#73184 = ORIENTED_EDGE ( 'NONE', *, *, #81814, .F. ) ;
#73185 = CARTESIAN_POINT ( 'NONE',  ( 74.79166666666667140, 3.975000000000003642, -6.884901960086285300 ) ) ;
#73186 = DIRECTION ( 'NONE',  ( 1.000000000000000000, 0.000000000000000000, 0.000000000000000000 ) ) ;
#73187 = CARTESIAN_POINT ( 'NONE',  ( 95.28709685856479439, 3.054999999999997495, 5.291415217122919401 ) ) ;
#73188 = ORIENTED_EDGE ( 'NONE', *, *, #112105, .T. ) ;
#73189 = FACE_OUTER_BOUND ( 'NONE', #142407, .T. ) ;
#73190 = VERTEX_POINT ( 'NONE', #127683 ) ;
#73192 = EDGE_CURVE ( 'NONE', #14419, #121472, #83459, .T. ) ;
#73191 = CARTESIAN_POINT ( 'NONE',  ( -21.29974487139158512, -27.71228299555221142, 4.000000000000000000 ) ) ;
#73193 = LINE ( 'NONE', #52813, #137143 ) ;
#73194 = LINE ( 'NONE', #9287, #99476 ) ;
#73195 = EDGE_LOOP ( 'NONE', ( #53444, #4989, #10081, #53711 ) ) ;
#73196 = ORIENTED_EDGE ( 'NONE', *, *, #96369, .F. ) ;
#73197 = VERTEX_POINT ( 'NONE', #5133 ) ;
#73198 = DIRECTION ( 'NONE',  ( -0.3543493200069162685, -0.000000000000000000, -0.9351131265310288487 ) ) ;
#73199 = DIRECTION ( 'NONE',  ( -0.3543493200069164351, 0.000000000000000000, -0.9351131265310288487 ) ) ;
#73200 = CARTESIAN_POINT ( 'NONE',  ( 11.87956980810188767, 3.967499999999998916, 6.871911579029510442 ) ) ;
#73201 = DIRECTION ( 'NONE',  ( 0.000000000000000000, 0.000000000000000000, 1.000000000000000000 ) ) ;
#73202 = EDGE_CURVE ( 'NONE', #141613, #80963, #56916, .T. ) ;
#73203 = VERTEX_POINT ( 'NONE', #72626 ) ;
#73204 = VERTEX_POINT ( 'NONE', #101089 ) ;
#73205 = DIRECTION ( 'NONE',  ( 0.7071067811865487940, 0.7071067811865463515, 0.000000000000000000 ) ) ;
#73207 = ORIENTED_EDGE ( 'NONE', *, *, #90817, .F. ) ;
#73206 = EDGE_CURVE ( 'NONE', #34286, #108094, #16010, .T. ) ;
#73208 = EDGE_LOOP ( 'NONE', ( #142608, #43343, #107696, #115470 ) ) ;
#73209 = VECTOR ( 'NONE', #70530, 1000.000000000000000 ) ;
#73210 = CARTESIAN_POINT ( 'NONE',  ( -11.99999999999991473, -0.4125381241607498639, 4.000000000000000000 ) ) ;
#73211 = DIRECTION ( 'NONE',  ( -0.5735764363510507113, 0.8191520442889885789, 1.003171929053520926E-16 ) ) ;
#73212 = ORIENTED_EDGE ( 'NONE', *, *, #111933, .T. ) ;
#73213 = CARTESIAN_POINT ( 'NONE',  ( 25.82816939922335209, 21.75929247661549581, 4.000000000000000000 ) ) ;
#73214 = EDGE_CURVE ( 'NONE', #84066, #77643, #2468, .T. ) ;
#73215 = CARTESIAN_POINT ( 'NONE',  ( 11.51078643762690490, -27.52281430457047406, 5.000000000000000000 ) ) ;
#73216 = CYLINDRICAL_SURFACE ( 'NONE', #96983, 0.5000000000000004441 ) ;
#73217 = SURFACE_STYLE_FILL_AREA ( #118089 ) ;
#73218 = ORIENTED_EDGE ( 'NONE', *, *, #58289, .F. ) ;
#73219 = CARTESIAN_POINT ( 'NONE',  ( -4.499999999999976019, 22.08746187583903264, 4.000000000000000000 ) ) ;
#73220 = FACE_BOUND ( 'NONE', #99599, .T. ) ;
#73221 = EDGE_LOOP ( 'NONE', ( #83106, #1332, #95031 ) ) ;
#73222 = LINE ( 'NONE', #62349, #96658 ) ;
#73224 = ADVANCED_FACE ( 'NONE', ( #17467 ), #99689, .T. ) ;
#73223 = CARTESIAN_POINT ( 'NONE',  ( 5.380000000000000782, 9.521314400968980422E-16, 0.000000000000000000 ) ) ;
#73225 = CARTESIAN_POINT ( 'NONE',  ( 78.29974487139158157, -27.71228299555260577, 4.000000000000000000 ) ) ;
#73226 = ORIENTED_EDGE ( 'NONE', *, *, #34838, .T. ) ;
#73227 = DIRECTION ( 'NONE',  ( 0.7071067811865487940, 0.7071067811865463515, 0.000000000000000000 ) ) ;
#73228 = ORIENTED_EDGE ( 'NONE', *, *, #33554, .F. ) ;
#73229 = ORIENTED_EDGE ( 'NONE', *, *, #76056, .T. ) ;
#73230 = EDGE_LOOP ( 'NONE', ( #17879, #117761, #52761, #122548, #124549 ) ) ;
#73231 = AXIS2_PLACEMENT_3D ( 'NONE', #133835, #13445, #80193 ) ;
#73232 = CARTESIAN_POINT ( 'NONE',  ( 27.62043019189810877, 3.055000000000001936, -5.291415217122916737 ) ) ;
#73233 = DIRECTION ( 'NONE',  ( 0.6830127018922181881, 0.6830127018922202975, -0.2588190451025214056 ) ) ;
#73234 = VECTOR ( 'NONE', #6982, 1000.000000000000000 ) ;
#73235 = LINE ( 'NONE', #95671, #113257 ) ;
#73236 = CARTESIAN_POINT ( 'NONE',  ( 13.49159235450332162, 9.902892378096218942E-16, 0.000000000000000000 ) ) ;
#73237 = PLANE ( 'NONE',  #59844 ) ;
#73239 = LINE ( 'NONE', #52174, #75062 ) ;
#73238 = DIRECTION ( 'NONE',  ( -0.7071067811865486830, 0.7071067811865464625, 0.000000000000000000 ) ) ;
#73240 = DIRECTION ( 'NONE',  ( 0.6830127018922181881, 0.6830127018922202975, -0.2588190451025214056 ) ) ;
#73241 = CARTESIAN_POINT ( 'NONE',  ( -12.83829387547372924, -6.740707523384205757, 16.75550250614864112 ) ) ;
#73242 = ADVANCED_FACE ( 'NONE', ( #137851 ), #30252, .T. ) ;
#73243 = CARTESIAN_POINT ( 'NONE',  ( 10.49999999999993605, 4.087461875839200509, 4.000000000000000000 ) ) ;
#73244 = LINE ( 'NONE', #74679, #98047 ) ;
#73245 = AXIS2_PLACEMENT_3D ( 'NONE', #139492, #29249, #108930 ) ;
#73246 = ORIENTED_EDGE ( 'NONE', *, *, #39936, .T. ) ;
#73247 = ORIENTED_EDGE ( 'NONE', *, *, #98030, .T. ) ;
#73248 = VERTEX_POINT ( 'NONE', #24258 ) ;
#73249 = EDGE_LOOP ( 'NONE', ( #85188, #31285, #118676, #53814 ) ) ;
#73250 = CARTESIAN_POINT ( 'NONE',  ( -1.320800000000306618, -4.493284886149243553E-13, 3.775643966265820328 ) ) ;
#73251 = EDGE_LOOP ( 'NONE', ( #9558, #133742, #94702, #113882 ) ) ;
#73252 = ORIENTED_EDGE ( 'NONE', *, *, #67685, .F. ) ;
#73253 = LINE ( 'NONE', #29019, #51428 ) ;
#73254 = DIRECTION ( 'NONE',  ( 0.6830127018922181881, 0.6830127018922202975, -0.2588190451025214056 ) ) ;
#73255 = ADVANCED_FACE ( 'NONE', ( #5854 ), #134457, .F. ) ;
#73256 = VECTOR ( 'NONE', #138420, 1000.000000000000000 ) ;
#73257 = EDGE_CURVE ( 'NONE', #48371, #140728, #112684, .T. ) ;
#73258 = CARTESIAN_POINT ( 'NONE',  ( 1.499999999999990896, 19.39370406404967184, 1.459788787078198258 ) ) ;
#73259 = ORIENTED_EDGE ( 'NONE', *, *, #142555, .T. ) ;
#73260 = CARTESIAN_POINT ( 'NONE',  ( -12.69999999999998153, 3.061616997868383634E-16, -2.500000000000000444 ) ) ;
#73261 = VERTEX_POINT ( 'NONE', #46779 ) ;
#73262 = VECTOR ( 'NONE', #40896, 999.9999999999998863 ) ;
#73264 = CARTESIAN_POINT ( 'NONE',  ( -20.99999999999984368, 17.58746187583906462, 4.000000000000000000 ) ) ;
#73263 = AXIS2_PLACEMENT_3D ( 'NONE', #85112, #30009, #74250 ) ;
#73265 = CARTESIAN_POINT ( 'NONE',  ( 7.139999999999985469, -39.92999999999999972, 18.93259187797431764 ) ) ;
#73266 = VECTOR ( 'NONE', #90664, 1000.000000000000000 ) ;
#73267 = CARTESIAN_POINT ( 'NONE',  ( 9.983736474768551972, -5.808823158059035485, -5.808823158059033709 ) ) ;
#73268 = ORIENTED_EDGE ( 'NONE', *, *, #89538, .F. ) ;
#73269 = CARTESIAN_POINT ( 'NONE',  ( 100.8287635252314516, 0.000000000000000000, -6.109999999999999432 ) ) ;
#73270 = CARTESIAN_POINT ( 'NONE',  ( 3.250000000000000000, 4.999999999999998224, 8.040613248383180784E-16 ) ) ;
#73271 = DIRECTION ( 'NONE',  ( -0.000000000000000000, -0.3543493200069152693, 0.9351131265310292928 ) ) ;
#73272 = DIRECTION ( 'NONE',  ( -0.7071067811865487940, 0.7071067811865463515, -0.000000000000000000 ) ) ;
#73273 = EDGE_LOOP ( 'NONE', ( #133867, #61640, #124392, #215 ) ) ;
#73274 = ORIENTED_EDGE ( 'NONE', *, *, #70924, .F. ) ;
#73275 = CARTESIAN_POINT ( 'NONE',  ( 131.8806778009766276, -49.14999999999999147, -40.92499999999998295 ) ) ;
#73276 = ORIENTED_EDGE ( 'NONE', *, *, #18392, .T. ) ;
#73277 = LINE ( 'NONE', #59553, #90287 ) ;
#73278 = DIRECTION ( 'NONE',  ( -0.7071067811865486830, -0.7071067811865464625, -0.000000000000000000 ) ) ;
#73279 = VECTOR ( 'NONE', #139841, 1000.000000000000000 ) ;
#73280 = LINE ( 'NONE', #29042, #84002 ) ;
#73281 = PLANE ( 'NONE',  #100469 ) ;
#73282 = EDGE_CURVE ( 'NONE', #73190, #82074, #90961, .T. ) ;
#73283 = ORIENTED_EDGE ( 'NONE', *, *, #128807, .T. ) ;
#73284 = CARTESIAN_POINT ( 'NONE',  ( -10.49999999999992717, -1.533600742197722910, 5.000000000000000000 ) ) ;
#73285 = CARTESIAN_POINT ( 'NONE',  ( 34.92499999999998295, -4.662012949885794733, -5.188494296035330855 ) ) ;
#73286 = CARTESIAN_POINT ( 'NONE',  ( 6.328169399223488867, 11.25929247661560595, 4.000000000000000000 ) ) ;
#73287 = VERTEX_POINT ( 'NONE', #798 ) ;
#73288 = CARTESIAN_POINT ( 'NONE',  ( -66.18398860626901126, 28.73617430169833753, 5.000000000000000000 ) ) ;
#73289 = CARTESIAN_POINT ( 'NONE',  ( -5.999999999999956479, 18.08204922493373346, 0.9627537363045027830 ) ) ;
#73290 = EDGE_LOOP ( 'NONE', ( #48468, #71451, #73546, #93070 ) ) ;
#73292 = EDGE_LOOP ( 'NONE', ( #52663, #37207, #45699, #132720 ) ) ;
#73291 = CARTESIAN_POINT ( 'NONE',  ( 0.000000000000000000, 0.000000000000000000, 6.750000000000000888 ) ) ;
#73293 = DIRECTION ( 'NONE',  ( 0.7071067811865487940, 0.7071067811865463515, 0.000000000000000000 ) ) ;
#73294 = LINE ( 'NONE', #98587, #73872 ) ;
#73295 = EDGE_LOOP ( 'NONE', ( #31799, #120302, #10272, #70897 ) ) ;
#73296 = DIRECTION ( 'NONE',  ( 0.6830127018922181881, 0.6830127018922202975, -0.2588190451025214056 ) ) ;
#73297 = CARTESIAN_POINT ( 'NONE',  ( 13.74845587132416291, -11.24070752338416490, 10.39518518046006079 ) ) ;
#73298 = EDGE_CURVE ( 'NONE', #44162, #16196, #131340, .T. ) ;
#73299 = VECTOR ( 'NONE', #140454, 1000.000000000000000 ) ;
#73300 = CARTESIAN_POINT ( 'NONE',  ( 81.18398860626899705, 28.73617430169844056, 5.000000000000000000 ) ) ;
#73301 = CARTESIAN_POINT ( 'NONE',  ( -54.18398860626899705, 28.73617430169825226, 5.000000000000000000 ) ) ;
#73302 = EDGE_CURVE ( 'NONE', #99607, #100020, #129807, .T. ) ;
#73303 = CARTESIAN_POINT ( 'NONE',  ( 34.42499999999998295, -19.45860074219776692, 5.000000000000000000 ) ) ;
#73304 = CARTESIAN_POINT ( 'NONE',  ( 1.499999999999997780, -14.94781430457067728, 5.000000000000000000 ) ) ;
#73305 = CARTESIAN_POINT ( 'NONE',  ( 47.81249999999999289, 5.819803920172571310, 5.819803920172576639 ) ) ;
#73306 = DIRECTION ( 'NONE',  ( -0.7071067811865486830, -0.7071067811865464625, 0.000000000000000000 ) ) ;
#73307 = PLANE ( 'NONE',  #53642 ) ;
#73308 = CARTESIAN_POINT ( 'NONE',  ( 26.99999999999999645, 5.837062628940091535, 2.500239961634333596 ) ) ;
#73309 = DIRECTION ( 'NONE',  ( 0.6830127018922180770, -0.6830127018922204085, -0.2588190451025213501 ) ) ;
#73311 = EDGE_CURVE ( 'NONE', #127430, #131000, #3469, .T. ) ;
#73310 = DIRECTION ( 'NONE',  ( -0.7071067811865487940, 0.7071067811865463515, 0.000000000000000000 ) ) ;
#73313 = EDGE_CURVE ( 'NONE', #9187, #93841, #25971, .T. ) ;
#73312 = EDGE_LOOP ( 'NONE', ( #33625, #25393, #59330, #42979 ) ) ;
#73314 =( BOUNDED_CURVE ( )  B_SPLINE_CURVE ( 3, ( #15534, #59815, #126463, #5388 ),
 .UNSPECIFIED., .F., .T. ) 
 B_SPLINE_CURVE_WITH_KNOTS ( ( 4, 4 ),
 ( 2.779374508378134045, 4.199602562396851368 ),
 .UNSPECIFIED. ) 
 CURVE ( )  GEOMETRIC_REPRESENTATION_ITEM ( )  RATIONAL_B_SPLINE_CURVE ( ( 1.000000000000000000, 0.8388583629366599403, 0.8388583629366599403, 1.000000000000000000 ) ) 
 REPRESENTATION_ITEM ( '' )  );
#73315 = ORIENTED_EDGE ( 'NONE', *, *, #66068, .F. ) ;
#73316 = VERTEX_POINT ( 'NONE', #36833 ) ;
#73317 = CARTESIAN_POINT ( 'NONE',  ( 107.7500000000000000, -9.735942053221458872E-16, 7.950000000000000178 ) ) ;
#73318 = ORIENTED_EDGE ( 'NONE', *, *, #69750, .F. ) ;
#73319 = ORIENTED_EDGE ( 'NONE', *, *, #106985, .F. ) ;
#73320 = ORIENTED_EDGE ( 'NONE', *, *, #34878, .F. ) ;
#73321 = AXIS2_PLACEMENT_3D ( 'NONE', #122858, #56224, #80795 ) ;
#73322 = CARTESIAN_POINT ( 'NONE',  ( 4.499999999999976019, 19.46639925780205616, 5.000000000000000000 ) ) ;
#73323 = CARTESIAN_POINT ( 'NONE',  ( 18.29974487139159223, -27.71228299555219010, 4.000000000000000000 ) ) ;
#73324 = ORIENTED_EDGE ( 'NONE', *, *, #42802, .T. ) ;
#73325 =( BOUNDED_CURVE ( )  B_SPLINE_CURVE ( 2, ( #50344, #127918, #38049, #16236, #27862, #40209, #28600, #116302, #18381, #51059, #61951, #139525, #61268 ),
 .UNSPECIFIED., .F., .T. ) 
 B_SPLINE_CURVE_WITH_KNOTS ( ( 3, 2, 2, 2, 2, 2, 3 ),
 ( 0.2666666666666666630, 0.2694444444444444309, 0.2722222222222221988, 0.2750000000000000222, 0.2777777777777777901, 0.2805555555555555580, 0.2833333333333333259 ),
 .UNSPECIFIED. ) 
 CURVE ( )  GEOMETRIC_REPRESENTATION_ITEM ( )  RATIONAL_B_SPLINE_CURVE ( ( 1.000000000000000000, 0.9659258262890683122, 1.000000000000000000, 0.9659258262890683122, 1.000000000000000000, 0.9659258262890683122, 1.000000000000000000, 0.9659258262890683122, 1.000000000000000000, 0.9659258262890683122, 1.000000000000000000, 0.9659258262890683122, 1.000000000000000000 ) ) 
 REPRESENTATION_ITEM ( '' )  );
#73326 = CARTESIAN_POINT ( 'NONE',  ( 0.000000000000000000, -2.375000000000000000, 0.000000000000000000 ) ) ;
#73327 = LINE ( 'NONE', #140015, #53292 ) ;
#73328 = ADVANCED_FACE ( 'NONE', ( #45090 ), #125285, .F. ) ;
#73330 = AXIS2_PLACEMENT_3D ( 'NONE', #5231, #37171, #82839 ) ;
#73329 = DIRECTION ( 'NONE',  ( 0.7071067811865486830, -0.7071067811865464625, -0.000000000000000000 ) ) ;
#73331 = CARTESIAN_POINT ( 'NONE',  ( 7.720000000000001528, 9.521314400968980422E-16, 0.000000000000000000 ) ) ;
#73332 = CARTESIAN_POINT ( 'NONE',  ( 104.7087635252314328, -7.482591942790329030E-16, 6.110000000000001208 ) ) ;
#73333 = VERTEX_POINT ( 'NONE', #81081 ) ;
#73334 = EDGE_CURVE ( 'NONE', #119622, #91654, #44356, .T. ) ;
#73335 = CARTESIAN_POINT ( 'NONE',  ( -14.95213108811772784, 4.188779951252514344, -32.28871390651440976 ) ) ;
#73336 = CARTESIAN_POINT ( 'NONE',  ( -50.99451991528749062, 28.92564299267973738, 4.000000000000000000 ) ) ;
#73337 = CARTESIAN_POINT ( 'NONE',  ( 34.49999999999975842, 10.94296225409029510, -9.576120664313178210 ) ) ;
#73338 = PLANE ( 'NONE',  #16790 ) ;
#73339 = PLANE ( 'NONE',  #121764 ) ;
#73340 = CARTESIAN_POINT ( 'NONE',  ( 41.78752705046289151, 0.000000000000000000, -7.949999999999998401 ) ) ;
#73341 = ADVANCED_FACE ( 'NONE', ( #87123 ), #102827, .F. ) ;
#73342 = AXIS2_PLACEMENT_3D ( 'NONE', #9530, #29871, #98009 ) ;
#73343 = DIRECTION ( 'NONE',  ( -0.7071067811865486830, -0.7071067811865464625, -0.000000000000000000 ) ) ;
#73344 = CARTESIAN_POINT ( 'NONE',  ( 174.7500000000000000, 7.919999999999947526, -18.97500000000001918 ) ) ;
#73345 = ORIENTED_EDGE ( 'NONE', *, *, #107749, .F. ) ;
#73346 = ORIENTED_EDGE ( 'NONE', *, *, #136759, .T. ) ;
#73347 = CARTESIAN_POINT ( 'NONE',  ( 126.1462635252314328, -4.472830434245840259, 4.472830434245839371 ) ) ;
#73348 = AXIS2_PLACEMENT_3D ( 'NONE', #92417, #48958, #72164 ) ;
#73349 = ORIENTED_EDGE ( 'NONE', *, *, #73732, .T. ) ;
#73350 = DIRECTION ( 'NONE',  ( -0.6830127018922180770, -0.6830127018922204085, -0.2588190451025213501 ) ) ;
#73351 = LINE ( 'NONE', #129130, #96429 ) ;
#73352 = EDGE_CURVE ( 'NONE', #108369, #60317, #70239, .T. ) ;
#73353 = DIRECTION ( 'NONE',  ( -0.000000000000000000, -0.3543493200069152693, 0.9351131265310292928 ) ) ;
#73354 = DIRECTION ( 'NONE',  ( 0.7071067811865486830, -0.7071067811865464625, -0.000000000000000000 ) ) ;
#73355 = DIRECTION ( 'NONE',  ( -1.000000000000000000, 0.000000000000000000, 0.000000000000000000 ) ) ;
#73356 = LINE ( 'NONE', #138605, #81216 ) ;
#73357 = CARTESIAN_POINT ( 'NONE',  ( 125.4745968585647944, 1.637169565754164058, -6.109999999999996767 ) ) ;
#73359 = VERTEX_POINT ( 'NONE', #88569 ) ;
#73358 = VECTOR ( 'NONE', #38258, 1000.000000000000000 ) ;
#73360 = CARTESIAN_POINT ( 'NONE',  ( -34.92500000000001137, 18.20450307870169482, 3.476483422452869565 ) ) ;
#73361 = ORIENTED_EDGE ( 'NONE', *, *, #14239, .T. ) ;
#73362 = EDGE_CURVE ( 'NONE', #128274, #120044, #66102, .T. ) ;
#73363 = CARTESIAN_POINT ( 'NONE',  ( -2.000000000000000000, 2.375000000000000000, 4.319999999999998508 ) ) ;
#73364 = DIRECTION ( 'NONE',  ( 0.7071067811865487940, 0.7071067811865463515, 0.000000000000000000 ) ) ;
#73365 = DIRECTION ( 'NONE',  ( 1.000000000000000000, 0.000000000000000000, 0.000000000000000000 ) ) ;
#73366 = EDGE_LOOP ( 'NONE', ( #57325, #3835, #79293, #49556 ) ) ;
#73367 = AXIS2_PLACEMENT_3D ( 'NONE', #139541, #27876, #37342 ) ;
#73368 = CARTESIAN_POINT ( 'NONE',  ( 49.14626352523143282, -4.472830434245840259, 4.472830434245839371 ) ) ;
#73369 = EDGE_LOOP ( 'NONE', ( #117107, #43470, #60310, #73944 ) ) ;
#73370 = LINE ( 'NONE', #29827, #26237 ) ;
#73371 = LINE ( 'NONE', #130946, #25424 ) ;
#73372 = CARTESIAN_POINT ( 'NONE',  ( -54.48921356237310221, -27.52281430457093236, 5.000000000000000000 ) ) ;
#73373 = EDGE_CURVE ( 'NONE', #45800, #78583, #10948, .T. ) ;
#73374 = EDGE_CURVE ( 'NONE', #94538, #87694, #21141, .T. ) ;
#73375 = CARTESIAN_POINT ( 'NONE',  ( 5.999999999999963585, -10.06887692260771061, 4.000000000000000000 ) ) ;
#73376 = VECTOR ( 'NONE', #39681, 1000.000000000000000 ) ;
#73377 = AXIS2_PLACEMENT_3D ( 'NONE', #76957, #78358, #67507 ) ;
#73378 = EDGE_CURVE ( 'NONE', #44903, #59504, #62672, .T. ) ;
#73379 = VECTOR ( 'NONE', #70163, 1000.000000000000227 ) ;
#73380 = CARTESIAN_POINT ( 'NONE',  ( 50.51626352523143737, -4.472830434245839371, 4.472830434245839371 ) ) ;
#73381 = VERTEX_POINT ( 'NONE', #136150 ) ;
#73382 = CARTESIAN_POINT ( 'NONE',  ( 33.29974487139158867, -27.71228299555229313, 4.000000000000000000 ) ) ;
#73383 = VECTOR ( 'NONE', #34647, 1000.000000000000000 ) ;
#73384 = CARTESIAN_POINT ( 'NONE',  ( 3.489213562373097322, -27.52281430457057709, 5.000000000000000000 ) ) ;
#73385 = ORIENTED_EDGE ( 'NONE', *, *, #123024, .T. ) ;
#73386 = ORIENTED_EDGE ( 'NONE', *, *, #90756, .T. ) ;
#73387 = AXIS2_PLACEMENT_3D ( 'NONE', #105937, #63218, #137899 ) ;
#73388 = ORIENTED_EDGE ( 'NONE', *, *, #5294, .T. ) ;
#73389 = CARTESIAN_POINT ( 'NONE',  ( 60.01669371712956291, 7.950000000000000178, -2.130196079827421318 ) ) ;
#73390 = EDGE_LOOP ( 'NONE', ( #132288, #78655, #87510, #61570 ) ) ;
#73391 = CARTESIAN_POINT ( 'NONE',  ( 3.489213562373097322, -27.52281430457057709, 5.000000000000000000 ) ) ;
#73392 = FACE_BOUND ( 'NONE', #127083, .T. ) ;
#73393 = CARTESIAN_POINT ( 'NONE',  ( 18.29974487139159223, -27.71228299555219010, 4.000000000000000000 ) ) ;
#73394 = DIRECTION ( 'NONE',  ( 0.6830127018922180770, -0.6830127018922204085, -0.2588190451025213501 ) ) ;
#73395 = ORIENTED_EDGE ( 'NONE', *, *, #3075, .F. ) ;
#73396 =( NAMED_UNIT ( * ) PLANE_ANGLE_UNIT ( ) SI_UNIT ( $, .RADIAN. ) );
#73397 = ORIENTED_EDGE ( 'NONE', *, *, #10993, .F. ) ;
#73398 = VECTOR ( 'NONE', #132822, 1000.000000000000000 ) ;
#73399 = ORIENTED_EDGE ( 'NONE', *, *, #57929, .T. ) ;
#73400 = CARTESIAN_POINT ( 'NONE',  ( -32.29289321881322650, -15.74070752338412760, 5.000000000000000000 ) ) ;
#73401 = ORIENTED_EDGE ( 'NONE', *, *, #3516, .T. ) ;
#73402 = CARTESIAN_POINT ( 'NONE',  ( 57.66209685856478728, -5.291415217122919401, 3.054999999999997939 ) ) ;
#73403 = VECTOR ( 'NONE', #83977, 1000.000000000000227 ) ;
#73404 = EDGE_LOOP ( 'NONE', ( #84295, #111671, #88684, #77614 ) ) ;
#73405 = DIRECTION ( 'NONE',  ( -0.7071067811865487940, 0.7071067811865463515, 0.000000000000000000 ) ) ;
#73406 = DIRECTION ( 'NONE',  ( 0.7071067811865487940, 0.7071067811865463515, 0.000000000000000000 ) ) ;
#73407 = VERTEX_POINT ( 'NONE', #114397 ) ;
#73408 = DIRECTION ( 'NONE',  ( 0.7071067811865487940, 0.7071067811865463515, 0.000000000000000000 ) ) ;
#73409 = VECTOR ( 'NONE', #3180, 1000.000000000000000 ) ;
#73410 = DIRECTION ( 'NONE',  ( 0.1737853339090542071, 0.1737853339090537907, 0.9693282805305111216 ) ) ;
#73411 = FACE_OUTER_BOUND ( 'NONE', #135750, .T. ) ;
#73412 = CARTESIAN_POINT ( 'NONE',  ( 0.000000000000000000, -9.500000000000000000, 0.000000000000000000 ) ) ;
#73413 = CARTESIAN_POINT ( 'NONE',  ( 16.18750000000000000, 4.461849672132297329, -4.461849672132302658 ) ) ;
#73414 = DIRECTION ( 'NONE',  ( -0.7071067811865486830, -0.7071067811865464625, 0.000000000000000000 ) ) ;
#73415 = ORIENTED_EDGE ( 'NONE', *, *, #38820, .T. ) ;
#73416 = VECTOR ( 'NONE', #8177, 1000.000000000000000 ) ;
#73417 = ORIENTED_EDGE ( 'NONE', *, *, #32105, .F. ) ;
#73418 = DIRECTION ( 'NONE',  ( -0.000000000000000000, 0.000000000000000000, 1.000000000000000000 ) ) ;
#73419 = FACE_OUTER_BOUND ( 'NONE', #13669, .T. ) ;
#73420 = EDGE_LOOP ( 'NONE', ( #37883, #21267, #75239 ) ) ;
#73421 = ORIENTED_EDGE ( 'NONE', *, *, #114155, .T. ) ;
#73422 = ORIENTED_EDGE ( 'NONE', *, *, #132915, .T. ) ;
#73423 = DIRECTION ( 'NONE',  ( 0.7071067811865486830, -0.7071067811865464625, -0.000000000000000000 ) ) ;
#73424 = VECTOR ( 'NONE', #137214, 1000.000000000000000 ) ;
#73425 = EDGE_CURVE ( 'NONE', #82074, #27289, #76994, .T. ) ;
#73426 = EDGE_CURVE ( 'NONE', #92047, #92458, #54516, .T. ) ;
#73427 = FACE_OUTER_BOUND ( 'NONE', #29109, .T. ) ;
#73428 = ORIENTED_EDGE ( 'NONE', *, *, #121125, .F. ) ;
#73429 = CARTESIAN_POINT ( 'NONE',  ( -20.99999999999984368, -7.447814304570752775, 5.000000000000000000 ) ) ;
#73430 = CARTESIAN_POINT ( 'NONE',  ( 14.99999999999990052, -6.412538124160687580, 4.000000000000000000 ) ) ;
#73431 = CARTESIAN_POINT ( 'NONE',  ( 8.379569808101887674, 3.967499999999998916, 6.871911579029510442 ) ) ;
#73432 = DIRECTION ( 'NONE',  ( -0.000000000000000000, 0.3543493200069153248, 0.9351131265310292928 ) ) ;
#73433 = ORIENTED_EDGE ( 'NONE', *, *, #60595, .F. ) ;
#73434 = CARTESIAN_POINT ( 'NONE',  ( 127.8079301918981230, -6.109999999999999432, 1.637169565754158507 ) ) ;
#73435 = AXIS2_PLACEMENT_3D ( 'NONE', #108106, #29852, #119692 ) ;
#73436 = EDGE_CURVE ( 'NONE', #43782, #130838, #135464, .T. ) ;
#73437 = CARTESIAN_POINT ( 'NONE',  ( 20.19999999999999929, 2.055000000000001492, 0.000000000000000000 ) ) ;
#73438 = DIRECTION ( 'NONE',  ( -0.000000000000000000, -0.3543493200069152693, 0.9351131265310292928 ) ) ;
#73440 = ORIENTED_EDGE ( 'NONE', *, *, #64806, .F. ) ;
#73439 = CARTESIAN_POINT ( 'NONE',  ( 2.292893218813439216, 20.25929247661551713, 5.000000000000000000 ) ) ;
#73441 = LINE ( 'NONE', #4525, #97953 ) ;
#73442 = ORIENTED_EDGE ( 'NONE', *, *, #70512, .T. ) ;
#73443 = CARTESIAN_POINT ( 'NONE',  ( 75.47502705046287019, -5.819803920172573086, 5.819803920172573086 ) ) ;
#73444 = PLANE ( 'NONE',  #79472 ) ;
#73445 = DIRECTION ( 'NONE',  ( -0.7071067811865486830, -0.7071067811865464625, -0.000000000000000000 ) ) ;
#73446 = ADVANCED_FACE ( 'NONE', ( #21856 ), #132805, .F. ) ;
#73447 = VERTEX_POINT ( 'NONE', #80377 ) ;
#73448 = AXIS2_PLACEMENT_3D ( 'NONE', #29330, #83019, #39529 ) ;
#73449 = LINE ( 'NONE', #115467, #79655 ) ;
#73450 = LINE ( 'NONE', #18301, #16369 ) ;
#73451 = CARTESIAN_POINT ( 'NONE',  ( -13.49999999999990052, 6.052185695429106893, 5.000000000000000000 ) ) ;
#73452 = ORIENTED_EDGE ( 'NONE', *, *, #108765, .F. ) ;
#73453 = ADVANCED_FACE ( 'NONE', ( #124566 ), #135664, .F. ) ;
#73454 = DIRECTION ( 'NONE',  ( -0.000000000000000000, 0.000000000000000000, 1.000000000000000000 ) ) ;
#73455 = DIRECTION ( 'NONE',  ( -0.7071067811865487940, 0.7071067811865463515, 0.000000000000000000 ) ) ;
#73456 = DIRECTION ( 'NONE',  ( -0.6830127018922181881, 0.6830127018922202975, -0.2588190451025214056 ) ) ;
#73457 = DIRECTION ( 'NONE',  ( -0.000000000000000000, -0.3543493200069152693, 0.9351131265310292928 ) ) ;
#73458 = VECTOR ( 'NONE', #1299, 1000.000000000000000 ) ;
#73459 = CYLINDRICAL_SURFACE ( 'NONE', #99337, 5.999999999999998224 ) ;
#73460 = ORIENTED_EDGE ( 'NONE', *, *, #6277, .F. ) ;
#73461 = ORIENTED_EDGE ( 'NONE', *, *, #84309, .F. ) ;
#73462 = LINE ( 'NONE', #116239, #3173 ) ;
#73463 = VECTOR ( 'NONE', #66420, 1000.000000000000000 ) ;
#73464 = AXIS2_PLACEMENT_3D ( 'NONE', #68422, #90124, #35071 ) ;
#73465 = CARTESIAN_POINT ( 'NONE',  ( 14.99956980810188689, -3.967499999999998028, -6.871911579029511330 ) ) ;
#73466 = DIRECTION ( 'NONE',  ( 0.7071067811865486830, -0.7071067811865464625, -0.000000000000000000 ) ) ;
#73467 = CIRCLE ( 'NONE', #27181, 2.055000000000001048 ) ;
#73468 = LINE ( 'NONE', #82225, #120072 ) ;
#73469 = DIRECTION ( 'NONE',  ( -1.000000000000000000, -0.000000000000000000, -0.000000000000000000 ) ) ;
#73470 = EDGE_LOOP ( 'NONE', ( #43563, #57004, #23805, #2059 ) ) ;
#73471 = EDGE_CURVE ( 'NONE', #92630, #132295, #120455, .T. ) ;
#73472 = SPHERICAL_SURFACE ( 'NONE', #41916, 0.5000000000000000000 ) ;
#73473 = LINE ( 'NONE', #91808, #11885 ) ;
#73474 = AXIS2_PLACEMENT_3D ( 'NONE', #49117, #27320, #15699 ) ;
#73475 = CARTESIAN_POINT ( 'NONE',  ( 0.000000000000000000, 0.000000000000000000, 5.000000000000000000 ) ) ;
#73476 = CARTESIAN_POINT ( 'NONE',  ( 48.47459685856478728, 1.637169565754164280, -6.109999999999997655 ) ) ;
#73477 = DIRECTION ( 'NONE',  ( 0.000000000000000000, -1.000000000000000000, 0.000000000000000000 ) ) ;
#73478 = ADVANCED_FACE ( 'NONE', ( #12434 ), #45120, .T. ) ;
#73479 = EDGE_CURVE ( 'NONE', #71697, #25861, #89989, .T. ) ;
#73480 = ORIENTED_EDGE ( 'NONE', *, *, #71013, .F. ) ;
#73481 = DIRECTION ( 'NONE',  ( 0.7071067811865486830, -0.7071067811865464625, -0.000000000000000000 ) ) ;
#73482 = EDGE_LOOP ( 'NONE', ( #57183, #117200, #105332, #72064 ) ) ;
#73483 = EDGE_LOOP ( 'NONE', ( #31178, #113472, #11596, #15922 ) ) ;
#73484 = CARTESIAN_POINT ( 'NONE',  ( -7.499999999999954703, 3.653845994658382779, -4.504631822206354386 ) ) ;
#73485 = ADVANCED_FACE ( 'NONE', ( #3669 ), #23295, .F. ) ;
#73486 = CARTESIAN_POINT ( 'NONE',  ( 21.60486233187507921, 21.75929247661549226, 21.32995629748181443 ) ) ;
#73487 = PLANE ( 'NONE',  #23431 ) ;
#73488 = DIRECTION ( 'NONE',  ( -0.6830127018922180770, -0.6830127018922204085, -0.2588190451025213501 ) ) ;
#73489 = EDGE_CURVE ( 'NONE', #96482, #95547, #17413, .T. ) ;
#73490 = CARTESIAN_POINT ( 'NONE',  ( 82.66666666666667140, 6.884901960086285300, 3.975000000000003642 ) ) ;
#73491 = CARTESIAN_POINT ( 'NONE',  ( 126.8754301918981184, -5.291415217122920289, -3.055000000000001492 ) ) ;
#73492 = EDGE_LOOP ( 'NONE', ( #106106, #122240, #76945, #55718, #83057 ) ) ;
#73493 = EDGE_CURVE ( 'NONE', #98697, #83142, #26188, .T. ) ;
#73494 = FACE_OUTER_BOUND ( 'NONE', #136426, .T. ) ;
#73495 = DIRECTION ( 'NONE',  ( 0.3543493200069162685, -0.000000000000000000, -0.9351131265310288487 ) ) ;
#73496 = CIRCLE ( 'NONE', #85065, 2.499999999999998668 ) ;
#73497 = LINE ( 'NONE', #95942, #47307 ) ;
#73498 = PLANE ( 'NONE',  #6779 ) ;
#73499 = LINE ( 'NONE', #53140, #128391 ) ;
#73500 =( BOUNDED_CURVE ( )  B_SPLINE_CURVE ( 3, ( #26506, #70751, #125096, #4686 ),
 .UNSPECIFIED., .F., .T. ) 
 B_SPLINE_CURVE_WITH_KNOTS ( ( 4, 4 ),
 ( 4.350170835173024386, 4.500739107949264017 ),
 .UNSPECIFIED. ) 
 CURVE ( )  GEOMETRIC_REPRESENTATION_ITEM ( )  RATIONAL_B_SPLINE_CURVE ( ( 1.000000000000000000, 0.9981116584018943083, 0.9981116584018943083, 1.000000000000000000 ) ) 
 REPRESENTATION_ITEM ( '' )  );
#73501 = DIRECTION ( 'NONE',  ( 0.000000000000000000, -1.000000000000000000, 0.000000000000000000 ) ) ;
#73502 = CARTESIAN_POINT ( 'NONE',  ( 63.95419371712955581, 6.884901960086283523, 3.975000000000002753 ) ) ;
#73503 = AXIS2_PLACEMENT_3D ( 'NONE', #50625, #81865, #17274 ) ;
#73504 = PLANE ( 'NONE',  #99394 ) ;
#73505 = EDGE_LOOP ( 'NONE', ( #85808, #113104, #53282, #96153 ) ) ;
#73506 = ORIENTED_EDGE ( 'NONE', *, *, #109095, .F. ) ;
#73507 = CARTESIAN_POINT ( 'NONE',  ( 57.14583333333332860, 2.130196079827431976, -7.949999999999999289 ) ) ;
#73508 = EDGE_CURVE ( 'NONE', #46464, #49172, #14588, .T. ) ;
#73509 = CARTESIAN_POINT ( 'NONE',  ( 34.92499999999998295, -12.18334561358941137, 4.500000000000000888 ) ) ;
#73510 = DIRECTION ( 'NONE',  ( -0.000000000000000000, -0.3543493200069152693, 0.9351131265310292928 ) ) ;
#73511 = VECTOR ( 'NONE', #24315, 999.9999999999998863 ) ;
#73512 = CARTESIAN_POINT ( 'NONE',  ( 45.18398860626900415, 28.73617430169818832, 5.000000000000000000 ) ) ;
#73513 = ORIENTED_EDGE ( 'NONE', *, *, #40173, .F. ) ;
#73514 = EDGE_CURVE ( 'NONE', #84503, #29420, #45980, .T. ) ;
#73515 = DIRECTION ( 'NONE',  ( -0.7071067811865486830, -0.7071067811865464625, -0.000000000000000000 ) ) ;
#73516 = CARTESIAN_POINT ( 'NONE',  ( 58.62543019189810423, 5.291415217122919401, 3.055000000000002824 ) ) ;
#73517 = ORIENTED_EDGE ( 'NONE', *, *, #22513, .F. ) ;
#73518 = VECTOR ( 'NONE', #53527, 1000.000000000000000 ) ;
#73519 = CARTESIAN_POINT ( 'NONE',  ( -12.69999999999998153, 0.000000000000000000, 0.000000000000000000 ) ) ;
#73520 = ORIENTED_EDGE ( 'NONE', *, *, #96857, .T. ) ;
#73521 = EDGE_LOOP ( 'NONE', ( #20347, #135787, #82282, #126443 ) ) ;
#73522 = DIRECTION ( 'NONE',  ( 0.3543493200069162685, -0.000000000000000000, -0.9351131265310288487 ) ) ;
#73523 = SURFACE_SIDE_STYLE ('',( #63387 ) ) ;
#73524 = LINE ( 'NONE', #62647, #127672 ) ;
#73525 = VECTOR ( 'NONE', #62163, 1000.000000000000000 ) ;
#73526 = FACE_OUTER_BOUND ( 'NONE', #66794, .T. ) ;
#73527 = CARTESIAN_POINT ( 'NONE',  ( 9.183988606268997046, 28.73617430169793607, 5.000000000000000000 ) ) ;
#73528 = LINE ( 'NONE', #127167, #92788 ) ;
#73530 = VERTEX_POINT ( 'NONE', #78427 ) ;
#73529 = PLANE ( 'NONE',  #63813 ) ;
#73531 = CARTESIAN_POINT ( 'NONE',  ( -19.49999999999986855, 21.43112307739196609, 4.000000000000000000 ) ) ;
#73532 = LINE ( 'NONE', #95261, #100307 ) ;
#73533 = EDGE_CURVE ( 'NONE', #124853, #127004, #124774, .T. ) ;
#73534 = LINE ( 'NONE', #27151, #106299 ) ;
#73535 = EDGE_CURVE ( 'NONE', #22717, #133731, #24042, .T. ) ;
#73536 = ORIENTED_EDGE ( 'NONE', *, *, #79475, .F. ) ;
#73537 = EDGE_CURVE ( 'NONE', #10426, #67860, #56717, .T. ) ;
#73538 = ORIENTED_EDGE ( 'NONE', *, *, #116848, .T. ) ;
#73539 = VECTOR ( 'NONE', #90317, 999.9999999999998863 ) ;
#73540 = SURFACE_STYLE_FILL_AREA ( #119847 ) ;
#73541 = CARTESIAN_POINT ( 'NONE',  ( 78.80793019189810877, -6.109999999999998543, 1.637169565754158063 ) ) ;
#73542 = DIRECTION ( 'NONE',  ( 0.6830127018922180770, -0.6830127018922204085, -0.2588190451025213501 ) ) ;
#73543 = CARTESIAN_POINT ( 'NONE',  ( -12.19999999999999929, -59.76999999999998892, -39.50000000000000000 ) ) ;
#73544 = PLANE ( 'NONE',  #73367 ) ;
#73545 = ORIENTED_EDGE ( 'NONE', *, *, #51367, .T. ) ;
#73546 = ORIENTED_EDGE ( 'NONE', *, *, #22332, .F. ) ;
#73547 = PLANE ( 'NONE',  #130208 ) ;
#73548 = EDGE_CURVE ( 'NONE', #88210, #49923, #34933, .T. ) ;
#73549 = EDGE_LOOP ( 'NONE', ( #6152, #47391, #106576, #109590 ) ) ;
#73550 = VERTEX_POINT ( 'NONE', #1532 ) ;
#73551 = DIRECTION ( 'NONE',  ( -0.6830127018922181881, 0.6830127018922202975, -0.2588190451025214056 ) ) ;
#73552 = ORIENTED_EDGE ( 'NONE', *, *, #101235, .T. ) ;
#73553 = LINE ( 'NONE', #120579, #82670 ) ;
#73554 = DIRECTION ( 'NONE',  ( 0.3543493200069162685, -0.000000000000000000, -0.9351131265310288487 ) ) ;
#73555 = AXIS2_PLACEMENT_3D ( 'NONE', #27340, #18593, #51272 ) ;
#73556 = FACE_BOUND ( 'NONE', #29264, .T. ) ;
#73557 = CARTESIAN_POINT ( 'NONE',  ( -17.99451991528748351, 28.92564299267950645, 4.000000000000000000 ) ) ;
#73558 = CARTESIAN_POINT ( 'NONE',  ( -14.99999999999989697, 13.93112307739204070, 4.000000000000000000 ) ) ;
#73560 = ORIENTED_EDGE ( 'NONE', *, *, #54836, .F. ) ;
#73559 = DIRECTION ( 'NONE',  ( -0.7071067811865486830, -0.7071067811865464625, -0.000000000000000000 ) ) ;
#73561 = AXIS2_PLACEMENT_3D ( 'NONE', #25234, #1324, #58655 ) ;
#73562 = VECTOR ( 'NONE', #140756, 1000.000000000000000 ) ;
#73563 = FACE_OUTER_BOUND ( 'NONE', #37977, .T. ) ;
#73564 = APPLICATION_PROTOCOL_DEFINITION ( 'draft international standard', 'automotive_design', 1998, #129112 ) ;
#73565 = VERTEX_POINT ( 'NONE', #45815 ) ;
#73566 = ORIENTED_EDGE ( 'NONE', *, *, #121981, .T. ) ;
#73567 = CARTESIAN_POINT ( 'NONE',  ( 86.39126352523145158, -4.472830434245838482, -4.472830434245838482 ) ) ;
#73568 = VERTEX_POINT ( 'NONE', #24744 ) ;
#73569 = CARTESIAN_POINT ( 'NONE',  ( -23.01088028653932582, -22.02621442084247860, 4.990779571109221990 ) ) ;
#73570 = PLANE ( 'NONE',  #134619 ) ;
#73571 = EDGE_CURVE ( 'NONE', #87041, #94289, #124071, .T. ) ;
#73572 = CARTESIAN_POINT ( 'NONE',  ( -33.29974487139158867, -27.71228299555229313, 4.000000000000000000 ) ) ;
#73573 = CARTESIAN_POINT ( 'NONE',  ( 45.48921356237309510, -27.52281430457087197, 5.000000000000000000 ) ) ;
#73574 = CARTESIAN_POINT ( 'NONE',  ( 7.208502053023265077, 22.22500000000000142, 20.96595896090590117 ) ) ;
#73575 = CARTESIAN_POINT ( 'NONE',  ( 21.18398860626899349, 28.73617430169802134, 5.000000000000000000 ) ) ;
#73576 = DIRECTION ( 'NONE',  ( -0.7071067811865486830, -0.7071067811865464625, -0.000000000000000000 ) ) ;
#73577 = DIRECTION ( 'NONE',  ( 0.7071067811865487940, 0.7071067811865463515, 0.000000000000000000 ) ) ;
#73578 = PLANE ( 'NONE',  #19548 ) ;
#73579 = CARTESIAN_POINT ( 'NONE',  ( -22.82816939922336630, 12.75929247661558996, 4.000000000000000000 ) ) ;
#73580 = FACE_OUTER_BOUND ( 'NONE', #98016, .T. ) ;
#73581 = LINE ( 'NONE', #137413, #7506 ) ;
#73582 = ORIENTED_EDGE ( 'NONE', *, *, #61450, .T. ) ;
#73583 = CARTESIAN_POINT ( 'NONE',  ( -22.49999999999985079, -12.66682484999668290, -0.6294897503864461674 ) ) ;
#73584 = CARTESIAN_POINT ( 'NONE',  ( 34.92499999999998295, -12.53194198458144903, -8.170704600677598961 ) ) ;
#73585 = ADVANCED_FACE ( 'NONE', ( #13843 ), #58869, .F. ) ;
#73586 = ORIENTED_EDGE ( 'NONE', *, *, #106256, .T. ) ;
#73587 = ORIENTED_EDGE ( 'NONE', *, *, #95744, .F. ) ;
#73588 = EDGE_CURVE ( 'NONE', #69767, #124649, #126210, .T. ) ;
#73589 = EDGE_LOOP ( 'NONE', ( #121535, #114149, #32574, #735 ) ) ;
#73590 = CARTESIAN_POINT ( 'NONE',  ( 36.89626352523143993, 4.472830434245840259, -4.472830434245838482 ) ) ;
#73591 = VECTOR ( 'NONE', #109582, 1000.000000000000000 ) ;
#73592 = EDGE_LOOP ( 'NONE', ( #92900, #5753, #2615, #36212 ) ) ;
#73593 = EDGE_CURVE ( 'NONE', #68517, #100573, #46674, .T. ) ;
#73594 = EDGE_CURVE ( 'NONE', #72640, #30768, #7242, .T. ) ;
#73595 = CARTESIAN_POINT ( 'NONE',  ( 17.54580628287044064, 5.278424836066143655, -3.047499999999997655 ) ) ;
#73596 = CARTESIAN_POINT ( 'NONE',  ( 11.08707631394196724, 10.76818482829728829, -26.45687733286667154 ) ) ;
#73597 = ORIENTED_EDGE ( 'NONE', *, *, #28407, .F. ) ;
#73598 = EDGE_CURVE ( 'NONE', #8801, #62928, #139962, .T. ) ;
#73599 = CARTESIAN_POINT ( 'NONE',  ( -27.29974487139158512, -27.71228299555225405, 4.000000000000000000 ) ) ;
#73600 = EDGE_LOOP ( 'NONE', ( #43753, #116731, #73101, #85644, #16331 ) ) ;
#73601 = DIRECTION ( 'NONE',  ( 0.3543493200069162685, -0.000000000000000000, -0.9351131265310288487 ) ) ;
#73602 = CARTESIAN_POINT ( 'NONE',  ( 34.92499999999998295, -3.183345613589516621, 4.500000000000000888 ) ) ;
#73604 = ORIENTED_EDGE ( 'NONE', *, *, #39331, .T. ) ;
#73603 = CARTESIAN_POINT ( 'NONE',  ( 7.171830600776422315, 9.759292476615620160, 4.000000000000000000 ) ) ;
#73605 = ORIENTED_EDGE ( 'NONE', *, *, #132415, .F. ) ;
#73606 = DIRECTION ( 'NONE',  ( 0.7071067811865487940, 0.7071067811865463515, 0.000000000000000000 ) ) ;
#73607 = EDGE_CURVE ( 'NONE', #45742, #56014, #5096, .T. ) ;
#73608 = ORIENTED_EDGE ( 'NONE', *, *, #138226, .T. ) ;
#73609 = LINE ( 'NONE', #30084, #4125 ) ;
#73610 = VERTEX_POINT ( 'NONE', #16723 ) ;
#73611 = ORIENTED_EDGE ( 'NONE', *, *, #9486, .T. ) ;
#73612 = ORIENTED_EDGE ( 'NONE', *, *, #109350, .T. ) ;
#73613 = ORIENTED_EDGE ( 'NONE', *, *, #86206, .F. ) ;
#73614 = DIRECTION ( 'NONE',  ( 0.7071067811865487940, 0.7071067811865463515, -0.000000000000000000 ) ) ;
#73615 = EDGE_CURVE ( 'NONE', #71971, #17986, #84164, .T. ) ;
#73616 = LINE ( 'NONE', #18477, #40062 ) ;
#73617 = CARTESIAN_POINT ( 'NONE',  ( 12.03892749862900402, 4.202752102959690472E-16, 0.000000000000000000 ) ) ;
#73618 = CARTESIAN_POINT ( 'NONE',  ( 7.139999999999997904, -35.14999999999999858, 17.49210858042622263 ) ) ;
#73619 = DIRECTION ( 'NONE',  ( -0.6830127018922181881, 0.6830127018922202975, -0.2588190451025214056 ) ) ;
#73620 = EDGE_LOOP ( 'NONE', ( #45060, #14664, #18937, #20606 ) ) ;
#73621 = DIRECTION ( 'NONE',  ( -0.6830127018922181881, 0.6830127018922202975, -0.2588190451025214056 ) ) ;
#73622 = ORIENTED_EDGE ( 'NONE', *, *, #85080, .F. ) ;
#73623 = EDGE_CURVE ( 'NONE', #48695, #115675, #26886, .T. ) ;
#73624 = DIRECTION ( 'NONE',  ( -0.000000000000000000, 0.3543493200069153248, 0.9351131265310292928 ) ) ;
#73625 = CARTESIAN_POINT ( 'NONE',  ( 27.39540314143522437, 2.126176841940962348, 7.934999999999989839 ) ) ;
#73626 = CARTESIAN_POINT ( 'NONE',  ( 8.475998614145455079, 22.03583458319438293, 4.979811245910090278 ) ) ;
#73627 = ORIENTED_EDGE ( 'NONE', *, *, #78191, .T. ) ;
#73628 = CARTESIAN_POINT ( 'NONE',  ( 23.47599861414535027, 22.03583458319437227, 4.979811245910089390 ) ) ;
#73629 = VECTOR ( 'NONE', #96536, 1000.000000000000000 ) ;
#73630 = CARTESIAN_POINT ( 'NONE',  ( 0.000000000000000000, 0.000000000000000000, 5.000000000000000000 ) ) ;
#73631 = ORIENTED_EDGE ( 'NONE', *, *, #126516, .F. ) ;
#73632 = ORIENTED_EDGE ( 'NONE', *, *, #68145, .F. ) ;
#73634 = ORIENTED_EDGE ( 'NONE', *, *, #132303, .F. ) ;
#73633 = EDGE_CURVE ( 'NONE', #16751, #129366, #82711, .T. ) ;
#73635 = DIRECTION ( 'NONE',  ( -0.7071067811865486830, -0.7071067811865464625, -0.000000000000000000 ) ) ;
#73636 = DIRECTION ( 'NONE',  ( -0.7071067811865487940, 0.7071067811865463515, -0.000000000000000000 ) ) ;
#73637 = DIRECTION ( 'NONE',  ( 0.7071067811865486830, -0.7071067811865464625, -0.000000000000000000 ) ) ;
#73638 = CARTESIAN_POINT ( 'NONE',  ( 0.000000000000000000, 0.000000000000000000, 5.000000000000000000 ) ) ;
#73639 = CARTESIAN_POINT ( 'NONE',  ( 73.41209685856478018, 5.291415217122922066, -3.054999999999995275 ) ) ;
#73640 = CARTESIAN_POINT ( 'NONE',  ( 28.49999999999980460, 15.05218569542901186, 5.000000000000000000 ) ) ;
#73641 = ADVANCED_FACE ( 'NONE', ( #116749 ), #73970, .T. ) ;
#73642 =( NAMED_UNIT ( * ) PLANE_ANGLE_UNIT ( ) SI_UNIT ( $, .RADIAN. ) );
#73643 = CARTESIAN_POINT ( 'NONE',  ( -2.999999999999980016, -16.60178936734448740, 0.8616154019347429527 ) ) ;
#73644 = LINE ( 'NONE', #138913, #79152 ) ;
#73645 = ADVANCED_FACE ( 'NONE', ( #92849 ), #28334, .F. ) ;
#73646 = DIRECTION ( 'NONE',  ( 0.000000000000000000, 0.000000000000000000, 1.000000000000000000 ) ) ;
#73647 = ORIENTED_EDGE ( 'NONE', *, *, #22906, .T. ) ;
#73648 = CARTESIAN_POINT ( 'NONE',  ( -2.994519915287485734, 28.92564299267940342, 4.000000000000000000 ) ) ;
#73649 = LINE ( 'NONE', #62794, #3585 ) ;
#73650 = VERTEX_POINT ( 'NONE', #17432 ) ;
#73651 = AXIS2_PLACEMENT_3D ( 'NONE', #35123, #134424, #35851 ) ;
#73652 = EDGE_CURVE ( 'NONE', #78474, #24379, #15967, .T. ) ;
#73653 = LINE ( 'NONE', #138194, #108609 ) ;
#73655 = ORIENTED_EDGE ( 'NONE', *, *, #136972, .T. ) ;
#73654 = DIRECTION ( 'NONE',  ( -0.7071067811865486830, -0.7071067811865464625, 0.000000000000000000 ) ) ;
#73656 = AXIS2_PLACEMENT_3D ( 'NONE', #93161, #140243, #5407 ) ;
#73657 = CARTESIAN_POINT ( 'NONE',  ( -5.816011393731002066, 28.73617430169783304, 5.000000000000000000 ) ) ;
#73658 = DIRECTION ( 'NONE',  ( -0.7071067811865486830, -0.7071067811865464625, 0.000000000000000000 ) ) ;
#73659 = ORIENTED_EDGE ( 'NONE', *, *, #70651, .T. ) ;
#73660 = ORIENTED_EDGE ( 'NONE', *, *, #142685, .F. ) ;
#73661 = LINE ( 'NONE', #106983, #2331 ) ;
#73662 = LINE ( 'NONE', #141789, #123120 ) ;
#73663 = AXIS2_PLACEMENT_3D ( 'NONE', #85315, #75205, #20057 ) ;
#73664 = VECTOR ( 'NONE', #51468, 1000.000000000000000 ) ;
#73665 = LINE ( 'NONE', #128062, #15155 ) ;
#73666 = CARTESIAN_POINT ( 'NONE',  ( 95.45419371712957002, 6.884901960086283523, 3.975000000000002753 ) ) ;
#73667 = DIRECTION ( 'NONE',  ( 0.7071067811865487940, 0.7071067811865463515, 0.000000000000000000 ) ) ;
#73668 = VERTEX_POINT ( 'NONE', #137085 ) ;
#73669 = EDGE_CURVE ( 'NONE', #94920, #117172, #60260, .T. ) ;
#73670 = DIRECTION ( 'NONE',  ( -0.5735764363510507113, 0.8191520442889885789, 1.003171929053520926E-16 ) ) ;
#73671 = DIRECTION ( 'NONE',  ( -0.7071067811865487940, 0.7071067811865463515, -0.000000000000000000 ) ) ;
#73672 = CARTESIAN_POINT ( 'NONE',  ( 13.84116387061258457, 6.089959206779446355, 4.000000000000000000 ) ) ;
#73673 = CARTESIAN_POINT ( 'NONE',  ( 34.92499999999998295, 22.22500000000000142, 4.000000000000000000 ) ) ;
#73674 = EDGE_LOOP ( 'NONE', ( #80598, #127535, #84168, #136888 ) ) ;
#73675 = EDGE_CURVE ( 'NONE', #16867, #15871, #50788, .T. ) ;
#73676 = DIRECTION ( 'NONE',  ( -0.000000000000000000, 0.3543493200069153248, 0.9351131265310292928 ) ) ;
#73677 = EDGE_LOOP ( 'NONE', ( #32042, #70527, #111032, #71310 ) ) ;
#73678 = CARTESIAN_POINT ( 'NONE',  ( 85.89626352523144703, 4.472830434245840259, -4.472830434245839371 ) ) ;
#73679 = DIRECTION ( 'NONE',  ( -0.7071067811865486830, -0.7071067811865464625, -0.000000000000000000 ) ) ;
#73680 = CARTESIAN_POINT ( 'NONE',  ( -14.99999999999989519, -19.22509904557637839, 1.855685503482144227 ) ) ;
#73681 = ORIENTED_EDGE ( 'NONE', *, *, #9676, .T. ) ;
#73682 = DIRECTION ( 'NONE',  ( -0.000000000000000000, 0.000000000000000000, 1.000000000000000000 ) ) ;
#73683 = VECTOR ( 'NONE', #119084, 1000.000000000000000 ) ;
#73684 = DIRECTION ( 'NONE',  ( -0.7071067811865486830, -0.7071067811865464625, 0.000000000000000000 ) ) ;
#73685 = CARTESIAN_POINT ( 'NONE',  ( 118.0583603837962130, -7.949999999999996625, -2.130196079827426203 ) ) ;
#73686 = EDGE_CURVE ( 'NONE', #13854, #70323, #39944, .T. ) ;
#73688 = VERTEX_POINT ( 'NONE', #49396 ) ;
#73687 = DIRECTION ( 'NONE',  ( -0.7071067811865487940, 0.7071067811865463515, 0.000000000000000000 ) ) ;
#73690 = VECTOR ( 'NONE', #43451, 1000.000000000000227 ) ;
#73689 = LINE ( 'NONE', #41057, #129651 ) ;
#73691 = CARTESIAN_POINT ( 'NONE',  ( -17.99451991528748351, 28.92564299267950645, 4.000000000000000000 ) ) ;
#73692 = CARTESIAN_POINT ( 'NONE',  ( 1.369639479247480862, 4.811953009385816285E-13, 6.725360520752516891 ) ) ;
#73693 = FACE_OUTER_BOUND ( 'NONE', #83324, .T. ) ;
#73694 = VERTEX_POINT ( 'NONE', #65981 ) ;
#73695 = EDGE_CURVE ( 'NONE', #29435, #122913, #129765, .T. ) ;
#73696 = ORIENTED_EDGE ( 'NONE', *, *, #1089, .T. ) ;
#73697 = CARTESIAN_POINT ( 'NONE',  ( 69.56293019189810423, 1.637169565754157174, 6.110000000000002984 ) ) ;
#73698 = EDGE_LOOP ( 'NONE', ( #89265, #65438, #108915, #11128 ) ) ;
#73699 = DIRECTION ( 'NONE',  ( -0.7071067811865486830, -0.7071067811865464625, 0.000000000000000000 ) ) ;
#73700 = DIRECTION ( 'NONE',  ( 0.000000000000000000, 0.000000000000000000, 1.000000000000000000 ) ) ;
#73701 = DIRECTION ( 'NONE',  ( 1.000000000000000000, 0.000000000000000000, 0.000000000000000000 ) ) ;
#73702 = ORIENTED_EDGE ( 'NONE', *, *, #9613, .F. ) ;
#73703 = AXIS2_PLACEMENT_3D ( 'NONE', #65227, #109410, #1339 ) ;
#73704 = CARTESIAN_POINT ( 'NONE',  ( 30.48921356237309510, -27.52281430457076894, 5.000000000000000000 ) ) ;
#73706 =( BOUNDED_CURVE ( )  B_SPLINE_CURVE ( 2, ( #76714, #10675, #129619, #9989, #31754, #30320, #31056, #75971, #20856, #74558, #65117, #40504, #54255 ),
 .UNSPECIFIED., .F., .F. ) 
 B_SPLINE_CURVE_WITH_KNOTS ( ( 3, 2, 2, 2, 2, 2, 3 ),
 ( 0.7500000000000000000, 0.7527777777777777679, 0.7555555555555555358, 0.7583333333333333037, 0.7611111111111110716, 0.7638888888888888395, 0.7666666666666667185 ),
 .UNSPECIFIED. ) 
 CURVE ( )  GEOMETRIC_REPRESENTATION_ITEM ( )  RATIONAL_B_SPLINE_CURVE ( ( 1.000000000000000000, 0.9659258262890683122, 1.000000000000000000, 0.9659258262890683122, 1.000000000000000000, 0.9659258262890683122, 1.000000000000000000, 0.9659258262890683122, 1.000000000000000000, 0.9659258262890683122, 1.000000000000000000, 0.9659258262890683122, 1.000000000000000000 ) ) 
 REPRESENTATION_ITEM ( '' )  );
#73705 = CARTESIAN_POINT ( 'NONE',  ( 7.828169399223476432, 9.759292476615614831, 4.000000000000000000 ) ) ;
#73707 = AXIS2_PLACEMENT_3D ( 'NONE', #71500, #70116, #104086 ) ;
#73708 = EDGE_LOOP ( 'NONE', ( #137061, #93200, #32978, #139252, #131056 ) ) ;
#73709 = DIRECTION ( 'NONE',  ( -0.6830127018922180770, -0.6830127018922204085, -0.2588190451025213501 ) ) ;
#73710 = CARTESIAN_POINT ( 'NONE',  ( 24.29974487139158867, -27.71228299555223273, 4.000000000000000000 ) ) ;
#73711 = CARTESIAN_POINT ( 'NONE',  ( 19.49999999999985789, -2.777013188829488666, 4.549262955118046570 ) ) ;
#73712 = VERTEX_POINT ( 'NONE', #55080 ) ;
#73713 = ORIENTED_EDGE ( 'NONE', *, *, #107455, .T. ) ;
#73714 = DIRECTION ( 'NONE',  ( 0.000000000000000000, 1.000000000000000000, 0.000000000000000000 ) ) ;
#73715 = DIRECTION ( 'NONE',  ( -0.7071067811865486830, 0.7071067811865464625, 0.000000000000000000 ) ) ;
#73716 = CARTESIAN_POINT ( 'NONE',  ( -25.49999999999982947, -1.592773361805396970, -6.492772025301170480 ) ) ;
#73717 = CARTESIAN_POINT ( 'NONE',  ( 21.18398860626899349, 28.73617430169802134, 5.000000000000000000 ) ) ;
#73718 = CARTESIAN_POINT ( 'NONE',  ( 53.60002705046289151, 5.819803920172570422, 5.819803920172575751 ) ) ;
#73719 = DIRECTION ( 'NONE',  ( 2.781805975412905890E-17, -0.3543493200069152693, 0.9351131265310292928 ) ) ;
#73720 =( LENGTH_UNIT ( ) NAMED_UNIT ( * ) SI_UNIT ( .MILLI., .METRE. ) );
#73721 = ORIENTED_EDGE ( 'NONE', *, *, #29534, .T. ) ;
#73722 = ORIENTED_EDGE ( 'NONE', *, *, #139595, .F. ) ;
#73723 = ORIENTED_EDGE ( 'NONE', *, *, #104776, .T. ) ;
#73724 = ORIENTED_EDGE ( 'NONE', *, *, #96607, .T. ) ;
#73725 = CARTESIAN_POINT ( 'NONE',  ( 3.792893218813436551, 3.759292476615678336, 5.000000000000000000 ) ) ;
#73726 = LINE ( 'NONE', #5593, #140387 ) ;
#73727 = SURFACE_SIDE_STYLE ('',( #37553 ) ) ;
#73728 = VERTEX_POINT ( 'NONE', #52892 ) ;
#73729 = CARTESIAN_POINT ( 'NONE',  ( 69.05836038379621300, -7.949999999999996625, -2.130196079827426203 ) ) ;
#73730 = CARTESIAN_POINT ( 'NONE',  ( 4.566871997512545356, -21.74070752338406365, 6.915939825044062239 ) ) ;
#73732 = EDGE_CURVE ( 'NONE', #56677, #103133, #31188, .T. ) ;
#73731 = DIRECTION ( 'NONE',  ( 1.000000000000000000, -0.000000000000000000, -0.000000000000000000 ) ) ;
#73733 = LINE ( 'NONE', #62889, #97077 ) ;
#73734 = AXIS2_PLACEMENT_3D ( 'NONE', #54169, #98357, #30224 ) ;
#73735 = AXIS2_PLACEMENT_3D ( 'NONE', #103536, #57241, #89823 ) ;
#73736 = CARTESIAN_POINT ( 'NONE',  ( 27.00000000000000355, -4.083527258847093222, -4.862849486279972488 ) ) ;
#73737 = EDGE_LOOP ( 'NONE', ( #99109, #35301, #44538, #73608 ) ) ;
#73738 = CARTESIAN_POINT ( 'NONE',  ( -32.99999999999976552, -0.03360074219774071558, 5.000000000000000000 ) ) ;
#73739 = CARTESIAN_POINT ( 'NONE',  ( 51.74999999999999289, -9.735942053221458872E-16, 7.950000000000000178 ) ) ;
#73740 = VECTOR ( 'NONE', #52321, 999.9999999999998863 ) ;
#73741 = ORIENTED_EDGE ( 'NONE', *, *, #38123, .T. ) ;
#73742 = CARTESIAN_POINT ( 'NONE',  ( 11.99999999999992006, -2.904428200921297609, -6.989807076074969316 ) ) ;
#73743 = ORIENTED_EDGE ( 'NONE', *, *, #131504, .T. ) ;
#73744 = VECTOR ( 'NONE', #4027, 1000.000000000000000 ) ;
#73745 = ADVANCED_FACE ( 'NONE', ( #110140 ), #48908, .T. ) ;
#73746 = EDGE_CURVE ( 'NONE', #1673, #75381, #21034, .T. ) ;
#73747 = DIRECTION ( 'NONE',  ( 0.000000000000000000, -1.000000000000000000, 0.000000000000000000 ) ) ;
#73748 = VERTEX_POINT ( 'NONE', #108691 ) ;
#73749 = CARTESIAN_POINT ( 'NONE',  ( 75.25043019189811844, 3.055000000000002824, -5.291415217122919401 ) ) ;
#73750 = EDGE_LOOP ( 'NONE', ( #71981, #123499, #4003, #28811 ) ) ;
#73751 = ORIENTED_EDGE ( 'NONE', *, *, #109920, .T. ) ;
#73752 = AXIS2_PLACEMENT_3D ( 'NONE', #72373, #29512, #117222 ) ;
#73753 = EDGE_CURVE ( 'NONE', #126258, #31605, #101680, .T. ) ;
#73754 = EDGE_CURVE ( 'NONE', #34379, #50924, #28085, .T. ) ;
#73755 = CARTESIAN_POINT ( 'NONE',  ( -8.994519915287490619, 28.92564299267944250, 4.000000000000000000 ) ) ;
#73757 = EDGE_CURVE ( 'NONE', #135458, #98615, #63121, .T. ) ;
#73756 = CARTESIAN_POINT ( 'NONE',  ( -9.489213562373095101, -27.52281430457062328, 5.000000000000000000 ) ) ;
#73758 = CARTESIAN_POINT ( 'NONE',  ( 112.2920968585647756, -5.291415217122921177, 3.054999999999999272 ) ) ;
#73759 = DIRECTION ( 'NONE',  ( 1.000000000000000000, 0.000000000000000000, 0.000000000000000000 ) ) ;
#73760 = EDGE_CURVE ( 'NONE', #26437, #139716, #130509, .T. ) ;
#73761 = PLANE ( 'NONE',  #102279 ) ;
#73762 = CARTESIAN_POINT ( 'NONE',  ( 11.72733514412567857, -2.500000000000001776, 0.000000000000000000 ) ) ;
#73763 = CARTESIAN_POINT ( 'NONE',  ( -12.78162688292485605, 21.74787736706806385, 4.999607392498049308 ) ) ;
#73764 = CIRCLE ( 'NONE', #8820, 7.950000000000000178 ) ;
#73765 = EDGE_CURVE ( 'NONE', #123337, #64814, #30467, .T. ) ;
#73766 = DIRECTION ( 'NONE',  ( -1.000000000000000000, -0.000000000000000000, -0.000000000000000000 ) ) ;
#73767 = CARTESIAN_POINT ( 'NONE',  ( 35.52487387214932113, 14.25929247661557220, 9.797011795316720395 ) ) ;
#73768 = DIRECTION ( 'NONE',  ( -0.7071067811865486830, -0.7071067811865464625, 0.000000000000000000 ) ) ;
#73769 = EDGE_CURVE ( 'NONE', #71410, #7557, #74707, .T. ) ;
#73770 = ORIENTED_EDGE ( 'NONE', *, *, #51218, .F. ) ;
#73771 = VECTOR ( 'NONE', #24968, 1000.000000000000000 ) ;
#73772 = DIRECTION ( 'NONE',  ( 1.000000000000000000, 0.000000000000000000, 0.000000000000000000 ) ) ;
#73773 = VERTEX_POINT ( 'NONE', #98564 ) ;
#73774 = ORIENTED_EDGE ( 'NONE', *, *, #132289, .T. ) ;
#73775 = ORIENTED_EDGE ( 'NONE', *, *, #52204, .T. ) ;
#73776 = CIRCLE ( 'NONE', #122283, 2.055000000000001048 ) ;
#73777 = VERTEX_POINT ( 'NONE', #142790 ) ;
#73778 = VECTOR ( 'NONE', #45848, 999.9999999999998863 ) ;
#73779 = CARTESIAN_POINT ( 'NONE',  ( 153.4000000000000057, -16.48000000000005016, -33.92499999999998295 ) ) ;
#73780 = CARTESIAN_POINT ( 'NONE',  ( -0.7928932188134476533, -5.240707523384234179, 5.000000000000000000 ) ) ;
#73781 = EDGE_CURVE ( 'NONE', #138304, #99771, #43482, .T. ) ;
#73782 = PRESENTATION_LAYER_ASSIGNMENT (  '', '', ( #83004 ) ) ;
#73783 = CARTESIAN_POINT ( 'NONE',  ( 12.19999999999999574, -28.33999999999998565, 13.17925390838734323 ) ) ;
#73784 = VERTEX_POINT ( 'NONE', #7967 ) ;
#73785 = CARTESIAN_POINT ( 'NONE',  ( 3.483440076894412041, -49.11775834062188295, 40.20665288735688137 ) ) ;
#73786 = ORIENTED_EDGE ( 'NONE', *, *, #136312, .T. ) ;
#73787 = AXIS2_PLACEMENT_3D ( 'NONE', #62985, #62256, #73144 ) ;
#73788 = EDGE_CURVE ( 'NONE', #86643, #398, #90407, .T. ) ;
#73789 = AXIS2_PLACEMENT_3D ( 'NONE', #101385, #44171, #23835 ) ;
#73790 = CARTESIAN_POINT ( 'NONE',  ( 2.603736474768552522, 5.808823158059036373, 5.808823158059032821 ) ) ;
#73791 = CARTESIAN_POINT ( 'NONE',  ( 34.75611968250419181, -15.18706574529245046, 4.955485411084878500 ) ) ;
#73792 = FACE_OUTER_BOUND ( 'NONE', #137552, .T. ) ;
#73793 = DIRECTION ( 'NONE',  ( -0.7071067811865487940, 0.7071067811865463515, 0.000000000000000000 ) ) ;
#73794 = EDGE_LOOP ( 'NONE', ( #80844, #45383, #141705, #73415 ) ) ;
#73795 = EDGE_LOOP ( 'NONE', ( #12958, #13770, #136001, #103801 ) ) ;
#73796 = ORIENTED_EDGE ( 'NONE', *, *, #12866, .F. ) ;
#73797 = CARTESIAN_POINT ( 'NONE',  ( -54.29974487139159578, -27.71228299555243879, 4.000000000000000000 ) ) ;
#73798 = CARTESIAN_POINT ( 'NONE',  ( 0.000000000000000000, 0.000000000000000000, 5.000000000000000000 ) ) ;
#73800 = VECTOR ( 'NONE', #25648, 1000.000000000000000 ) ;
#73799 = CARTESIAN_POINT ( 'NONE',  ( -5.292893218813416567, -0.7407075233842753681, 5.000000000000000000 ) ) ;
#73801 = CARTESIAN_POINT ( 'NONE',  ( 3.707106781186525257, 2.259292476615692546, 5.000000000000000000 ) ) ;
#73802 = CARTESIAN_POINT ( 'NONE',  ( -6.005480084712508493, 28.92564299267933947, 4.000000000000000000 ) ) ;
#73803 = FACE_OUTER_BOUND ( 'NONE', #29943, .T. ) ;
#73804 = CARTESIAN_POINT ( 'NONE',  ( 10.58990935480161610, 9.759292476615618384, 11.28811694763781226 ) ) ;
#73805 = ADVANCED_FACE ( 'NONE', ( #121729 ), #76111, .T. ) ;
#73806 = CARTESIAN_POINT ( 'NONE',  ( -31.49999999999977973, 9.431123077392092213, 4.000000000000000000 ) ) ;
#73807 = CARTESIAN_POINT ( 'NONE',  ( 32.08376352523143993, -6.110000000000001208, -3.741295971395164515E-16 ) ) ;
#73808 = CARTESIAN_POINT ( 'NONE',  ( -12.71230993966019618, -21.73547319004781642, 4.999917730833664642 ) ) ;
#73809 = CARTESIAN_POINT ( 'NONE',  ( 13.60986171580761805, 4.202752102959690472E-16, 0.000000000000000000 ) ) ;
#73810 = ADVANCED_FACE ( 'NONE', ( #143493 ), #52208, .F. ) ;
#73811 = VERTEX_POINT ( 'NONE', #140633 ) ;
#73812 = CARTESIAN_POINT ( 'NONE',  ( -31.49999999999977973, -15.29013452822857388, 0.3645803511609629344 ) ) ;
#73813 = CARTESIAN_POINT ( 'NONE',  ( -13.83673880763391217, -22.22500000000000142, -2.991130486387429510 ) ) ;
#73814 = EDGE_LOOP ( 'NONE', ( #96309, #21666, #122468, #45573 ) ) ;
#73815 = ADVANCED_FACE ( 'NONE', ( #118888 ), #19577, .F. ) ;
#73816 = CARTESIAN_POINT ( 'NONE',  ( 26.40000000000000568, -16.48000000000005016, 33.92499999999998295 ) ) ;
#73818 = ORIENTED_EDGE ( 'NONE', *, *, #15510, .F. ) ;
#73817 = FACE_OUTER_BOUND ( 'NONE', #97585, .T. ) ;
#73819 = DIRECTION ( 'NONE',  ( 0.7071067811865486830, -0.7071067811865464625, -0.000000000000000000 ) ) ;
#73820 = CARTESIAN_POINT ( 'NONE',  ( -59.99451991528749772, 28.92564299267980132, 4.000000000000000000 ) ) ;
#73821 = EDGE_LOOP ( 'NONE', ( #115691, #5809, #35528, #132040 ) ) ;
#73822 = CARTESIAN_POINT ( 'NONE',  ( 5.293876922608006019, 22.22500000000000142, 4.000000000000000000 ) ) ;
#73823 = UNCERTAINTY_MEASURE_WITH_UNIT (LENGTH_MEASURE( 1.000000000000000082E-05 ), #40008, 'distance_accuracy_value', 'NONE');
#73824 = VERTEX_POINT ( 'NONE', #36866 ) ;
#73825 = FILL_AREA_STYLE ('',( #29588 ) ) ;
#73826 = CARTESIAN_POINT ( 'NONE',  ( 120.2458603837962272, 3.974999999999996980, 6.884901960086287964 ) ) ;
#73827 = DIRECTION ( 'NONE',  ( -0.000000000000000000, 0.3543493200069153248, 0.9351131265310292928 ) ) ;
#73828 = PLANE ( 'NONE',  #108393 ) ;
#73829 = ADVANCED_FACE ( 'NONE', ( #58698 ), #91295, .F. ) ;
#73830 = DIRECTION ( 'NONE',  ( -1.000000000000000000, -0.000000000000000000, -0.000000000000000000 ) ) ;
#73831 =( NAMED_UNIT ( * ) PLANE_ANGLE_UNIT ( ) SI_UNIT ( $, .RADIAN. ) );
#73832 = DIRECTION ( 'NONE',  ( 0.7071067811865487940, 0.7071067811865463515, -0.000000000000000000 ) ) ;
#73833 = CARTESIAN_POINT ( 'NONE',  ( 4.958333333333333925, -3.047499999999997211, -5.278424836066143655 ) ) ;
#73834 = CARTESIAN_POINT ( 'NONE',  ( 5.666236474768552078, 7.934999999999990727, -1.457635852685135314E-15 ) ) ;
#73835 = CARTESIAN_POINT ( 'NONE',  ( 10.17183060077640100, 21.75929247661550647, 4.000000000000000000 ) ) ;
#73836 = DIRECTION ( 'NONE',  ( -0.6830127018922180770, -0.6830127018922204085, -0.2588190451025213501 ) ) ;
#73837 = ORIENTED_EDGE ( 'NONE', *, *, #48164, .T. ) ;
#73838 = ORIENTED_EDGE ( 'NONE', *, *, #88418, .T. ) ;
#73839 = CARTESIAN_POINT ( 'NONE',  ( 86.60416666666664298, 2.130196079827422206, 7.950000000000001954 ) ) ;
#73840 = CARTESIAN_POINT ( 'NONE',  ( -72.29974487139158157, -27.71228299555256669, 4.000000000000000000 ) ) ;
#73841 = VERTEX_POINT ( 'NONE', #123201 ) ;
#73842 = EDGE_CURVE ( 'NONE', #68263, #113749, #14417, .T. ) ;
#73843 = CARTESIAN_POINT ( 'NONE',  ( -8.999999999999932498, -13.44781430457069504, 5.000000000000000000 ) ) ;
#73844 = CARTESIAN_POINT ( 'NONE',  ( 0.7928932188134442116, 12.75929247661559529, 5.000000000000000000 ) ) ;
#73845 =( NAMED_UNIT ( * ) PLANE_ANGLE_UNIT ( ) SI_UNIT ( $, .RADIAN. ) );
#73846 = CIRCLE ( 'NONE', #59993, 2.055000000000000604 ) ;
#73847 = CARTESIAN_POINT ( 'NONE',  ( 31.28752705046289151, 0.000000000000000000, -7.949999999999998401 ) ) ;
#73848 = ORIENTED_EDGE ( 'NONE', *, *, #74720, .T. ) ;
#73849 = VECTOR ( 'NONE', #59848, 1000.000000000000227 ) ;
#73850 = VECTOR ( 'NONE', #133194, 1000.000000000000227 ) ;
#73851 = VECTOR ( 'NONE', #32338, 999.9999999999998863 ) ;
#73852 = LINE ( 'NONE', #93466, #139105 ) ;
#73853 = VECTOR ( 'NONE', #94923, 999.9999999999998863 ) ;
#73854 = CARTESIAN_POINT ( 'NONE',  ( 29.20666063542132207, 21.75929247661549581, 4.998822639870703632 ) ) ;
#73855 = LINE ( 'NONE', #85418, #125248 ) ;
#73856 = EDGE_CURVE ( 'NONE', #76474, #10908, #35826, .T. ) ;
#73857 = CARTESIAN_POINT ( 'NONE',  ( 3.289788898235945780, -22.22500000000000142, 19.48101205736676889 ) ) ;
#73859 = ORIENTED_EDGE ( 'NONE', *, *, #107376, .T. ) ;
#73858 = CARTESIAN_POINT ( 'NONE',  ( -24.18398860626899705, 28.73617430169804265, 5.000000000000000000 ) ) ;
#73860 = DIRECTION ( 'NONE',  ( 1.000000000000000000, 0.000000000000000000, 0.000000000000000000 ) ) ;
#73861 = DIRECTION ( 'NONE',  ( 0.000000000000000000, 0.000000000000000000, 1.000000000000000000 ) ) ;
#73862 = CARTESIAN_POINT ( 'NONE',  ( 24.18398860626899705, 28.73617430169804265, 5.000000000000000000 ) ) ;
#73863 = CARTESIAN_POINT ( 'NONE',  ( 7.499999999999950262, 18.05218569542898877, 5.000000000000000000 ) ) ;
#73864 = LINE ( 'NONE', #118037, #121661 ) ;
#73865 = CARTESIAN_POINT ( 'NONE',  ( -78.18398860626899705, 28.73617430169841924, 5.000000000000000000 ) ) ;
#73866 = EDGE_LOOP ( 'NONE', ( #135526, #20759, #26090, #142750 ) ) ;
#73867 = VERTEX_POINT ( 'NONE', #135499 ) ;
#73868 = CARTESIAN_POINT ( 'NONE',  ( 104.2712635252314470, 4.472830434245839371, 4.472830434245842035 ) ) ;
#73869 =( BOUNDED_CURVE ( )  B_SPLINE_CURVE ( 3, ( #55741, #91241, #609, #124551 ),
 .UNSPECIFIED., .F., .T. ) 
 B_SPLINE_CURVE_WITH_KNOTS ( ( 4, 4 ),
 ( 5.106027341939269881, 6.645403452391244414 ),
 .UNSPECIFIED. ) 
 CURVE ( )  GEOMETRIC_REPRESENTATION_ITEM ( )  RATIONAL_B_SPLINE_CURVE ( ( 1.000000000000000000, 0.8120851936182256203, 0.8120851936182256203, 1.000000000000000000 ) ) 
 REPRESENTATION_ITEM ( '' )  );
#73870 = ORIENTED_EDGE ( 'NONE', *, *, #43692, .T. ) ;
#73871 = DIRECTION ( 'NONE',  ( 0.5735764363510444941, 0.8191520442889929088, 0.000000000000000000 ) ) ;
#73872 = VECTOR ( 'NONE', #107323, 999.9999999999998863 ) ;
#73873 = CARTESIAN_POINT ( 'NONE',  ( 8.750000000000000000, -7.464222240803106570E-16, -6.094999999999989981 ) ) ;
#73874 = ORIENTED_EDGE ( 'NONE', *, *, #86436, .F. ) ;
#73875 = DIRECTION ( 'NONE',  ( 0.7071067811865487940, 0.7071067811865463515, -0.000000000000000000 ) ) ;
#73877 = ADVANCED_FACE ( 'NONE', ( #89824 ), #134067, .F. ) ;
#73876 = DIRECTION ( 'NONE',  ( 0.000000000000000000, -1.000000000000000000, 0.000000000000000000 ) ) ;
#73878 = VECTOR ( 'NONE', #105389, 999.9999999999998863 ) ;
#73879 = CARTESIAN_POINT ( 'NONE',  ( 99.51626352523145158, -4.472830434245839371, 4.472830434245839371 ) ) ;
#73880 = EDGE_CURVE ( 'NONE', #41017, #54692, #13668, .T. ) ;
#73881 = ORIENTED_EDGE ( 'NONE', *, *, #28888, .F. ) ;
#73882 = FACE_OUTER_BOUND ( 'NONE', #4351, .T. ) ;
#73883 = ORIENTED_EDGE ( 'NONE', *, *, #43906, .F. ) ;
#73884 = CARTESIAN_POINT ( 'NONE',  ( 12.48921356237309155, -27.52281430457064104, 5.000000000000000000 ) ) ;
#73885 = CARTESIAN_POINT ( 'NONE',  ( -75.48921356237309510, -27.52281430457107803, 5.000000000000000000 ) ) ;
#73886 = VECTOR ( 'NONE', #37330, 1000.000000000000000 ) ;
#73887 = CARTESIAN_POINT ( 'NONE',  ( 75.18398860626899705, 28.73617430169839793, 5.000000000000000000 ) ) ;
#73888 = COLOUR_RGB ( '', 0.09019608, 0.27058824, 0.51372549) ;
#73889 = EDGE_LOOP ( 'NONE', ( #112388, #79715 ) ) ;
#73890 = ORIENTED_EDGE ( 'NONE', *, *, #120485, .T. ) ;
#73891 = ORIENTED_EDGE ( 'NONE', *, *, #23596, .F. ) ;
#73892 = FACE_OUTER_BOUND ( 'NONE', #131772, .T. ) ;
#73893 = ADVANCED_FACE ( 'NONE', ( #12966 ), #34755, .F. ) ;
#73894 = LINE ( 'NONE', #106474, #10583 ) ;
#73895 = CARTESIAN_POINT ( 'NONE',  ( 11.00456980810188590, 6.871911579029510442, -3.967499999999998916 ) ) ;
#73896 = VECTOR ( 'NONE', #30149, 1000.000000000000000 ) ;
#73897 = CONICAL_SURFACE ( 'NONE', #11341, 2.055000000000001048, 0.9599310885968758145 ) ;
#73898 = CARTESIAN_POINT ( 'NONE',  ( 21.87500000000000355, -6.094999999999989981, 3.732111120401553285E-16 ) ) ;
#73899 = ORIENTED_EDGE ( 'NONE', *, *, #17194, .F. ) ;
#73900 = ORIENTED_EDGE ( 'NONE', *, *, #117140, .T. ) ;
#73901 = FACE_OUTER_BOUND ( 'NONE', #106050, .T. ) ;
#73902 = ORIENTED_EDGE ( 'NONE', *, *, #107225, .F. ) ;
#73903 = EDGE_LOOP ( 'NONE', ( #126450, #50658, #90927, #90763 ) ) ;
#73904 = VECTOR ( 'NONE', #111030, 999.9999999999998863 ) ;
#73905 = FACE_OUTER_BOUND ( 'NONE', #103681, .T. ) ;
#73906 = CARTESIAN_POINT ( 'NONE',  ( 4.499999999999979572, 4.466399257802216027, 5.000000000000000000 ) ) ;
#73907 = ORIENTED_EDGE ( 'NONE', *, *, #95673, .F. ) ;
#73908 = CARTESIAN_POINT ( 'NONE',  ( 7.000000000000000888, 0.000000000000000000, 6.094999999999989981 ) ) ;
#73909 = ADVANCED_FACE ( 'NONE', ( #57242 ), #2067, .T. ) ;
#73910 = DIRECTION ( 'NONE',  ( 0.7071067811865487940, 0.7071067811865463515, 0.000000000000000000 ) ) ;
#73911 = CARTESIAN_POINT ( 'NONE',  ( -23.29289321881329045, 14.25929247661557042, 5.000000000000000000 ) ) ;
#73912 = CARTESIAN_POINT ( 'NONE',  ( 5.281315875828549444, 4.584330080086930965E-16, 0.000000000000000000 ) ) ;
#73913 = ORIENTED_EDGE ( 'NONE', *, *, #94539, .T. ) ;
#73914 = CARTESIAN_POINT ( 'NONE',  ( 33.29974487139158867, -27.71228299555229313, 4.000000000000000000 ) ) ;
#73915 = PLANE ( 'NONE',  #70862 ) ;
#73916 = ORIENTED_EDGE ( 'NONE', *, *, #124857, .T. ) ;
#73917 = FACE_OUTER_BOUND ( 'NONE', #112356, .T. ) ;
#73918 = FACE_OUTER_BOUND ( 'NONE', #96810, .T. ) ;
#73919 = CARTESIAN_POINT ( 'NONE',  ( -25.49999999999982236, -13.53360074219759746, 5.000000000000000000 ) ) ;
#73921 = VERTEX_POINT ( 'NONE', #66670 ) ;
#73920 = EDGE_CURVE ( 'NONE', #93975, #126820, #131319, .T. ) ;
#73922 = DIRECTION ( 'NONE',  ( 0.000000000000000000, 0.000000000000000000, 1.000000000000000000 ) ) ;
#73923 = ORIENTED_EDGE ( 'NONE', *, *, #50054, .F. ) ;
#73924 = EDGE_LOOP ( 'NONE', ( #84797, #95183, #60703, #138525 ) ) ;
#73925 = VERTEX_POINT ( 'NONE', #46379 ) ;
#73926 =( BOUNDED_CURVE ( )  B_SPLINE_CURVE ( 2, ( #89810, #656, #78251, #34740, #33346, #76839, #112302, #121012, #99236, #44197, #77547, #22389, #122432 ),
 .UNSPECIFIED., .F., .T. ) 
 B_SPLINE_CURVE_WITH_KNOTS ( ( 3, 2, 2, 2, 2, 2, 3 ),
 ( 0.2000000000000000111, 0.2027777777777777790, 0.2055555555555555469, 0.2083333333333333426, 0.2111111111111111105, 0.2138888888888888784, 0.2166666666666666741 ),
 .UNSPECIFIED. ) 
 CURVE ( )  GEOMETRIC_REPRESENTATION_ITEM ( )  RATIONAL_B_SPLINE_CURVE ( ( 1.000000000000000000, 0.9659258262890683122, 1.000000000000000000, 0.9659258262890683122, 1.000000000000000000, 0.9659258262890683122, 1.000000000000000000, 0.9659258262890683122, 1.000000000000000000, 0.9659258262890683122, 1.000000000000000000, 0.9659258262890683122, 1.000000000000000000 ) ) 
 REPRESENTATION_ITEM ( '' )  );
#73927 = ADVANCED_FACE ( 'NONE', ( #79731 ), #68827, .F. ) ;
#73928 = CARTESIAN_POINT ( 'NONE',  ( 30.82876352523145158, 0.000000000000000000, -6.109999999999998543 ) ) ;
#73929 = DIRECTION ( 'NONE',  ( -0.7071067811865487940, 0.7071067811865463515, 0.000000000000000000 ) ) ;
#73931 = EDGE_CURVE ( 'NONE', #6272, #122150, #25278, .T. ) ;
#73930 = CARTESIAN_POINT ( 'NONE',  ( 42.18398860626899705, 28.73617430169816700, 5.000000000000000000 ) ) ;
#73932 = DIRECTION ( 'NONE',  ( -0.7071067811865487940, 0.7071067811865463515, 0.000000000000000000 ) ) ;
#73933 = EDGE_CURVE ( 'NONE', #141351, #6455, #55804, .T. ) ;
#73934 = DIRECTION ( 'NONE',  ( 0.6830127018922181881, 0.6830127018922202975, -0.2588190451025214056 ) ) ;
#73935 = LINE ( 'NONE', #118112, #36627 ) ;
#73936 = EDGE_CURVE ( 'NONE', #126961, #68281, #100007, .T. ) ;
#73937 = PLANE ( 'NONE',  #111737 ) ;
#73938 = LINE ( 'NONE', #74677, #22726 ) ;
#73939 = DIRECTION ( 'NONE',  ( -0.000000000000000000, 0.3543493200069153248, 0.9351131265310292928 ) ) ;
#73940 = LINE ( 'NONE', #86259, #84101 ) ;
#73941 = EDGE_CURVE ( 'NONE', #59938, #137008, #104443, .T. ) ;
#73942 = ORIENTED_EDGE ( 'NONE', *, *, #51404, .T. ) ;
#73943 = VERTEX_POINT ( 'NONE', #49211 ) ;
#73944 = ORIENTED_EDGE ( 'NONE', *, *, #117786, .F. ) ;
#73945 = ORIENTED_EDGE ( 'NONE', *, *, #54447, .T. ) ;
#73946 = CARTESIAN_POINT ( 'NONE',  ( 31.49999999999978684, -8.947814304570730570, 5.000000000000000000 ) ) ;
#73947 = CONICAL_SURFACE ( 'NONE', #136443, 2.500000000000000444, 0.9599310885968830309 ) ;
#73948 = VECTOR ( 'NONE', #14059, 1000.000000000000227 ) ;
#73949 = ORIENTED_EDGE ( 'NONE', *, *, #64241, .T. ) ;
#73950 = CIRCLE ( 'NONE', #80895, 0.5000000000000004441 ) ;
#73952 = ORIENTED_EDGE ( 'NONE', *, *, #69714, .F. ) ;
#73951 = VECTOR ( 'NONE', #117213, 1000.000000000000114 ) ;
#73953 = PLANE ( 'NONE',  #118559 ) ;
#73954 = CARTESIAN_POINT ( 'NONE',  ( 60.18398860626900415, 28.73617430169829490, 5.000000000000000000 ) ) ;
#73955 = EDGE_CURVE ( 'NONE', #80026, #94676, #106374, .T. ) ;
#73956 = EDGE_CURVE ( 'NONE', #59180, #1974, #40474, .T. ) ;
#73957 = CARTESIAN_POINT ( 'NONE',  ( 32.20710678118632586, 18.75929247661552424, 5.000000000000000000 ) ) ;
#73958 = EDGE_LOOP ( 'NONE', ( #122550, #102346, #6604 ) ) ;
#73959 = CARTESIAN_POINT ( 'NONE',  ( 2.999999999999975131, -7.068876922607738145, 4.000000000000000000 ) ) ;
#73961 = ORIENTED_EDGE ( 'NONE', *, *, #79285, .T. ) ;
#73960 = VECTOR ( 'NONE', #22438, 1000.000000000000227 ) ;
#73962 = ADVANCED_FACE ( 'NONE', ( #71661 ), #81854, .F. ) ;
#73963 = DIRECTION ( 'NONE',  ( -0.7071067811865486830, -0.7071067811865464625, -0.000000000000000000 ) ) ;
#73964 = DIRECTION ( 'NONE',  ( 0.000000000000000000, 0.000000000000000000, -1.000000000000000000 ) ) ;
#73965 = CARTESIAN_POINT ( 'NONE',  ( 6.483736474768551972, -5.808823158059035485, -5.808823158059033709 ) ) ;
#73966 = EDGE_LOOP ( 'NONE', ( #1217, #140637, #40135, #87998 ) ) ;
#73967 = CARTESIAN_POINT ( 'NONE',  ( 94.26626352523143737, 4.472830434245839371, -4.472830434245839371 ) ) ;
#73968 = CARTESIAN_POINT ( 'NONE',  ( -59.99451991528749772, 28.92564299267980132, 4.000000000000000000 ) ) ;
#73969 = CARTESIAN_POINT ( 'NONE',  ( -36.48921356237310221, -27.52281430457080802, 5.000000000000000000 ) ) ;
#73970 = PLANE ( 'NONE',  #141509 ) ;
#73971 = VERTEX_POINT ( 'NONE', #105675 ) ;
#73972 = ORIENTED_EDGE ( 'NONE', *, *, #83420, .T. ) ;
#73973 = DIRECTION ( 'NONE',  ( -0.5150380749100710309, 0.000000000000000000, 0.8571673007021021196 ) ) ;
#73974 = ORIENTED_EDGE ( 'NONE', *, *, #122041, .F. ) ;
#73975 = DIRECTION ( 'NONE',  ( -0.6830127018922180770, -0.6830127018922204085, -0.2588190451025213501 ) ) ;
#73977 = DIRECTION ( 'NONE',  ( 0.000000000000000000, 0.000000000000000000, 1.000000000000000000 ) ) ;
#73976 = VECTOR ( 'NONE', #47460, 1000.000000000000000 ) ;
#73978 = CARTESIAN_POINT ( 'NONE',  ( -34.42500000000001137, -13.45860074219784863, 5.000000000000000000 ) ) ;
#73979 = CARTESIAN_POINT ( 'NONE',  ( -26.99999999999980815, -4.068876922607768343, 4.000000000000000000 ) ) ;
#73980 = VERTEX_POINT ( 'NONE', #7057 ) ;
#73981 = PLANE ( 'NONE',  #11394 ) ;
#73982 = CONICAL_SURFACE ( 'NONE', #134210, 7.950000000000000178, 0.7853981633974396193 ) ;
#73983 = DIRECTION ( 'NONE',  ( -0.7071067811865487940, 0.7071067811865463515, -0.000000000000000000 ) ) ;
#73984 = FACE_OUTER_BOUND ( 'NONE', #104349, .T. ) ;
#73985 = ADVANCED_FACE ( 'NONE', ( #115827 ), #137640, .F. ) ;
#73986 = VERTEX_POINT ( 'NONE', #138340 ) ;
#73987 = CARTESIAN_POINT ( 'NONE',  ( 0.000000000000000000, 0.000000000000000000, 5.000000000000000000 ) ) ;
#73988 = AXIS2_PLACEMENT_3D ( 'NONE', #5912, #72693, #114003 ) ;
#73989 = DIRECTION ( 'NONE',  ( -0.7071067811865486830, -0.7071067811865464625, 0.000000000000000000 ) ) ;
#73990 = ORIENTED_EDGE ( 'NONE', *, *, #138720, .F. ) ;
#73991 = AXIS2_PLACEMENT_3D ( 'NONE', #110518, #132336, #56216 ) ;
#73993 = ORIENTED_EDGE ( 'NONE', *, *, #24952, .T. ) ;
#73992 = DIRECTION ( 'NONE',  ( -0.000000000000000000, 0.3543493200069153248, 0.9351131265310292928 ) ) ;
#73994 = ORIENTED_EDGE ( 'NONE', *, *, #110496, .F. ) ;
#73995 = AXIS2_PLACEMENT_3D ( 'NONE', #16057, #6600, #104534 ) ;
#73996 = CARTESIAN_POINT ( 'NONE',  ( 5.999999999999960032, 11.96639925780213964, 5.000000000000000000 ) ) ;
#73997 = AXIS2_PLACEMENT_3D ( 'NONE', #20510, #87231, #74216 ) ;
#73998 = PLANE ( 'NONE',  #15973 ) ;
#73999 = ORIENTED_EDGE ( 'NONE', *, *, #112961, .F. ) ;
#74000 = DIRECTION ( 'NONE',  ( 0.000000000000000000, 0.000000000000000000, 1.000000000000000000 ) ) ;
#74001 = EDGE_CURVE ( 'NONE', #103751, #123300, #59382, .T. ) ;
#74002 = PLANE ( 'NONE',  #49863 ) ;
#74003 = CARTESIAN_POINT ( 'NONE',  ( 28.49999999999980105, 19.39370406404969671, 1.459788787078136307 ) ) ;
#74004 = DIRECTION ( 'NONE',  ( -0.7071067811865487940, 0.7071067811865463515, 0.000000000000000000 ) ) ;
#74005 = DIRECTION ( 'NONE',  ( -1.000000000000000000, -1.224606353822377258E-16, -0.000000000000000000 ) ) ;
#74006 = EDGE_CURVE ( 'NONE', #91203, #6385, #5650, .T. ) ;
#74007 = CARTESIAN_POINT ( 'NONE',  ( 3.354166666666667407, 1.633150327867690432, 6.094999999999991758 ) ) ;
#74008 = CARTESIAN_POINT ( 'NONE',  ( 48.10416666666665009, 2.130196079827422206, 7.950000000000001954 ) ) ;
#74009 = LINE ( 'NONE', #8005, #125294 ) ;
#74011 = CONICAL_SURFACE ( 'NONE', #39359, 2.500000000000000444, 0.9599310885968830309 ) ;
#74010 = LINE ( 'NONE', #21031, #36411 ) ;
#74012 = LINE ( 'NONE', #71893, #18844 ) ;
#74013 = LINE ( 'NONE', #142834, #13623 ) ;
#74014 = CARTESIAN_POINT ( 'NONE',  ( 17.12514619309224173, -14.24070752338413293, 9.401115078912619438 ) ) ;
#74015 = CARTESIAN_POINT ( 'NONE',  ( 11.99999999999992717, -4.447814304570779420, 5.000000000000000000 ) ) ;
#74016 = VERTEX_POINT ( 'NONE', #94797 ) ;
#74017 = ORIENTED_EDGE ( 'NONE', *, *, #9084, .F. ) ;
#74018 = ORIENTED_EDGE ( 'NONE', *, *, #120169, .T. ) ;
#74019 = CARTESIAN_POINT ( 'NONE',  ( 106.8750000000000000, 7.950000000000000178, 1.460391307983218535E-15 ) ) ;
#74020 = ORIENTED_EDGE ( 'NONE', *, *, #118482, .F. ) ;
#74021 = VERTEX_POINT ( 'NONE', #39762 ) ;
#74022 = ADVANCED_FACE ( 'NONE', ( #51339 ), #4177, .F. ) ;
#74023 = ORIENTED_EDGE ( 'NONE', *, *, #114060, .F. ) ;
#74024 = CARTESIAN_POINT ( 'NONE',  ( 0.000000000000000000, 0.000000000000000000, 5.000000000000000000 ) ) ;
#74025 = CARTESIAN_POINT ( 'NONE',  ( 34.92382263987068569, 21.75929247661549937, 4.252424926123345550 ) ) ;
#74026 = ORIENTED_EDGE ( 'NONE', *, *, #100282, .T. ) ;
#74027 = LINE ( 'NONE', #117494, #53165 ) ;
#74028 = DIRECTION ( 'NONE',  ( -0.3543493200069162685, -0.000000000000000000, -0.9351131265310288487 ) ) ;
#74029 = DIRECTION ( 'NONE',  ( -1.000000000000000000, -1.224606353822377258E-16, -0.000000000000000000 ) ) ;
#74030 = LINE ( 'NONE', #72648, #120666 ) ;
#74031 = CARTESIAN_POINT ( 'NONE',  ( 103.5420968585647756, 5.291415217122923842, -3.054999999999996163 ) ) ;
#74032 = EDGE_CURVE ( 'NONE', #127835, #18455, #47395, .T. ) ;
#74033 = EDGE_LOOP ( 'NONE', ( #72252, #7385, #108218, #39272, #89552 ) ) ;
#74034 = DIRECTION ( 'NONE',  ( -0.7071067811865487940, 0.7071067811865463515, -0.000000000000000000 ) ) ;
#74035 = DIRECTION ( 'NONE',  ( 0.7071067811865486830, -0.7071067811865464625, -0.000000000000000000 ) ) ;
#74036 = FACE_OUTER_BOUND ( 'NONE', #59883, .T. ) ;
#74037 = DIRECTION ( 'NONE',  ( -0.7071067811865486830, 0.7071067811865464625, 0.000000000000000000 ) ) ;
#74038 = CYLINDRICAL_SURFACE ( 'NONE', #22210, 1.000000000000000888 ) ;
#74039 = DIRECTION ( 'NONE',  ( 1.000000000000000000, 0.000000000000000000, 0.000000000000000000 ) ) ;
#74040 = CARTESIAN_POINT ( 'NONE',  ( -18.48921356237309510, -27.52281430457068367, 5.000000000000000000 ) ) ;
#74041 = CARTESIAN_POINT ( 'NONE',  ( -32.99999999999976552, -7.447814304570749222, 5.000000000000000000 ) ) ;
#74042 = VERTEX_POINT ( 'NONE', #99081 ) ;
#74043 = VERTEX_POINT ( 'NONE', #131036 ) ;
#74044 = CARTESIAN_POINT ( 'NONE',  ( 125.8545968585647756, -1.637169565754161615, 6.110000000000000320 ) ) ;
#74045 = ORIENTED_EDGE ( 'NONE', *, *, #92402, .T. ) ;
#74046 = LINE ( 'NONE', #31966, #37038 ) ;
#74047 = LINE ( 'NONE', #21077, #124205 ) ;
#74048 = FACE_OUTER_BOUND ( 'NONE', #70325, .T. ) ;
#74049 = CARTESIAN_POINT ( 'NONE',  ( 57.18398860626899705, 28.73617430169827358, 5.000000000000000000 ) ) ;
#74050 = DIRECTION ( 'NONE',  ( 0.000000000000000000, 0.000000000000000000, -1.000000000000000000 ) ) ;
#74051 = DIRECTION ( 'NONE',  ( 1.000000000000000000, 0.000000000000000000, 0.000000000000000000 ) ) ;
#74052 = CARTESIAN_POINT ( 'NONE',  ( 121.0995968585647660, -6.109999999999997655, -1.637169565754160283 ) ) ;
#74053 = EDGE_CURVE ( 'NONE', #53831, #27000, #53470, .T. ) ;
#74054 = EDGE_LOOP ( 'NONE', ( #67176, #58871, #37466, #1967 ) ) ;
#74055 = LINE ( 'NONE', #16818, #20146 ) ;
#74056 = VERTEX_POINT ( 'NONE', #32437 ) ;
#74057 = PLANE ( 'NONE',  #48537 ) ;
#74058 = VECTOR ( 'NONE', #107456, 999.9999999999998863 ) ;
#74059 = VECTOR ( 'NONE', #123743, 1000.000000000000000 ) ;
#74060 = VECTOR ( 'NONE', #89302, 1000.000000000000000 ) ;
#74061 = DIRECTION ( 'NONE',  ( -0.7071067811865487940, 0.7071067811865463515, -0.000000000000000000 ) ) ;
#74062 = FILL_AREA_STYLE_COLOUR ( '', #35176 ) ;
#74063 = VECTOR ( 'NONE', #74119, 999.9999999999998863 ) ;
#74064 = CARTESIAN_POINT ( 'NONE',  ( 30.29974487139158867, -27.71228299555227537, 4.000000000000000000 ) ) ;
#74065 = VERTEX_POINT ( 'NONE', #120849 ) ;
#74066 = CARTESIAN_POINT ( 'NONE',  ( 41.41709685856477563, 3.054999999999998828, 5.291415217122922066 ) ) ;
#74067 = ORIENTED_EDGE ( 'NONE', *, *, #51089, .F. ) ;
#74068 = FACE_OUTER_BOUND ( 'NONE', #95153, .T. ) ;
#74069 = EDGE_CURVE ( 'NONE', #9302, #63481, #128875, .T. ) ;
#74070 = CARTESIAN_POINT ( 'NONE',  ( 44.99451991528749772, 28.92564299267969474, 4.000000000000000000 ) ) ;
#74071 = PLANE ( 'NONE',  #115011 ) ;
#74072 = LINE ( 'NONE', #100105, #29842 ) ;
#74073 = AXIS2_PLACEMENT_3D ( 'NONE', #14092, #74029, #94339 ) ;
#74074 = PRODUCT_RELATED_PRODUCT_CATEGORY ( 'part', '', ( #56020 ) ) ;
#74075 = CARTESIAN_POINT ( 'NONE',  ( 39.57876352523144448, -7.482591942790325086E-16, 6.109999999999998543 ) ) ;
#74076 = ORIENTED_EDGE ( 'NONE', *, *, #14860, .F. ) ;
#74077 = CYLINDRICAL_SURFACE ( 'NONE', #138239, 1.898649999999994842 ) ;
#74078 = VERTEX_POINT ( 'NONE', #63658 ) ;
#74079 = ORIENTED_EDGE ( 'NONE', *, *, #131313, .F. ) ;
#74080 = AXIS2_PLACEMENT_3D ( 'NONE', #74193, #63349, #107519 ) ;
#74081 = AXIS2_PLACEMENT_3D ( 'NONE', #18239, #73394, #65390 ) ;
#74082 = ORIENTED_EDGE ( 'NONE', *, *, #81182, .T. ) ;
#74083 = EDGE_CURVE ( 'NONE', #80743, #27726, #74528, .T. ) ;
#74084 = VECTOR ( 'NONE', #43214, 999.9999999999998863 ) ;
#74085 = CARTESIAN_POINT ( 'NONE',  ( -48.29974487139158867, -27.71228299555239971, 4.000000000000000000 ) ) ;
#74086 = CARTESIAN_POINT ( 'NONE',  ( -55.65468426143998215, -34.51840020119762187, 17.97447928118982929 ) ) ;
#74087 = VERTEX_POINT ( 'NONE', #31716 ) ;
#74088 = LINE ( 'NONE', #107416, #55230 ) ;
#74089 = DIRECTION ( 'NONE',  ( -1.000000000000000000, 0.000000000000000000, 0.000000000000000000 ) ) ;
#74090 = AXIS2_PLACEMENT_3D ( 'NONE', #3562, #45013, #123264 ) ;
#74091 = DIRECTION ( 'NONE',  ( -0.7071067811865487940, 0.7071067811865463515, -0.000000000000000000 ) ) ;
#74092 = FACE_BOUND ( 'NONE', #122694, .T. ) ;
#74093 = ORIENTED_EDGE ( 'NONE', *, *, #41928, .T. ) ;
#74094 = PRESENTATION_STYLE_ASSIGNMENT (( #128481 ) ) ;
#74095 = VECTOR ( 'NONE', #122594, 1000.000000000000227 ) ;
#74096 = DIRECTION ( 'NONE',  ( 0.5735764363510451602, 0.8191520442889924647, 0.000000000000000000 ) ) ;
#74097 = EDGE_LOOP ( 'NONE', ( #83081, #41400, #28749, #84318 ) ) ;
#74098 = DIRECTION ( 'NONE',  ( 0.7071067811865487940, 0.7071067811865463515, 0.000000000000000000 ) ) ;
#74099 = VERTEX_POINT ( 'NONE', #75936 ) ;
#74100 = CIRCLE ( 'NONE', #11550, 2.500000000000000444 ) ;
#74101 = EDGE_LOOP ( 'NONE', ( #16724, #100724, #68651, #39590 ) ) ;
#74102 = LINE ( 'NONE', #41453, #100343 ) ;
#74103 = ORIENTED_EDGE ( 'NONE', *, *, #13327, .T. ) ;
#74104 = EDGE_CURVE ( 'NONE', #74867, #134670, #80275, .T. ) ;
#74105 = CARTESIAN_POINT ( 'NONE',  ( 58.39126352523145158, -4.472830434245838482, -4.472830434245838482 ) ) ;
#74106 = ORIENTED_EDGE ( 'NONE', *, *, #57506, .F. ) ;
#74107 = LINE ( 'NONE', #126338, #55675 ) ;
#74108 = EDGE_CURVE ( 'NONE', #119037, #100881, #100585, .T. ) ;
#74109 = DIRECTION ( 'NONE',  ( 0.7071067811865487940, 0.7071067811865463515, 0.000000000000000000 ) ) ;
#74110 = ORIENTED_EDGE ( 'NONE', *, *, #45139, .F. ) ;
#74111 = DIRECTION ( 'NONE',  ( 0.6830127018922180770, -0.6830127018922204085, -0.2588190451025213501 ) ) ;
#74112 = AXIS2_PLACEMENT_3D ( 'NONE', #137146, #25503, #37850 ) ;
#74113 = EDGE_CURVE ( 'NONE', #32976, #3234, #65817, .T. ) ;
#74114 = EDGE_CURVE ( 'NONE', #111086, #9245, #84671, .T. ) ;
#74115 = PLANE ( 'NONE',  #27048 ) ;
#74116 = ADVANCED_BREP_SHAPE_REPRESENTATION ( '', ( #46666, #127880 ), #121007 ) ;
#74117 = DIRECTION ( 'NONE',  ( 0.3543493200069162685, -0.000000000000000000, -0.9351131265310288487 ) ) ;
#74118 = LINE ( 'NONE', #140773, #135119 ) ;
#74119 = DIRECTION ( 'NONE',  ( -0.7071067811865486830, -0.7071067811865464625, 0.000000000000000000 ) ) ;
#74120 = ORIENTED_EDGE ( 'NONE', *, *, #118690, .T. ) ;
#74121 = AXIS2_PLACEMENT_3D ( 'NONE', #47435, #28500, #39379 ) ;
#74122 = ORIENTED_EDGE ( 'NONE', *, *, #142380, .F. ) ;
#74123 = DIRECTION ( 'NONE',  ( -0.7071067811865487940, 0.7071067811865463515, -0.000000000000000000 ) ) ;
#74124 = CARTESIAN_POINT ( 'NONE',  ( 18.63425672184678916, -2.500000000000000000, 3.061616997868383634E-16 ) ) ;
#74125 = ORIENTED_EDGE ( 'NONE', *, *, #24707, .F. ) ;
#74126 = ORIENTED_EDGE ( 'NONE', *, *, #112885, .T. ) ;
#74127 = VERTEX_POINT ( 'NONE', #7794 ) ;
#74128 = CARTESIAN_POINT ( 'NONE',  ( 8.843876922607519120, -22.22500000000000497, 4.000000000000000000 ) ) ;
#74130 = EDGE_CURVE ( 'NONE', #78350, #105963, #125369, .T. ) ;
#74129 = CARTESIAN_POINT ( 'NONE',  ( 55.05836038379621300, -7.949999999999996625, -2.130196079827426203 ) ) ;
#74131 = EDGE_CURVE ( 'NONE', #120155, #4917, #117964, .T. ) ;
#74132 = CARTESIAN_POINT ( 'NONE',  ( 30.48921356237309510, -27.52281430457076894, 5.000000000000000000 ) ) ;
#74133 = EDGE_LOOP ( 'NONE', ( #126072, #99380, #17586, #72972, #62383 ) ) ;
#74134 = FACE_OUTER_BOUND ( 'NONE', #20673, .T. ) ;
#74135 = EDGE_CURVE ( 'NONE', #82254, #3598, #120110, .T. ) ;
#74136 = LINE ( 'NONE', #28501, #44703 ) ;
#74137 = CARTESIAN_POINT ( 'NONE',  ( 18.44206980810188767, 7.934999999999993392, 2.126176841940951689 ) ) ;
#74138 = PLANE ( 'NONE',  #19481 ) ;
#74139 = ORIENTED_EDGE ( 'NONE', *, *, #31383, .T. ) ;
#74140 = CARTESIAN_POINT ( 'NONE',  ( 121.0995968585647660, -6.109999999999998543, -1.637169565754160727 ) ) ;
#74141 = CARTESIAN_POINT ( 'NONE',  ( -36.18398860626899705, 28.73617430169812437, 5.000000000000000000 ) ) ;
#74142 = CARTESIAN_POINT ( 'NONE',  ( 0.000000000000000000, -4.999999999999999112, -7.627214432543508948 ) ) ;
#74143 = ADVANCED_FACE ( 'NONE', ( #41155 ), #85362, .F. ) ;
#74145 = ORIENTED_EDGE ( 'NONE', *, *, #76119, .T. ) ;
#74144 = DIRECTION ( 'NONE',  ( 0.7071067811865486830, -0.7071067811865464625, -0.000000000000000000 ) ) ;
#74146 = DIRECTION ( 'NONE',  ( 0.7071067811865486830, -0.7071067811865464625, -0.000000000000000000 ) ) ;
#74147 = VERTEX_POINT ( 'NONE', #91119 ) ;
#74148 = DIRECTION ( 'NONE',  ( -0.3543493200069162685, -0.000000000000000000, -0.9351131265310288487 ) ) ;
#74149 = CARTESIAN_POINT ( 'NONE',  ( 34.42499999999998295, 2.977185695429370504, 5.000000000000000000 ) ) ;
#74150 = LINE ( 'NONE', #53846, #5534 ) ;
#74151 = ORIENTED_EDGE ( 'NONE', *, *, #13058, .T. ) ;
#74152 = VECTOR ( 'NONE', #19394, 1000.000000000000000 ) ;
#74153 = DIRECTION ( 'NONE',  ( -1.000000000000000000, 0.000000000000000000, 0.000000000000000000 ) ) ;
#74154 = DIRECTION ( 'NONE',  ( -0.7071067811865486830, -0.7071067811865464625, 0.000000000000000000 ) ) ;
#74155 = CARTESIAN_POINT ( 'NONE',  ( -34.49999999999975842, 21.05432934483072671, 4.994342998332167660 ) ) ;
#74156 = VECTOR ( 'NONE', #45217, 999.9999999999998863 ) ;
#74157 = EDGE_CURVE ( 'NONE', #94079, #12165, #112146, .T. ) ;
#74158 = VERTEX_POINT ( 'NONE', #67203 ) ;
#74159 = VECTOR ( 'NONE', #94789, 1000.000000000000000 ) ;
#74160 = VECTOR ( 'NONE', #117461, 1000.000000000000114 ) ;
#74161 = AXIS2_PLACEMENT_3D ( 'NONE', #33366, #65986, #91300 ) ;
#74162 = DIRECTION ( 'NONE',  ( 0.7071067811865487940, 0.7071067811865463515, -0.000000000000000000 ) ) ;
#74163 = DIRECTION ( 'NONE',  ( 0.7071067811865487940, 0.7071067811865463515, -0.000000000000000000 ) ) ;
#74164 = AXIS2_PLACEMENT_3D ( 'NONE', #41855, #141904, #20073 ) ;
#74165 = CARTESIAN_POINT ( 'NONE',  ( -1.499999999999987566, -2.568876922607790103, 4.000000000000000000 ) ) ;
#74166 = PLANE ( 'NONE',  #62334 ) ;
#74167 = ORIENTED_EDGE ( 'NONE', *, *, #12075, .T. ) ;
#74168 = ORIENTED_EDGE ( 'NONE', *, *, #58965, .T. ) ;
#74169 = CARTESIAN_POINT ( 'NONE',  ( 19.73493329717937428, 12.75929247661558996, 18.34774599283951702 ) ) ;
#74170 = VECTOR ( 'NONE', #82589, 1000.000000000000000 ) ;
#74171 = DIRECTION ( 'NONE',  ( 0.000000000000000000, 0.000000000000000000, -1.000000000000000000 ) ) ;
#74172 = ADVANCED_FACE ( 'NONE', ( #57781 ), #22937, .F. ) ;
#74173 = CARTESIAN_POINT ( 'NONE',  ( 10.77040314143521904, -7.934999999999989839, 2.126176841940957907 ) ) ;
#74174 = CARTESIAN_POINT ( 'NONE',  ( -31.82816939922330945, 9.759292476615621936, 4.000000000000000000 ) ) ;
#74175 = CARTESIAN_POINT ( 'NONE',  ( -18.32816939922339827, 14.25929247661557397, 4.000000000000000000 ) ) ;
#74176 = ORIENTED_EDGE ( 'NONE', *, *, #98653, .T. ) ;
#74177 = DIRECTION ( 'NONE',  ( -0.7071067811865487940, 0.7071067811865463515, 0.000000000000000000 ) ) ;
#74178 = DIRECTION ( 'NONE',  ( -0.7071067811865486830, -0.7071067811865464625, -0.000000000000000000 ) ) ;
#74179 = CARTESIAN_POINT ( 'NONE',  ( 10.17183060077640100, 6.759292476615647693, 4.000000000000000000 ) ) ;
#74180 = VECTOR ( 'NONE', #13724, 1000.000000000000227 ) ;
#74181 = CARTESIAN_POINT ( 'NONE',  ( -19.49999999999985434, -4.533600742197692490, 5.000000000000000000 ) ) ;
#74182 = CARTESIAN_POINT ( 'NONE',  ( 35.64126352523145158, 4.472830434245837594, 4.472830434245841147 ) ) ;
#74183 = DIRECTION ( 'NONE',  ( -0.000000000000000000, -0.6666666666666656305, -0.7453559924999307862 ) ) ;
#74184 = VECTOR ( 'NONE', #34463, 1000.000000000000227 ) ;
#74185 = ORIENTED_EDGE ( 'NONE', *, *, #104747, .F. ) ;
#74186 = CARTESIAN_POINT ( 'NONE',  ( 45.18398860626900415, 28.73617430169818832, 5.000000000000000000 ) ) ;
#74187 = VECTOR ( 'NONE', #121858, 1000.000000000000000 ) ;
#74188 = ORIENTED_EDGE ( 'NONE', *, *, #94046, .T. ) ;
#74189 = EDGE_CURVE ( 'NONE', #42198, #40019, #12797, .T. ) ;
#74190 = VECTOR ( 'NONE', #22108, 1000.000000000000000 ) ;
#74191 = VERTEX_POINT ( 'NONE', #112834 ) ;
#74192 = DIRECTION ( 'NONE',  ( -0.7071067811865487940, 0.7071067811865463515, -0.000000000000000000 ) ) ;
#74193 = CARTESIAN_POINT ( 'NONE',  ( -7.940000000000007496, -60.26999999999998892, -10.00000000000000178 ) ) ;
#74194 = AXIS2_PLACEMENT_3D ( 'NONE', #140162, #8172, #52411 ) ;
#74195 = DIRECTION ( 'NONE',  ( -0.6830127018922180770, -0.6830127018922204085, -0.2588190451025213501 ) ) ;
#74196 = DIRECTION ( 'NONE',  ( -0.000000000000000000, -0.000000000000000000, 1.000000000000000000 ) ) ;
#74197 = CARTESIAN_POINT ( 'NONE',  ( 22.17183060077632817, -11.24070752338416490, 4.000000000000000000 ) ) ;
#74198 = CARTESIAN_POINT ( 'NONE',  ( -57.29974487139158157, -27.71228299555246011, 4.000000000000000000 ) ) ;
#74199 = DIRECTION ( 'NONE',  ( -0.7071067811865487940, 0.7071067811865463515, 0.000000000000000000 ) ) ;
#74200 = EDGE_CURVE ( 'NONE', #32877, #85323, #44028, .T. ) ;
#74201 = VECTOR ( 'NONE', #80948, 1000.000000000000000 ) ;
#74202 = EDGE_LOOP ( 'NONE', ( #17188, #77478, #91889, #142676 ) ) ;
#74203 = DIRECTION ( 'NONE',  ( -0.000000000000000000, 0.3543493200069153248, 0.9351131265310292928 ) ) ;
#74204 = DIRECTION ( 'NONE',  ( 0.6830127018922180770, -0.6830127018922204085, -0.2588190451025213501 ) ) ;
#74205 = CARTESIAN_POINT ( 'NONE',  ( -8.999999999999934275, -16.60178936734449451, 0.8616154019347290749 ) ) ;
#74206 = CARTESIAN_POINT ( 'NONE',  ( -34.92500000000001137, -15.18334561358941315, 4.500000000000000888 ) ) ;
#74207 = LINE ( 'NONE', #52430, #45118 ) ;
#74208 = DIRECTION ( 'NONE',  ( -0.7071067811865486830, -0.7071067811865464625, 0.000000000000000000 ) ) ;
#74209 = CARTESIAN_POINT ( 'NONE',  ( 60.60002705046288440, 5.819803920172570422, 5.819803920172574863 ) ) ;
#74210 = DIRECTION ( 'NONE',  ( 1.000000000000000000, 0.000000000000000000, 0.000000000000000000 ) ) ;
#74211 = COLOUR_RGB ( '', 0.40784314, 0.44705882, 0.49803922) ;
#74212 = ORIENTED_EDGE ( 'NONE', *, *, #44709, .F. ) ;
#74213 = ORIENTED_EDGE ( 'NONE', *, *, #129035, .F. ) ;
#74214 = CARTESIAN_POINT ( 'NONE',  ( 57.29166666666665719, 3.975000000000003642, -6.884901960086285300 ) ) ;
#74215 = FACE_OUTER_BOUND ( 'NONE', #3391, .T. ) ;
#74216 = DIRECTION ( 'NONE',  ( 0.7071067811865487940, -0.7071067811865463515, 0.000000000000000000 ) ) ;
#74217 = CONICAL_SURFACE ( 'NONE', #111233, 8.094999999999991758, 0.7853981633974466137 ) ;
#74218 = CARTESIAN_POINT ( 'NONE',  ( 60.18398860626900415, 28.73617430169829490, 5.000000000000000000 ) ) ;
#74219 = ORIENTED_EDGE ( 'NONE', *, *, #40855, .F. ) ;
#74220 = CARTESIAN_POINT ( 'NONE',  ( 32.93749999999999289, 5.819803920172574863, -5.819803920172573086 ) ) ;
#74221 = CARTESIAN_POINT ( 'NONE',  ( 50.02126352523143282, -4.472830434245839371, -4.472830434245840259 ) ) ;
#74222 = EDGE_CURVE ( 'NONE', #55809, #111783, #101967, .T. ) ;
#74223 = ORIENTED_EDGE ( 'NONE', *, *, #137527, .T. ) ;
#74224 = DIRECTION ( 'NONE',  ( -1.000000000000000000, -1.224606353822377258E-16, -0.000000000000000000 ) ) ;
#74225 = ORIENTED_EDGE ( 'NONE', *, *, #10564, .F. ) ;
#74226 = EDGE_LOOP ( 'NONE', ( #86441, #45868, #32641, #116498 ) ) ;
#74227 = CIRCLE ( 'NONE', #9286, 2.500000000000000888 ) ;
#74228 = CARTESIAN_POINT ( 'NONE',  ( 20.97999999999999687, 9.521314400968980422E-16, 0.000000000000000000 ) ) ;
#74229 = LINE ( 'NONE', #95253, #77816 ) ;
#74230 = CARTESIAN_POINT ( 'NONE',  ( 6.299744871391586898, -27.71228299555210484, 4.000000000000000000 ) ) ;
#74231 = PLANE ( 'NONE',  #138978 ) ;
#74233 = ADVANCED_FACE ( 'NONE', ( #80244 ), #88246, .F. ) ;
#74232 = ORIENTED_EDGE ( 'NONE', *, *, #17034, .T. ) ;
#74234 = CARTESIAN_POINT ( 'NONE',  ( -60.48921356237309510, -27.52281430457097500, 5.000000000000000000 ) ) ;
#74236 = ORIENTED_EDGE ( 'NONE', *, *, #142931, .F. ) ;
#74235 = PLANE ( 'NONE',  #19807 ) ;
#74237 = ADVANCED_FACE ( 'NONE', ( #78799 ), #56370, .F. ) ;
#74238 = CARTESIAN_POINT ( 'NONE',  ( 15.16666666666666785, -5.278424836066145431, -3.047499999999993658 ) ) ;
#74239 = DIRECTION ( 'NONE',  ( 0.7071067811865486830, -0.7071067811865464625, -0.000000000000000000 ) ) ;
#74240 = SURFACE_STYLE_USAGE ( .BOTH. , #7524 ) ;
#74241 = LINE ( 'NONE', #141647, #111169 ) ;
#74242 = VECTOR ( 'NONE', #46045, 1000.000000000000000 ) ;
#74243 = CARTESIAN_POINT ( 'NONE',  ( 9.005480084712511157, 28.92564299267931816, 4.000000000000000000 ) ) ;
#74244 = EDGE_LOOP ( 'NONE', ( #108492, #134877, #39068, #128954 ) ) ;
#74246 = VERTEX_POINT ( 'NONE', #45479 ) ;
#74245 = EDGE_CURVE ( 'NONE', #137134, #38880, #135336, .T. ) ;
#74247 = EDGE_CURVE ( 'NONE', #124621, #121207, #69360, .T. ) ;
#74248 = CARTESIAN_POINT ( 'NONE',  ( 71.51626352523145158, -4.472830434245839371, 4.472830434245839371 ) ) ;
#74249 = DIRECTION ( 'NONE',  ( 1.000000000000000000, 0.000000000000000000, 0.000000000000000000 ) ) ;
#74250 = DIRECTION ( 'NONE',  ( 0.7071067811865487940, -0.7071067811865463515, 0.000000000000000000 ) ) ;
#74251 = CARTESIAN_POINT ( 'NONE',  ( -5.994519915287488843, 28.92564299267942118, 4.000000000000000000 ) ) ;
#74252 = VERTEX_POINT ( 'NONE', #46197 ) ;
#74253 = ORIENTED_EDGE ( 'NONE', *, *, #113271, .F. ) ;
#74254 = DIRECTION ( 'NONE',  ( -0.7071067811865486830, -0.7071067811865464625, 0.000000000000000000 ) ) ;
#74256 = VECTOR ( 'NONE', #126932, 1000.000000000000000 ) ;
#74255 = CARTESIAN_POINT ( 'NONE',  ( 17.39060256275758221, -2.561874075326514788, 4.636692559446315975 ) ) ;
#74257 = ORIENTED_EDGE ( 'NONE', *, *, #92753, .F. ) ;
#74258 = EDGE_CURVE ( 'NONE', #69001, #101876, #121564, .T. ) ;
#74259 = COLOUR_RGB ( '', 0.72549020, 0.75294118, 0.79215686) ;
#74261 = VERTEX_POINT ( 'NONE', #90371 ) ;
#74260 = CIRCLE ( 'NONE', #2391, 2.500000000000000888 ) ;
#74262 = DIRECTION ( 'NONE',  ( 0.3543493200069162685, -0.000000000000000000, -0.9351131265310288487 ) ) ;
#74263 = ORIENTED_EDGE ( 'NONE', *, *, #101737, .T. ) ;
#74264 = CARTESIAN_POINT ( 'NONE',  ( 0.000000000000000000, 0.000000000000000000, 5.000000000000000000 ) ) ;
#74265 = DIRECTION ( 'NONE',  ( -0.7071067811865487940, 0.7071067811865463515, -0.000000000000000000 ) ) ;
#74266 = CIRCLE ( 'NONE', #109000, 5.968999999999998529 ) ;
#74267 = AXIS2_PLACEMENT_3D ( 'NONE', #71687, #50634, #128211 ) ;
#74268 = CONICAL_SURFACE ( 'NONE', #20941, 2.055000000000001048, 0.9599310885968758145 ) ;
#74269 = AXIS2_PLACEMENT_3D ( 'NONE', #41410, #117523, #74794 ) ;
#74270 = COLOUR_RGB ( '', 0.72549020, 0.75294118, 0.79215686) ;
#74271 = CARTESIAN_POINT ( 'NONE',  ( -6.489213562373093325, -27.52281430457059841, 5.000000000000000000 ) ) ;
#74272 = FACE_BOUND ( 'NONE', #1790, .T. ) ;
#74273 = CARTESIAN_POINT ( 'NONE',  ( 34.17183060077623225, -8.240707523384193323, 4.000000000000000000 ) ) ;
#74274 = CARTESIAN_POINT ( 'NONE',  ( -12.69999999999998153, 3.061616997868383634E-16, -2.500000000000000444 ) ) ;
#74276 = CARTESIAN_POINT ( 'NONE',  ( 1.353980332882009252, 0.4000000000000001887, -2.467792535850613866 ) ) ;
#74275 = AXIS2_PLACEMENT_3D ( 'NONE', #72307, #70851, #103429 ) ;
#74278 = VERTEX_POINT ( 'NONE', #44782 ) ;
#74277 = CARTESIAN_POINT ( 'NONE',  ( 51.85002705046288440, -5.819803920172573086, -5.819803920172573086 ) ) ;
#74279 = DIRECTION ( 'NONE',  ( 0.000000000000000000, 0.000000000000000000, -1.000000000000000000 ) ) ;
#74280 = VERTEX_POINT ( 'NONE', #33870 ) ;
#74282 = ORIENTED_EDGE ( 'NONE', *, *, #41640, .T. ) ;
#74281 = EDGE_CURVE ( 'NONE', #6180, #98003, #24403, .T. ) ;
#74283 = CARTESIAN_POINT ( 'NONE',  ( 83.32876352523143737, 0.000000000000000000, -6.109999999999998543 ) ) ;
#74284 = ORIENTED_EDGE ( 'NONE', *, *, #102266, .T. ) ;
#74285 = VECTOR ( 'NONE', #82835, 999.9999999999998863 ) ;
#74286 = CARTESIAN_POINT ( 'NONE',  ( 31.49999999999977973, -16.91253812416059077, 4.000000000000000000 ) ) ;
#74287 = EDGE_CURVE ( 'NONE', #120984, #20734, #22235, .T. ) ;
#74288 = AXIS2_PLACEMENT_3D ( 'NONE', #120126, #96238, #77414 ) ;
#74289 = CARTESIAN_POINT ( 'NONE',  ( 4.171830600776439191, -17.24070752338410628, 4.000000000000000000 ) ) ;
#74290 = EDGE_CURVE ( 'NONE', #87033, #117239, #95238, .T. ) ;
#74291 = EDGE_CURVE ( 'NONE', #9775, #39717, #133886, .T. ) ;
#74292 = CIRCLE ( 'NONE', #83518, 1.499999999999999556 ) ;
#74293 = DIRECTION ( 'NONE',  ( 0.6830127018922181881, 0.6830127018922202975, -0.2588190451025214056 ) ) ;
#74294 = CYLINDRICAL_SURFACE ( 'NONE', #108569, 2.500000000000000000 ) ;
#74295 = CIRCLE ( 'NONE', #132264, 2.055000000000000604 ) ;
#74296 = CARTESIAN_POINT ( 'NONE',  ( 11.99999999999991651, -15.41253812416059787, 4.000000000000000000 ) ) ;
#74297 = DIRECTION ( 'NONE',  ( 0.000000000000000000, 0.000000000000000000, 1.000000000000000000 ) ) ;
#74298 = DIRECTION ( 'NONE',  ( -1.000000000000000000, -0.000000000000000000, -0.000000000000000000 ) ) ;
#74299 = VECTOR ( 'NONE', #67468, 1000.000000000000000 ) ;
#74300 = DIRECTION ( 'NONE',  ( -0.000000000000000000, -0.3543493200069153248, -0.9351131265310291818 ) ) ;
#74301 = CARTESIAN_POINT ( 'NONE',  ( 180.5498074873981125, -49.14999999999999858, -40.57313449935461591 ) ) ;
#74302 = LINE ( 'NONE', #19194, #79297 ) ;
#74303 = ORIENTED_EDGE ( 'NONE', *, *, #116058, .T. ) ;
#74304 = AXIS2_PLACEMENT_3D ( 'NONE', #52251, #61728, #31232 ) ;
#74305 = CARTESIAN_POINT ( 'NONE',  ( 2.999999999999981792, 7.931123077392108200, 4.000000000000000000 ) ) ;
#74306 = DIRECTION ( 'NONE',  ( 0.000000000000000000, -1.000000000000000000, 0.000000000000000000 ) ) ;
#74307 = ORIENTED_EDGE ( 'NONE', *, *, #51078, .T. ) ;
#74308 = ORIENTED_EDGE ( 'NONE', *, *, #103245, .T. ) ;
#74309 = EDGE_CURVE ( 'NONE', #64363, #61603, #40427, .T. ) ;
#74310 = VECTOR ( 'NONE', #40156, 999.9999999999998863 ) ;
#74312 = EDGE_LOOP ( 'NONE', ( #107622, #104412, #74345, #57426 ) ) ;
#74311 = EDGE_CURVE ( 'NONE', #60942, #106916, #5482, .T. ) ;
#74313 = CARTESIAN_POINT ( 'NONE',  ( 40.39626352523143993, 4.472830434245840259, -4.472830434245838482 ) ) ;
#74314 = EDGE_LOOP ( 'NONE', ( #129161, #35617, #40913, #116487 ) ) ;
#74315 = CARTESIAN_POINT ( 'NONE',  ( 28.17183060077627843, 9.759292476615620160, 4.000000000000000000 ) ) ;
#74316 = VECTOR ( 'NONE', #97599, 1000.000000000000000 ) ;
#74317 = CARTESIAN_POINT ( 'NONE',  ( 28.62913961620377279, 5.278424836066147208, 3.047499999999990550 ) ) ;
#74318 = CARTESIAN_POINT ( 'NONE',  ( 1.826117250740552755, 12.50058190090600441, -26.81569114864833381 ) ) ;
#74319 = ADVANCED_FACE ( 'NONE', ( #49034 ), #102198, .T. ) ;
#74320 = ORIENTED_EDGE ( 'NONE', *, *, #111428, .F. ) ;
#74321 = CARTESIAN_POINT ( 'NONE',  ( 13.18000000000000149, -2.055000000000000160, 0.000000000000000000 ) ) ;
#74322 = ORIENTED_EDGE ( 'NONE', *, *, #105046, .F. ) ;
#74323 = DIRECTION ( 'NONE',  ( 0.7071067811865487940, 0.7071067811865463515, 0.000000000000000000 ) ) ;
#74324 = AXIS2_PLACEMENT_3D ( 'NONE', #129475, #54800, #98979 ) ;
#74325 = CARTESIAN_POINT ( 'NONE',  ( 5.755190629914537226, 4.202752102959690472E-16, 0.000000000000000000 ) ) ;
#74326 = ADVANCED_FACE ( 'NONE', ( #27244 ), #72248, .F. ) ;
#74328 = ORIENTED_EDGE ( 'NONE', *, *, #110930, .F. ) ;
#74327 = CARTESIAN_POINT ( 'NONE',  ( -1.499999999999990896, 18.43112307739199451, 4.000000000000000000 ) ) ;
#74329 = AXIS2_PLACEMENT_3D ( 'NONE', #16546, #135514, #58713 ) ;
#74330 = EDGE_LOOP ( 'NONE', ( #85344, #69456, #48819, #26198, #140485 ) ) ;
#74331 = CARTESIAN_POINT ( 'NONE',  ( -15.32816939922341781, -9.740707523384180888, 4.000000000000000000 ) ) ;
#74332 = DIRECTION ( 'NONE',  ( 0.3543493200069162685, -0.000000000000000000, -0.9351131265310288487 ) ) ;
#74333 = ORIENTED_EDGE ( 'NONE', *, *, #103177, .F. ) ;
#74334 = FACE_OUTER_BOUND ( 'NONE', #83907, .T. ) ;
#74335 = ORIENTED_EDGE ( 'NONE', *, *, #92943, .F. ) ;
#74336 = ORIENTED_EDGE ( 'NONE', *, *, #92219, .F. ) ;
#74337 = ORIENTED_EDGE ( 'NONE', *, *, #6979, .T. ) ;
#74338 = DIRECTION ( 'NONE',  ( -0.7071067811865487940, 0.7071067811865463515, -0.000000000000000000 ) ) ;
#74339 = ADVANCED_FACE ( 'NONE', ( #137463 ), #17105, .T. ) ;
#74340 = VECTOR ( 'NONE', #35488, 1000.000000000000000 ) ;
#74341 = DIRECTION ( 'NONE',  ( 0.5735764363510451602, 0.8191520442889924647, 0.000000000000000000 ) ) ;
#74342 = DIRECTION ( 'NONE',  ( -0.000000000000000000, -0.3543493200069152693, 0.9351131265310292928 ) ) ;
#74343 = CARTESIAN_POINT ( 'NONE',  ( -47.99451991528749062, 28.92564299267971251, 4.000000000000000000 ) ) ;
#74344 = DIRECTION ( 'NONE',  ( -0.7071067811865486830, -0.7071067811865464625, 0.000000000000000000 ) ) ;
#74345 = ORIENTED_EDGE ( 'NONE', *, *, #57796, .F. ) ;
#74346 = DIRECTION ( 'NONE',  ( 0.7071067811865487940, 0.7071067811865463515, 0.000000000000000000 ) ) ;
#74347 = ORIENTED_EDGE ( 'NONE', *, *, #72882, .F. ) ;
#74348 = EDGE_CURVE ( 'NONE', #139436, #18445, #15618, .T. ) ;
#74349 = AXIS2_PLACEMENT_3D ( 'NONE', #34817, #23179, #67466 ) ;
#74350 =( BOUNDED_CURVE ( )  B_SPLINE_CURVE ( 2, ( #32987, #42428, #83229, #115806, #127432, #39747, #72396, #128177, #16516, #62203, #60804, #17250, #65624 ),
 .UNSPECIFIED., .F., .T. ) 
 B_SPLINE_CURVE_WITH_KNOTS ( ( 3, 2, 2, 2, 2, 2, 3 ),
 ( 0.1333333333333333315, 0.1361111111111110994, 0.1388888888888888951, 0.1416666666666666630, 0.1444444444444444309, 0.1472222222222222265, 0.1499999999999999944 ),
 .UNSPECIFIED. ) 
 CURVE ( )  GEOMETRIC_REPRESENTATION_ITEM ( )  RATIONAL_B_SPLINE_CURVE ( ( 1.000000000000000000, 0.9659258262890683122, 1.000000000000000000, 0.9659258262890683122, 1.000000000000000000, 0.9659258262890683122, 1.000000000000000000, 0.9659258262890683122, 1.000000000000000000, 0.9659258262890683122, 1.000000000000000000, 0.9659258262890683122, 1.000000000000000000 ) ) 
 REPRESENTATION_ITEM ( '' )  );
#74351 = EDGE_CURVE ( 'NONE', #96542, #94223, #47630, .T. ) ;
#74352 = CARTESIAN_POINT ( 'NONE',  ( 32.20790314143521726, -6.871911579029513106, -3.967499999999993587 ) ) ;
#74353 = ORIENTED_EDGE ( 'NONE', *, *, #16527, .F. ) ;
#74354 = FACE_OUTER_BOUND ( 'NONE', #121885, .T. ) ;
#74355 = DIRECTION ( 'NONE',  ( -0.7071067811865487940, 0.7071067811865463515, 0.000000000000000000 ) ) ;
#74356 = EDGE_LOOP ( 'NONE', ( #30356, #60248, #49529, #26841 ) ) ;
#74357 = EDGE_LOOP ( 'NONE', ( #28084, #69403, #85755, #120227 ) ) ;
#74358 = DIRECTION ( 'NONE',  ( 0.6830127018922181881, 0.6830127018922202975, -0.2588190451025214056 ) ) ;
#74359 = DIRECTION ( 'NONE',  ( 0.000000000000000000, -0.3543493200069153248, 0.9351131265310292928 ) ) ;
#74360 = CARTESIAN_POINT ( 'NONE',  ( 51.48921356237309510, -27.52281430457091460, 5.000000000000000000 ) ) ;
#74361 = LINE ( 'NONE', #27985, #38171 ) ;
#74363 = EDGE_CURVE ( 'NONE', #19902, #99485, #92496, .T. ) ;
#74362 = VECTOR ( 'NONE', #136357, 999.9999999999998863 ) ;
#74364 = CARTESIAN_POINT ( 'NONE',  ( 2.837178562577524071E-15, -50.22575108203882621, -35.38524182944816943 ) ) ;
#74365 = CARTESIAN_POINT ( 'NONE',  ( 62.62043019189811588, 3.055000000000002380, -5.291415217122917625 ) ) ;
#74366 = CARTESIAN_POINT ( 'NONE',  ( -22.49999999999984368, 9.431123077392086884, 4.000000000000000000 ) ) ;
#74367 = AXIS2_PLACEMENT_3D ( 'NONE', #11303, #12045, #132458 ) ;
#74368 = AXIS2_PLACEMENT_3D ( 'NONE', #99176, #76035, #42715 ) ;
#74369 = DIRECTION ( 'NONE',  ( 0.6830127018922180770, -0.6830127018922204085, -0.2588190451025213501 ) ) ;
#74370 = DIRECTION ( 'NONE',  ( -0.7071067811865487940, 0.7071067811865463515, 0.000000000000000000 ) ) ;
#74371 = CARTESIAN_POINT ( 'NONE',  ( 7.939999999999994174, -60.26999999999998892, -7.752100000000004876 ) ) ;
#74372 = ORIENTED_EDGE ( 'NONE', *, *, #117375, .T. ) ;
#74373 = DIRECTION ( 'NONE',  ( -0.000000000000000000, 0.000000000000000000, 1.000000000000000000 ) ) ;
#74374 = EDGE_LOOP ( 'NONE', ( #93304, #135951, #102759, #67393 ) ) ;
#74375 = VECTOR ( 'NONE', #131215, 1000.000000000000114 ) ;
#74376 = VECTOR ( 'NONE', #108927, 1000.000000000000000 ) ;
#74377 = AXIS2_PLACEMENT_3D ( 'NONE', #32647, #66005, #87726 ) ;
#74378 = DIRECTION ( 'NONE',  ( 0.6830127018922181881, 0.6830127018922202975, -0.2588190451025214056 ) ) ;
#74380 = CARTESIAN_POINT ( 'NONE',  ( -19.05499999999999261, 3.130000000000007887, -22.35000000000000142 ) ) ;
#74379 = CONICAL_SURFACE ( 'NONE', #18767, 2.055000000000001048, 0.9599310885968758145 ) ;
#74381 = ORIENTED_EDGE ( 'NONE', *, *, #129377, .T. ) ;
#74382 = VECTOR ( 'NONE', #34208, 1000.000000000000000 ) ;
#74383 = FACE_OUTER_BOUND ( 'NONE', #104589, .T. ) ;
#74385 = ORIENTED_EDGE ( 'NONE', *, *, #98093, .T. ) ;
#74384 = CARTESIAN_POINT ( 'NONE',  ( 29.16170612452601674, -6.740707523384216415, 16.75550250614874415 ) ) ;
#74386 = CARTESIAN_POINT ( 'NONE',  ( 27.99999999999996803, -49.14999999999999147, 45.92499999999999005 ) ) ;
#74387 = LINE ( 'NONE', #73657, #41747 ) ;
#74388 = CARTESIAN_POINT ( 'NONE',  ( 23.99999999999983658, -4.447814304570781196, 5.000000000000000000 ) ) ;
#74389 = ORIENTED_EDGE ( 'NONE', *, *, #42760, .F. ) ;
#74390 = VERTEX_POINT ( 'NONE', #14939 ) ;
#74391 = DIRECTION ( 'NONE',  ( 0.7071067811865486830, -0.7071067811865464625, -0.000000000000000000 ) ) ;
#74392 = VECTOR ( 'NONE', #77979, 1000.000000000000000 ) ;
#74393 = FACE_OUTER_BOUND ( 'NONE', #16981, .T. ) ;
#74394 = CARTESIAN_POINT ( 'NONE',  ( 95.89169371712955581, 2.130196079827421762, 7.950000000000001066 ) ) ;
#74395 = CARTESIAN_POINT ( 'NONE',  ( -32.67183060077624646, 8.259292476615637923, 4.000000000000000000 ) ) ;
#74396 = CARTESIAN_POINT ( 'NONE',  ( 6.938893903907228378E-15, -16.44781430457067017, 5.000000000000000000 ) ) ;
#74397 = ORIENTED_EDGE ( 'NONE', *, *, #1632, .F. ) ;
#74398 = VECTOR ( 'NONE', #92071, 999.9999999999998863 ) ;
#74399 = DIRECTION ( 'NONE',  ( -0.7071067811865487940, 0.7071067811865463515, 0.000000000000000000 ) ) ;
#74400 = EDGE_CURVE ( 'NONE', #83675, #24719, #94640, .T. ) ;
#74401 = DIRECTION ( 'NONE',  ( 0.7071067811865487940, 0.7071067811865463515, 0.000000000000000000 ) ) ;
#74402 = DIRECTION ( 'NONE',  ( -1.000000000000000000, -0.000000000000000000, -0.000000000000000000 ) ) ;
#74403 = ORIENTED_EDGE ( 'NONE', *, *, #130762, .F. ) ;
#74404 = CIRCLE ( 'NONE', #120607, 3.378199999999997871 ) ;
#74405 = CARTESIAN_POINT ( 'NONE',  ( -6.349999999999999645, 1.530808498934155579E-16, -1.249999999999970690 ) ) ;
#74406 = ORIENTED_EDGE ( 'NONE', *, *, #12515, .F. ) ;
#74407 = VECTOR ( 'NONE', #87609, 1000.000000000000000 ) ;
#74408 = CARTESIAN_POINT ( 'NONE',  ( 71.16709685856477563, -3.055000000000000160, -5.291415217122921177 ) ) ;
#74409 = CIRCLE ( 'NONE', #11855, 2.247899999999996901 ) ;
#74410 = CARTESIAN_POINT ( 'NONE',  ( 30.65494483745363041, 5.259292476615662792, 12.77922209995901071 ) ) ;
#74411 = LINE ( 'NONE', #140358, #111819 ) ;
#74412 = ORIENTED_EDGE ( 'NONE', *, *, #92308, .F. ) ;
#74413 = AXIS2_PLACEMENT_3D ( 'NONE', #2109, #125370, #26058 ) ;
#74414 = CARTESIAN_POINT ( 'NONE',  ( 28.49999999999981171, 13.46639925780212366, 5.000000000000000000 ) ) ;
#74415 = DIRECTION ( 'NONE',  ( -0.6830127018922180770, -0.6830127018922204085, -0.2588190451025213501 ) ) ;
#74416 = DIRECTION ( 'NONE',  ( 0.7071067811865486830, -0.7071067811865464625, -0.000000000000000000 ) ) ;
#74417 = EDGE_CURVE ( 'NONE', #75827, #113019, #136723, .T. ) ;
#74418 = AXIS2_PLACEMENT_3D ( 'NONE', #68862, #80446, #56585 ) ;
#74419 = DIRECTION ( 'NONE',  ( -0.000000000000000000, 0.000000000000000000, 1.000000000000000000 ) ) ;
#74421 = ORIENTED_EDGE ( 'NONE', *, *, #89514, .F. ) ;
#74420 = CARTESIAN_POINT ( 'NONE',  ( -12.20000000000000284, -25.83999999999998920, 13.17925390838734323 ) ) ;
#74422 = EDGE_CURVE ( 'NONE', #23253, #28047, #51738, .T. ) ;
#74423 = CARTESIAN_POINT ( 'NONE',  ( -8.207106781186491062, 18.75929247661553489, 5.000000000000000000 ) ) ;
#74424 = SURFACE_STYLE_FILL_AREA ( #6238 ) ;
#74425 = ADVANCED_FACE ( 'NONE', ( #59907 ), #72955, .F. ) ;
#74426 = EDGE_LOOP ( 'NONE', ( #68620, #12492, #96867, #104576, #115228 ) ) ;
#74427 = ORIENTED_EDGE ( 'NONE', *, *, #35510, .F. ) ;
#74428 = CARTESIAN_POINT ( 'NONE',  ( 71.45876352523143282, 0.000000000000000000, -6.110000000000001208 ) ) ;
#74429 =( GEOMETRIC_REPRESENTATION_CONTEXT ( 3 ) GLOBAL_UNCERTAINTY_ASSIGNED_CONTEXT ( ( #15817 ) ) GLOBAL_UNIT_ASSIGNED_CONTEXT ( ( #94570, #71422, #59151 ) ) REPRESENTATION_CONTEXT ( 'NONE', 'WORKASPACE' ) );
#74430 = ORIENTED_EDGE ( 'NONE', *, *, #36954, .F. ) ;
#74431 = EDGE_CURVE ( 'NONE', #91733, #130435, #114267, .T. ) ;
#74432 = CARTESIAN_POINT ( 'NONE',  ( 28.49999999999981171, -4.533600742197688938, 5.000000000000000000 ) ) ;
#74433 = LINE ( 'NONE', #20009, #92010 ) ;
#74434 = AXIS2_PLACEMENT_3D ( 'NONE', #11975, #103111, #92211 ) ;
#74435 = DIRECTION ( 'NONE',  ( -0.7071067811865486830, -0.7071067811865464625, 0.000000000000000000 ) ) ;
#74436 = DIRECTION ( 'NONE',  ( -0.7071067811865487940, 0.7071067811865463515, -0.000000000000000000 ) ) ;
#74437 = VERTEX_POINT ( 'NONE', #26551 ) ;
#74438 = AXIS2_PLACEMENT_3D ( 'NONE', #22247, #44041, #89672 ) ;
#74439 = CARTESIAN_POINT ( 'NONE',  ( -4.641757024588570424, 15.75929247661555088, 19.34181609438700633 ) ) ;
#74440 = DIRECTION ( 'NONE',  ( 0.7071067811865487940, 0.7071067811865463515, 0.000000000000000000 ) ) ;
#74441 = EDGE_CURVE ( 'NONE', #31644, #32667, #9642, .T. ) ;
#74442 = ORIENTED_EDGE ( 'NONE', *, *, #20735, .T. ) ;
#74443 = DIRECTION ( 'NONE',  ( -0.000000000000000000, -0.3543493200069152693, 0.9351131265310292928 ) ) ;
#74444 = VECTOR ( 'NONE', #131816, 1000.000000000000000 ) ;
#74445 = CARTESIAN_POINT ( 'NONE',  ( 48.29974487139158867, -27.71228299555239971, 4.000000000000000000 ) ) ;
#74446 = DIRECTION ( 'NONE',  ( -1.000000000000000000, -0.000000000000000000, -0.000000000000000000 ) ) ;
#74447 = VECTOR ( 'NONE', #126547, 1000.000000000000227 ) ;
#74448 = EDGE_CURVE ( 'NONE', #100283, #143396, #38156, .T. ) ;
#74449 = ORIENTED_EDGE ( 'NONE', *, *, #9161, .T. ) ;
#74450 = ORIENTED_EDGE ( 'NONE', *, *, #60246, .F. ) ;
#74451 = FACE_BOUND ( 'NONE', #76733, .T. ) ;
#74452 = CARTESIAN_POINT ( 'NONE',  ( 22.49999999999984368, -17.56887692260762535, 4.000000000000000000 ) ) ;
#74453 = CARTESIAN_POINT ( 'NONE',  ( 35.99451991528749772, 28.92564299267963079, 4.000000000000000000 ) ) ;
#74454 = CARTESIAN_POINT ( 'NONE',  ( -41.99451991528749062, 28.92564299267967343, 4.000000000000000000 ) ) ;
#74455 = EDGE_CURVE ( 'NONE', #124291, #18445, #134708, .T. ) ;
#74456 = VECTOR ( 'NONE', #85576, 1000.000000000000000 ) ;
#74457 = LINE ( 'NONE', #54150, #34227 ) ;
#74458 = FACE_OUTER_BOUND ( 'NONE', #63521, .T. ) ;
#74459 = ORIENTED_EDGE ( 'NONE', *, *, #71021, .T. ) ;
#74460 = VERTEX_POINT ( 'NONE', #140309 ) ;
#74461 = ORIENTED_EDGE ( 'NONE', *, *, #104835, .T. ) ;
#74462 = ORIENTED_EDGE ( 'NONE', *, *, #5989, .F. ) ;
#74463 = EDGE_CURVE ( 'NONE', #120796, #120211, #142467, .T. ) ;
#74464 = VECTOR ( 'NONE', #91792, 1000.000000000000000 ) ;
#74465 = DIRECTION ( 'NONE',  ( 0.000000000000000000, -0.3543493200069153803, -0.9351131265310292928 ) ) ;
#74466 = EDGE_CURVE ( 'NONE', #101826, #43833, #141005, .T. ) ;
#74468 = EDGE_CURVE ( 'NONE', #17205, #62844, #43155, .T. ) ;
#74467 = VECTOR ( 'NONE', #106720, 1000.000000000000000 ) ;
#74469 =( BOUNDED_SURFACE ( )  B_SPLINE_SURFACE ( 1, 2, ( 
 ( #33843, #88216, #44750, #108482, #75902, #9162, #110634, #120075, #120817, #54188, #11312, #43286, #22207, #55594, #63629, #132466, #77367, #76641, #21524, #33155, #65788, #121530, #66470, #109946, #10615, #99782, #457, #133161, #69320, #91760, #3307, #113505, #36661, #57742, #25063, #92456, #48261, #101209, #14197, #125105, #1849, #45445, #133850, #57036, #46904, #102665, #68617, #58490, #56341, #34541, #46157, #14909, #78767, #122235, #103335, #23658, #100519, #112800, #24370, #90336, #1163, #37394, #124398, #134587, #67927, #22907, #47597, #35284, #79525, #101931, #123712, #13460, #2594, #91083, #89625, #135304, #122976, #135986, #80906, #35985, #80214, #25790, #136690, #70067, #114231, #59182, #3982, #12761, #67171, #111363, #12053, #112114, #18452, #27938, #62021, #81639, #28676, #106178, #49725, #48994, #139594, #72923, #125843, #105478, #26516, #70762, #4696, #61333, #6142, #15585, #59864, #114907, #62735, #104040, #39554, #16317, #127238, #93193, #72209, #137430, #17747, #117070, #38119, #7593, #17070, #82339, #96038, #6855, #106914, #126524, #5443, #27211, #29350, #71454, #83781, #116378, #73595, #83040, #84485, #117762, #140275, #51134, #40279, #115613, #60610, #95330, #104783, #128681, #51852, #50419, #94605, #93900, #138138, #38824, #138860, #127995, #65613, #32229, #98889, #119910, #87327, #11140, #110470, #19899, #76464, #43818, #64150, #107628, #52540, #119217, #109050, #21350, #130852, #131540, #118507, #96722, #108311, #77190, #140965, #40964, #22042, #85883, #19206, #143123, #85162, #55416, #43117, #31515, #75740, #63464, #121363, #130121, #20614, #120633, #109781, #129378, #42417, #8290, #30822, #9740, #10449, #64869, #54709, #88036, #98204, #99596, #132286, #32974, #75048, #66297, #8983, #30066, #74317, #41669, #53243, #54009, #97460, #141712, #86629, #142431, #11874, #111943, #88770, #56163, #35832, #77877, #25617, #12601, #122800, #100347, #132999, #45280, #122069, #57572, #47439, #998, #80054, #56877, #23482, #89453, #112639 ),
 ( #133688, #101757, #134409, #135824, #1690, #3149, #36508, #59028, #124228, #58319, #34371, #274, #113332, #22734, #14015, #24906, #45981, #79349, #101034, #78591, #67749, #90911, #102500, #69154, #135142, #91602, #123551, #46731, #114062, #69892, #90163, #80748, #124935, #35107, #67002, #24213, #68460, #13300, #14752, #2417, #44572, #111187, #33678, #126360, #139425, #59711, #103182, #84327, #4516, #81471, #17584, #3824, #93743, #5275, #27050, #37219, #18284, #105322, #71297, #48827, #48112, #83607, #115449, #16140, #38654, #93027, #127819, #37953, #117595, #106012, #73431, #50253, #137974, #92293, #103872, #26353, #61851, #114750, #60432, #136517, #15424, #138695, #125671, #128524, #104613, #82189, #137258, #70609, #49561, #82885, #16900, #6682, #127074, #39381, #27765, #72029, #116209, #61172, #5975, #28502, #94442, #72763, #116915, #50961, #95156, #40112, #29190, #19741, #86452, #62556, #43641, #108862, #95874, #64692, #108147, #54542, #42241, #106733, #76287, #8813, #53071, #120444, #98720, #7420, #20440, #121189, #51680, #130679, #140121, #87149, #40799, #98032, #141536, #97266, #9556, #30647, #142266, #74878, #53828, #74137, #31351, #42951, #87861, #32794, #77017, #32055, #131371, #75570, #10284, #132100, #85000, #119740, #142950, #63977, #129208, #21172, #65428, #29894, #96555, #119053, #109604, #118330, #140793, #41491, #19033, #107464, #8127, #63297, #52368, #85699, #129945, #24036, #111761, #56710, #88, #58133, #66832, #1525, #68295, #2238, #110297, #23289, #44391, #11690, #134233, #101574, #100870, #46550, #124061, #79168, #135655, #13124, #24736, #90739, #34203, #45807, #89984, #36344, #34926, #134966, #100177, #35663, #55979, #67570, #79889, #68983, #826, #102330, #12427, #113162, #21882, #112471, #13835, #133514, #132828, #2978, #57395, #66132, #123372, #10975, #55243, #88598, #47271, #91443, #99422, #33513, #77712, #80573, #121889, #22563, #45114, #111011, #89290, #78420, #122618, #60994, #16718, #3660, #50783, #60253, #25439 ) ),
 .UNSPECIFIED., .F., .F., .F. ) 
 B_SPLINE_SURFACE_WITH_KNOTS ( ( 2, 2 ),
 ( 3, 2, 2, 2, 2, 2, 2, 2, 2, 2, 2, 2, 2, 2, 2, 2, 2, 2, 2, 2, 2, 2, 2, 2, 2, 2, 2, 2, 2, 2, 2, 2, 2, 2, 2, 2, 2, 2, 2, 2, 2, 2, 2, 2, 2, 2, 2, 2, 2, 2, 2, 2, 2, 2, 2, 2, 2, 2, 2, 2, 2, 2, 2, 2, 2, 2, 2, 2, 2, 2, 2, 2, 2, 2, 2, 2, 2, 2, 2, 2, 2, 2, 2, 2, 2, 2, 2, 2, 2, 2, 2, 2, 2, 2, 2, 2, 2, 2, 2, 2, 2, 2, 2, 2, 2, 2, 2, 2, 2, 2, 2, 2, 2, 2, 2, 2, 2, 2, 2, 2, 3 ),
 ( 0.000000000000000000, 1.000000000000000000 ),
 ( 0.000000000000000000, 0.008333333333333333218, 0.01666666666666666644, 0.02500000000000000139, 0.03333333333333333287, 0.04166666666666666435, 0.05000000000000000278, 0.05833333333333333426, 0.06666666666666666574, 0.07499999999999999722, 0.08333333333333332871, 0.09166666666666666019, 0.1000000000000000056, 0.1083333333333333370, 0.1166666666666666685, 0.1250000000000000000, 0.1333333333333333315, 0.1416666666666666630, 0.1499999999999999944, 0.1583333333333333259, 0.1666666666666666574, 0.1749999999999999889, 0.1833333333333333204, 0.1916666666666666796, 0.2000000000000000111, 0.2083333333333333426, 0.2166666666666666741, 0.2250000000000000056, 0.2333333333333333370, 0.2416666666666666685, 0.2500000000000000000, 0.2583333333333333592, 0.2666666666666666630, 0.2750000000000000222, 0.2833333333333333259, 0.2916666666666666852, 0.2999999999999999889, 0.3083333333333333481, 0.3166666666666666519, 0.3250000000000000111, 0.3333333333333333148, 0.3416666666666666741, 0.3499999999999999778, 0.3583333333333333370, 0.3666666666666666408, 0.3750000000000000000, 0.3833333333333333592, 0.3916666666666666630, 0.4000000000000000222, 0.4083333333333333259, 0.4166666666666666852, 0.4249999999999999889, 0.4333333333333333481, 0.4416666666666666519, 0.4500000000000000111, 0.4583333333333333148, 0.4666666666666666741, 0.4749999999999999778, 0.4833333333333333370, 0.4916666666666666408, 0.5000000000000000000, 0.5083333333333333037, 0.5166666666666667185, 0.5250000000000000222, 0.5333333333333333259, 0.5416666666666666297, 0.5500000000000000444, 0.5583333333333333481, 0.5666666666666666519, 0.5749999999999999556, 0.5833333333333333703, 0.5916666666666666741, 0.5999999999999999778, 0.6083333333333332815, 0.6166666666666666963, 0.6250000000000000000, 0.6333333333333333037, 0.6416666666666667185, 0.6500000000000000222, 0.6583333333333333259, 0.6666666666666666297, 0.6750000000000000444, 0.6833333333333333481, 0.6916666666666666519, 0.6999999999999999556, 0.7083333333333333703, 0.7166666666666666741, 0.7249999999999999778, 0.7333333333333332815, 0.7416666666666666963, 0.7500000000000000000, 0.7583333333333333037, 0.7666666666666667185, 0.7750000000000000222, 0.7833333333333333259, 0.7916666666666666297, 0.8000000000000000444, 0.8083333333333333481, 0.8166666666666666519, 0.8249999999999999556, 0.8333333333333333703, 0.8416666666666666741, 0.8499999999999999778, 0.8583333333333332815, 0.8666666666666666963, 0.8750000000000000000, 0.8833333333333333037, 0.8916666666666667185, 0.9000000000000000222, 0.9083333333333333259, 0.9166666666666666297, 0.9250000000000000444, 0.9333333333333333481, 0.9416666666666666519, 0.9499999999999999556, 0.9583333333333333703, 0.9666666666666666741, 0.9749999999999999778, 0.9833333333333332815, 0.9916666666666666963, 1.000000000000000000 ),
 .UNSPECIFIED. ) 
 GEOMETRIC_REPRESENTATION_ITEM ( )  RATIONAL_B_SPLINE_SURFACE ( (
 ( 1.000000000000000000, 0.9659258262890683122, 1.000000000000000000, 0.9659258262890683122, 1.000000000000000000, 0.9659258262890683122, 1.000000000000000000, 0.9659258262890683122, 1.000000000000000000, 0.9659258262890683122, 1.000000000000000000, 0.9659258262890683122, 1.000000000000000000, 0.9659258262890683122, 1.000000000000000000, 0.9659258262890683122, 1.000000000000000000, 0.9659258262890683122, 1.000000000000000000, 0.9659258262890683122, 1.000000000000000000, 0.9659258262890683122, 1.000000000000000000, 0.9659258262890683122, 1.000000000000000000, 0.9659258262890683122, 1.000000000000000000, 0.9659258262890683122, 1.000000000000000000, 0.9659258262890683122, 1.000000000000000000, 0.9659258262890683122, 1.000000000000000000, 0.9659258262890683122, 1.000000000000000000, 0.9659258262890683122, 1.000000000000000000, 0.9659258262890683122, 1.000000000000000000, 0.9659258262890683122, 1.000000000000000000, 0.9659258262890683122, 1.000000000000000000, 0.9659258262890683122, 1.000000000000000000, 0.9659258262890683122, 1.000000000000000000, 0.9659258262890683122, 1.000000000000000000, 0.9659258262890683122, 1.000000000000000000, 0.9659258262890683122, 1.000000000000000000, 0.9659258262890683122, 1.000000000000000000, 0.9659258262890683122, 1.000000000000000000, 0.9659258262890683122, 1.000000000000000000, 0.9659258262890683122, 1.000000000000000000, 0.9659258262890683122, 1.000000000000000000, 0.9659258262890683122, 1.000000000000000000, 0.9659258262890683122, 1.000000000000000000, 0.9659258262890683122, 1.000000000000000000, 0.9659258262890683122, 1.000000000000000000, 0.9659258262890683122, 1.000000000000000000, 0.9659258262890683122, 1.000000000000000000, 0.9659258262890683122, 1.000000000000000000, 0.9659258262890683122, 1.000000000000000000, 0.9659258262890683122, 1.000000000000000000, 0.9659258262890683122, 1.000000000000000000, 0.9659258262890683122, 1.000000000000000000, 0.9659258262890683122, 1.000000000000000000, 0.9659258262890683122, 1.000000000000000000, 0.9659258262890683122, 1.000000000000000000, 0.9659258262890683122, 1.000000000000000000, 0.9659258262890683122, 1.000000000000000000, 0.9659258262890683122, 1.000000000000000000, 0.9659258262890683122, 1.000000000000000000, 0.9659258262890683122, 1.000000000000000000, 0.9659258262890683122, 1.000000000000000000, 0.9659258262890683122, 1.000000000000000000, 0.9659258262890683122, 1.000000000000000000, 0.9659258262890683122, 1.000000000000000000, 0.9659258262890683122, 1.000000000000000000, 0.9659258262890683122, 1.000000000000000000, 0.9659258262890683122, 1.000000000000000000, 0.9659258262890683122, 1.000000000000000000, 0.9659258262890683122, 1.000000000000000000, 0.9659258262890683122, 1.000000000000000000, 0.9659258262890683122, 1.000000000000000000, 0.9659258262890683122, 1.000000000000000000, 0.9659258262890683122, 1.000000000000000000, 0.9659258262890683122, 1.000000000000000000, 0.9659258262890683122, 1.000000000000000000, 0.9659258262890683122, 1.000000000000000000, 0.9659258262890683122, 1.000000000000000000, 0.9659258262890683122, 1.000000000000000000, 0.9659258262890683122, 1.000000000000000000, 0.9659258262890683122, 1.000000000000000000, 0.9659258262890683122, 1.000000000000000000, 0.9659258262890683122, 1.000000000000000000, 0.9659258262890683122, 1.000000000000000000, 0.9659258262890683122, 1.000000000000000000, 0.9659258262890683122, 1.000000000000000000, 0.9659258262890683122, 1.000000000000000000, 0.9659258262890683122, 1.000000000000000000, 0.9659258262890683122, 1.000000000000000000, 0.9659258262890683122, 1.000000000000000000, 0.9659258262890683122, 1.000000000000000000, 0.9659258262890683122, 1.000000000000000000, 0.9659258262890683122, 1.000000000000000000, 0.9659258262890683122, 1.000000000000000000, 0.9659258262890683122, 1.000000000000000000, 0.9659258262890683122, 1.000000000000000000, 0.9659258262890683122, 1.000000000000000000, 0.9659258262890683122, 1.000000000000000000, 0.9659258262890683122, 1.000000000000000000, 0.9659258262890683122, 1.000000000000000000, 0.9659258262890683122, 1.000000000000000000, 0.9659258262890683122, 1.000000000000000000, 0.9659258262890683122, 1.000000000000000000, 0.9659258262890683122, 1.000000000000000000, 0.9659258262890683122, 1.000000000000000000, 0.9659258262890683122, 1.000000000000000000, 0.9659258262890683122, 1.000000000000000000, 0.9659258262890683122, 1.000000000000000000, 0.9659258262890683122, 1.000000000000000000, 0.9659258262890683122, 1.000000000000000000, 0.9659258262890683122, 1.000000000000000000, 0.9659258262890683122, 1.000000000000000000, 0.9659258262890683122, 1.000000000000000000, 0.9659258262890683122, 1.000000000000000000, 0.9659258262890683122, 1.000000000000000000, 0.9659258262890683122, 1.000000000000000000, 0.9659258262890683122, 1.000000000000000000, 0.9659258262890683122, 1.000000000000000000, 0.9659258262890683122, 1.000000000000000000, 0.9659258262890683122, 1.000000000000000000, 0.9659258262890683122, 1.000000000000000000, 0.9659258262890683122, 1.000000000000000000, 0.9659258262890683122, 1.000000000000000000, 0.9659258262890683122, 1.000000000000000000, 0.9659258262890683122, 1.000000000000000000, 0.9659258262890683122, 1.000000000000000000, 0.9659258262890683122, 1.000000000000000000, 0.9659258262890683122, 1.000000000000000000, 0.9659258262890683122, 1.000000000000000000, 0.9659258262890683122, 1.000000000000000000, 0.9659258262890683122, 1.000000000000000000),
 ( 1.000000000000000000, 0.9659258262890683122, 1.000000000000000000, 0.9659258262890683122, 1.000000000000000000, 0.9659258262890683122, 1.000000000000000000, 0.9659258262890683122, 1.000000000000000000, 0.9659258262890683122, 1.000000000000000000, 0.9659258262890683122, 1.000000000000000000, 0.9659258262890683122, 1.000000000000000000, 0.9659258262890683122, 1.000000000000000000, 0.9659258262890683122, 1.000000000000000000, 0.9659258262890683122, 1.000000000000000000, 0.9659258262890683122, 1.000000000000000000, 0.9659258262890683122, 1.000000000000000000, 0.9659258262890683122, 1.000000000000000000, 0.9659258262890683122, 1.000000000000000000, 0.9659258262890683122, 1.000000000000000000, 0.9659258262890683122, 1.000000000000000000, 0.9659258262890683122, 1.000000000000000000, 0.9659258262890683122, 1.000000000000000000, 0.9659258262890683122, 1.000000000000000000, 0.9659258262890683122, 1.000000000000000000, 0.9659258262890683122, 1.000000000000000000, 0.9659258262890683122, 1.000000000000000000, 0.9659258262890683122, 1.000000000000000000, 0.9659258262890683122, 1.000000000000000000, 0.9659258262890683122, 1.000000000000000000, 0.9659258262890683122, 1.000000000000000000, 0.9659258262890683122, 1.000000000000000000, 0.9659258262890683122, 1.000000000000000000, 0.9659258262890683122, 1.000000000000000000, 0.9659258262890683122, 1.000000000000000000, 0.9659258262890683122, 1.000000000000000000, 0.9659258262890683122, 1.000000000000000000, 0.9659258262890683122, 1.000000000000000000, 0.9659258262890683122, 1.000000000000000000, 0.9659258262890683122, 1.000000000000000000, 0.9659258262890683122, 1.000000000000000000, 0.9659258262890683122, 1.000000000000000000, 0.9659258262890683122, 1.000000000000000000, 0.9659258262890683122, 1.000000000000000000, 0.9659258262890683122, 1.000000000000000000, 0.9659258262890683122, 1.000000000000000000, 0.9659258262890683122, 1.000000000000000000, 0.9659258262890683122, 1.000000000000000000, 0.9659258262890683122, 1.000000000000000000, 0.9659258262890683122, 1.000000000000000000, 0.9659258262890683122, 1.000000000000000000, 0.9659258262890683122, 1.000000000000000000, 0.9659258262890683122, 1.000000000000000000, 0.9659258262890683122, 1.000000000000000000, 0.9659258262890683122, 1.000000000000000000, 0.9659258262890683122, 1.000000000000000000, 0.9659258262890683122, 1.000000000000000000, 0.9659258262890683122, 1.000000000000000000, 0.9659258262890683122, 1.000000000000000000, 0.9659258262890683122, 1.000000000000000000, 0.9659258262890683122, 1.000000000000000000, 0.9659258262890683122, 1.000000000000000000, 0.9659258262890683122, 1.000000000000000000, 0.9659258262890683122, 1.000000000000000000, 0.9659258262890683122, 1.000000000000000000, 0.9659258262890683122, 1.000000000000000000, 0.9659258262890683122, 1.000000000000000000, 0.9659258262890683122, 1.000000000000000000, 0.9659258262890683122, 1.000000000000000000, 0.9659258262890683122, 1.000000000000000000, 0.9659258262890683122, 1.000000000000000000, 0.9659258262890683122, 1.000000000000000000, 0.9659258262890683122, 1.000000000000000000, 0.9659258262890683122, 1.000000000000000000, 0.9659258262890683122, 1.000000000000000000, 0.9659258262890683122, 1.000000000000000000, 0.9659258262890683122, 1.000000000000000000, 0.9659258262890683122, 1.000000000000000000, 0.9659258262890683122, 1.000000000000000000, 0.9659258262890683122, 1.000000000000000000, 0.9659258262890683122, 1.000000000000000000, 0.9659258262890683122, 1.000000000000000000, 0.9659258262890683122, 1.000000000000000000, 0.9659258262890683122, 1.000000000000000000, 0.9659258262890683122, 1.000000000000000000, 0.9659258262890683122, 1.000000000000000000, 0.9659258262890683122, 1.000000000000000000, 0.9659258262890683122, 1.000000000000000000, 0.9659258262890683122, 1.000000000000000000, 0.9659258262890683122, 1.000000000000000000, 0.9659258262890683122, 1.000000000000000000, 0.9659258262890683122, 1.000000000000000000, 0.9659258262890683122, 1.000000000000000000, 0.9659258262890683122, 1.000000000000000000, 0.9659258262890683122, 1.000000000000000000, 0.9659258262890683122, 1.000000000000000000, 0.9659258262890683122, 1.000000000000000000, 0.9659258262890683122, 1.000000000000000000, 0.9659258262890683122, 1.000000000000000000, 0.9659258262890683122, 1.000000000000000000, 0.9659258262890683122, 1.000000000000000000, 0.9659258262890683122, 1.000000000000000000, 0.9659258262890683122, 1.000000000000000000, 0.9659258262890683122, 1.000000000000000000, 0.9659258262890683122, 1.000000000000000000, 0.9659258262890683122, 1.000000000000000000, 0.9659258262890683122, 1.000000000000000000, 0.9659258262890683122, 1.000000000000000000, 0.9659258262890683122, 1.000000000000000000, 0.9659258262890683122, 1.000000000000000000, 0.9659258262890683122, 1.000000000000000000, 0.9659258262890683122, 1.000000000000000000, 0.9659258262890683122, 1.000000000000000000, 0.9659258262890683122, 1.000000000000000000, 0.9659258262890683122, 1.000000000000000000, 0.9659258262890683122, 1.000000000000000000, 0.9659258262890683122, 1.000000000000000000, 0.9659258262890683122, 1.000000000000000000, 0.9659258262890683122, 1.000000000000000000, 0.9659258262890683122, 1.000000000000000000, 0.9659258262890683122, 1.000000000000000000, 0.9659258262890683122, 1.000000000000000000, 0.9659258262890683122, 1.000000000000000000, 0.9659258262890683122, 1.000000000000000000, 0.9659258262890683122, 1.000000000000000000) ) ) 
 REPRESENTATION_ITEM ( '' )  SURFACE ( )  );
#74470 = AXIS2_PLACEMENT_3D ( 'NONE', #114190, #125067, #14157 ) ;
#74471 = CARTESIAN_POINT ( 'NONE',  ( -48.48921356237309510, -27.52281430457089328, 5.000000000000000000 ) ) ;
#74472 = VERTEX_POINT ( 'NONE', #63499 ) ;
#74473 = CARTESIAN_POINT ( 'NONE',  ( 0.000000000000000000, 0.000000000000000000, 5.000000000000000000 ) ) ;
#74474 = DIRECTION ( 'NONE',  ( 0.7071067811865487940, 0.7071067811865463515, 0.000000000000000000 ) ) ;
#74475 = LINE ( 'NONE', #109218, #103690 ) ;
#74476 = CARTESIAN_POINT ( 'NONE',  ( -33.29974487139158867, -27.71228299555229313, 4.000000000000000000 ) ) ;
#74477 = VECTOR ( 'NONE', #93956, 1000.000000000000000 ) ;
#74478 = VECTOR ( 'NONE', #102185, 999.9999999999998863 ) ;
#74479 =( GEOMETRIC_REPRESENTATION_CONTEXT ( 3 ) GLOBAL_UNCERTAINTY_ASSIGNED_CONTEXT ( ( #33190 ) ) GLOBAL_UNIT_ASSIGNED_CONTEXT ( ( #75858, #141839, #13414 ) ) REPRESENTATION_CONTEXT ( 'NONE', 'WORKASPACE' ) );
#74480 = DIRECTION ( 'NONE',  ( 0.6830127018922180770, -0.6830127018922204085, -0.2588190451025213501 ) ) ;
#74481 = VERTEX_POINT ( 'NONE', #75085 ) ;
#74482 = EDGE_CURVE ( 'NONE', #94079, #100675, #96757, .T. ) ;
#74483 = MECHANICAL_DESIGN_GEOMETRIC_PRESENTATION_REPRESENTATION (  '', ( #129692 ), #99919 ) ;
#74484 = CARTESIAN_POINT ( 'NONE',  ( 7.499999999999944045, 13.56627193232215767, -10.57019076586066930 ) ) ;
#74485 = CARTESIAN_POINT ( 'NONE',  ( 51.02083333333333570, 7.949999999999998401, 2.130196079827431532 ) ) ;
#74486 = ORIENTED_EDGE ( 'NONE', *, *, #93418, .F. ) ;
#74487 = LINE ( 'NONE', #96184, #87520 ) ;
#74488 = ORIENTED_EDGE ( 'NONE', *, *, #128045, .F. ) ;
#74489 = EDGE_CURVE ( 'NONE', #38622, #35249, #75782, .T. ) ;
#74490 = PLANE ( 'NONE',  #96892 ) ;
#74491 = EDGE_LOOP ( 'NONE', ( #96144, #10104, #19407, #17355 ) ) ;
#74492 = CARTESIAN_POINT ( 'NONE',  ( 60.81293019189811133, -1.637169565754159617, -6.110000000000001208 ) ) ;
#74493 = ORIENTED_EDGE ( 'NONE', *, *, #135338, .F. ) ;
#74494 = ORIENTED_EDGE ( 'NONE', *, *, #135044, .T. ) ;
#74495 = B_SPLINE_CURVE_WITH_KNOTS ( 'NONE', 3,
 ( #67175, #20795, #65047, #32410 ),
 .UNSPECIFIED., .F., .F.,
 ( 4, 4 ),
 ( 0.003785693138453204761, 0.004021000868919195545 ),
 .UNSPECIFIED. ) ;
#74496 = DIRECTION ( 'NONE',  ( -0.6830127018922180770, -0.6830127018922204085, -0.2588190451025213501 ) ) ;
#74497 = CARTESIAN_POINT ( 'NONE',  ( 0.000000000000000000, 0.000000000000000000, 5.000000000000000000 ) ) ;
#74498 = CARTESIAN_POINT ( 'NONE',  ( 95.08376352523144703, -6.110000000000001208, -3.741295971395164515E-16 ) ) ;
#74499 = CARTESIAN_POINT ( 'NONE',  ( 19.72673754300674176, 9.106605730562614909, 4.258036837949496167 ) ) ;
#74500 = ADVANCED_FACE ( 'NONE', ( #130163 ), #87365, .T. ) ;
#74501 = DIRECTION ( 'NONE',  ( -0.7071067811865486830, -0.7071067811865464625, 0.000000000000000000 ) ) ;
#74502 = LINE ( 'NONE', #118688, #85731 ) ;
#74503 = ADVANCED_FACE ( 'NONE', ( #6891 ), #118543, .F. ) ;
#74504 = CARTESIAN_POINT ( 'NONE',  ( 3.250000000000000000, 0.000000000000000000, 0.000000000000000000 ) ) ;
#74505 = CARTESIAN_POINT ( 'NONE',  ( 0.000000000000000000, 0.000000000000000000, 5.000000000000000000 ) ) ;
#74506 = AXIS2_PLACEMENT_3D ( 'NONE', #9318, #86937, #55748 ) ;
#74507 = DIRECTION ( 'NONE',  ( -0.000000000000000000, 0.000000000000000000, 1.000000000000000000 ) ) ;
#74508 = ORIENTED_EDGE ( 'NONE', *, *, #86397, .T. ) ;
#74509 = VECTOR ( 'NONE', #96674, 1000.000000000000000 ) ;
#74510 = CARTESIAN_POINT ( 'NONE',  ( 2.999999999999999112, 1.399999999999987699, -20.40202195861970580 ) ) ;
#74511 = EDGE_LOOP ( 'NONE', ( #102966, #6789, #129092, #18600, #117712, #112267, #27046 ) ) ;
#74512 = VECTOR ( 'NONE', #97257, 1000.000000000000000 ) ;
#74513 = ORIENTED_EDGE ( 'NONE', *, *, #63936, .F. ) ;
#74514 = ORIENTED_EDGE ( 'NONE', *, *, #60106, .T. ) ;
#74515 = ORIENTED_EDGE ( 'NONE', *, *, #19128, .T. ) ;
#74516 = VECTOR ( 'NONE', #142171, 1000.000000000000000 ) ;
#74517 = CARTESIAN_POINT ( 'NONE',  ( -54.18398860626899705, 28.73617430169825226, 5.000000000000000000 ) ) ;
#74518 = DIRECTION ( 'NONE',  ( 0.7071067811865487940, 0.7071067811865463515, -0.000000000000000000 ) ) ;
#74519 = LINE ( 'NONE', #118703, #74152 ) ;
#74520 = ORIENTED_EDGE ( 'NONE', *, *, #107356, .F. ) ;
#74521 =( NAMED_UNIT ( * ) SI_UNIT ( $, .STERADIAN. ) SOLID_ANGLE_UNIT ( ) );
#74522 = VERTEX_POINT ( 'NONE', #8326 ) ;
#74523 = CIRCLE ( 'NONE', #60688, 2.500000000000000444 ) ;
#74524 = ADVANCED_FACE ( 'NONE', ( #130886 ), #20653, .T. ) ;
#74525 = CARTESIAN_POINT ( 'NONE',  ( -0.02126352523144730070, -5.808823158059033709, 5.808823158059035485 ) ) ;
#74526 = CARTESIAN_POINT ( 'NONE',  ( -33.18398860626899705, 28.73617430169810305, 5.000000000000000000 ) ) ;
#74527 = DIRECTION ( 'NONE',  ( -0.7071067811865486830, -0.7071067811865464625, 0.000000000000000000 ) ) ;
#74528 = LINE ( 'NONE', #142623, #106819 ) ;
#74529 = ORIENTED_EDGE ( 'NONE', *, *, #89445, .F. ) ;
#74530 = ORIENTED_EDGE ( 'NONE', *, *, #71029, .F. ) ;
#74531 = AXIS2_PLACEMENT_3D ( 'NONE', #50696, #30363, #5729 ) ;
#74532 = ORIENTED_EDGE ( 'NONE', *, *, #50517, .T. ) ;
#74533 = CARTESIAN_POINT ( 'NONE',  ( -34.92500000000001137, -22.22500000000000142, 4.500000000000000888 ) ) ;
#74534 = DIRECTION ( 'NONE',  ( -0.3543493200069163240, 0.000000000000000000, -0.9351131265310288487 ) ) ;
#74535 = VECTOR ( 'NONE', #26921, 1000.000000000000000 ) ;
#74536 = CARTESIAN_POINT ( 'NONE',  ( 24.29974487139158867, -27.71228299555223273, 4.000000000000000000 ) ) ;
#74537 = FACE_OUTER_BOUND ( 'NONE', #80340, .T. ) ;
#74538 = LINE ( 'NONE', #108526, #92001 ) ;
#74539 = DIRECTION ( 'NONE',  ( -0.000000000000000000, -0.000000000000000000, 1.000000000000000000 ) ) ;
#74540 = CARTESIAN_POINT ( 'NONE',  ( 25.66709685856477563, -3.055000000000000160, -5.291415217122921177 ) ) ;
#74541 = FACE_OUTER_BOUND ( 'NONE', #75044, .T. ) ;
#74542 = DIRECTION ( 'NONE',  ( 0.000000000000000000, -1.000000000000000000, 0.000000000000000000 ) ) ;
#74543 = ORIENTED_EDGE ( 'NONE', *, *, #9905, .F. ) ;
#74544 = DIRECTION ( 'NONE',  ( 0.7071067811865487940, -0.7071067811865463515, 0.000000000000000000 ) ) ;
#74545 = VECTOR ( 'NONE', #81491, 1000.000000000000000 ) ;
#74546 = CARTESIAN_POINT ( 'NONE',  ( 6.328169399223481761, 14.25929247661557930, 4.000000000000000000 ) ) ;
#74547 = VERTEX_POINT ( 'NONE', #19941 ) ;
#74548 = CARTESIAN_POINT ( 'NONE',  ( 60.29974487139158867, -27.71228299555248142, 4.000000000000000000 ) ) ;
#74550 = VERTEX_POINT ( 'NONE', #32272 ) ;
#74549 = CARTESIAN_POINT ( 'NONE',  ( 0.000000000000000000, 0.000000000000000000, 5.000000000000000000 ) ) ;
#74551 = DIRECTION ( 'NONE',  ( -0.7071067811865486830, -0.7071067811865464625, 0.000000000000000000 ) ) ;
#74553 = ORIENTED_EDGE ( 'NONE', *, *, #6047, .F. ) ;
#74552 = AXIS2_PLACEMENT_3D ( 'NONE', #89702, #12836, #11385 ) ;
#74554 = PLANE ( 'NONE',  #88346 ) ;
#74555 = ORIENTED_EDGE ( 'NONE', *, *, #53652, .T. ) ;
#74556 = CYLINDRICAL_SURFACE ( 'NONE', #121645, 3.999999999999989786 ) ;
#74557 = CARTESIAN_POINT ( 'NONE',  ( 118.2041937171295700, -6.884901960086285300, -3.975000000000000089 ) ) ;
#74558 = CARTESIAN_POINT ( 'NONE',  ( 49.22502705046289151, 5.819803920172573974, -5.819803920172573086 ) ) ;
#74559 = LINE ( 'NONE', #87562, #127264 ) ;
#74560 = LINE ( 'NONE', #7838, #111676 ) ;
#74561 = CARTESIAN_POINT ( 'NONE',  ( 24.48921356237309510, -27.52281430457072631, 5.000000000000000000 ) ) ;
#74562 = CARTESIAN_POINT ( 'NONE',  ( 4.812499999999999112, -4.461849672132299993, -4.461849672132299105 ) ) ;
#74563 = CARTESIAN_POINT ( 'NONE',  ( 19.52040314143522437, 7.934999999999988951, -2.126176841940961904 ) ) ;
#74564 = AXIS2_PLACEMENT_3D ( 'NONE', #58358, #93069, #72072 ) ;
#74565 = AXIS2_PLACEMENT_3D ( 'NONE', #141535, #42240, #119739 ) ;
#74567 = PLANE ( 'NONE',  #60564 ) ;
#74566 = VECTOR ( 'NONE', #133452, 999.9999999999998863 ) ;
#74568 = CARTESIAN_POINT ( 'NONE',  ( 19.05000000000000071, 3.174999999999997158, 4.000000000000000000 ) ) ;
#74569 = ORIENTED_EDGE ( 'NONE', *, *, #29406, .T. ) ;
#74570 =( BOUNDED_CURVE ( )  B_SPLINE_CURVE ( 3, ( #16993, #16232, #36586, #114839 ),
 .UNSPECIFIED., .F., .F. ) 
 B_SPLINE_CURVE_WITH_KNOTS ( ( 4, 4 ),
 ( 2.001653308786169649, 3.503810798801450854 ),
 .UNSPECIFIED. ) 
 CURVE ( )  GEOMETRIC_REPRESENTATION_ITEM ( )  RATIONAL_B_SPLINE_CURVE ( ( 1.000000000000000000, 0.8206354192515240564, 0.8206354192515240564, 1.000000000000000000 ) ) 
 REPRESENTATION_ITEM ( '' )  );
#74571 = VERTEX_POINT ( 'NONE', #53285 ) ;
#74572 = VECTOR ( 'NONE', #9543, 1000.000000000000000 ) ;
#74573 = CIRCLE ( 'NONE', #104657, 2.055000000000000604 ) ;
#74574 = LINE ( 'NONE', #52779, #116156 ) ;
#74575 = EDGE_LOOP ( 'NONE', ( #76807, #121892, #97712, #73207 ) ) ;
#74576 = CARTESIAN_POINT ( 'NONE',  ( 63.18398860626900415, 28.73617430169831621, 5.000000000000000000 ) ) ;
#74577 = CARTESIAN_POINT ( 'NONE',  ( -72.48921356237309510, -27.52281430457106026, 5.000000000000000000 ) ) ;
#74578 = VECTOR ( 'NONE', #141806, 999.9999999999998863 ) ;
#74579 = COLOUR_RGB ( '', 0.09019608, 0.27058824, 0.51372549) ;
#74580 = CARTESIAN_POINT ( 'NONE',  ( -19.49999999999987921, 16.18958161055400780, -11.56426086740815862 ) ) ;
#74581 = VERTEX_POINT ( 'NONE', #64187 ) ;
#74582 = CARTESIAN_POINT ( 'NONE',  ( -34.42500000000001137, 2.977185695429387824, 5.000000000000000000 ) ) ;
#74583 = EDGE_CURVE ( 'NONE', #74923, #81473, #85198, .T. ) ;
#74584 = CARTESIAN_POINT ( 'NONE',  ( 3.299744871391591339, -27.71228299555208352, 4.000000000000000000 ) ) ;
#74585 = DIRECTION ( 'NONE',  ( 0.7071067811865486830, -0.7071067811865464625, -0.000000000000000000 ) ) ;
#74586 = ADVANCED_FACE ( 'NONE', ( #64907 ), #76505, .T. ) ;
#74587 = EDGE_CURVE ( 'NONE', #20582, #69099, #19244, .T. ) ;
#74588 = LINE ( 'NONE', #31081, #81900 ) ;
#74590 = ORIENTED_EDGE ( 'NONE', *, *, #52543, .T. ) ;
#74589 = DIRECTION ( 'NONE',  ( 1.000000000000000000, 0.000000000000000000, 0.000000000000000000 ) ) ;
#74591 = CARTESIAN_POINT ( 'NONE',  ( -7.499999999999947597, 12.43112307739205669, 4.000000000000000000 ) ) ;
#74592 = CYLINDRICAL_SURFACE ( 'NONE', #63750, 2.500000000000000000 ) ;
#74593 = FACE_OUTER_BOUND ( 'NONE', #83952, .T. ) ;
#74594 = FACE_OUTER_BOUND ( 'NONE', #17699, .T. ) ;
#74595 = CARTESIAN_POINT ( 'NONE',  ( 57.42758194782751247, -45.84254607569047124, 35.55177538329026277 ) ) ;
#74596 = EDGE_CURVE ( 'NONE', #3936, #132792, #84522, .T. ) ;
#74598 = ADVANCED_FACE ( 'NONE', ( #141758 ), #86661, .T. ) ;
#74597 = VERTEX_POINT ( 'NONE', #7628 ) ;
#74599 = EDGE_LOOP ( 'NONE', ( #9075, #88833, #27558, #36655, #110980 ) ) ;
#74600 = ORIENTED_EDGE ( 'NONE', *, *, #83805, .F. ) ;
#74601 = CARTESIAN_POINT ( 'NONE',  ( 100.9170968585647756, 3.054999999999998828, 5.291415217122922066 ) ) ;
#74602 = VERTEX_POINT ( 'NONE', #56206 ) ;
#74603 = EDGE_CURVE ( 'NONE', #91909, #2221, #115347, .T. ) ;
#74604 = CARTESIAN_POINT ( 'NONE',  ( 124.4403572661728390, -44.90675832754093477, 35.11767176072991248 ) ) ;
#74605 = CARTESIAN_POINT ( 'NONE',  ( -69.29974487139159578, -27.71228299555254537, 4.000000000000000000 ) ) ;
#74606 = ORIENTED_EDGE ( 'NONE', *, *, #8861, .F. ) ;
#74607 = CARTESIAN_POINT ( 'NONE',  ( 2.510786437626908008, -27.52281430457053446, 5.000000000000000000 ) ) ;
#74608 = CARTESIAN_POINT ( 'NONE',  ( -30.29974487139158867, -27.71228299555227537, 4.000000000000000000 ) ) ;
#74609 = EDGE_CURVE ( 'NONE', #57693, #142882, #101799, .T. ) ;
#74610 = CARTESIAN_POINT ( 'NONE',  ( 98.64126352523145158, 4.472830434245836706, 4.472830434245840259 ) ) ;
#74611 = ORIENTED_EDGE ( 'NONE', *, *, #140993, .F. ) ;
#74612 = AXIS2_PLACEMENT_3D ( 'NONE', #143478, #122431, #121011 ) ;
#74613 = DIRECTION ( 'NONE',  ( 0.000000000000000000, -1.000000000000000000, 0.000000000000000000 ) ) ;
#74614 = LINE ( 'NONE', #31107, #105477 ) ;
#74615 = PLANE ( 'NONE',  #112009 ) ;
#74616 = AXIS2_PLACEMENT_3D ( 'NONE', #13036, #12335, #46451 ) ;
#74617 = DIRECTION ( 'NONE',  ( 0.6830127018922180770, -0.6830127018922204085, -0.2588190451025213501 ) ) ;
#74618 = ORIENTED_EDGE ( 'NONE', *, *, #5682, .F. ) ;
#74619 = ORIENTED_EDGE ( 'NONE', *, *, #21008, .T. ) ;
#74620 = EDGE_LOOP ( 'NONE', ( #108119, #116865, #115555, #44512 ) ) ;
#74621 = DIRECTION ( 'NONE',  ( 0.3543493200069162685, -0.000000000000000000, -0.9351131265310288487 ) ) ;
#74622 = CARTESIAN_POINT ( 'NONE',  ( -19.17183060077633172, -5.240707523384225297, 4.000000000000000000 ) ) ;
#74623 = CARTESIAN_POINT ( 'NONE',  ( 14.35873647476855375, 5.808823158059031044, -5.808823158059037262 ) ) ;
#74624 = EDGE_CURVE ( 'NONE', #70462, #116635, #1033, .T. ) ;
#74625 = STYLED_ITEM ( 'NONE', ( #90709 ), #26149 ) ;
#74626 = LINE ( 'NONE', #5748, #13186 ) ;
#74627 = CARTESIAN_POINT ( 'NONE',  ( 0.1561230773924129900, -22.22500000000000142, 4.000000000000000000 ) ) ;
#74628 = ORIENTED_EDGE ( 'NONE', *, *, #88666, .T. ) ;
#74629 = ORIENTED_EDGE ( 'NONE', *, *, #113395, .T. ) ;
#74630 = CARTESIAN_POINT ( 'NONE',  ( 57.48921356237308800, -27.52281430457095368, 5.000000000000000000 ) ) ;
#74631 = ORIENTED_EDGE ( 'NONE', *, *, #105336, .T. ) ;
#74632 = VERTEX_POINT ( 'NONE', #11177 ) ;
#74633 = VECTOR ( 'NONE', #10562, 999.9999999999998863 ) ;
#74634 = EDGE_CURVE ( 'NONE', #36186, #66777, #35147, .T. ) ;
#74635 = VECTOR ( 'NONE', #96255, 999.9999999999998863 ) ;
#74636 = EDGE_CURVE ( 'NONE', #50410, #108517, #79389, .T. ) ;
#74637 = FACE_OUTER_BOUND ( 'NONE', #26655, .T. ) ;
#74638 = LINE ( 'NONE', #89082, #75246 ) ;
#74639 = VERTEX_POINT ( 'NONE', #314 ) ;
#74640 = PLANE ( 'NONE',  #138533 ) ;
#74641 = CYLINDRICAL_SURFACE ( 'NONE', #94681, 6.094999999999989093 ) ;
#74642 = ADVANCED_FACE ( 'NONE', ( #22766 ), #67044, .F. ) ;
#74643 = LINE ( 'NONE', #73215, #24765 ) ;
#74644 = AXIS2_PLACEMENT_3D ( 'NONE', #121042, #2077, #132686 ) ;
#74645 = CARTESIAN_POINT ( 'NONE',  ( -6.792893218813405909, -5.240707523384232402, 5.000000000000000000 ) ) ;
#74646 = VECTOR ( 'NONE', #94894, 999.9999999999998863 ) ;
#74647 = ORIENTED_EDGE ( 'NONE', *, *, #127599, .F. ) ;
#74648 = EDGE_CURVE ( 'NONE', #109724, #90846, #65656, .T. ) ;
#74649 = LINE ( 'NONE', #41270, #16255 ) ;
#74650 = FACE_OUTER_BOUND ( 'NONE', #76303, .T. ) ;
#74651 = ORIENTED_EDGE ( 'NONE', *, *, #87318, .F. ) ;
#74652 = DIRECTION ( 'NONE',  ( 0.7071067811865486830, -0.7071067811865464625, -0.000000000000000000 ) ) ;
#74653 = DIRECTION ( 'NONE',  ( 0.7071067811865487940, 0.7071067811865463515, 0.000000000000000000 ) ) ;
#74654 = ORIENTED_EDGE ( 'NONE', *, *, #81818, .T. ) ;
#74655 = CARTESIAN_POINT ( 'NONE',  ( 41.99451991528749062, 28.92564299267967343, 4.000000000000000000 ) ) ;
#74656 = ORIENTED_EDGE ( 'NONE', *, *, #101087, .F. ) ;
#74657 = LINE ( 'NONE', #106512, #15747 ) ;
#74658 = EDGE_LOOP ( 'NONE', ( #32460, #126920, #15766, #137206 ) ) ;
#74659 = VERTEX_POINT ( 'NONE', #43864 ) ;
#74660 = VECTOR ( 'NONE', #10877, 1000.000000000000000 ) ;
#74661 = EDGE_CURVE ( 'NONE', #15122, #36919, #22082, .T. ) ;
#74662 = ORIENTED_EDGE ( 'NONE', *, *, #101670, .T. ) ;
#74663 = DIRECTION ( 'NONE',  ( 0.000000000000000000, -1.000000000000000000, 0.000000000000000000 ) ) ;
#74664 = CARTESIAN_POINT ( 'NONE',  ( -2.816011393730999401, 28.73617430169785436, 5.000000000000000000 ) ) ;
#74665 = LINE ( 'NONE', #118854, #139827 ) ;
#74666 = CARTESIAN_POINT ( 'NONE',  ( 126.0004301918981042, -3.055000000000002380, 5.291415217122920289 ) ) ;
#74667 = DIRECTION ( 'NONE',  ( 1.000000000000000000, 0.000000000000000000, 0.000000000000000000 ) ) ;
#74668 = ADVANCED_FACE ( 'NONE', ( #90205 ), #45320, .F. ) ;
#74669 = CARTESIAN_POINT ( 'NONE',  ( 30.70710678118633652, 11.25929247661560773, 5.000000000000000000 ) ) ;
#74670 = DIRECTION ( 'NONE',  ( -0.6830127018922181881, 0.6830127018922202975, -0.2588190451025214056 ) ) ;
#74671 = VECTOR ( 'NONE', #115137, 1000.000000000000000 ) ;
#74672 = VECTOR ( 'NONE', #68480, 999.9999999999998863 ) ;
#74673 = VECTOR ( 'NONE', #142385, 999.9999999999998863 ) ;
#74674 = DIRECTION ( 'NONE',  ( -0.3543493200069162685, -0.000000000000000000, -0.9351131265310288487 ) ) ;
#74675 = AXIS2_PLACEMENT_3D ( 'NONE', #28688, #26529, #61344 ) ;
#74676 = VECTOR ( 'NONE', #20949, 1000.000000000000000 ) ;
#74677 = CARTESIAN_POINT ( 'NONE',  ( -48.18398860626899705, 28.73617430169820608, 5.000000000000000000 ) ) ;
#74678 = DIRECTION ( 'NONE',  ( -0.7071067811865486830, 0.7071067811865464625, 0.000000000000000000 ) ) ;
#74679 = CARTESIAN_POINT ( 'NONE',  ( -30.29974487139158867, -27.71228299555227537, 4.000000000000000000 ) ) ;
#74680 = ORIENTED_EDGE ( 'NONE', *, *, #117997, .F. ) ;
#74681 = EDGE_LOOP ( 'NONE', ( #84572, #17356, #110825, #95818 ) ) ;
#74682 = VECTOR ( 'NONE', #113250, 1000.000000000000000 ) ;
#74683 = ORIENTED_EDGE ( 'NONE', *, *, #126927, .F. ) ;
#74684 = VECTOR ( 'NONE', #9624, 1000.000000000000000 ) ;
#74685 = EDGE_LOOP ( 'NONE', ( #109614, #106602, #135020, #87196 ) ) ;
#74686 = STYLED_ITEM ( 'NONE', ( #65187 ), #34315 ) ;
#74687 = DIRECTION ( 'NONE',  ( -1.000000000000000000, -1.224606353822377258E-16, -0.000000000000000000 ) ) ;
#74688 = ORIENTED_EDGE ( 'NONE', *, *, #41673, .F. ) ;
#74689 = EDGE_LOOP ( 'NONE', ( #5119, #129761, #108919, #64645 ) ) ;
#74690 = CARTESIAN_POINT ( 'NONE',  ( -13.49999999999990763, 6.431123077392117082, 4.000000000000000000 ) ) ;
#74691 = DIRECTION ( 'NONE',  ( -0.3543493200069162685, -0.000000000000000000, -0.9351131265310288487 ) ) ;
#74692 = EDGE_CURVE ( 'NONE', #85310, #106451, #30586, .T. ) ;
#74693 = DIRECTION ( 'NONE',  ( 0.3543493200069162685, -0.000000000000000000, -0.9351131265310288487 ) ) ;
#74694 = EDGE_CURVE ( 'NONE', #6269, #81442, #10488, .T. ) ;
#74695 = ORIENTED_EDGE ( 'NONE', *, *, #615, .F. ) ;
#74696 = CARTESIAN_POINT ( 'NONE',  ( -16.99806943317890173, -22.22500000000000142, 4.500000000000000888 ) ) ;
#74697 = ORIENTED_EDGE ( 'NONE', *, *, #68569, .T. ) ;
#74698 = CARTESIAN_POINT ( 'NONE',  ( -15.67180000000000284, 3.174999999999997158, 1.444000000000000394 ) ) ;
#74699 = EDGE_CURVE ( 'NONE', #128485, #66817, #23520, .T. ) ;
#74700 = CARTESIAN_POINT ( 'NONE',  ( 29.99451991528749417, 28.92564299267958816, 4.000000000000000000 ) ) ;
#74701 = VECTOR ( 'NONE', #102543, 1000.000000000000227 ) ;
#74702 = CARTESIAN_POINT ( 'NONE',  ( 14.35873647476855197, 5.808823158059031044, -5.808823158059038150 ) ) ;
#74703 = ORIENTED_EDGE ( 'NONE', *, *, #43420, .F. ) ;
#74704 = CARTESIAN_POINT ( 'NONE',  ( 87.55793019189812298, 6.110000000000001208, -1.637169565754156286 ) ) ;
#74705 = DIRECTION ( 'NONE',  ( -0.7071067811865487940, 0.7071067811865463515, 0.000000000000000000 ) ) ;
#74706 = CARTESIAN_POINT ( 'NONE',  ( 2.671830600776454734, 2.259292476615692546, 4.000000000000000000 ) ) ;
#74707 = LINE ( 'NONE', #142103, #125257 ) ;
#74708 = ORIENTED_EDGE ( 'NONE', *, *, #4492, .T. ) ;
#74709 = ORIENTED_EDGE ( 'NONE', *, *, #102336, .T. ) ;
#74710 = LINE ( 'NONE', #118151, #38077 ) ;
#74711 = EDGE_LOOP ( 'NONE', ( #119647, #109835, #103638, #65248 ) ) ;
#74712 = FACE_OUTER_BOUND ( 'NONE', #23422, .T. ) ;
#74713 = CARTESIAN_POINT ( 'NONE',  ( -9.489213562373095101, -27.52281430457062328, 5.000000000000000000 ) ) ;
#74714 = DIRECTION ( 'NONE',  ( -0.7071067811865486830, -0.7071067811865464625, 0.000000000000000000 ) ) ;
#74715 = CARTESIAN_POINT ( 'NONE',  ( 36.48921356237310221, -27.52281430457080802, 5.000000000000000000 ) ) ;
#74717 = EDGE_CURVE ( 'NONE', #108713, #89253, #68495, .T. ) ;
#74716 = ORIENTED_EDGE ( 'NONE', *, *, #134996, .T. ) ;
#74718 = AXIS2_PLACEMENT_3D ( 'NONE', #97444, #86611, #19887 ) ;
#74719 = DIRECTION ( 'NONE',  ( 0.000000000000000000, -1.000000000000000000, 0.000000000000000000 ) ) ;
#74720 = EDGE_CURVE ( 'NONE', #126557, #72219, #77232, .T. ) ;
#74721 = VECTOR ( 'NONE', #74341, 1000.000000000000000 ) ;
#74722 =( NAMED_UNIT ( * ) SI_UNIT ( $, .STERADIAN. ) SOLID_ANGLE_UNIT ( ) );
#74723 = DIRECTION ( 'NONE',  ( -0.7071067811865487940, 0.7071067811865463515, -0.000000000000000000 ) ) ;
#74724 = ORIENTED_EDGE ( 'NONE', *, *, #59320, .F. ) ;
#74725 = PLANE ( 'NONE',  #92949 ) ;
#74726 = FACE_OUTER_BOUND ( 'NONE', #68160, .T. ) ;
#74727 = ORIENTED_EDGE ( 'NONE', *, *, #35355, .F. ) ;
#74729 = ORIENTED_EDGE ( 'NONE', *, *, #95027, .T. ) ;
#74728 = CARTESIAN_POINT ( 'NONE',  ( 0.3394530118782473349, -51.90335959434331414, -39.28179725402795697 ) ) ;
#74730 = ORIENTED_EDGE ( 'NONE', *, *, #128941, .T. ) ;
#74731 = ADVANCED_FACE ( 'NONE', ( #138009 ), #50291, .F. ) ;
#74732 = FACE_OUTER_BOUND ( 'NONE', #46074, .T. ) ;
#74733 = DIRECTION ( 'NONE',  ( 0.6830127018922181881, 0.6830127018922202975, -0.2588190451025214056 ) ) ;
#74734 = ORIENTED_EDGE ( 'NONE', *, *, #87596, .T. ) ;
#74735 = CARTESIAN_POINT ( 'NONE',  ( 156.1500000000000057, -49.14999999999999147, 53.92499999999997584 ) ) ;
#74736 = CARTESIAN_POINT ( 'NONE',  ( -1.499999999999987566, 13.56627193232215056, -10.57019076586069062 ) ) ;
#74737 = LINE ( 'NONE', #108016, #53036 ) ;
#74738 =( BOUNDED_CURVE ( )  B_SPLINE_CURVE ( 3, ( #37950, #26348, #138692, #103868 ),
 .UNSPECIFIED., .F., .T. ) 
 B_SPLINE_CURVE_WITH_KNOTS ( ( 4, 4 ),
 ( 1.901594255663612065, 1.933014472006554740 ),
 .UNSPECIFIED. ) 
 CURVE ( )  GEOMETRIC_REPRESENTATION_ITEM ( )  RATIONAL_B_SPLINE_CURVE ( ( 1.000000000000000000, 0.9999177325257868620, 0.9999177325257868620, 1.000000000000000000 ) ) 
 REPRESENTATION_ITEM ( '' )  );
#74739 = DIRECTION ( 'NONE',  ( 0.7071067811865487940, 0.7071067811865463515, -0.000000000000000000 ) ) ;
#74740 = CARTESIAN_POINT ( 'NONE',  ( 34.92499999999998295, 16.70193056682081334, 4.500000000000000888 ) ) ;
#74741 = FACE_OUTER_BOUND ( 'NONE', #92839, .T. ) ;
#74742 = AXIS2_PLACEMENT_3D ( 'NONE', #3775, #66946, #22677 ) ;
#74743 = CARTESIAN_POINT ( 'NONE',  ( 10.49999999999993072, 9.431123077392090437, 4.000000000000000000 ) ) ;
#74744 = PLANE ( 'NONE',  #14135 ) ;
#74745 = DIRECTION ( 'NONE',  ( 0.7071067811865487940, -0.7071067811865463515, 0.000000000000000000 ) ) ;
#74746 = DIRECTION ( 'NONE',  ( 0.7071067811865487940, 0.7071067811865463515, 0.000000000000000000 ) ) ;
#74747 = AXIS2_PLACEMENT_3D ( 'NONE', #89534, #34444, #22121 ) ;
#74748 = FACE_OUTER_BOUND ( 'NONE', #85428, .T. ) ;
#74749 = DIRECTION ( 'NONE',  ( 0.5735764363510451602, 0.8191520442889924647, 0.000000000000000000 ) ) ;
#74750 =( NAMED_UNIT ( * ) PLANE_ANGLE_UNIT ( ) SI_UNIT ( $, .RADIAN. ) );
#74751 = ORIENTED_EDGE ( 'NONE', *, *, #108480, .T. ) ;
#74752 = ORIENTED_EDGE ( 'NONE', *, *, #98817, .T. ) ;
#74753 = EDGE_LOOP ( 'NONE', ( #132230, #95651, #15611, #84817 ) ) ;
#74754 = CARTESIAN_POINT ( 'NONE',  ( 108.9166666666666572, -6.884901960086287076, -3.975000000000000977 ) ) ;
#74756 = EDGE_CURVE ( 'NONE', #55173, #53059, #61212, .T. ) ;
#74755 = VERTEX_POINT ( 'NONE', #103910 ) ;
#74757 = ORIENTED_EDGE ( 'NONE', *, *, #2742, .T. ) ;
#74758 = ORIENTED_EDGE ( 'NONE', *, *, #43307, .T. ) ;
#74759 = DIRECTION ( 'NONE',  ( -0.7071067811865487940, 0.7071067811865463515, -0.000000000000000000 ) ) ;
#74760 = DIRECTION ( 'NONE',  ( -0.3543493200069162685, -0.000000000000000000, -0.9351131265310288487 ) ) ;
#74761 = VECTOR ( 'NONE', #13590, 1000.000000000000000 ) ;
#74762 = VERTEX_POINT ( 'NONE', #92328 ) ;
#74763 = DIRECTION ( 'NONE',  ( -0.000000000000000000, 0.3543493200069153248, 0.9351131265310292928 ) ) ;
#74764 = EDGE_CURVE ( 'NONE', #84565, #140843, #91642, .T. ) ;
#74765 = CARTESIAN_POINT ( 'NONE',  ( 10.82816939922345156, 18.75929247661552424, 4.000000000000000000 ) ) ;
#74766 = CARTESIAN_POINT ( 'NONE',  ( -27.48921356237309155, -27.52281430457074762, 5.000000000000000000 ) ) ;
#74767 = CARTESIAN_POINT ( 'NONE',  ( -72.48921356237309510, -27.52281430457106026, 5.000000000000000000 ) ) ;
#74768 = CARTESIAN_POINT ( 'NONE',  ( 105.7295968585647898, -6.110000000000000320, -1.637169565754161393 ) ) ;
#74769 = ORIENTED_EDGE ( 'NONE', *, *, #86907, .T. ) ;
#74770 = ADVANCED_FACE ( 'NONE', ( #94478 ), #103216, .F. ) ;
#74771 = CARTESIAN_POINT ( 'NONE',  ( 22.56687199751243611, -21.74070752338406720, 6.915939825044020495 ) ) ;
#74773 = AXIS2_PLACEMENT_3D ( 'NONE', #73862, #16609, #93474 ) ;
#74772 = CARTESIAN_POINT ( 'NONE',  ( -10.17183060077640278, 12.75929247661558996, 4.000000000000000000 ) ) ;
#74774 = DIRECTION ( 'NONE',  ( -0.7071067811865487940, 0.7071067811865463515, -0.000000000000000000 ) ) ;
#74775 = DIRECTION ( 'NONE',  ( -0.3543493200069162685, -0.000000000000000000, -0.9351131265310288487 ) ) ;
#74776 = DIRECTION ( 'NONE',  ( -8.673617379884025611E-16, 0.000000000000000000, 1.000000000000000000 ) ) ;
#74777 = CARTESIAN_POINT ( 'NONE',  ( 6.639999999999993463, -34.51840020119762897, 17.97447928118983285 ) ) ;
#74778 = EDGE_CURVE ( 'NONE', #31340, #95370, #4559, .T. ) ;
#74779 = ADVANCED_FACE ( 'NONE', ( #125717 ), #27088, .F. ) ;
#74780 = VERTEX_POINT ( 'NONE', #70645 ) ;
#74781 = VERTEX_POINT ( 'NONE', #24937 ) ;
#74782 = CARTESIAN_POINT ( 'NONE',  ( 29.58333333333332149, 6.884901960086290629, -3.974999999999994316 ) ) ;
#74783 = ADVANCED_FACE ( 'NONE', ( #3190 ), #125469, .T. ) ;
#74784 = ORIENTED_EDGE ( 'NONE', *, *, #6981, .F. ) ;
#74785 = LINE ( 'NONE', #6590, #53277 ) ;
#74786 = EDGE_CURVE ( 'NONE', #141528, #34917, #82922, .T. ) ;
#74787 = CARTESIAN_POINT ( 'NONE',  ( 23.99999999999982947, 19.93112307739197675, 4.000000000000000000 ) ) ;
#74788 = VECTOR ( 'NONE', #123400, 1000.000000000000227 ) ;
#74789 = ADVANCED_FACE ( 'NONE', ( #135864 ), #83791, .T. ) ;
#74790 = CARTESIAN_POINT ( 'NONE',  ( 23.54739889332687497, 7.099584588756134629, 5.000000000000000000 ) ) ;
#74791 = CARTESIAN_POINT ( 'NONE',  ( 5.669897814527313784, 17.25929247661553845, 19.83885114516069947 ) ) ;
#74792 = VECTOR ( 'NONE', #36520, 1000.000000000000000 ) ;
#74793 = CARTESIAN_POINT ( 'NONE',  ( -27.70710678118634718, -9.740707523384177335, 5.000000000000000000 ) ) ;
#74795 = VECTOR ( 'NONE', #132982, 1000.000000000000227 ) ;
#74794 = DIRECTION ( 'NONE',  ( 0.000000000000000000, 0.000000000000000000, 1.000000000000000000 ) ) ;
#74796 = EDGE_CURVE ( 'NONE', #122347, #52394, #104647, .T. ) ;
#74797 = CARTESIAN_POINT ( 'NONE',  ( 120.2245968585648086, -1.637169565754160949, 6.109999999999997655 ) ) ;
#74798 = ORIENTED_EDGE ( 'NONE', *, *, #138809, .F. ) ;
#74799 = CARTESIAN_POINT ( 'NONE',  ( 0.000000000000000000, -4.870000000000014317, -36.99999999997771738 ) ) ;
#74800 = ORIENTED_EDGE ( 'NONE', *, *, #46335, .T. ) ;
#74801 = VECTOR ( 'NONE', #65611, 1000.000000000000000 ) ;
#74802 = VECTOR ( 'NONE', #85981, 1000.000000000000000 ) ;
#74803 = CARTESIAN_POINT ( 'NONE',  ( 70.51669371712954160, 7.950000000000000178, -2.130196079827421318 ) ) ;
#74804 = LINE ( 'NONE', #3595, #47833 ) ;
#74805 = DIRECTION ( 'NONE',  ( 0.7071067811865486830, -0.7071067811865464625, -0.000000000000000000 ) ) ;
#74806 = ADVANCED_FACE ( 'NONE', ( #27806 ), #5320, .F. ) ;
#74807 = CARTESIAN_POINT ( 'NONE',  ( 17.16170612452609490, -6.740707523384205757, 16.75550250614871217 ) ) ;
#74808 = ORIENTED_EDGE ( 'NONE', *, *, #58312, .T. ) ;
#74809 = CARTESIAN_POINT ( 'NONE',  ( 46.22959685856476852, -6.110000000000000320, -1.637169565754161393 ) ) ;
#74810 = EDGE_LOOP ( 'NONE', ( #36592, #30631, #47293, #6170 ) ) ;
#74811 = LINE ( 'NONE', #87790, #14426 ) ;
#74812 = LINE ( 'NONE', #95809, #138781 ) ;
#74813 = FACE_OUTER_BOUND ( 'NONE', #99150, .T. ) ;
#74814 = CARTESIAN_POINT ( 'NONE',  ( -11.99451991528749417, 28.92564299267946382, 4.000000000000000000 ) ) ;
#74815 = EDGE_CURVE ( 'NONE', #3936, #108682, #81509, .T. ) ;
#74816 = CARTESIAN_POINT ( 'NONE',  ( 39.72459685856478018, -1.637169565754160949, 6.109999999999997655 ) ) ;
#74817 = VERTEX_POINT ( 'NONE', #36545 ) ;
#74818 = CARTESIAN_POINT ( 'NONE',  ( 14.29298673570684919, -21.74070752338406365, 4.999753212805221558 ) ) ;
#74819 = ORIENTED_EDGE ( 'NONE', *, *, #89348, .T. ) ;
#74820 = ORIENTED_EDGE ( 'NONE', *, *, #70429, .T. ) ;
#74821 = ORIENTED_EDGE ( 'NONE', *, *, #17475, .F. ) ;
#74822 = AXIS2_PLACEMENT_3D ( 'NONE', #129019, #29695, #118115 ) ;
#74823 = PRODUCT_DEFINITION_SHAPE ( 'NONE', 'NONE',  #143562 ) ;
#74824 = CARTESIAN_POINT ( 'NONE',  ( 22.53999999999999915, 2.055000000000001492, 0.000000000000000000 ) ) ;
#74825 = UNCERTAINTY_MEASURE_WITH_UNIT (LENGTH_MEASURE( 1.000000000000000082E-05 ), #73720, 'distance_accuracy_value', 'NONE');
#74826 = ORIENTED_EDGE ( 'NONE', *, *, #119993, .F. ) ;
#74827 = DIRECTION ( 'NONE',  ( -1.734723475976806848E-16, 1.000000000000000000, 0.000000000000000000 ) ) ;
#74828 = EDGE_CURVE ( 'NONE', #38388, #70673, #25660, .T. ) ;
#74829 = CARTESIAN_POINT ( 'NONE',  ( 24.48921356237309510, -27.52281430457072631, 5.000000000000000000 ) ) ;
#74830 = ADVANCED_FACE ( 'NONE', ( #114788 ), #113372, .F. ) ;
#74831 = FACE_OUTER_BOUND ( 'NONE', #69250, .T. ) ;
#74832 = FACE_BOUND ( 'NONE', #52950, .T. ) ;
#74833 = EDGE_LOOP ( 'NONE', ( #27458, #33471, #31318, #78579 ) ) ;
#74834 = LINE ( 'NONE', #8770, #119744 ) ;
#74835 = DIRECTION ( 'NONE',  ( 0.7071067811865487940, -0.7071067811865463515, 0.000000000000000000 ) ) ;
#74836 = CARTESIAN_POINT ( 'NONE',  ( 0.1839886062690032631, 28.73617430169787568, 5.000000000000000000 ) ) ;
#74837 = VERTEX_POINT ( 'NONE', #116246 ) ;
#74838 = CARTESIAN_POINT ( 'NONE',  ( -78.29974487139158157, -27.71228299555260577, 4.000000000000000000 ) ) ;
#74839 = ORIENTED_EDGE ( 'NONE', *, *, #117089, .F. ) ;
#74840 = ORIENTED_EDGE ( 'NONE', *, *, #6826, .T. ) ;
#74841 = DIRECTION ( 'NONE',  ( -1.000000000000000000, -1.224606353822377258E-16, -0.000000000000000000 ) ) ;
#74842 = VERTEX_POINT ( 'NONE', #102540 ) ;
#74843 = VECTOR ( 'NONE', #18885, 1000.000000000000000 ) ;
#74844 = CARTESIAN_POINT ( 'NONE',  ( 55.47459685856477307, 1.637169565754164280, -6.109999999999996767 ) ) ;
#74846 = ORIENTED_EDGE ( 'NONE', *, *, #99080, .T. ) ;
#74845 = VECTOR ( 'NONE', #73624, 1000.000000000000000 ) ;
#74847 = PLANE ( 'NONE',  #32592 ) ;
#74848 = CARTESIAN_POINT ( 'NONE',  ( 33.18398860626899705, 28.73617430169810305, 5.000000000000000000 ) ) ;
#74849 = EDGE_CURVE ( 'NONE', #40992, #71472, #47474, .T. ) ;
#74850 = VECTOR ( 'NONE', #107608, 1000.000000000000000 ) ;
#74851 = VERTEX_POINT ( 'NONE', #20475 ) ;
#74852 = CARTESIAN_POINT ( 'NONE',  ( 29.99999999999979039, 8.966399257802173395, 5.000000000000000000 ) ) ;
#74853 = CYLINDRICAL_SURFACE ( 'NONE', #124596, 7.950000000000000178 ) ;
#74854 = VECTOR ( 'NONE', #60149, 999.9999999999998863 ) ;
#74855 = LINE ( 'NONE', #119032, #110331 ) ;
#74856 = EDGE_CURVE ( 'NONE', #11235, #80300, #86488, .T. ) ;
#74857 = LINE ( 'NONE', #29872, #85197 ) ;
#74858 = CARTESIAN_POINT ( 'NONE',  ( -60.29974487139158867, -27.71228299555248142, 4.000000000000000000 ) ) ;
#74859 = DIRECTION ( 'NONE',  ( -0.6830127018922180770, -0.6830127018922202975, -0.2588190451025213501 ) ) ;
#74860 = CARTESIAN_POINT ( 'NONE',  ( 5.999999999999972466, 4.552185695429124657, 5.000000000000000000 ) ) ;
#74861 = VERTEX_POINT ( 'NONE', #129243 ) ;
#74862 = VECTOR ( 'NONE', #103069, 1000.000000000000000 ) ;
#74863 = EDGE_LOOP ( 'NONE', ( #56949, #132796, #124056 ) ) ;
#74864 = DIRECTION ( 'NONE',  ( 1.000000000000000000, 0.000000000000000000, 0.000000000000000000 ) ) ;
#74865 = CARTESIAN_POINT ( 'NONE',  ( -27.18398860626900060, 28.73617430169806042, 5.000000000000000000 ) ) ;
#74866 = ORIENTED_EDGE ( 'NONE', *, *, #134742, .F. ) ;
#74867 = VERTEX_POINT ( 'NONE', #130719 ) ;
#74868 = ORIENTED_EDGE ( 'NONE', *, *, #42171, .F. ) ;
#74869 = DIRECTION ( 'NONE',  ( -0.7071067811865486830, 0.7071067811865464625, 0.000000000000000000 ) ) ;
#74870 = CARTESIAN_POINT ( 'NONE',  ( 0.000000000000000000, -21.72500000000000142, 4.500000000000000888 ) ) ;
#74871 = ADVANCED_FACE ( 'NONE', ( #42987 ), #95915, .F. ) ;
#74872 = ADVANCED_FACE ( 'NONE', ( #9592 ), #108903, .F. ) ;
#74873 = DIRECTION ( 'NONE',  ( 0.7071067811865486830, -0.7071067811865464625, -0.000000000000000000 ) ) ;
#74874 = VECTOR ( 'NONE', #87965, 1000.000000000000000 ) ;
#74875 = EDGE_LOOP ( 'NONE', ( #137464, #3690, #68345, #28152, #70814, #32984 ) ) ;
#74876 = CARTESIAN_POINT ( 'NONE',  ( 18.18398860626898994, 28.73617430169800002, 5.000000000000000000 ) ) ;
#74877 = LINE ( 'NONE', #107460, #7578 ) ;
#74878 = CARTESIAN_POINT ( 'NONE',  ( 18.15040314143522338, 7.934999999999989839, -2.126176841940961904 ) ) ;
#74879 = ORIENTED_EDGE ( 'NONE', *, *, #53279, .T. ) ;
#74881 = ADVANCED_FACE ( 'NONE', ( #116953 ), #127859, .T. ) ;
#74880 = CARTESIAN_POINT ( 'NONE',  ( 119.3495968585647944, 6.109999999999997655, 1.637169565754163836 ) ) ;
#74882 = CARTESIAN_POINT ( 'NONE',  ( 0.000000000000000000, -19.06887692260762535, 4.000000000000000000 ) ) ;
#74883 = DIRECTION ( 'NONE',  ( -0.7071067811865486830, 0.7071067811865464625, 0.000000000000000000 ) ) ;
#74884 = AXIS2_PLACEMENT_3D ( 'NONE', #6525, #93601, #18878 ) ;
#74886 = ORIENTED_EDGE ( 'NONE', *, *, #100398, .T. ) ;
#74885 = LINE ( 'NONE', #96562, #44930 ) ;
#74887 = CARTESIAN_POINT ( 'NONE',  ( -22.49999999999984013, -20.94781430457062044, 5.000000000000000000 ) ) ;
#74888 = VERTEX_POINT ( 'NONE', #74175 ) ;
#74889 = CARTESIAN_POINT ( 'NONE',  ( -15.70710678118642711, -15.74070752338412404, 5.000000000000000000 ) ) ;
#74890 = DIRECTION ( 'NONE',  ( 0.7071067811865487940, -0.7071067811865463515, 0.000000000000000000 ) ) ;
#74891 = DIRECTION ( 'NONE',  ( -0.000000000000000000, 1.000000000000000000, -0.000000000000000000 ) ) ;
#74893 = ORIENTED_EDGE ( 'NONE', *, *, #55397, .F. ) ;
#74892 = VECTOR ( 'NONE', #121170, 999.9999999999998863 ) ;
#74894 = ADVANCED_FACE ( 'NONE', ( #106049 ), #37526, .T. ) ;
#74895 = CARTESIAN_POINT ( 'NONE',  ( -2.999999999999975131, -7.447814304570750998, 5.000000000000000000 ) ) ;
#74896 = DIRECTION ( 'NONE',  ( 0.000000000000000000, 1.000000000000000000, 5.782411586589357244E-15 ) ) ;
#74897 = VECTOR ( 'NONE', #139684, 1000.000000000000000 ) ;
#74898 = ORIENTED_EDGE ( 'NONE', *, *, #63013, .T. ) ;
#74899 = FACE_OUTER_BOUND ( 'NONE', #104876, .T. ) ;
#74900 = DIRECTION ( 'NONE',  ( -0.000000000000000000, 0.000000000000000000, 1.000000000000000000 ) ) ;
#74901 = LINE ( 'NONE', #17608, #102506 ) ;
#74902 = ORIENTED_EDGE ( 'NONE', *, *, #44684, .T. ) ;
#74903 = CARTESIAN_POINT ( 'NONE',  ( 3.645833333333334370, -1.633150327867695095, 6.094999999999987317 ) ) ;
#74904 = DIRECTION ( 'NONE',  ( -0.7071067811865486830, 0.7071067811865464625, 0.000000000000000000 ) ) ;
#74905 = EDGE_LOOP ( 'NONE', ( #9242, #40974, #9971, #5590 ) ) ;
#74906 = EDGE_CURVE ( 'NONE', #130610, #84223, #30683, .T. ) ;
#74907 = ORIENTED_EDGE ( 'NONE', *, *, #55659, .F. ) ;
#74908 = CARTESIAN_POINT ( 'NONE',  ( 20.99451991528748707, 28.92564299267952777, 4.000000000000000000 ) ) ;
#74909 = DIRECTION ( 'NONE',  ( -1.000000000000000000, 0.000000000000000000, 0.000000000000000000 ) ) ;
#74910 = VECTOR ( 'NONE', #30613, 1000.000000000000000 ) ;
#74911 = CARTESIAN_POINT ( 'NONE',  ( 10.04123647476855297, 0.000000000000000000, 7.934999999999990727 ) ) ;
#74912 = CARTESIAN_POINT ( 'NONE',  ( 0.000000000000000000, 1.163414459189985682E-15, -9.500000000000001776 ) ) ;
#74913 = AXIS2_PLACEMENT_3D ( 'NONE', #87022, #111632, #44251 ) ;
#74914 = DIRECTION ( 'NONE',  ( -0.000000000000000000, 0.3543493200069153248, 0.9351131265310292928 ) ) ;
#74915 = DIRECTION ( 'NONE',  ( -0.000000000000000000, -0.3543493200069152693, 0.9351131265310292928 ) ) ;
#74916 = EDGE_LOOP ( 'NONE', ( #3974, #32405, #125374, #93166 ) ) ;
#74917 = SURFACE_STYLE_USAGE ( .BOTH. , #10323 ) ;
#74918 = DIRECTION ( 'NONE',  ( 0.3543493200069162685, -0.000000000000000000, -0.9351131265310288487 ) ) ;
#74919 = DIRECTION ( 'NONE',  ( -0.000000000000000000, 0.3543493200069153248, 0.9351131265310292928 ) ) ;
#74920 = LINE ( 'NONE', #53878, #1936 ) ;
#74921 = CARTESIAN_POINT ( 'NONE',  ( 33.59959685856477307, -6.109999999999998543, -1.637169565754160727 ) ) ;
#74922 = CARTESIAN_POINT ( 'NONE',  ( -25.49999999999981526, 3.052185695429136647, 5.000000000000000000 ) ) ;
#74923 = VERTEX_POINT ( 'NONE', #128555 ) ;
#74924 = CARTESIAN_POINT ( 'NONE',  ( 2.999999999999976463, -19.22509904557636418, 1.855685503482186638 ) ) ;
#74925 = AXIS2_PLACEMENT_3D ( 'NONE', #90175, #11890, #45292 ) ;
#74926 = EDGE_LOOP ( 'NONE', ( #136463, #37899, #20190 ) ) ;
#74927 = ORIENTED_EDGE ( 'NONE', *, *, #7460, .F. ) ;
#74928 = DIRECTION ( 'NONE',  ( -0.000000000000000000, -0.3543493200069152693, 0.9351131265310292928 ) ) ;
#74929 = CARTESIAN_POINT ( 'NONE',  ( -28.49999999999980460, 1.030536316426487797, -5.498701923753732679 ) ) ;
#74930 = ORIENTED_EDGE ( 'NONE', *, *, #96129, .T. ) ;
#74931 = DIRECTION ( 'NONE',  ( 0.3543493200069162685, -0.000000000000000000, -0.9351131265310288487 ) ) ;
#74933 = VECTOR ( 'NONE', #119239, 1000.000000000000000 ) ;
#74932 = LINE ( 'NONE', #19089, #113666 ) ;
#74934 = FACE_OUTER_BOUND ( 'NONE', #28810, .T. ) ;
#74935 = DIRECTION ( 'NONE',  ( -0.000000000000000000, 0.000000000000000000, 1.000000000000000000 ) ) ;
#74936 = CARTESIAN_POINT ( 'NONE',  ( 24.29974487139158867, -27.71228299555223273, 4.000000000000000000 ) ) ;
#74937 = ORIENTED_EDGE ( 'NONE', *, *, #74634, .T. ) ;
#74938 = CARTESIAN_POINT ( 'NONE',  ( 32.87852683662832476, -20.24070752338407431, 7.412974875817714526 ) ) ;
#74939 = DIRECTION ( 'NONE',  ( 0.6830127018922181881, 0.6830127018922202975, -0.2588190451025214056 ) ) ;
#74940 = LINE ( 'NONE', #51749, #75120 ) ;
#74941 = DIRECTION ( 'NONE',  ( -0.7071067811865487940, 0.7071067811865463515, 0.000000000000000000 ) ) ;
#74942 = CARTESIAN_POINT ( 'NONE',  ( -5.206660635421487271, 21.75929247661549937, 4.998822639870708073 ) ) ;
#74943 = SURFACE_STYLE_USAGE ( .BOTH. , #49084 ) ;
#74944 = CARTESIAN_POINT ( 'NONE',  ( 0.000000000000000000, 0.000000000000000000, 5.000000000000000000 ) ) ;
#74945 = VECTOR ( 'NONE', #130278, 1000.000000000000114 ) ;
#74946 = CARTESIAN_POINT ( 'NONE',  ( 53.30836038379623432, 7.949999999999997513, 2.130196079827431088 ) ) ;
#74947 = EDGE_CURVE ( 'NONE', #13986, #27362, #107504, .T. ) ;
#74948 = VECTOR ( 'NONE', #93385, 1000.000000000000000 ) ;
#74949 = CARTESIAN_POINT ( 'NONE',  ( -63.18398860626900415, 28.73617430169831621, 5.000000000000000000 ) ) ;
#74950 = VERTEX_POINT ( 'NONE', #42276 ) ;
#74951 = ORIENTED_EDGE ( 'NONE', *, *, #125148, .T. ) ;
#74952 = CARTESIAN_POINT ( 'NONE',  ( 55.83333333333332860, -6.884901960086287964, 3.974999999999998312 ) ) ;
#74953 = LINE ( 'NONE', #116987, #128038 ) ;
#74954 = EDGE_CURVE ( 'NONE', #113754, #16, #64721, .T. ) ;
#74955 = CARTESIAN_POINT ( 'NONE',  ( 19.05000000000000071, 3.174999999999997158, 1.444000000000000394 ) ) ;
#74956 = ADVANCED_FACE ( 'NONE', ( #140156 ), #6716, .F. ) ;
#74957 = VECTOR ( 'NONE', #120920, 1000.000000000000000 ) ;
#74958 =( LENGTH_UNIT ( ) NAMED_UNIT ( * ) SI_UNIT ( .MILLI., .METRE. ) );
#74959 = ORIENTED_EDGE ( 'NONE', *, *, #20755, .F. ) ;
#74960 = EDGE_CURVE ( 'NONE', #68410, #86186, #72799, .T. ) ;
#74961 = FACE_OUTER_BOUND ( 'NONE', #46705, .T. ) ;
#74962 = CARTESIAN_POINT ( 'NONE',  ( 50.60459685856477563, 1.637169565754164946, -6.109999999999999432 ) ) ;
#74963 = EDGE_LOOP ( 'NONE', ( #54872, #104976, #32526, #24581 ) ) ;
#74964 = CARTESIAN_POINT ( 'NONE',  ( 34.42499999999998295, -10.45860074219784330, 5.000000000000000000 ) ) ;
#74965 = ORIENTED_EDGE ( 'NONE', *, *, #125848, .F. ) ;
#74966 = ORIENTED_EDGE ( 'NONE', *, *, #8281, .F. ) ;
#74967 = DIRECTION ( 'NONE',  ( 0.7071067811865487940, -0.7071067811865463515, 0.000000000000000000 ) ) ;
#74968 = CARTESIAN_POINT ( 'NONE',  ( -26.99999999999981526, -6.108550654416982972, -3.114665004255028791 ) ) ;
#74969 = CARTESIAN_POINT ( 'NONE',  ( 34.42499999999998295, 0.000000000000000000, 4.500000000000000888 ) ) ;
#74970 = EDGE_CURVE ( 'NONE', #121677, #60780, #63332, .T. ) ;
#74971 = LINE ( 'NONE', #108967, #20868 ) ;
#74972 = VERTEX_POINT ( 'NONE', #19068 ) ;
#74973 = EDGE_CURVE ( 'NONE', #42501, #85630, #7456, .T. ) ;
#74974 = CARTESIAN_POINT ( 'NONE',  ( 93.75000000000000000, -9.735942053221458872E-16, 7.950000000000000178 ) ) ;
#74976 = EDGE_LOOP ( 'NONE', ( #131143, #21040, #66801, #85663 ) ) ;
#74975 = CARTESIAN_POINT ( 'NONE',  ( -21.60769999999998703, 3.130000000000008331, 0.000000000000000000 ) ) ;
#74977 = CARTESIAN_POINT ( 'NONE',  ( 82.83376352523144703, 6.110000000000001208, 1.122388791418549305E-15 ) ) ;
#74978 = CARTESIAN_POINT ( 'NONE',  ( 14.72916666666666607, -6.094999999999989093, 1.633150327867691542 ) ) ;
#74979 = CARTESIAN_POINT ( 'NONE',  ( 52.26932219902318622, -52.14999999999999147, -40.92499999999998295 ) ) ;
#74980 = CIRCLE ( 'NONE', #130532, 5.968999999999998529 ) ;
#74981 = DIRECTION ( 'NONE',  ( 0.000000000000000000, 0.000000000000000000, -1.000000000000000000 ) ) ;
#74982 = EDGE_CURVE ( 'NONE', #29768, #31472, #64014, .T. ) ;
#74983 = ORIENTED_EDGE ( 'NONE', *, *, #11423, .F. ) ;
#74984 = COLOUR_RGB ( '', 0.72549020, 0.75294118, 0.79215686) ;
#74985 = PLANE ( 'NONE',  #91643 ) ;
#74986 = CARTESIAN_POINT ( 'NONE',  ( 63.20376352523145158, 6.109999999999998543, 1.122388791418548911E-15 ) ) ;
#74987 = DIRECTION ( 'NONE',  ( -0.7071067811865486830, -0.7071067811865464625, 0.000000000000000000 ) ) ;
#74988 = CARTESIAN_POINT ( 'NONE',  ( 30.29974487139158867, -27.71228299555227537, 4.000000000000000000 ) ) ;
#74989 = DIRECTION ( 'NONE',  ( 0.6830127018922181881, 0.6830127018922202975, -0.2588190451025214056 ) ) ;
#74990 = ORIENTED_EDGE ( 'NONE', *, *, #104853, .T. ) ;
#74992 = ADVANCED_FACE ( 'NONE', ( #18318 ), #62592, .F. ) ;
#74991 = ORIENTED_EDGE ( 'NONE', *, *, #54364, .F. ) ;
#74993 = DIRECTION ( 'NONE',  ( -0.7071067811865487940, 0.7071067811865463515, 0.000000000000000000 ) ) ;
#74994 = CARTESIAN_POINT ( 'NONE',  ( -8.999999999999928946, 4.552185695429119328, 5.000000000000000000 ) ) ;
#74995 = VERTEX_POINT ( 'NONE', #51722 ) ;
#74996 = AXIS2_PLACEMENT_3D ( 'NONE', #136132, #12206, #24518 ) ;
#74997 = VERTEX_POINT ( 'NONE', #53106 ) ;
#74998 = DIRECTION ( 'NONE',  ( 0.7071067811865487940, 0.7071067811865463515, -0.000000000000000000 ) ) ;
#74999 = ORIENTED_EDGE ( 'NONE', *, *, #76400, .F. ) ;
#75000 = LINE ( 'NONE', #126647, #109413 ) ;
#75001 = CARTESIAN_POINT ( 'NONE',  ( 0.5732283800867132850, 0.5999999999999989786, 4.263122468548287358 ) ) ;
#75002 = ADVANCED_FACE ( 'NONE', ( #97307 ), #5065, .T. ) ;
#75003 = CARTESIAN_POINT ( 'NONE',  ( 66.29974487139159578, -27.71228299555252406, 4.000000000000000000 ) ) ;
#75004 = FACE_BOUND ( 'NONE', #26881, .T. ) ;
#75005 = DIRECTION ( 'NONE',  ( -0.6830127018922180770, -0.6830127018922204085, -0.2588190451025213501 ) ) ;
#75006 = PLANE ( 'NONE',  #20230 ) ;
#75008 = ORIENTED_EDGE ( 'NONE', *, *, #8270, .T. ) ;
#75007 = CARTESIAN_POINT ( 'NONE',  ( -31.49999999999977973, 8.900465351122127444, -2.516491619111439260 ) ) ;
#75009 = VECTOR ( 'NONE', #116369, 1000.000000000000000 ) ;
#75010 = LINE ( 'NONE', #119184, #76502 ) ;
#75011 = ADVANCED_FACE ( 'NONE', ( #56017 ), #1561, .F. ) ;
#75012 = ORIENTED_EDGE ( 'NONE', *, *, #129800, .F. ) ;
#75013 = VECTOR ( 'NONE', #102904, 999.9999999999998863 ) ;
#75014 = ORIENTED_EDGE ( 'NONE', *, *, #19218, .F. ) ;
#75015 = CARTESIAN_POINT ( 'NONE',  ( 88.72459685856478018, -1.637169565754160949, 6.109999999999997655 ) ) ;
#75016 = EDGE_LOOP ( 'NONE', ( #142061, #105180, #132602, #48029 ) ) ;
#75017 = DIRECTION ( 'NONE',  ( -0.7071067811865486830, -0.7071067811865464625, -0.000000000000000000 ) ) ;
#75018 = EDGE_CURVE ( 'NONE', #80227, #40577, #55284, .T. ) ;
#75019 = ORIENTED_EDGE ( 'NONE', *, *, #135064, .T. ) ;
#75020 = CARTESIAN_POINT ( 'NONE',  ( 30.79289321881324071, 12.75929247661559174, 5.000000000000000000 ) ) ;
#75021 = VECTOR ( 'NONE', #79177, 999.9999999999998863 ) ;
#75022 = DIRECTION ( 'NONE',  ( 0.6830127018922180770, -0.6830127018922204085, -0.2588190451025213501 ) ) ;
#75023 = CARTESIAN_POINT ( 'NONE',  ( -3.489213562373097322, -27.52281430457057709, 5.000000000000000000 ) ) ;
#75024 = DIRECTION ( 'NONE',  ( 0.7071067811865487940, 0.7071067811865463515, 0.000000000000000000 ) ) ;
#75025 = VECTOR ( 'NONE', #77731, 1000.000000000000114 ) ;
#75026 = EDGE_CURVE ( 'NONE', #56677, #129051, #22602, .T. ) ;
#75027 = LINE ( 'NONE', #96022, #36662 ) ;
#75028 = LINE ( 'NONE', #22029, #70535 ) ;
#75029 = DIRECTION ( 'NONE',  ( 0.9659258262890703106, 0.000000000000000000, -0.2588190451025131900 ) ) ;
#75030 = DIRECTION ( 'NONE',  ( -0.6830127018922181881, 0.6830127018922202975, -0.2588190451025214056 ) ) ;
#75031 = VERTEX_POINT ( 'NONE', #12465 ) ;
#75032 = DIRECTION ( 'NONE',  ( -1.000000000000000000, -1.224606353822377258E-16, -0.000000000000000000 ) ) ;
#75033 = EDGE_LOOP ( 'NONE', ( #109597, #15996, #124707 ) ) ;
#75034 = LINE ( 'NONE', #73583, #91254 ) ;
#75035 =( BOUNDED_CURVE ( )  B_SPLINE_CURVE ( 3, ( #114299, #61402, #49071, #72283 ),
 .UNSPECIFIED., .F., .T. ) 
 B_SPLINE_CURVE_WITH_KNOTS ( ( 4, 4 ),
 ( 5.043186909253412509, 5.074607125596327428 ),
 .UNSPECIFIED. ) 
 CURVE ( )  GEOMETRIC_REPRESENTATION_ITEM ( )  RATIONAL_B_SPLINE_CURVE ( ( 1.000000000000000000, 0.9999177325257868620, 0.9999177325257868620, 1.000000000000000000 ) ) 
 REPRESENTATION_ITEM ( '' )  );
#75036 = DIRECTION ( 'NONE',  ( 0.6830127018922180770, -0.6830127018922204085, -0.2588190451025213501 ) ) ;
#75037 = AXIS2_PLACEMENT_3D ( 'NONE', #130712, #62586, #87890 ) ;
#75038 = ORIENTED_EDGE ( 'NONE', *, *, #83284, .F. ) ;
#75039 = ORIENTED_EDGE ( 'NONE', *, *, #73155, .F. ) ;
#75040 = VECTOR ( 'NONE', #55985, 1000.000000000000000 ) ;
#75041 = EDGE_CURVE ( 'NONE', #86087, #82492, #77752, .T. ) ;
#75042 = ORIENTED_EDGE ( 'NONE', *, *, #58617, .F. ) ;
#75043 = CARTESIAN_POINT ( 'NONE',  ( 33.39626352523143993, 4.472830434245840259, -4.472830434245838482 ) ) ;
#75044 = EDGE_LOOP ( 'NONE', ( #104079, #30684, #49537, #101754 ) ) ;
#75045 = CARTESIAN_POINT ( 'NONE',  ( 3.500000000000000444, 0.000000000000000000, 6.094999999999989981 ) ) ;
#75046 = VECTOR ( 'NONE', #67355, 1000.000000000000000 ) ;
#75047 = AXIS2_PLACEMENT_3D ( 'NONE', #15435, #59724, #103884 ) ;
#75048 = CARTESIAN_POINT ( 'NONE',  ( 28.04580628287044064, 5.278424836066143655, -3.047499999999997655 ) ) ;
#75049 = CARTESIAN_POINT ( 'NONE',  ( 2.682347683340221334, 13.58957659137172591, -24.48930257366534846 ) ) ;
#75050 = ORIENTED_EDGE ( 'NONE', *, *, #66766, .T. ) ;
#75051 = LINE ( 'NONE', #106918, #142916 ) ;
#75052 = VERTEX_POINT ( 'NONE', #65465 ) ;
#75053 = CARTESIAN_POINT ( 'NONE',  ( 18.78162688292482230, 21.74787736706806740, 4.999607392498048419 ) ) ;
#75054 = VECTOR ( 'NONE', #135161, 1000.000000000000000 ) ;
#75055 = CARTESIAN_POINT ( 'NONE',  ( 12.19999999999999574, -40.43000000000000682, -39.50000000000000000 ) ) ;
#75057 = ORIENTED_EDGE ( 'NONE', *, *, #138826, .T. ) ;
#75056 = LINE ( 'NONE', #52549, #37875 ) ;
#75058 = ORIENTED_EDGE ( 'NONE', *, *, #81486, .F. ) ;
#75059 = DIRECTION ( 'NONE',  ( 0.7071067811865487940, -0.7071067811865463515, 0.000000000000000000 ) ) ;
#75060 = DIRECTION ( 'NONE',  ( -0.000000000000000000, -0.000000000000000000, 1.000000000000000000 ) ) ;
#75061 = EDGE_LOOP ( 'NONE', ( #22251, #116901, #68606, #82738 ) ) ;
#75062 = VECTOR ( 'NONE', #8621, 1000.000000000000000 ) ;
#75063 = CARTESIAN_POINT ( 'NONE',  ( 108.5791937171295700, 3.975000000000002753, -6.884901960086283523 ) ) ;
#75064 = VERTEX_POINT ( 'NONE', #67608 ) ;
#75066 = VERTEX_POINT ( 'NONE', #132862 ) ;
#75065 = EDGE_CURVE ( 'NONE', #43661, #40590, #32878, .T. ) ;
#75067 = ORIENTED_EDGE ( 'NONE', *, *, #133808, .F. ) ;
#75068 = DIRECTION ( 'NONE',  ( -0.7071067811865486830, -0.7071067811865464625, 0.000000000000000000 ) ) ;
#75069 = VECTOR ( 'NONE', #29913, 1000.000000000000000 ) ;
#75070 = CARTESIAN_POINT ( 'NONE',  ( 28.00000000000002487, -57.14999999999999147, -34.92499999999976978 ) ) ;
#75071 = CARTESIAN_POINT ( 'NONE',  ( 18.79653912142945060, 3.821174125832445049E-16, 0.000000000000000000 ) ) ;
#75072 = LINE ( 'NONE', #93395, #125592 ) ;
#75074 = ADVANCED_FACE ( 'NONE', ( #132139 ), #54577, .F. ) ;
#75073 = CARTESIAN_POINT ( 'NONE',  ( -5.700255128608413102, -27.71228299555201957, 4.000000000000000000 ) ) ;
#75075 = CARTESIAN_POINT ( 'NONE',  ( -56.99451991528749062, 28.92564299267978001, 4.000000000000000000 ) ) ;
#75076 = ORIENTED_EDGE ( 'NONE', *, *, #20378, .T. ) ;
#75077 = EDGE_CURVE ( 'NONE', #123227, #76657, #123414, .T. ) ;
#75078 = CARTESIAN_POINT ( 'NONE',  ( 66.18398860626901126, 28.73617430169833753, 5.000000000000000000 ) ) ;
#75079 = ORIENTED_EDGE ( 'NONE', *, *, #6295, .F. ) ;
#75080 = CARTESIAN_POINT ( 'NONE',  ( -25.49999999999982236, 19.39370406404964697, 1.459788787078258876 ) ) ;
#75081 = CARTESIAN_POINT ( 'NONE',  ( -12.70710678118645021, 2.259292476615694323, 5.000000000000000000 ) ) ;
#75083 = VERTEX_POINT ( 'NONE', #100212 ) ;
#75082 = VECTOR ( 'NONE', #139426, 1000.000000000000227 ) ;
#75084 = DIRECTION ( 'NONE',  ( 0.6830127018922180770, -0.6830127018922204085, -0.2588190451025213501 ) ) ;
#75085 = CARTESIAN_POINT ( 'NONE',  ( 22.17183060077631751, -8.240707523384200428, 4.000000000000000000 ) ) ;
#75086 = VERTEX_POINT ( 'NONE', #32829 ) ;
#75087 = ORIENTED_EDGE ( 'NONE', *, *, #137418, .T. ) ;
#75088 = CARTESIAN_POINT ( 'NONE',  ( 39.18398860626899705, 28.73617430169814568, 5.000000000000000000 ) ) ;
#75089 = CARTESIAN_POINT ( 'NONE',  ( -34.92500000000001137, -22.22500000000000142, 4.000000000000000000 ) ) ;
#75090 = UNCERTAINTY_MEASURE_WITH_UNIT (LENGTH_MEASURE( 1.000000000000000082E-05 ), #64441, 'distance_accuracy_value', 'NONE');
#75091 = CARTESIAN_POINT ( 'NONE',  ( -25.39999999999996305, 0.000000000000000000, 0.000000000000000000 ) ) ;
#75092 = CARTESIAN_POINT ( 'NONE',  ( -34.92500000000001137, 7.067865804795134821, 10.74360474999298454 ) ) ;
#75093 = CARTESIAN_POINT ( 'NONE',  ( 0.6686314397420025646, -52.14999999947626463, -41.03936837847411567 ) ) ;
#75094 = CARTESIAN_POINT ( 'NONE',  ( 64.07876352523145158, -7.482591942790327058E-16, 6.109999999999999432 ) ) ;
#75095 = EDGE_CURVE ( 'NONE', #93458, #82873, #15125, .T. ) ;
#75096 = VECTOR ( 'NONE', #51652, 999.9999999999998863 ) ;
#75097 = CARTESIAN_POINT ( 'NONE',  ( 27.18398860626900060, 28.73617430169806042, 5.000000000000000000 ) ) ;
#75098 = CARTESIAN_POINT ( 'NONE',  ( -6.183988606268994381, 28.73617430169791476, 5.000000000000000000 ) ) ;
#75099 = LINE ( 'NONE', #40329, #18874 ) ;
#75100 = ORIENTED_EDGE ( 'NONE', *, *, #120601, .T. ) ;
#75101 = DIRECTION ( 'NONE',  ( -0.000000000000000000, 0.000000000000000000, 1.000000000000000000 ) ) ;
#75102 = VERTEX_POINT ( 'NONE', #45849 ) ;
#75103 = LINE ( 'NONE', #131600, #128766 ) ;
#75104 = CARTESIAN_POINT ( 'NONE',  ( -36.18398860626899705, 28.73617430169812437, 5.000000000000000000 ) ) ;
#75105 = VERTEX_POINT ( 'NONE', #66870 ) ;
#75106 = CARTESIAN_POINT ( 'NONE',  ( 48.29974487139158867, -27.71228299555239971, 4.000000000000000000 ) ) ;
#75108 = ORIENTED_EDGE ( 'NONE', *, *, #19912, .T. ) ;
#75107 = DIRECTION ( 'NONE',  ( 0.3543493200069163240, -0.000000000000000000, -0.9351131265310288487 ) ) ;
#75109 = PLANE ( 'NONE',  #85575 ) ;
#75110 = CARTESIAN_POINT ( 'NONE',  ( 30.18398860626900060, 28.73617430169808173, 5.000000000000000000 ) ) ;
#75111 = CARTESIAN_POINT ( 'NONE',  ( -33.48921356237309510, -27.52281430457078670, 5.000000000000000000 ) ) ;
#75112 = ORIENTED_EDGE ( 'NONE', *, *, #22055, .T. ) ;
#75113 = ORIENTED_EDGE ( 'NONE', *, *, #142595, .T. ) ;
#75114 = PRESENTATION_STYLE_ASSIGNMENT (( #139663 ) ) ;
#75115 = LINE ( 'NONE', #101829, #32891 ) ;
#75116 = VECTOR ( 'NONE', #101560, 999.9999999999998863 ) ;
#75117 = CARTESIAN_POINT ( 'NONE',  ( 81.29974487139159578, -27.71228299555262709, 4.000000000000000000 ) ) ;
#75118 = CARTESIAN_POINT ( 'NONE',  ( 89.03752705046288440, -9.735942053221456900E-16, 7.949999999999998401 ) ) ;
#75119 = FACE_OUTER_BOUND ( 'NONE', #106260, .T. ) ;
#75120 = VECTOR ( 'NONE', #42308, 1000.000000000000000 ) ;
#75121 = EDGE_CURVE ( 'NONE', #65792, #6819, #88630, .T. ) ;
#75122 = LINE ( 'NONE', #96110, #71505 ) ;
#75123 = VERTEX_POINT ( 'NONE', #11014 ) ;
#75124 = CARTESIAN_POINT ( 'NONE',  ( -29.99451991528749417, 28.92564299267958816, 4.000000000000000000 ) ) ;
#75125 = ADVANCED_FACE ( 'NONE', ( #860 ), #88534, .T. ) ;
#75126 = CIRCLE ( 'NONE', #70777, 2.055000000000000604 ) ;
#75127 = DIRECTION ( 'NONE',  ( -0.000000000000000000, 1.000000000000000000, -0.000000000000000000 ) ) ;
#75128 = CARTESIAN_POINT ( 'NONE',  ( 29.75000000000000355, -7.464222240803106570E-16, -6.094999999999989981 ) ) ;
#75129 = ORIENTED_EDGE ( 'NONE', *, *, #56575, .F. ) ;
#75130 = EDGE_CURVE ( 'NONE', #34999, #106208, #43681, .T. ) ;
#75131 = EDGE_CURVE ( 'NONE', #132715, #89674, #134268, .T. ) ;
#75132 = DIRECTION ( 'NONE',  ( -0.000000000000000000, 0.000000000000000000, 1.000000000000000000 ) ) ;
#75133 = ORIENTED_EDGE ( 'NONE', *, *, #111799, .F. ) ;
#75134 = AXIS2_PLACEMENT_3D ( 'NONE', #5659, #36192, #48474 ) ;
#75135 = AXIS2_PLACEMENT_3D ( 'NONE', #34289, #58238, #136442 ) ;
#75136 = CARTESIAN_POINT ( 'NONE',  ( 77.29209685856477563, -5.291415217122921177, 3.054999999999999272 ) ) ;
#75137 = PLANE ( 'NONE',  #13045 ) ;
#75138 = LINE ( 'NONE', #96813, #84107 ) ;
#75139 = VERTEX_POINT ( 'NONE', #32092 ) ;
#75140 = FACE_OUTER_BOUND ( 'NONE', #23468, .T. ) ;
#75141 = DIRECTION ( 'NONE',  ( -0.7071067811865487940, 0.7071067811865463515, -0.000000000000000000 ) ) ;
#75142 = ADVANCED_FACE ( 'NONE', ( #79209 ), #24075, .F. ) ;
#75143 = CIRCLE ( 'NONE', #19528, 2.500000000000000888 ) ;
#75144 = CARTESIAN_POINT ( 'NONE',  ( 81.18398860626899705, 28.73617430169844056, 5.000000000000000000 ) ) ;
#75145 = EDGE_CURVE ( 'NONE', #59489, #12358, #103566, .T. ) ;
#75146 = DIRECTION ( 'NONE',  ( -0.6830127018922181881, 0.6830127018922202975, -0.2588190451025214056 ) ) ;
#75148 = VERTEX_POINT ( 'NONE', #109646 ) ;
#75147 = PLANE ( 'NONE',  #135439 ) ;
#75149 = FACE_OUTER_BOUND ( 'NONE', #81195, .T. ) ;
#75150 = LINE ( 'NONE', #40377, #140212 ) ;
#75151 = CARTESIAN_POINT ( 'NONE',  ( 32.99451991528749062, 28.92564299267960948, 4.000000000000000000 ) ) ;
#75152 = DIRECTION ( 'NONE',  ( 0.3543493200069162685, -0.000000000000000000, -0.9351131265310288487 ) ) ;
#75153 = AXIS2_PLACEMENT_3D ( 'NONE', #25088, #91783, #25819 ) ;
#75154 = EDGE_LOOP ( 'NONE', ( #2227, #115234, #31643, #72433 ) ) ;
#75155 = EDGE_CURVE ( 'NONE', #79224, #56507, #10320, .T. ) ;
#75156 = EDGE_LOOP ( 'NONE', ( #131509, #82728, #112129, #59404 ) ) ;
#75157 = CARTESIAN_POINT ( 'NONE',  ( 64.75043019189810423, 3.055000000000002824, -5.291415217122919401 ) ) ;
#75158 = VECTOR ( 'NONE', #135438, 1000.000000000000000 ) ;
#75159 = VECTOR ( 'NONE', #26020, 1000.000000000000000 ) ;
#75160 = ORIENTED_EDGE ( 'NONE', *, *, #15049, .F. ) ;
#75161 = CARTESIAN_POINT ( 'NONE',  ( 17.70025512860841488, -27.71228299555193786, 4.000000000000000000 ) ) ;
#75162 = DIRECTION ( 'NONE',  ( 0.7071067811865487940, -0.7071067811865463515, 0.000000000000000000 ) ) ;
#75163 = LINE ( 'NONE', #51250, #80516 ) ;
#75164 = DIRECTION ( 'NONE',  ( -0.7071067811865487940, 0.7071067811865463515, 0.000000000000000000 ) ) ;
#75165 = ORIENTED_EDGE ( 'NONE', *, *, #76462, .F. ) ;
#75166 = EDGE_CURVE ( 'NONE', #31876, #138628, #127481, .T. ) ;
#75167 = CARTESIAN_POINT ( 'NONE',  ( -3.812461875839445291, -22.22500000000000142, 4.000000000000000000 ) ) ;
#75168 = DIRECTION ( 'NONE',  ( -1.000000000000000000, -1.224606353822377258E-16, -0.000000000000000000 ) ) ;
#75169 = AXIS2_PLACEMENT_3D ( 'NONE', #5429, #72910, #95313 ) ;
#75170 = ORIENTED_EDGE ( 'NONE', *, *, #87824, .F. ) ;
#75171 = PLANE ( 'NONE',  #368 ) ;
#75172 = FACE_OUTER_BOUND ( 'NONE', #95712, .T. ) ;
#75173 = EDGE_CURVE ( 'NONE', #125882, #2713, #95560, .T. ) ;
#75174 = DIRECTION ( 'NONE',  ( -0.6830127018922180770, -0.6830127018922204085, -0.2588190451025213501 ) ) ;
#75175 = VERTEX_POINT ( 'NONE', #84695 ) ;
#75176 = ORIENTED_EDGE ( 'NONE', *, *, #52482, .F. ) ;
#75177 = DIRECTION ( 'NONE',  ( -0.7071067811865486830, -0.7071067811865464625, 0.000000000000000000 ) ) ;
#75178 = CARTESIAN_POINT ( 'NONE',  ( 181.0474453055293793, -48.63825160239814238, 38.47250499286696623 ) ) ;
#75179 = EDGE_CURVE ( 'NONE', #79735, #71611, #7086, .T. ) ;
#75180 = PLANE ( 'NONE',  #51283 ) ;
#75181 = LINE ( 'NONE', #132428, #48285 ) ;
#75182 = EDGE_CURVE ( 'NONE', #126053, #132490, #50636, .T. ) ;
#75183 = DIRECTION ( 'NONE',  ( 0.000000000000000000, 0.000000000000000000, -1.000000000000000000 ) ) ;
#75184 = CARTESIAN_POINT ( 'NONE',  ( -26.99999999999981881, -19.06887692260762179, 4.000000000000000000 ) ) ;
#75185 = EDGE_CURVE ( 'NONE', #65687, #21154, #58461, .T. ) ;
#75186 = ORIENTED_EDGE ( 'NONE', *, *, #111520, .T. ) ;
#75187 = EDGE_LOOP ( 'NONE', ( #130135, #136125, #31394, #12816 ) ) ;
#75188 = CARTESIAN_POINT ( 'NONE',  ( 111.4745968585647802, 1.637169565754164280, -6.109999999999996767 ) ) ;
#75189 = ORIENTED_EDGE ( 'NONE', *, *, #77304, .F. ) ;
#75190 = ORIENTED_EDGE ( 'NONE', *, *, #62000, .F. ) ;
#75191 = CARTESIAN_POINT ( 'NONE',  ( -15.70701326429294475, -21.74070752338406365, 4.999753212805219782 ) ) ;
#75192 = AXIS2_PLACEMENT_3D ( 'NONE', #84807, #117404, #128330 ) ;
#75193 = DIRECTION ( 'NONE',  ( -0.6830127018922180770, -0.6830127018922204085, -0.2588190451025213501 ) ) ;
#75194 = CARTESIAN_POINT ( 'NONE',  ( 2.207106781186532363, 0.7592924766157069794, 5.000000000000000000 ) ) ;
#75195 = ORIENTED_EDGE ( 'NONE', *, *, #72476, .F. ) ;
#75196 = DIRECTION ( 'NONE',  ( 1.734723475976806848E-16, -1.000000000000000000, 0.000000000000000000 ) ) ;
#75197 = PLANE ( 'NONE',  #77277 ) ;
#75198 = DIRECTION ( 'NONE',  ( 0.7071067811865487940, 0.7071067811865463515, 0.000000000000000000 ) ) ;
#75199 = CARTESIAN_POINT ( 'NONE',  ( -13.82816939922342669, 21.75929247661550647, 4.000000000000000000 ) ) ;
#75200 = LINE ( 'NONE', #130287, #113908 ) ;
#75201 = ORIENTED_EDGE ( 'NONE', *, *, #18214, .T. ) ;
#75202 = DIRECTION ( 'NONE',  ( -0.000000000000000000, 0.3543493200069153248, 0.9351131265310292928 ) ) ;
#75203 = CARTESIAN_POINT ( 'NONE',  ( 13.17183060077637613, -14.24070752338414181, 4.000000000000000000 ) ) ;
#75204 = ORIENTED_EDGE ( 'NONE', *, *, #141170, .F. ) ;
#75205 = DIRECTION ( 'NONE',  ( -1.000000000000000000, -1.224606353822377258E-16, -0.000000000000000000 ) ) ;
#75206 = ORIENTED_EDGE ( 'NONE', *, *, #60003, .F. ) ;
#75207 = ORIENTED_EDGE ( 'NONE', *, *, #7603, .T. ) ;
#75208 = ORIENTED_EDGE ( 'NONE', *, *, #107117, .T. ) ;
#75209 = CARTESIAN_POINT ( 'NONE',  ( 61.39626352523142572, 4.472830434245840259, -4.472830434245838482 ) ) ;
#75210 = EDGE_LOOP ( 'NONE', ( #22874, #45392, #76014, #44979 ) ) ;
#75211 = ORIENTED_EDGE ( 'NONE', *, *, #105266, .F. ) ;
#75212 = LINE ( 'NONE', #55592, #120736 ) ;
#75213 = COLOUR_RGB ( '', 0.66274510, 0.83137255, 0.94901961) ;
#75214 = FILL_AREA_STYLE_COLOUR ( '', #21826 ) ;
#75215 = CARTESIAN_POINT ( 'NONE',  ( 97.12543019189810423, 5.291415217122919401, 3.055000000000002824 ) ) ;
#75216 = CARTESIAN_POINT ( 'NONE',  ( -18.75860074219783868, 21.72500000000000853, 5.000000000000000000 ) ) ;
#75217 = AXIS2_PLACEMENT_3D ( 'NONE', #100241, #10350, #1595 ) ;
#75218 = EDGE_CURVE ( 'NONE', #128354, #19651, #72438, .T. ) ;
#75219 = LINE ( 'NONE', #20796, #115992 ) ;
#75220 = ORIENTED_EDGE ( 'NONE', *, *, #99995, .T. ) ;
#75221 = DIRECTION ( 'NONE',  ( 0.3543493200069162685, -0.000000000000000000, -0.9351131265310288487 ) ) ;
#75222 = DIRECTION ( 'NONE',  ( -0.7071067811865486830, -0.7071067811865464625, 0.000000000000000000 ) ) ;
#75223 = CARTESIAN_POINT ( 'NONE',  ( 19.58200623001875940, 3.821174125832445049E-16, 0.000000000000000000 ) ) ;
#75224 = LINE ( 'NONE', #41134, #119188 ) ;
#75225 = ORIENTED_EDGE ( 'NONE', *, *, #61456, .F. ) ;
#75226 = DIRECTION ( 'NONE',  ( -0.000000000000000000, 0.000000000000000000, 1.000000000000000000 ) ) ;
#75227 = ORIENTED_EDGE ( 'NONE', *, *, #74135, .T. ) ;
#75228 = ORIENTED_EDGE ( 'NONE', *, *, #141966, .T. ) ;
#75229 = ORIENTED_EDGE ( 'NONE', *, *, #65527, .T. ) ;
#75230 = CARTESIAN_POINT ( 'NONE',  ( 118.1829301918981230, -1.637169565754158951, -6.109999999999998543 ) ) ;
#75231 = VERTEX_POINT ( 'NONE', #117991 ) ;
#75232 = PLANE ( 'NONE',  #104802 ) ;
#75233 = DIRECTION ( 'NONE',  ( -0.3543493200069162685, -0.000000000000000000, -0.9351131265310288487 ) ) ;
#75234 = EDGE_CURVE ( 'NONE', #27746, #107457, #128898, .T. ) ;
#75235 = CARTESIAN_POINT ( 'NONE',  ( 34.75611968250419181, 13.70565069852390927, 4.955485411084884717 ) ) ;
#75236 = ORIENTED_EDGE ( 'NONE', *, *, #52520, .F. ) ;
#75237 = EDGE_CURVE ( 'NONE', #72919, #83224, #136931, .T. ) ;
#75238 = CARTESIAN_POINT ( 'NONE',  ( 3.730677800976790248, -49.14999999999999147, 40.92499999999998295 ) ) ;
#75239 = ORIENTED_EDGE ( 'NONE', *, *, #137980, .F. ) ;
#75240 = VECTOR ( 'NONE', #31600, 1000.000000000000000 ) ;
#75241 =( GEOMETRIC_REPRESENTATION_CONTEXT ( 3 ) GLOBAL_UNCERTAINTY_ASSIGNED_CONTEXT ( ( #55109 ) ) GLOBAL_UNIT_ASSIGNED_CONTEXT ( ( #82033, #124780, #92856 ) ) REPRESENTATION_CONTEXT ( 'NONE', 'WORKASPACE' ) );
#75242 = CARTESIAN_POINT ( 'NONE',  ( 33.17123647476855552, 0.000000000000000000, 7.934999999999990727 ) ) ;
#75243 = DIRECTION ( 'NONE',  ( 0.6830127018922180770, -0.6830127018922204085, -0.2588190451025213501 ) ) ;
#75244 = VECTOR ( 'NONE', #89637, 1000.000000000000000 ) ;
#75245 = CARTESIAN_POINT ( 'NONE',  ( 48.18398860626899705, 28.73617430169820608, 5.000000000000000000 ) ) ;
#75247 = EDGE_CURVE ( 'NONE', #81137, #11235, #17286, .T. ) ;
#75246 = VECTOR ( 'NONE', #143432, 1000.000000000000227 ) ;
#75248 = CARTESIAN_POINT ( 'NONE',  ( -72.18398860626899705, 28.73617430169837661, 5.000000000000000000 ) ) ;
#75249 = VERTEX_POINT ( 'NONE', #61550 ) ;
#75250 = ORIENTED_EDGE ( 'NONE', *, *, #61206, .F. ) ;
#75251 = ORIENTED_EDGE ( 'NONE', *, *, #43023, .T. ) ;
#75252 = CARTESIAN_POINT ( 'NONE',  ( 13.17183060077637613, 21.75929247661549937, 4.000000000000000000 ) ) ;
#75253 = CARTESIAN_POINT ( 'NONE',  ( -12.70000000000000462, -22.26999999999999247, -0.5000000000000004441 ) ) ;
#75254 = DIRECTION ( 'NONE',  ( 0.000000000000000000, -1.000000000000000000, 0.000000000000000000 ) ) ;
#75255 = DIRECTION ( 'NONE',  ( -0.7071067811865486830, -0.7071067811865464625, 0.000000000000000000 ) ) ;
#75256 = ADVANCED_FACE ( 'NONE', ( #18694 ), #62970, .T. ) ;
#75257 = FACE_OUTER_BOUND ( 'NONE', #56624, .T. ) ;
#75258 = CARTESIAN_POINT ( 'NONE',  ( 28.72959685856476497, -6.110000000000000320, -1.637169565754161393 ) ) ;
#75259 = CARTESIAN_POINT ( 'NONE',  ( 11.99451991528749417, 28.92564299267946382, 4.000000000000000000 ) ) ;
#75260 = DIRECTION ( 'NONE',  ( -0.000000000000000000, -1.000000000000000000, -0.000000000000000000 ) ) ;
#75261 = ORIENTED_EDGE ( 'NONE', *, *, #39775, .T. ) ;
#75262 = PLANE ( 'NONE',  #55772 ) ;
#75263 = ORIENTED_EDGE ( 'NONE', *, *, #115532, .T. ) ;
#75264 = EDGE_CURVE ( 'NONE', #12119, #122337, #26739, .T. ) ;
#75265 = DIRECTION ( 'NONE',  ( -0.6830127018922180770, -0.6830127018922204085, -0.2588190451025213501 ) ) ;
#75266 = VERTEX_POINT ( 'NONE', #94823 ) ;
#75268 = VERTEX_POINT ( 'NONE', #37642 ) ;
#75267 = DIRECTION ( 'NONE',  ( -1.000000000000000000, -0.000000000000000000, -0.000000000000000000 ) ) ;
#75269 = LINE ( 'NONE', #41177, #39909 ) ;
#75270 = EDGE_LOOP ( 'NONE', ( #23673, #4633, #20201, #36110, #67092, #21072, #136314, #91925, #45042, #79648, #112836, #98581, #120853, #115283, #94641, #69470, #40795, #2913, #69649, #99106, #81352, #56885, #63413, #143467, #74751, #22236, #117072, #62077, #107325, #53427, #77565, #66373, #105307, #63287, #58188, #30754, #61226, #40144, #62875, #40288, #24524, #100857, #127670, #86331 ) ) ;
#75271 = EDGE_LOOP ( 'NONE', ( #113247, #116387, #34988, #7314 ) ) ;
#75272 = DIRECTION ( 'NONE',  ( -0.7071067811865487940, 0.7071067811865463515, -0.000000000000000000 ) ) ;
#75273 = ORIENTED_EDGE ( 'NONE', *, *, #11354, .F. ) ;
#75274 = DIRECTION ( 'NONE',  ( 0.7071067811865487940, 0.7071067811865463515, 0.000000000000000000 ) ) ;
#75275 = CARTESIAN_POINT ( 'NONE',  ( 113.8291937171295558, -3.975000000000001865, 6.884901960086284411 ) ) ;
#75276 = DIRECTION ( 'NONE',  ( 2.110369192185896011E-16, -1.000000000000000000, 0.000000000000000000 ) ) ;
#75277 = CARTESIAN_POINT ( 'NONE',  ( -14.70025512860841133, -27.71228299555195917, 4.000000000000000000 ) ) ;
#75278 = DIRECTION ( 'NONE',  ( 0.7071067811865487940, 0.7071067811865463515, 0.000000000000000000 ) ) ;
#75280 = ADVANCED_FACE ( 'NONE', ( #139087 ), #39792, .F. ) ;
#75279 = LINE ( 'NONE', #45521, #128288 ) ;
#75281 = DIRECTION ( 'NONE',  ( -0.7071067811865486830, 0.7071067811865464625, 0.000000000000000000 ) ) ;
#75282 = CARTESIAN_POINT ( 'NONE',  ( 6.270833333333333925, 6.094999999999991758, 1.633150327867687102 ) ) ;
#75283 = CARTESIAN_POINT ( 'NONE',  ( 21.70790314143522082, -6.871911579029513106, -3.967499999999993587 ) ) ;
#75284 = LINE ( 'NONE', #45525, #16518 ) ;
#75285 = DIRECTION ( 'NONE',  ( -1.000000000000000000, -1.224606353822377258E-16, -0.000000000000000000 ) ) ;
#75286 = ORIENTED_EDGE ( 'NONE', *, *, #81999, .F. ) ;
#75288 = ORIENTED_EDGE ( 'NONE', *, *, #7093, .T. ) ;
#75287 = EDGE_CURVE ( 'NONE', #85316, #29037, #128214, .T. ) ;
#75289 = EDGE_CURVE ( 'NONE', #112409, #626, #60105, .T. ) ;
#75290 = DIRECTION ( 'NONE',  ( 0.000000000000000000, 0.000000000000000000, 1.000000000000000000 ) ) ;
#75291 = EDGE_LOOP ( 'NONE', ( #100663, #107940, #65604, #31769 ) ) ;
#75292 = CARTESIAN_POINT ( 'NONE',  ( -16.49999999999988631, 10.46639925780215918, 5.000000000000000000 ) ) ;
#75293 = CARTESIAN_POINT ( 'NONE',  ( 33.32816939922329880, -15.74070752338412760, 4.000000000000000000 ) ) ;
#75294 = DIRECTION ( 'NONE',  ( 0.000000000000000000, 0.000000000000000000, -1.000000000000000000 ) ) ;
#75295 = VERTEX_POINT ( 'NONE', #28892 ) ;
#75296 = EDGE_CURVE ( 'NONE', #20428, #84993, #15812, .T. ) ;
#75297 = LINE ( 'NONE', #80301, #85890 ) ;
#75298 = DIRECTION ( 'NONE',  ( -0.6830127018922180770, -0.6830127018922204085, -0.2588190451025213501 ) ) ;
#75299 = EDGE_CURVE ( 'NONE', #122251, #138807, #82556, .T. ) ;
#75300 = ADVANCED_FACE ( 'NONE', ( #27432 ), #63089, .T. ) ;
#75301 = DIRECTION ( 'NONE',  ( 0.7071067811865486830, -0.7071067811865464625, -0.000000000000000000 ) ) ;
#75303 = ORIENTED_EDGE ( 'NONE', *, *, #57855, .F. ) ;
#75302 = CARTESIAN_POINT ( 'NONE',  ( 1.353980332882009252, 0.3999999999999995226, 2.467792535850613866 ) ) ;
#75304 = CARTESIAN_POINT ( 'NONE',  ( -10.49999999999993250, 10.94296225409025958, -9.576120664313281239 ) ) ;
#75305 = CARTESIAN_POINT ( 'NONE',  ( 69.83333333333332860, -6.884901960086287964, 3.974999999999998312 ) ) ;
#75306 = CARTESIAN_POINT ( 'NONE',  ( 18.32840764549667512, 9.139736423841732040E-16, 0.000000000000000000 ) ) ;
#75307 = CARTESIAN_POINT ( 'NONE',  ( 57.34909574878652450, -49.32595796886462836, 36.54674188582600181 ) ) ;
#75308 = ORIENTED_EDGE ( 'NONE', *, *, #28880, .T. ) ;
#75309 = AXIS2_PLACEMENT_3D ( 'NONE', #51237, #18552, #85256 ) ;
#75310 = VERTEX_POINT ( 'NONE', #5676 ) ;
#75311 = VERTEX_POINT ( 'NONE', #43339 ) ;
#75312 = CARTESIAN_POINT ( 'NONE',  ( 106.1670968585647756, -3.055000000000000160, -5.291415217122921177 ) ) ;
#75313 = VERTEX_POINT ( 'NONE', #130355 ) ;
#75314 = EDGE_CURVE ( 'NONE', #57383, #55894, #20125, .T. ) ;
#75315 = VECTOR ( 'NONE', #49463, 1000.000000000000000 ) ;
#75316 = DIRECTION ( 'NONE',  ( -0.7071067811865486830, 0.7071067811865464625, 0.000000000000000000 ) ) ;
#75317 = CARTESIAN_POINT ( 'NONE',  ( 21.76000000000000156, 9.521314400968980422E-16, 0.000000000000000000 ) ) ;
#75318 = EDGE_LOOP ( 'NONE', ( #80185, #103190, #141826, #120624 ) ) ;
#75319 = ADVANCED_FACE ( 'NONE', ( #20848 ), #9219, .F. ) ;
#75320 = LINE ( 'NONE', #1968, #56023 ) ;
#75321 = CARTESIAN_POINT ( 'NONE',  ( 2.700255128608413990, -27.71228299555204089, 4.000000000000000000 ) ) ;
#75322 = CARTESIAN_POINT ( 'NONE',  ( 97.03709685856479439, -3.054999999999998828, -5.291415217122919401 ) ) ;
#75323 = VECTOR ( 'NONE', #104467, 999.9999999999998863 ) ;
#75324 = ORIENTED_EDGE ( 'NONE', *, *, #27952, .T. ) ;
#75325 = LINE ( 'NONE', #22314, #141556 ) ;
#75326 = DIRECTION ( 'NONE',  ( -1.000000000000000000, -0.000000000000000000, -0.000000000000000000 ) ) ;
#75327 = DIRECTION ( 'NONE',  ( -1.000000000000000000, -1.224606353822377258E-16, -0.000000000000000000 ) ) ;
#75328 = LINE ( 'NONE', #86193, #62479 ) ;
#75329 = VERTEX_POINT ( 'NONE', #76704 ) ;
#75330 = ORIENTED_EDGE ( 'NONE', *, *, #11583, .T. ) ;
#75331 = ORIENTED_EDGE ( 'NONE', *, *, #67032, .T. ) ;
#75332 = PLANE ( 'NONE',  #23629 ) ;
#75333 = LINE ( 'NONE', #131128, #112549 ) ;
#75334 = CARTESIAN_POINT ( 'NONE',  ( 19.90040314143522338, -7.934999999999988951, 2.126176841940957907 ) ) ;
#75335 = DIRECTION ( 'NONE',  ( 0.000000000000000000, 0.000000000000000000, 1.000000000000000000 ) ) ;
#75336 = AXIS2_PLACEMENT_3D ( 'NONE', #60891, #15170, #59450 ) ;
#75337 = PLANE ( 'NONE',  #30190 ) ;
#75338 = EDGE_CURVE ( 'NONE', #42695, #81804, #31743, .T. ) ;
#75340 = EDGE_CURVE ( 'NONE', #2943, #20392, #121588, .T. ) ;
#75339 = AXIS2_PLACEMENT_3D ( 'NONE', #54015, #19212, #131548 ) ;
#75341 = CONICAL_SURFACE ( 'NONE', #12793, 2.055000000000000604, 0.9599310885968764806 ) ;
#75342 = EDGE_LOOP ( 'NONE', ( #14962, #9586, #122026, #36283 ) ) ;
#75344 = EDGE_LOOP ( 'NONE', ( #53458, #18272, #136180 ) ) ;
#75343 = VECTOR ( 'NONE', #2925, 1000.000000000000114 ) ;
#75345 = CARTESIAN_POINT ( 'NONE',  ( -21.96495920677946856, -2.033836129387410985, 4.000000000000000000 ) ) ;
#75346 = ORIENTED_EDGE ( 'NONE', *, *, #102732, .F. ) ;
#75347 = ORIENTED_EDGE ( 'NONE', *, *, #13932, .F. ) ;
#75348 = CARTESIAN_POINT ( 'NONE',  ( 17.64583333333333215, -1.633150327867690210, 6.094999999999989981 ) ) ;
#75349 = CARTESIAN_POINT ( 'NONE',  ( 61.03752705046289151, -9.735942053221456900E-16, 7.949999999999998401 ) ) ;
#75350 = ORIENTED_EDGE ( 'NONE', *, *, #40258, .F. ) ;
#75351 = CARTESIAN_POINT ( 'NONE',  ( 55.39583333333331439, -2.130196079827351596, 7.950000000000043698 ) ) ;
#75352 = LINE ( 'NONE', #43426, #64098 ) ;
#75353 = LINE ( 'NONE', #29668, #110856 ) ;
#75354 = CARTESIAN_POINT ( 'NONE',  ( -26.99999999999981171, 10.55218569542906160, 5.000000000000000000 ) ) ;
#75355 = VERTEX_POINT ( 'NONE', #132524 ) ;
#75356 = CARTESIAN_POINT ( 'NONE',  ( -42.29974487139158157, -27.71228299555235708, 4.000000000000000000 ) ) ;
#75357 = ORIENTED_EDGE ( 'NONE', *, *, #106648, .F. ) ;
#75358 = CARTESIAN_POINT ( 'NONE',  ( 24.48921356237309510, -27.52281430457072631, 5.000000000000000000 ) ) ;
#75359 = CARTESIAN_POINT ( 'NONE',  ( 20.99451991528748707, 28.92564299267952777, 4.000000000000000000 ) ) ;
#75360 = ORIENTED_EDGE ( 'NONE', *, *, #79535, .T. ) ;
#75361 = LINE ( 'NONE', #20223, #74676 ) ;
#75362 = EDGE_LOOP ( 'NONE', ( #99254, #124471, #51505, #58009 ) ) ;
#75363 = CARTESIAN_POINT ( 'NONE',  ( 1.554198602559970332, 0.4000000000000001887, -2.412907414356850300 ) ) ;
#75364 = VERTEX_POINT ( 'NONE', #87551 ) ;
#75365 = ORIENTED_EDGE ( 'NONE', *, *, #28993, .F. ) ;
#75366 = EDGE_LOOP ( 'NONE', ( #63516, #51573, #47465, #87933 ) ) ;
#75367 = CARTESIAN_POINT ( 'NONE',  ( 27.76626352523143737, 4.472830434245838482, -4.472830434245837594 ) ) ;
#75368 = CARTESIAN_POINT ( 'NONE',  ( -34.42500000000001137, -22.22500000000000142, 5.000000000000000000 ) ) ;
#75369 = CARTESIAN_POINT ( 'NONE',  ( -1.567156510475481435, -22.22500000000000142, -7.640533879852384302 ) ) ;
#75370 = DIRECTION ( 'NONE',  ( 0.000000000000000000, -1.000000000000000000, 0.000000000000000000 ) ) ;
#75371 = EDGE_CURVE ( 'NONE', #89781, #13143, #53499, .T. ) ;
#75372 = PLANE ( 'NONE',  #122306 ) ;
#75373 = PLANE ( 'NONE',  #25031 ) ;
#75374 = FACE_OUTER_BOUND ( 'NONE', #28890, .T. ) ;
#75375 = DIRECTION ( 'NONE',  ( -0.7071067811865486830, -0.7071067811865464625, 0.000000000000000000 ) ) ;
#75376 = FACE_OUTER_BOUND ( 'NONE', #55365, .T. ) ;
#75377 = CARTESIAN_POINT ( 'NONE',  ( 36.48921356237310221, -27.52281430457080802, 5.000000000000000000 ) ) ;
#75378 = ORIENTED_EDGE ( 'NONE', *, *, #68796, .F. ) ;
#75379 = ORIENTED_EDGE ( 'NONE', *, *, #129106, .T. ) ;
#75380 = ORIENTED_EDGE ( 'NONE', *, *, #22020, .T. ) ;
#75381 = VERTEX_POINT ( 'NONE', #64371 ) ;
#75382 = DIRECTION ( 'NONE',  ( -0.6830127018922180770, -0.6830127018922204085, -0.2588190451025213501 ) ) ;
#75383 = ORIENTED_EDGE ( 'NONE', *, *, #17298, .F. ) ;
#75385 = ORIENTED_EDGE ( 'NONE', *, *, #8095, .T. ) ;
#75384 = EDGE_CURVE ( 'NONE', #38574, #87786, #141958, .T. ) ;
#75386 = PLANE ( 'NONE',  #65314 ) ;
#75387 = EDGE_CURVE ( 'NONE', #91904, #117764, #22257, .T. ) ;
#75388 = EDGE_CURVE ( 'NONE', #116419, #59816, #10666, .T. ) ;
#75389 = CARTESIAN_POINT ( 'NONE',  ( 14.99451991528749595, 28.92564299267948513, 4.000000000000000000 ) ) ;
#75390 = EDGE_LOOP ( 'NONE', ( #111863, #54985, #23474, #33795 ) ) ;
#75391 = CARTESIAN_POINT ( 'NONE',  ( 23.99999999999983302, -0.1606350220012988939, 4.664761815935144718 ) ) ;
#75392 = EDGE_LOOP ( 'NONE', ( #70296, #47682, #104077, #128493 ) ) ;
#75394 = EDGE_CURVE ( 'NONE', #116862, #111356, #109296, .T. ) ;
#75393 = DIRECTION ( 'NONE',  ( -0.3543493200069162685, -0.000000000000000000, -0.9351131265310288487 ) ) ;
#75395 = EDGE_CURVE ( 'NONE', #126332, #126491, #16806, .T. ) ;
#75396 = CONICAL_SURFACE ( 'NONE', #12863, 2.500000000000000444, 0.9599310885968830309 ) ;
#75397 = LINE ( 'NONE', #51511, #95910 ) ;
#75398 = CARTESIAN_POINT ( 'NONE',  ( 7.942069808101886785, 7.934999999999993392, 2.126176841940951689 ) ) ;
#75399 = ORIENTED_EDGE ( 'NONE', *, *, #17957, .T. ) ;
#75400 = CARTESIAN_POINT ( 'NONE',  ( 95.72459685856476597, -1.637169565754161171, 6.109999999999998543 ) ) ;
#75401 = CARTESIAN_POINT ( 'NONE',  ( 7.431334631360206444, -8.913301243404507801, -3.293706071196084384 ) ) ;
#75402 = PRESENTATION_LAYER_ASSIGNMENT (  '', '', ( #24283 ) ) ;
#75403 = EDGE_CURVE ( 'NONE', #27017, #89318, #75269, .T. ) ;
#75404 = CARTESIAN_POINT ( 'NONE',  ( -32.29289321881323360, -6.740707523384211086, 5.000000000000000000 ) ) ;
#75405 = CARTESIAN_POINT ( 'NONE',  ( -0.1839886062690032631, 28.73617430169787568, 5.000000000000000000 ) ) ;
#75406 = ORIENTED_EDGE ( 'NONE', *, *, #133863, .F. ) ;
#75407 = VERTEX_POINT ( 'NONE', #107841 ) ;
#75408 = CARTESIAN_POINT ( 'NONE',  ( 7.408407645496676963, 9.139736423841732040E-16, 0.000000000000000000 ) ) ;
#75409 = EDGE_LOOP ( 'NONE', ( #140651, #28971, #13797, #1843, #51049, #74328 ) ) ;
#75410 = FACE_OUTER_BOUND ( 'NONE', #13225, .T. ) ;
#75411 = CARTESIAN_POINT ( 'NONE',  ( 18.48921356237309510, -27.52281430457068367, 5.000000000000000000 ) ) ;
#75412 = FACE_OUTER_BOUND ( 'NONE', #79872, .T. ) ;
#75413 = CARTESIAN_POINT ( 'NONE',  ( -10.43312800248735606, -21.74070752338405654, 6.915939825044099543 ) ) ;
#75415 = ORIENTED_EDGE ( 'NONE', *, *, #27284, .F. ) ;
#75414 =( BOUNDED_CURVE ( )  B_SPLINE_CURVE ( 3, ( #139241, #138507, #28327, #50782 ),
 .UNSPECIFIED., .F., .F. ) 
 B_SPLINE_CURVE_WITH_KNOTS ( ( 4, 4 ),
 ( 5.920967161967927161, 7.341195215986580536 ),
 .UNSPECIFIED. ) 
 CURVE ( )  GEOMETRIC_REPRESENTATION_ITEM ( )  RATIONAL_B_SPLINE_CURVE ( ( 1.000000000000000000, 0.8388583629366737071, 0.8388583629366737071, 1.000000000000000000 ) ) 
 REPRESENTATION_ITEM ( '' )  );
#75416 = CARTESIAN_POINT ( 'NONE',  ( 0.000000000000000000, 0.000000000000000000, 5.000000000000000000 ) ) ;
#75417 = ADVANCED_FACE ( 'NONE', ( #143349 ), #96948, .F. ) ;
#75418 = VECTOR ( 'NONE', #62091, 1000.000000000000227 ) ;
#75419 = DIRECTION ( 'NONE',  ( -1.000000000000000000, -0.000000000000000000, -0.000000000000000000 ) ) ;
#75420 = ORIENTED_EDGE ( 'NONE', *, *, #89947, .T. ) ;
#75421 = LINE ( 'NONE', #94992, #28069 ) ;
#75422 = EDGE_CURVE ( 'NONE', #23928, #49613, #140487, .T. ) ;
#75423 = LINE ( 'NONE', #76875, #12342 ) ;
#75424 = VERTEX_POINT ( 'NONE', #131776 ) ;
#75426 = ORIENTED_EDGE ( 'NONE', *, *, #23885, .T. ) ;
#75425 = CARTESIAN_POINT ( 'NONE',  ( -0.4892135623730947680, -27.52281430457055578, 5.000000000000000000 ) ) ;
#75427 = ORIENTED_EDGE ( 'NONE', *, *, #29156, .F. ) ;
#75428 = LINE ( 'NONE', #7272, #35427 ) ;
#75429 = CARTESIAN_POINT ( 'NONE',  ( 78.48921356237309510, -27.52281430457109934, 5.000000000000000000 ) ) ;
#75430 = ADVANCED_FACE ( 'NONE', ( #65108 ), #85387, .F. ) ;
#75431 = VERTEX_POINT ( 'NONE', #41917 ) ;
#75432 = DIRECTION ( 'NONE',  ( 0.7071067811865487940, -0.7071067811865463515, 0.000000000000000000 ) ) ;
#75433 = CIRCLE ( 'NONE', #31454, 2.055000000000001048 ) ;
#75434 = CARTESIAN_POINT ( 'NONE',  ( 23.99451991528749062, 28.92564299267954908, 4.000000000000000000 ) ) ;
#75435 = VECTOR ( 'NONE', #135752, 1000.000000000000000 ) ;
#75436 = VECTOR ( 'NONE', #116016, 1000.000000000000227 ) ;
#75437 = CARTESIAN_POINT ( 'NONE',  ( 0.000000000000000000, 0.000000000000000000, 5.000000000000000000 ) ) ;
#75438 = CARTESIAN_POINT ( 'NONE',  ( 32.06249999999999289, -5.819803920172573086, -5.819803920172573974 ) ) ;
#75439 = PLANE ( 'NONE',  #46740 ) ;
#75441 = EDGE_CURVE ( 'NONE', #143132, #133910, #32466, .T. ) ;
#75440 = CARTESIAN_POINT ( 'NONE',  ( -34.26506670282030598, 12.75929247661558996, 18.34774599283964136 ) ) ;
#75442 = PLANE ( 'NONE',  #13639 ) ;
#75443 = CARTESIAN_POINT ( 'NONE',  ( -69.29974487139159578, -27.71228299555254537, 4.000000000000000000 ) ) ;
#75444 = DIRECTION ( 'NONE',  ( 0.6830127018922181881, 0.6830127018922202975, -0.2588190451025214056 ) ) ;
#75445 = LINE ( 'NONE', #8008, #117719 ) ;
#75446 = AXIS2_PLACEMENT_3D ( 'NONE', #129602, #119424, #132518 ) ;
#75447 = CARTESIAN_POINT ( 'NONE',  ( 29.99999999999979039, 7.588810512006244124, -3.013526669885294496 ) ) ;
#75448 = CARTESIAN_POINT ( 'NONE',  ( -11.51078643762690490, -27.52281430457047406, 5.000000000000000000 ) ) ;
#75449 = ORIENTED_EDGE ( 'NONE', *, *, #25073, .F. ) ;
#75450 = ORIENTED_EDGE ( 'NONE', *, *, #33830, .T. ) ;
#75451 = ORIENTED_EDGE ( 'NONE', *, *, #83173, .F. ) ;
#75452 = EDGE_CURVE ( 'NONE', #120532, #34652, #86126, .T. ) ;
#75453 = CARTESIAN_POINT ( 'NONE',  ( 112.7083333333333286, -3.974999999999999201, -6.884901960086287964 ) ) ;
#75454 = ORIENTED_EDGE ( 'NONE', *, *, #107044, .F. ) ;
#75455 = ORIENTED_EDGE ( 'NONE', *, *, #65994, .F. ) ;
#75456 = EDGE_CURVE ( 'NONE', #78816, #2171, #120134, .T. ) ;
#75457 = ORIENTED_EDGE ( 'NONE', *, *, #8443, .F. ) ;
#75458 = FACE_OUTER_BOUND ( 'NONE', #12185, .T. ) ;
#75459 = DIRECTION ( 'NONE',  ( -0.7071067811865486830, 0.7071067811865464625, 0.000000000000000000 ) ) ;
#75460 = ORIENTED_EDGE ( 'NONE', *, *, #58757, .F. ) ;
#75461 = DIRECTION ( 'NONE',  ( -1.000000000000000000, -1.224606353822377258E-16, -0.000000000000000000 ) ) ;
#75462 = EDGE_CURVE ( 'NONE', #46985, #117324, #89684, .T. ) ;
#75463 = DIRECTION ( 'NONE',  ( -0.3543493200069162685, -0.000000000000000000, -0.9351131265310288487 ) ) ;
#75464 = DIRECTION ( 'NONE',  ( -0.7071067811865486830, -0.7071067811865464625, 0.000000000000000000 ) ) ;
#75465 = CARTESIAN_POINT ( 'NONE',  ( 34.42499999999998295, 22.22500000000000142, 5.000000000000000000 ) ) ;
#75466 = CARTESIAN_POINT ( 'NONE',  ( 99.31293019189810423, -1.637169565754159617, -6.110000000000001208 ) ) ;
#75467 = ORIENTED_EDGE ( 'NONE', *, *, #115859, .T. ) ;
#75468 = CARTESIAN_POINT ( 'NONE',  ( -1.915787159634013470, 12.50960769155452468, -26.80828596576004941 ) ) ;
#75469 = SURFACE_STYLE_FILL_AREA ( #41391 ) ;
#75470 = CARTESIAN_POINT ( 'NONE',  ( 20.81601139373100295, 28.73617430169773002, 5.000000000000000000 ) ) ;
#75471 = DIRECTION ( 'NONE',  ( -0.7071067811865486830, -0.7071067811865464625, 0.000000000000000000 ) ) ;
#75472 = DIRECTION ( 'NONE',  ( 0.7071067811865487940, 0.7071067811865463515, 0.000000000000000000 ) ) ;
#75473 = DIRECTION ( 'NONE',  ( 0.6830127018922180770, -0.6830127018922204085, -0.2588190451025213501 ) ) ;
#75474 = CARTESIAN_POINT ( 'NONE',  ( 31.14169371712956291, -2.130196079827424871, -7.949999999999999289 ) ) ;
#75475 = CARTESIAN_POINT ( 'NONE',  ( 6.932893218813446445, -34.80096641561353010, 18.05156865852269021 ) ) ;
#75476 = ORIENTED_EDGE ( 'NONE', *, *, #66124, .F. ) ;
#75477 = ORIENTED_EDGE ( 'NONE', *, *, #9165, .F. ) ;
#75478 = CARTESIAN_POINT ( 'NONE',  ( 25.49999999999999645, 0.000000000000000000, -7.950000000000000178 ) ) ;
#75479 = ORIENTED_EDGE ( 'NONE', *, *, #62909, .F. ) ;
#75480 = EDGE_CURVE ( 'NONE', #95062, #16368, #69383, .T. ) ;
#75481 = DIRECTION ( 'NONE',  ( 1.000000000000000000, 1.224606353822377258E-16, 0.000000000000000000 ) ) ;
#75482 = DIRECTION ( 'NONE',  ( -0.000000000000000000, 1.000000000000000000, -0.000000000000000000 ) ) ;
#75483 = CARTESIAN_POINT ( 'NONE',  ( 14.99999999999991296, 20.58746187583903620, 4.000000000000000000 ) ) ;
#75484 = EDGE_CURVE ( 'NONE', #100092, #62391, #32432, .T. ) ;
#75485 = CARTESIAN_POINT ( 'NONE',  ( -11.81601139373100651, 28.73617430169779041, 5.000000000000000000 ) ) ;
#75486 = CARTESIAN_POINT ( 'NONE',  ( 119.2037635252314658, 6.109999999999998543, 1.122388791418548911E-15 ) ) ;
#75487 = ORIENTED_EDGE ( 'NONE', *, *, #101551, .F. ) ;
#75488 = CARTESIAN_POINT ( 'NONE',  ( 18.48921356237309510, -27.52281430457068367, 5.000000000000000000 ) ) ;
#75489 = VERTEX_POINT ( 'NONE', #133911 ) ;
#75490 = CARTESIAN_POINT ( 'NONE',  ( -27.48921356237309155, -27.52281430457074762, 5.000000000000000000 ) ) ;
#75491 = CARTESIAN_POINT ( 'NONE',  ( -2.994519915287485734, 28.92564299267940342, 4.000000000000000000 ) ) ;
#75492 = DIRECTION ( 'NONE',  ( -0.7071067811865486830, -0.7071067811865464625, -0.000000000000000000 ) ) ;
#75493 = FACE_OUTER_BOUND ( 'NONE', #84141, .T. ) ;
#75494 = ORIENTED_EDGE ( 'NONE', *, *, #122900, .F. ) ;
#75495 = EDGE_CURVE ( 'NONE', #47009, #88720, #88996, .T. ) ;
#75496 = CARTESIAN_POINT ( 'NONE',  ( 47.97959685856477563, 6.109999999999999432, 1.637169565754164280 ) ) ;
#75497 = EDGE_LOOP ( 'NONE', ( #79750, #110260, #20933, #104327 ) ) ;
#75498 = LINE ( 'NONE', #63231, #5401 ) ;
#75499 = CARTESIAN_POINT ( 'NONE',  ( 17.99451991528748351, 28.92564299267950645, 4.000000000000000000 ) ) ;
#75500 = CARTESIAN_POINT ( 'NONE',  ( -12.19999999999999929, -59.76999999999998892, -39.50000000000000000 ) ) ;
#75501 = CARTESIAN_POINT ( 'NONE',  ( 26.99999999999980815, 11.58746187583913390, 4.000000000000000000 ) ) ;
#75502 = VECTOR ( 'NONE', #51976, 1000.000000000000000 ) ;
#75503 = EDGE_CURVE ( 'NONE', #67140, #13632, #136044, .T. ) ;
#75504 = CARTESIAN_POINT ( 'NONE',  ( 35.78709685856478018, 3.054999999999997495, 5.291415217122919401 ) ) ;
#75505 = ORIENTED_EDGE ( 'NONE', *, *, #53404, .F. ) ;
#75506 = AXIS2_PLACEMENT_3D ( 'NONE', #72512, #105772, #140561 ) ;
#75507 = CARTESIAN_POINT ( 'NONE',  ( 34.42499999999998295, -4.458600742197917910, 5.000000000000000000 ) ) ;
#75508 = VERTEX_POINT ( 'NONE', #68675 ) ;
#75509 = ORIENTED_EDGE ( 'NONE', *, *, #78533, .T. ) ;
#75510 = ORIENTED_EDGE ( 'NONE', *, *, #13181, .T. ) ;
#75511 = ADVANCED_FACE ( 'NONE', ( #36047 ), #69498, .T. ) ;
#75512 = ADVANCED_FACE ( 'NONE', ( #113568 ), #12112, .F. ) ;
#75513 = CARTESIAN_POINT ( 'NONE',  ( 79.55836038379622721, -7.949999999999996625, -2.130196079827426203 ) ) ;
#75514 = VERTEX_POINT ( 'NONE', #110688 ) ;
#75515 = CARTESIAN_POINT ( 'NONE',  ( -34.45011844616454511, 6.002304141593897135, 5.000000000000000888 ) ) ;
#75516 = MECHANICAL_DESIGN_GEOMETRIC_PRESENTATION_REPRESENTATION (  '', ( #38462 ), #26860 ) ;
#75517 = PLANE ( 'NONE',  #43303 ) ;
#75518 = DIRECTION ( 'NONE',  ( 0.7071067811865486830, -0.7071067811865464625, -0.000000000000000000 ) ) ;
#75519 = DIRECTION ( 'NONE',  ( 0.7071067811865487940, -0.7071067811865463515, 0.000000000000000000 ) ) ;
#75521 = FACE_BOUND ( 'NONE', #124885, .T. ) ;
#75520 = AXIS2_PLACEMENT_3D ( 'NONE', #46280, #59298, #70186 ) ;
#75523 = EDGE_CURVE ( 'NONE', #16561, #96125, #91144, .T. ) ;
#75522 = ORIENTED_EDGE ( 'NONE', *, *, #37126, .T. ) ;
#75524 = LINE ( 'NONE', #6636, #66499 ) ;
#75525 = DIRECTION ( 'NONE',  ( 0.7071067811865486830, -0.7071067811865464625, -0.000000000000000000 ) ) ;
#75526 = CARTESIAN_POINT ( 'NONE',  ( 6.707106781186498168, 17.25929247661554911, 5.000000000000000000 ) ) ;
#75527 = ORIENTED_EDGE ( 'NONE', *, *, #50898, .F. ) ;
#75528 = CARTESIAN_POINT ( 'NONE',  ( -44.99451991528749772, 28.92564299267969474, 4.000000000000000000 ) ) ;
#75529 = ORIENTED_EDGE ( 'NONE', *, *, #91601, .F. ) ;
#75530 = ORIENTED_EDGE ( 'NONE', *, *, #43024, .F. ) ;
#75531 = DIRECTION ( 'NONE',  ( 0.6830127018922180770, -0.6830127018922204085, -0.2588190451025213501 ) ) ;
#75532 = AXIS2_PLACEMENT_3D ( 'NONE', #26986, #125613, #105262 ) ;
#75533 = ORIENTED_EDGE ( 'NONE', *, *, #112209, .F. ) ;
#75534 = VECTOR ( 'NONE', #9681, 1000.000000000000000 ) ;
#75535 = AXIS2_PLACEMENT_3D ( 'NONE', #68192, #112366, #13022 ) ;
#75536 = CARTESIAN_POINT ( 'NONE',  ( 56.93293019189810877, 1.637169565754156508, 6.110000000000000320 ) ) ;
#75537 = ORIENTED_EDGE ( 'NONE', *, *, #45168, .F. ) ;
#75538 = DIRECTION ( 'NONE',  ( -0.000000000000000000, 0.3543493200069153248, 0.9351131265310292928 ) ) ;
#75539 = VERTEX_POINT ( 'NONE', #101995 ) ;
#75540 = VECTOR ( 'NONE', #117334, 1000.000000000000000 ) ;
#75541 = CARTESIAN_POINT ( 'NONE',  ( -12.15612307739231923, -22.22499999999999432, 4.000000000000000000 ) ) ;
#75542 = ORIENTED_EDGE ( 'NONE', *, *, #95009, .T. ) ;
#75543 = DIRECTION ( 'NONE',  ( 0.7071067811865487940, 0.7071067811865463515, 0.000000000000000000 ) ) ;
#75544 = CARTESIAN_POINT ( 'NONE',  ( 0.000000000000000000, 0.000000000000000000, 0.000000000000000000 ) ) ;
#75545 = AXIS2_PLACEMENT_3D ( 'NONE', #102200, #24617, #35543 ) ;
#75546 = LINE ( 'NONE', #119719, #57205 ) ;
#75547 = SURFACE_STYLE_USAGE ( .BOTH. , #8791 ) ;
#75548 = CARTESIAN_POINT ( 'NONE',  ( 10.49999999999992184, 22.01701374228156283, 2.453858888625607193 ) ) ;
#75549 = PLANE ( 'NONE',  #137380 ) ;
#75550 = PLANE ( 'NONE',  #57947 ) ;
#75551 = ORIENTED_EDGE ( 'NONE', *, *, #28033, .T. ) ;
#75552 = EDGE_CURVE ( 'NONE', #9731, #76434, #134373, .T. ) ;
#75553 = ORIENTED_EDGE ( 'NONE', *, *, #92454, .T. ) ;
#75554 = EDGE_LOOP ( 'NONE', ( #50301, #15263, #64861, #46150 ) ) ;
#75555 = CARTESIAN_POINT ( 'NONE',  ( -27.79333936457828358, 21.75929247661549581, 4.998822639870701856 ) ) ;
#75556 = LINE ( 'NONE', #16889, #141623 ) ;
#75557 = ORIENTED_EDGE ( 'NONE', *, *, #105987, .T. ) ;
#75558 = ADVANCED_FACE ( 'NONE', ( #25857 ), #11369, .T. ) ;
#75559 = ORIENTED_EDGE ( 'NONE', *, *, #16759, .T. ) ;
#75560 = DIRECTION ( 'NONE',  ( 0.6830127018922181881, 0.6830127018922202975, -0.2588190451025214056 ) ) ;
#75561 = DIRECTION ( 'NONE',  ( 0.7071067811865487940, -0.7071067811865463515, 0.000000000000000000 ) ) ;
#75562 = EDGE_CURVE ( 'NONE', #45356, #139610, #111431, .T. ) ;
#75563 = ADVANCED_FACE ( 'NONE', ( #45506 ), #104101, .F. ) ;
#75564 = CARTESIAN_POINT ( 'NONE',  ( 17.91508676806227029, -12.74070752338415247, 18.74364270924358422 ) ) ;
#75565 = ORIENTED_EDGE ( 'NONE', *, *, #7229, .T. ) ;
#75566 = CARTESIAN_POINT ( 'NONE',  ( 9.183988606268997046, 28.73617430169793607, 5.000000000000000000 ) ) ;
#75568 = ADVANCED_FACE ( 'NONE', ( #16380 ), #17128, .T. ) ;
#75567 = CARTESIAN_POINT ( 'NONE',  ( 19.10813147593277250, 4.202752102959690472E-16, 0.000000000000000000 ) ) ;
#75569 = EDGE_CURVE ( 'NONE', #26874, #59437, #128739, .T. ) ;
#75570 = CARTESIAN_POINT ( 'NONE',  ( 19.60873647476855197, -5.808823158059033709, 5.808823158059035485 ) ) ;
#75571 = CARTESIAN_POINT ( 'NONE',  ( -24.18398860626899705, 28.73617430169804265, 5.000000000000000000 ) ) ;
#75572 = ADVANCED_FACE ( 'NONE', ( #126579 ), #70130, .F. ) ;
#75573 = ORIENTED_EDGE ( 'NONE', *, *, #29371, .T. ) ;
#75574 = CARTESIAN_POINT ( 'NONE',  ( 123.1412635252314374, 4.472830434245837594, 4.472830434245841147 ) ) ;
#75575 = EDGE_CURVE ( 'NONE', #108859, #125764, #93256, .T. ) ;
#75576 = DIRECTION ( 'NONE',  ( -0.7071067811865486830, -0.7071067811865464625, -0.000000000000000000 ) ) ;
#75577 = CARTESIAN_POINT ( 'NONE',  ( -34.92500000000001137, -5.993876922608009750, 4.000000000000000000 ) ) ;
#75579 = ORIENTED_EDGE ( 'NONE', *, *, #12955, .F. ) ;
#75578 = CARTESIAN_POINT ( 'NONE',  ( 15.70710678118643955, 11.25929247661560950, 5.000000000000000000 ) ) ;
#75580 = AXIS2_PLACEMENT_3D ( 'NONE', #50502, #6938, #17834 ) ;
#75581 = CARTESIAN_POINT ( 'NONE',  ( 66.87086038379622721, 6.884901960086289741, -3.974999999999993427 ) ) ;
#75582 = ORIENTED_EDGE ( 'NONE', *, *, #40066, .F. ) ;
#75583 = ADVANCED_FACE ( 'NONE', ( #72978 ), #114290, .T. ) ;
#75584 = DIRECTION ( 'NONE',  ( -0.7071067811865486830, -0.7071067811865464625, 0.000000000000000000 ) ) ;
#75585 = CARTESIAN_POINT ( 'NONE',  ( 26.40000000000000568, -17.48000000000005016, -12.70000000000045404 ) ) ;
#75586 = LINE ( 'NONE', #119755, #44935 ) ;
#75587 = ORIENTED_EDGE ( 'NONE', *, *, #56967, .F. ) ;
#75588 = EDGE_CURVE ( 'NONE', #98816, #113076, #115679, .T. ) ;
#75589 = CARTESIAN_POINT ( 'NONE',  ( 15.49238828748955576, 4.584330080086930965E-16, 0.000000000000000000 ) ) ;
#75590 = CARTESIAN_POINT ( 'NONE',  ( -23.47599861414534672, 22.03583458319436872, 4.979811245910092055 ) ) ;
#75591 = VECTOR ( 'NONE', #59076, 1000.000000000000000 ) ;
#75592 = VERTEX_POINT ( 'NONE', #136750 ) ;
#75593 = CARTESIAN_POINT ( 'NONE',  ( -27.18398860626900060, 28.73617430169806042, 5.000000000000000000 ) ) ;
#75594 = DIRECTION ( 'NONE',  ( 0.7071067811865486830, -0.7071067811865464625, -0.000000000000000000 ) ) ;
#75595 = ORIENTED_EDGE ( 'NONE', *, *, #50395, .T. ) ;
#75596 = EDGE_CURVE ( 'NONE', #85671, #18530, #50479, .T. ) ;
#75597 = CARTESIAN_POINT ( 'NONE',  ( -5.916851932270658310, 21.75929247661548871, 7.311836541448040627 ) ) ;
#75598 = CARTESIAN_POINT ( 'NONE',  ( 27.48921356237309155, -27.52281430457074762, 5.000000000000000000 ) ) ;
#75599 = ORIENTED_EDGE ( 'NONE', *, *, #135676, .F. ) ;
#75600 = ORIENTED_EDGE ( 'NONE', *, *, #77714, .F. ) ;
#75601 = CARTESIAN_POINT ( 'NONE',  ( 72.29974487139158157, -27.71228299555256669, 4.000000000000000000 ) ) ;
#75602 = CARTESIAN_POINT ( 'NONE',  ( 0.3281693992235289459, -0.7407075233842805861, 4.000000000000000000 ) ) ;
#75603 = EDGE_CURVE ( 'NONE', #49858, #1646, #4042, .T. ) ;
#75604 = AXIS2_PLACEMENT_3D ( 'NONE', #4677, #48977, #104765 ) ;
#75605 = CARTESIAN_POINT ( 'NONE',  ( 19.05000000000000071, 3.174999999999997158, 4.000000000000000000 ) ) ;
#75606 = PLANE ( 'NONE',  #64649 ) ;
#75607 = CARTESIAN_POINT ( 'NONE',  ( 18.18398860626898994, 28.73617430169800002, 5.000000000000000000 ) ) ;
#75608 = PRESENTATION_LAYER_ASSIGNMENT (  '', '', ( #33909 ) ) ;
#75609 = VERTEX_POINT ( 'NONE', #83103 ) ;
#75610 = DIRECTION ( 'NONE',  ( 0.7071067811865486830, -0.7071067811865463515, 0.000000000000000000 ) ) ;
#75611 = LINE ( 'NONE', #119785, #97967 ) ;
#75612 = CARTESIAN_POINT ( 'NONE',  ( 126.5282023469572152, -6.688762929388991196, -1.806560149088825895 ) ) ;
#75613 = CARTESIAN_POINT ( 'NONE',  ( 39.28709685856478018, 3.054999999999997939, 5.291415217122920289 ) ) ;
#75614 = CARTESIAN_POINT ( 'NONE',  ( -17.67183060077634593, -18.74070752338409207, 4.000000000000000000 ) ) ;
#75615 = VERTEX_POINT ( 'NONE', #83850 ) ;
#75616 = ORIENTED_EDGE ( 'NONE', *, *, #141851, .T. ) ;
#75617 = EDGE_CURVE ( 'NONE', #55039, #67716, #6914, .T. ) ;
#75618 = DIRECTION ( 'NONE',  ( -0.000000000000000000, 0.3543493200069153248, 0.9351131265310292928 ) ) ;
#75619 = ORIENTED_EDGE ( 'NONE', *, *, #91372, .T. ) ;
#75620 = VECTOR ( 'NONE', #16464, 1000.000000000000227 ) ;
#75621 = EDGE_CURVE ( 'NONE', #85320, #52679, #138922, .T. ) ;
#75622 = ORIENTED_EDGE ( 'NONE', *, *, #40849, .F. ) ;
#75623 = CARTESIAN_POINT ( 'NONE',  ( 29.99999999999980105, -4.447814304570781196, 5.000000000000000000 ) ) ;
#75624 = FACE_OUTER_BOUND ( 'NONE', #124777, .T. ) ;
#75625 = ORIENTED_EDGE ( 'NONE', *, *, #111236, .T. ) ;
#75626 = EDGE_CURVE ( 'NONE', #12371, #80353, #48329, .T. ) ;
#75627 = DIRECTION ( 'NONE',  ( 0.7071067811865486830, -0.7071067811865464625, -0.000000000000000000 ) ) ;
#75628 = CARTESIAN_POINT ( 'NONE',  ( 8.501836514860380944, -17.24070752338410628, 8.407044977365202953 ) ) ;
#75629 = LINE ( 'NONE', #118389, #83432 ) ;
#75630 = CARTESIAN_POINT ( 'NONE',  ( 82.95833333333332860, 3.974999999999997424, 6.884901960086288852 ) ) ;
#75631 = LINE ( 'NONE', #64747, #114799 ) ;
#75632 = ORIENTED_EDGE ( 'NONE', *, *, #45824, .T. ) ;
#75633 = DIRECTION ( 'NONE',  ( 0.3543493200069162685, -0.000000000000000000, -0.9351131265310288487 ) ) ;
#75634 = LINE ( 'NONE', #40858, #547 ) ;
#75635 = CARTESIAN_POINT ( 'NONE',  ( 17.39159235450332019, -2.500000000000000444, 3.061616997868384620E-16 ) ) ;
#75636 = DIRECTION ( 'NONE',  ( 0.000000000000000000, 1.000000000000000000, 0.000000000000000000 ) ) ;
#75637 = CARTESIAN_POINT ( 'NONE',  ( 0.000000000000000000, 0.000000000000000000, 5.000000000000000000 ) ) ;
#75638 = AXIS2_PLACEMENT_3D ( 'NONE', #142887, #20, #44315 ) ;
#75639 = DIRECTION ( 'NONE',  ( 0.7071067811865487940, 0.7071067811865463515, 0.000000000000000000 ) ) ;
#75640 = PLANE ( 'NONE',  #6414 ) ;
#75641 = AXIS2_PLACEMENT_3D ( 'NONE', #23976, #124708, #46486 ) ;
#75642 = CARTESIAN_POINT ( 'NONE',  ( 55.20419371712956291, -6.884901960086285300, -3.975000000000000089 ) ) ;
#75643 = VECTOR ( 'NONE', #13927, 1000.000000000000000 ) ;
#75644 = LINE ( 'NONE', #64761, #120192 ) ;
#75645 = ORIENTED_EDGE ( 'NONE', *, *, #61697, .F. ) ;
#75646 = ORIENTED_EDGE ( 'NONE', *, *, #117639, .F. ) ;
#75647 = CARTESIAN_POINT ( 'NONE',  ( 58.75000000000000000, -9.735942053221458872E-16, 7.950000000000000178 ) ) ;
#75648 = LINE ( 'NONE', #13029, #16980 ) ;
#75649 = ADVANCED_FACE ( 'NONE', ( #28008 ), #15647, .F. ) ;
#75650 = DIRECTION ( 'NONE',  ( 0.7071067811865487940, 0.7071067811865463515, 0.000000000000000000 ) ) ;
#75651 = CARTESIAN_POINT ( 'NONE',  ( -21.70701326429289324, -21.74070752338406010, 4.999753212805221558 ) ) ;
#75652 = ORIENTED_EDGE ( 'NONE', *, *, #28168, .F. ) ;
#75653 = DIRECTION ( 'NONE',  ( -0.7071067811865487940, 0.7071067811865463515, 0.000000000000000000 ) ) ;
#75654 = CARTESIAN_POINT ( 'NONE',  ( 13.24976746729824129, 4.588264127556670680, 4.661243073242808066 ) ) ;
#75655 = CARTESIAN_POINT ( 'NONE',  ( 43.02126352523142572, -4.472830434245839371, -4.472830434245840259 ) ) ;
#75656 = EDGE_LOOP ( 'NONE', ( #110004, #99383, #64694, #54410, #132737, #38220 ) ) ;
#75657 =( NAMED_UNIT ( * ) SI_UNIT ( $, .STERADIAN. ) SOLID_ANGLE_UNIT ( ) );
#75658 = ORIENTED_EDGE ( 'NONE', *, *, #137782, .F. ) ;
#75659 = ORIENTED_EDGE ( 'NONE', *, *, #140869, .T. ) ;
#75660 = CARTESIAN_POINT ( 'NONE',  ( 0.000000000000000000, 0.000000000000000000, -4.487534009422227577 ) ) ;
#75661 = CARTESIAN_POINT ( 'NONE',  ( -1.396568071053559734, -14.24070752338413648, 19.24067776001725960 ) ) ;
#75662 = DIRECTION ( 'NONE',  ( 0.000000000000000000, -1.000000000000000000, 0.000000000000000000 ) ) ;
#75663 = CARTESIAN_POINT ( 'NONE',  ( 16.99806943317890529, -22.22500000000000142, 4.500000000000000888 ) ) ;
#75664 = ORIENTED_EDGE ( 'NONE', *, *, #24678, .T. ) ;
#75665 = EDGE_CURVE ( 'NONE', #35917, #73867, #76735, .T. ) ;
#75666 = CARTESIAN_POINT ( 'NONE',  ( 17.06332250466817158, 4.584330080086930965E-16, 0.000000000000000000 ) ) ;
#75668 = ORIENTED_EDGE ( 'NONE', *, *, #45645, .T. ) ;
#75667 = DIRECTION ( 'NONE',  ( -0.000000000000000000, -0.000000000000000000, 1.000000000000000000 ) ) ;
#75669 = CARTESIAN_POINT ( 'NONE',  ( 82.54209685856478984, 5.291415217122923842, -3.054999999999996163 ) ) ;
#75670 = CARTESIAN_POINT ( 'NONE',  ( 0.000000000000000000, -0.4000000000000003553, 2.015694669338588429 ) ) ;
#75671 = FACE_OUTER_BOUND ( 'NONE', #24898, .T. ) ;
#75672 = CARTESIAN_POINT ( 'NONE',  ( 34.92499999999998295, -21.72500000000000142, 5.000000000000000000 ) ) ;
#75673 = CARTESIAN_POINT ( 'NONE',  ( -33.32816939922328459, 20.25929247661552779, 4.000000000000000000 ) ) ;
#75674 = CARTESIAN_POINT ( 'NONE',  ( -34.17183060077623225, -17.24070752338410983, 4.000000000000000000 ) ) ;
#75675 = EDGE_CURVE ( 'NONE', #29061, #136372, #11591, .T. ) ;
#75676 = VERTEX_POINT ( 'NONE', #62083 ) ;
#75677 = AXIS2_PLACEMENT_3D ( 'NONE', #121712, #110822, #57225 ) ;
#75678 = FACE_OUTER_BOUND ( 'NONE', #130412, .T. ) ;
#75679 = CARTESIAN_POINT ( 'NONE',  ( 68.74543019189812298, -5.291415217122918513, -3.055000000000000160 ) ) ;
#75680 = DIRECTION ( 'NONE',  ( -0.3543493200069162685, -0.000000000000000000, -0.9351131265310288487 ) ) ;
#75681 = CARTESIAN_POINT ( 'NONE',  ( -28.00193056682078918, -22.22500000000000142, 4.500000000000000888 ) ) ;
#75682 = DIRECTION ( 'NONE',  ( 0.7071067811865487940, -0.7071067811865463515, 0.000000000000000000 ) ) ;
#75683 = VERTEX_POINT ( 'NONE', #95396 ) ;
#75684 = EDGE_LOOP ( 'NONE', ( #96101, #86080, #85590, #142193 ) ) ;
#75685 = VECTOR ( 'NONE', #116653, 1000.000000000000227 ) ;
#75686 = DIRECTION ( 'NONE',  ( 0.7071067811865487940, 0.7071067811865463515, 0.000000000000000000 ) ) ;
#75687 = ORIENTED_EDGE ( 'NONE', *, *, #90380, .T. ) ;
#75688 = EDGE_CURVE ( 'NONE', #53690, #122791, #84547, .T. ) ;
#75689 = VERTEX_POINT ( 'NONE', #120704 ) ;
#75690 = ADVANCED_FACE ( 'NONE', ( #130913 ), #141035, .F. ) ;
#75691 = CARTESIAN_POINT ( 'NONE',  ( 28.49999999999980460, 22.01701374228157704, 2.453858888625564560 ) ) ;
#75692 = EDGE_LOOP ( 'NONE', ( #12018, #15001, #139369, #16727, #126242, #115717 ) ) ;
#75693 = LINE ( 'NONE', #131498, #86253 ) ;
#75694 = LINE ( 'NONE', #18408, #108083 ) ;
#75695 = AXIS2_PLACEMENT_3D ( 'NONE', #32108, #99473, #55302 ) ;
#75696 = CARTESIAN_POINT ( 'NONE',  ( 39.48921356237310221, -27.52281430457082934, 5.000000000000000000 ) ) ;
#75697 = VECTOR ( 'NONE', #83365, 1000.000000000000227 ) ;
#75698 = FACE_BOUND ( 'NONE', #32676, .T. ) ;
#75699 = EDGE_CURVE ( 'NONE', #41122, #128067, #41740, .T. ) ;
#75700 = FACE_OUTER_BOUND ( 'NONE', #78602, .T. ) ;
#75701 = CARTESIAN_POINT ( 'NONE',  ( -21.96495920677946856, -2.033836129387410985, 4.000000000000000000 ) ) ;
#75702 = LINE ( 'NONE', #140931, #1686 ) ;
#75704 = ORIENTED_EDGE ( 'NONE', *, *, #22505, .T. ) ;
#75703 = CARTESIAN_POINT ( 'NONE',  ( 7.940000000000001279, -35.14999999999999858, -8.101350000000007157 ) ) ;
#75705 = CARTESIAN_POINT ( 'NONE',  ( 14.81601139373099585, 28.73617430169776910, 5.000000000000000000 ) ) ;
#75706 = ITEM_DEFINED_TRANSFORMATION ( 'NONE', 'NONE', #139685,  #127880 ) ;
#75708 = VERTEX_POINT ( 'NONE', #53313 ) ;
#75707 = AXIS2_PLACEMENT_3D ( 'NONE', #58110, #23268, #21862 ) ;
#75709 = EDGE_LOOP ( 'NONE', ( #31171, #7179, #117223, #21202 ) ) ;
#75710 = CARTESIAN_POINT ( 'NONE',  ( 81.72459685856476597, -1.637169565754160949, 6.109999999999997655 ) ) ;
#75711 = VERTEX_POINT ( 'NONE', #98268 ) ;
#75712 = CARTESIAN_POINT ( 'NONE',  ( -23.29298673570678702, -21.74070752338405299, 4.999753212805217117 ) ) ;
#75713 = CARTESIAN_POINT ( 'NONE',  ( -5.816011393731002066, 28.73617430169783304, 5.000000000000000000 ) ) ;
#75714 = VERTEX_POINT ( 'NONE', #87395 ) ;
#75715 = DIRECTION ( 'NONE',  ( 0.000000000000000000, -1.000000000000000000, 0.000000000000000000 ) ) ;
#75716 = CARTESIAN_POINT ( 'NONE',  ( 3.250000000000000000, 0.000000000000000000, 4.999999999999998224 ) ) ;
#75717 = LINE ( 'NONE', #8962, #120056 ) ;
#75718 = DIRECTION ( 'NONE',  ( 1.000000000000000000, 1.224606353822377258E-16, 0.000000000000000000 ) ) ;
#75719 = PLANE ( 'NONE',  #1850 ) ;
#75720 = CARTESIAN_POINT ( 'NONE',  ( -28.82816939922332722, -2.240707523384255939, 4.000000000000000000 ) ) ;
#75721 = CARTESIAN_POINT ( 'NONE',  ( 0.4000000000000001887, 0.000000000000000000, -1.249999999999969802 ) ) ;
#75722 = DIRECTION ( 'NONE',  ( -1.000000000000000000, -1.224606353822377258E-16, -0.000000000000000000 ) ) ;
#75723 = EDGE_LOOP ( 'NONE', ( #9055, #136149, #114252, #137324 ) ) ;
#75724 = CYLINDRICAL_SURFACE ( 'NONE', #107065, 6.094999999999989093 ) ;
#75725 = VERTEX_POINT ( 'NONE', #98951 ) ;
#75726 = CARTESIAN_POINT ( 'NONE',  ( -7.171830600776418763, -2.240707523384260824, 4.000000000000000000 ) ) ;
#75727 = DIRECTION ( 'NONE',  ( -0.7071067811865486830, -0.7071067811865464625, 0.000000000000000000 ) ) ;
#75728 = ORIENTED_EDGE ( 'NONE', *, *, #135977, .F. ) ;
#75730 = ORIENTED_EDGE ( 'NONE', *, *, #142204, .T. ) ;
#75729 = AXIS2_PLACEMENT_3D ( 'NONE', #66598, #121656, #33289 ) ;
#75731 = VERTEX_POINT ( 'NONE', #65683 ) ;
#75732 = CARTESIAN_POINT ( 'NONE',  ( 32.37543019189810423, -5.291415217122920289, -3.055000000000001492 ) ) ;
#75733 = EDGE_LOOP ( 'NONE', ( #66839, #81636, #128340, #18132 ) ) ;
#75734 = CARTESIAN_POINT ( 'NONE',  ( 92.53752705046289861, -9.735942053221456900E-16, 7.949999999999998401 ) ) ;
#75735 = AXIS2_PLACEMENT_3D ( 'NONE', #140922, #141667, #119175 ) ;
#75736 = VECTOR ( 'NONE', #9491, 1000.000000000000000 ) ;
#75737 = FACE_OUTER_BOUND ( 'NONE', #128792, .T. ) ;
#75739 = EDGE_CURVE ( 'NONE', #115165, #136354, #74387, .T. ) ;
#75738 = AXIS2_PLACEMENT_3D ( 'NONE', #84919, #138601, #52984 ) ;
#75740 = CARTESIAN_POINT ( 'NONE',  ( 25.12913961620377279, 5.278424836066147208, 3.047499999999990550 ) ) ;
#75741 = CARTESIAN_POINT ( 'NONE',  ( 4.546519005068298647, 12.01231087727541968, -27.25263027609279831 ) ) ;
#75742 = EDGE_CURVE ( 'NONE', #38188, #65156, #31584, .T. ) ;
#75743 = ORIENTED_EDGE ( 'NONE', *, *, #103956, .F. ) ;
#75744 = FACE_OUTER_BOUND ( 'NONE', #6708, .T. ) ;
#75746 = ORIENTED_EDGE ( 'NONE', *, *, #129757, .T. ) ;
#75745 = EDGE_CURVE ( 'NONE', #80320, #50236, #75807, .T. ) ;
#75747 = DIRECTION ( 'NONE',  ( -1.000000000000000000, -1.224606353822377258E-16, -0.000000000000000000 ) ) ;
#75748 = VECTOR ( 'NONE', #32140, 999.9999999999998863 ) ;
#75749 = FACE_OUTER_BOUND ( 'NONE', #132379, .T. ) ;
#75751 = ORIENTED_EDGE ( 'NONE', *, *, #84508, .T. ) ;
#75750 = DIRECTION ( 'NONE',  ( 0.7071067811865487940, 0.7071067811865463515, 0.000000000000000000 ) ) ;
#75752 = ORIENTED_EDGE ( 'NONE', *, *, #32747, .F. ) ;
#75753 = EDGE_CURVE ( 'NONE', #94242, #6978, #141784, .T. ) ;
#75754 = FACE_OUTER_BOUND ( 'NONE', #35996, .T. ) ;
#75755 = DIRECTION ( 'NONE',  ( -0.000000000000000000, -0.3543493200069152693, 0.9351131265310292928 ) ) ;
#75756 = CARTESIAN_POINT ( 'NONE',  ( 8.994519915287490619, 28.92564299267944250, 4.000000000000000000 ) ) ;
#75757 = ORIENTED_EDGE ( 'NONE', *, *, #101040, .T. ) ;
#75758 = CARTESIAN_POINT ( 'NONE',  ( 12.48921356237309155, -27.52281430457064104, 5.000000000000000000 ) ) ;
#75759 = ORIENTED_EDGE ( 'NONE', *, *, #62584, .T. ) ;
#75760 = EDGE_LOOP ( 'NONE', ( #23891, #2224, #139022, #87116 ) ) ;
#75761 = VERTEX_POINT ( 'NONE', #41021 ) ;
#75762 = EDGE_CURVE ( 'NONE', #23165, #78911, #85955, .T. ) ;
#75763 = DIRECTION ( 'NONE',  ( -1.000000000000000000, -0.000000000000000000, -0.000000000000000000 ) ) ;
#75764 = CARTESIAN_POINT ( 'NONE',  ( -14.99999999999989875, 7.931123077392104648, 4.000000000000000000 ) ) ;
#75765 = CARTESIAN_POINT ( 'NONE',  ( 34.92499999999998295, 22.22500000000000142, 4.000000000000000000 ) ) ;
#75766 = DIRECTION ( 'NONE',  ( -0.000000000000000000, -0.3543493200069152693, 0.9351131265310292928 ) ) ;
#75767 = DIRECTION ( 'NONE',  ( 0.7071067811865487940, 0.7071067811865463515, -0.000000000000000000 ) ) ;
#75768 = EDGE_CURVE ( 'NONE', #16920, #33497, #91538, .T. ) ;
#75769 = CARTESIAN_POINT ( 'NONE',  ( -18.32816939922339117, -18.74070752338409562, 4.000000000000000000 ) ) ;
#75770 = CARTESIAN_POINT ( 'NONE',  ( 9.489213562373095101, -27.52281430457062328, 5.000000000000000000 ) ) ;
#75771 = EDGE_CURVE ( 'NONE', #54960, #81537, #10511, .T. ) ;
#75772 = ORIENTED_EDGE ( 'NONE', *, *, #52834, .F. ) ;
#75773 = DIRECTION ( 'NONE',  ( -0.6830127018922180770, -0.6830127018922204085, -0.2588190451025213501 ) ) ;
#75774 = ORIENTED_EDGE ( 'NONE', *, *, #68172, .T. ) ;
#75775 = AXIS2_PLACEMENT_3D ( 'NONE', #34918, #67561, #3649 ) ;
#75776 = LINE ( 'NONE', #109815, #88804 ) ;
#75777 = EDGE_CURVE ( 'NONE', #5899, #66460, #129449, .T. ) ;
#75778 = CARTESIAN_POINT ( 'NONE',  ( -63.18398860626900415, 28.73617430169831621, 5.000000000000000000 ) ) ;
#75779 = VECTOR ( 'NONE', #69264, 1000.000000000000000 ) ;
#75780 = ORIENTED_EDGE ( 'NONE', *, *, #114096, .T. ) ;
#75781 = LINE ( 'NONE', #86660, #4328 ) ;
#75782 = LINE ( 'NONE', #85924, #67539 ) ;
#75783 = ORIENTED_EDGE ( 'NONE', *, *, #138887, .T. ) ;
#75784 = VERTEX_POINT ( 'NONE', #76530 ) ;
#75785 = DIRECTION ( 'NONE',  ( -0.7071067811865487940, 0.7071067811865463515, -0.000000000000000000 ) ) ;
#75786 = CARTESIAN_POINT ( 'NONE',  ( -24.18398860626899705, 28.73617430169804265, 5.000000000000000000 ) ) ;
#75787 = CARTESIAN_POINT ( 'NONE',  ( 26.24139925780185578, 21.72500000000000142, 5.000000000000000000 ) ) ;
#75788 =( LENGTH_UNIT ( ) NAMED_UNIT ( * ) SI_UNIT ( .MILLI., .METRE. ) );
#75789 = FACE_OUTER_BOUND ( 'NONE', #12857, .T. ) ;
#75790 = CARTESIAN_POINT ( 'NONE',  ( 62.47459685856478018, 1.637169565754164280, -6.109999999999997655 ) ) ;
#75791 = LINE ( 'NONE', #107677, #30197 ) ;
#75792 = CARTESIAN_POINT ( 'NONE',  ( 5.999999999999954703, 7.931123077392102871, 4.000000000000000000 ) ) ;
#75793 = LINE ( 'NONE', #64917, #9371 ) ;
#75794 = LINE ( 'NONE', #65671, #25589 ) ;
#75795 = ORIENTED_EDGE ( 'NONE', *, *, #125963, .T. ) ;
#75796 = CARTESIAN_POINT ( 'NONE',  ( -32.99999999999976552, 11.96639925780213431, 5.000000000000000000 ) ) ;
#75797 = EDGE_CURVE ( 'NONE', #26207, #4325, #21418, .T. ) ;
#75798 = VECTOR ( 'NONE', #62998, 1000.000000000000000 ) ;
#75799 = VERTEX_POINT ( 'NONE', #63528 ) ;
#75800 = LINE ( 'NONE', #119961, #6095 ) ;
#75801 = DIRECTION ( 'NONE',  ( -0.6830127018922180770, -0.6830127018922204085, -0.2588190451025213501 ) ) ;
#75802 = VERTEX_POINT ( 'NONE', #18519 ) ;
#75803 = LINE ( 'NONE', #119966, #110898 ) ;
#75805 = ORIENTED_EDGE ( 'NONE', *, *, #57280, .T. ) ;
#75804 = DIRECTION ( 'NONE',  ( 0.7071067811865487940, 0.7071067811865463515, 0.000000000000000000 ) ) ;
#75806 = DIRECTION ( 'NONE',  ( -0.000000000000000000, 0.000000000000000000, 1.000000000000000000 ) ) ;
#75807 = LINE ( 'NONE', #119972, #71880 ) ;
#75808 = LINE ( 'NONE', #52606, #44967 ) ;
#75809 = ORIENTED_EDGE ( 'NONE', *, *, #6575, .F. ) ;
#75810 = ORIENTED_EDGE ( 'NONE', *, *, #68796, .T. ) ;
#75811 = DIRECTION ( 'NONE',  ( -1.000000000000000000, -1.224606353822377258E-16, -0.000000000000000000 ) ) ;
#75812 = LINE ( 'NONE', #29423, #7374 ) ;
#75813 = DIRECTION ( 'NONE',  ( 0.7071067811865486830, -0.7071067811865464625, -0.000000000000000000 ) ) ;
#75814 = ADVANCED_FACE ( 'NONE', ( #140336 ), #62801, .F. ) ;
#75815 = CARTESIAN_POINT ( 'NONE',  ( 15.05159235450332034, -2.500000000000000000, 3.061616997868384127E-16 ) ) ;
#75816 = CARTESIAN_POINT ( 'NONE',  ( 84.51669371712955581, 7.950000000000001066, -2.130196079827421318 ) ) ;
#75817 = FACE_OUTER_BOUND ( 'NONE', #116373, .T. ) ;
#75818 = CARTESIAN_POINT ( 'NONE',  ( 34.49999999999975842, -10.53574439159940113, 4.994342998332163219 ) ) ;
#75819 = ORIENTED_EDGE ( 'NONE', *, *, #117266, .F. ) ;
#75820 = VECTOR ( 'NONE', #76978, 1000.000000000000000 ) ;
#75821 = CARTESIAN_POINT ( 'NONE',  ( 3.489213562373097322, -27.52281430457057709, 5.000000000000000000 ) ) ;
#75822 = EDGE_CURVE ( 'NONE', #97989, #4786, #39483, .T. ) ;
#75823 = DIRECTION ( 'NONE',  ( 0.000000000000000000, -1.000000000000000000, 0.000000000000000000 ) ) ;
#75824 = CARTESIAN_POINT ( 'NONE',  ( -31.17183060077625001, 15.75929247661555443, 4.000000000000000000 ) ) ;
#75825 = ORIENTED_EDGE ( 'NONE', *, *, #39468, .T. ) ;
#75826 = DIRECTION ( 'NONE',  ( -0.000000000000000000, 0.3543493200069153248, 0.9351131265310292928 ) ) ;
#75827 = VERTEX_POINT ( 'NONE', #85223 ) ;
#75828 = ADVANCED_FACE ( 'NONE', ( #30133 ), #107692, .F. ) ;
#75829 = CARTESIAN_POINT ( 'NONE',  ( 72.47959685856478984, 6.109999999999999432, 1.637169565754164280 ) ) ;
#75830 = LINE ( 'NONE', #84569, #29199 ) ;
#75831 = DIRECTION ( 'NONE',  ( 1.000000000000000000, 0.000000000000000000, 0.000000000000000000 ) ) ;
#75832 = EDGE_LOOP ( 'NONE', ( #88250, #23229, #91821, #5142 ) ) ;
#75833 = DIRECTION ( 'NONE',  ( -1.000000000000000000, -1.224606353822377258E-16, -0.000000000000000000 ) ) ;
#75834 = VECTOR ( 'NONE', #57760, 1000.000000000000227 ) ;
#75835 = CARTESIAN_POINT ( 'NONE',  ( 20.99451991528748707, 28.92564299267952777, 4.000000000000000000 ) ) ;
#75836 =( GEOMETRIC_REPRESENTATION_CONTEXT ( 3 ) GLOBAL_UNCERTAINTY_ASSIGNED_CONTEXT ( ( #28567 ) ) GLOBAL_UNIT_ASSIGNED_CONTEXT ( ( #62873, #63596, #140401 ) ) REPRESENTATION_CONTEXT ( 'NONE', 'WORKASPACE' ) );
#75837 = DIRECTION ( 'NONE',  ( -0.3543493200069162685, -0.000000000000000000, -0.9351131265310288487 ) ) ;
#75838 = EDGE_CURVE ( 'NONE', #40937, #102057, #109125, .T. ) ;
#75839 = CARTESIAN_POINT ( 'NONE',  ( 23.51078643762690490, -27.52281430457038880, 5.000000000000000000 ) ) ;
#75841 = ORIENTED_EDGE ( 'NONE', *, *, #70029, .T. ) ;
#75840 = CARTESIAN_POINT ( 'NONE',  ( 32.99999999999977973, -9.033600742197641864, 5.000000000000000000 ) ) ;
#75842 = DIRECTION ( 'NONE',  ( 0.7071067811865487940, -0.7071067811865463515, 0.000000000000000000 ) ) ;
#75843 = LINE ( 'NONE', #20719, #107785 ) ;
#75844 = DIRECTION ( 'NONE',  ( -0.3543493200069162685, -0.000000000000000000, -0.9351131265310288487 ) ) ;
#75845 = AXIS2_PLACEMENT_3D ( 'NONE', #102107, #13631, #112268 ) ;
#75846 = VECTOR ( 'NONE', #230, 1000.000000000000000 ) ;
#75847 = ORIENTED_EDGE ( 'NONE', *, *, #88898, .T. ) ;
#75848 = ORIENTED_EDGE ( 'NONE', *, *, #7940, .F. ) ;
#75849 = AXIS2_PLACEMENT_3D ( 'NONE', #41965, #86180, #99158 ) ;
#75850 = CARTESIAN_POINT ( 'NONE',  ( 63.43793019189811133, -6.110000000000001208, 1.637169565754158951 ) ) ;
#75851 = ORIENTED_EDGE ( 'NONE', *, *, #80367, .F. ) ;
#75852 = PLANE ( 'NONE',  #5918 ) ;
#75853 = LINE ( 'NONE', #32344, #122116 ) ;
#75855 = FACE_OUTER_BOUND ( 'NONE', #26930, .T. ) ;
#75854 = VECTOR ( 'NONE', #63577, 1000.000000000000000 ) ;
#75856 = ORIENTED_EDGE ( 'NONE', *, *, #143083, .F. ) ;
#75857 = CARTESIAN_POINT ( 'NONE',  ( -15.48921356237309510, -27.52281430457066236, 5.000000000000000000 ) ) ;
#75858 =( LENGTH_UNIT ( ) NAMED_UNIT ( * ) SI_UNIT ( .MILLI., .METRE. ) );
#75859 = EDGE_LOOP ( 'NONE', ( #74709, #45834, #62314, #67976 ) ) ;
#75860 = EDGE_CURVE ( 'NONE', #33966, #112760, #109883, .T. ) ;
#75861 = LINE ( 'NONE', #96845, #32921 ) ;
#75862 = DIRECTION ( 'NONE',  ( 0.000000000000000000, 0.000000000000000000, 1.000000000000000000 ) ) ;
#75863 = DIRECTION ( 'NONE',  ( 0.6830127018922181881, 0.6830127018922202975, -0.2588190451025214056 ) ) ;
#75864 =( BOUNDED_CURVE ( )  B_SPLINE_CURVE ( 3, ( #68199, #101479, #78320, #110904 ),
 .UNSPECIFIED., .F., .T. ) 
 B_SPLINE_CURVE_WITH_KNOTS ( ( 4, 4 ),
 ( 5.536208752217765650, 5.573248253235211891 ),
 .UNSPECIFIED. ) 
 CURVE ( )  GEOMETRIC_REPRESENTATION_ITEM ( )  RATIONAL_B_SPLINE_CURVE ( ( 1.000000000000000000, 0.9998856762146628441, 0.9998856762146628441, 1.000000000000000000 ) ) 
 REPRESENTATION_ITEM ( '' )  );
#75865 = VERTEX_POINT ( 'NONE', #44641 ) ;
#75866 = EDGE_LOOP ( 'NONE', ( #55562, #12336, #42954, #112297 ) ) ;
#75867 = EDGE_CURVE ( 'NONE', #37645, #39717, #11202, .T. ) ;
#75868 = FACE_BOUND ( 'NONE', #111474, .T. ) ;
#75869 = EDGE_CURVE ( 'NONE', #131124, #126973, #79416, .T. ) ;
#75870 = CARTESIAN_POINT ( 'NONE',  ( -23.81601139373100295, 28.73617430169770870, 5.000000000000000000 ) ) ;
#75871 = DIRECTION ( 'NONE',  ( -0.7071067811865486830, -0.7071067811865464625, -0.000000000000000000 ) ) ;
#75872 = CARTESIAN_POINT ( 'NONE',  ( 62.10416666666666430, 2.130196079827422206, 7.950000000000001954 ) ) ;
#75873 = CARTESIAN_POINT ( 'NONE',  ( 0.000000000000000000, 0.000000000000000000, 5.000000000000000000 ) ) ;
#75874 = CARTESIAN_POINT ( 'NONE',  ( 42.48921356237308800, -27.52281430457085065, 5.000000000000000000 ) ) ;
#75875 =( NAMED_UNIT ( * ) SI_UNIT ( $, .STERADIAN. ) SOLID_ANGLE_UNIT ( ) );
#75876 = ORIENTED_EDGE ( 'NONE', *, *, #123134, .F. ) ;
#75877 = AXIS2_PLACEMENT_3D ( 'NONE', #94108, #117275, #84003 ) ;
#75878 = ORIENTED_EDGE ( 'NONE', *, *, #94098, .T. ) ;
#75879 = CARTESIAN_POINT ( 'NONE',  ( 114.3912635252314374, -4.472830434245838482, -4.472830434245838482 ) ) ;
#75880 = VERTEX_POINT ( 'NONE', #46791 ) ;
#75881 = ORIENTED_EDGE ( 'NONE', *, *, #111550, .F. ) ;
#75882 = CARTESIAN_POINT ( 'NONE',  ( 184.1499999999998067, -49.85820393249939286, 34.92500000000001847 ) ) ;
#75883 = ADVANCED_FACE ( 'NONE', ( #77944 ), #135202, .F. ) ;
#75884 = CARTESIAN_POINT ( 'NONE',  ( 23.70025512860841133, -27.71228299555189523, 4.000000000000000000 ) ) ;
#75885 = VERTEX_POINT ( 'NONE', #69213 ) ;
#75886 = CARTESIAN_POINT ( 'NONE',  ( -18.51168605928420519, 6.759292476615645917, 16.35960578974473734 ) ) ;
#75887 = CARTESIAN_POINT ( 'NONE',  ( 34.49999999999975131, -19.91253812416055879, 4.000000000000000000 ) ) ;
#75889 = FACE_OUTER_BOUND ( 'NONE', #113461, .T. ) ;
#75888 = DIRECTION ( 'NONE',  ( 0.7071067811865487940, 0.7071067811865463515, -0.000000000000000000 ) ) ;
#75890 = CARTESIAN_POINT ( 'NONE',  ( -15.70710678118643422, 20.25929247661551713, 5.000000000000000000 ) ) ;
#75891 = CARTESIAN_POINT ( 'NONE',  ( 1.312016898163277157, 0.1750100709684468681, 3.778747987217102366 ) ) ;
#75892 = ORIENTED_EDGE ( 'NONE', *, *, #130295, .F. ) ;
#75893 = CARTESIAN_POINT ( 'NONE',  ( -60.48921356237309510, -27.52281430457097500, 5.000000000000000000 ) ) ;
#75894 = DIRECTION ( 'NONE',  ( -0.000000000000000000, 1.000000000000000000, -0.000000000000000000 ) ) ;
#75895 = ORIENTED_EDGE ( 'NONE', *, *, #118983, .F. ) ;
#75896 = VERTEX_POINT ( 'NONE', #58380 ) ;
#75897 = ORIENTED_EDGE ( 'NONE', *, *, #49074, .F. ) ;
#75898 = CARTESIAN_POINT ( 'NONE',  ( 59.50043019189810423, -3.055000000000002380, 5.291415217122920289 ) ) ;
#75899 = ORIENTED_EDGE ( 'NONE', *, *, #20587, .T. ) ;
#75900 = CARTESIAN_POINT ( 'NONE',  ( 12.18398860626900060, 28.73617430169795739, 5.000000000000000000 ) ) ;
#75901 = EDGE_CURVE ( 'NONE', #92375, #39654, #35889, .T. ) ;
#75902 = CARTESIAN_POINT ( 'NONE',  ( -1.704193717129561136, -5.278424836066144543, 3.047499999999995879 ) ) ;
#75903 = VECTOR ( 'NONE', #48978, 1000.000000000000000 ) ;
#75904 = CARTESIAN_POINT ( 'NONE',  ( 104.2712635252314470, 4.472830434245838482, 4.472830434245842035 ) ) ;
#75905 = LINE ( 'NONE', #120077, #19374 ) ;
#75906 = ADVANCED_FACE ( 'NONE', ( #12658 ), #68514, .T. ) ;
#75907 = CARTESIAN_POINT ( 'NONE',  ( -39.29974487139159578, -27.71228299555233576, 4.000000000000000000 ) ) ;
#75908 = VERTEX_POINT ( 'NONE', #1053 ) ;
#75909 = LINE ( 'NONE', #20798, #2508 ) ;
#75910 = CARTESIAN_POINT ( 'NONE',  ( 23.99999999999983302, -3.033600742197707145, 5.000000000000000000 ) ) ;
#75911 = EDGE_CURVE ( 'NONE', #80946, #138457, #26734, .T. ) ;
#75912 = EDGE_CURVE ( 'NONE', #112149, #99304, #45342, .T. ) ;
#75913 = CARTESIAN_POINT ( 'NONE',  ( 7.326124847093153925, 4.202752102959690472E-16, 0.000000000000000000 ) ) ;
#75914 = DIRECTION ( 'NONE',  ( -0.7071067811865487940, 0.7071067811865463515, -0.000000000000000000 ) ) ;
#75915 = ORIENTED_EDGE ( 'NONE', *, *, #71343, .T. ) ;
#75916 = AXIS2_PLACEMENT_3D ( 'NONE', #35739, #35006, #125578 ) ;
#75917 = DIRECTION ( 'NONE',  ( 0.7071067811865486830, -0.7071067811865464625, -0.000000000000000000 ) ) ;
#75918 = ORIENTED_EDGE ( 'NONE', *, *, #33574, .T. ) ;
#75919 = VERTEX_POINT ( 'NONE', #132353 ) ;
#75920 = ORIENTED_EDGE ( 'NONE', *, *, #78909, .T. ) ;
#75921 = CARTESIAN_POINT ( 'NONE',  ( 118.0370968585647802, -3.054999999999998828, -5.291415217122919401 ) ) ;
#75922 = ORIENTED_EDGE ( 'NONE', *, *, #112390, .T. ) ;
#75923 = VECTOR ( 'NONE', #119231, 1000.000000000000227 ) ;
#75924 = FACE_OUTER_BOUND ( 'NONE', #98583, .T. ) ;
#75925 = AXIS2_PLACEMENT_3D ( 'NONE', #103148, #80709, #124904 ) ;
#75926 = EDGE_CURVE ( 'NONE', #109090, #1274, #121426, .T. ) ;
#75927 = CARTESIAN_POINT ( 'NONE',  ( -39.48921356237310221, -27.52281430457082934, 5.000000000000000000 ) ) ;
#75928 = ADVANCED_FACE ( 'NONE', ( #66360 ), #123612, .T. ) ;
#75929 = ORIENTED_EDGE ( 'NONE', *, *, #132523, .F. ) ;
#75930 = CARTESIAN_POINT ( 'NONE',  ( 0.000000000000000000, 0.000000000000000000, 5.000000000000000000 ) ) ;
#75931 = VERTEX_POINT ( 'NONE', #100411 ) ;
#75932 = EDGE_CURVE ( 'NONE', #24466, #8834, #110531, .T. ) ;
#75933 = CARTESIAN_POINT ( 'NONE',  ( 11.79123647476855297, -9.717572351234235426E-16, -7.934999999999990727 ) ) ;
#75934 = FILL_AREA_STYLE ('',( #107817 ) ) ;
#75935 = CARTESIAN_POINT ( 'NONE',  ( 19.49999999999987210, 18.05218569542898521, 5.000000000000000000 ) ) ;
#75936 = CARTESIAN_POINT ( 'NONE',  ( 14.29289321881336328, -3.740707523384241728, 5.000000000000000000 ) ) ;
#75937 = ORIENTED_EDGE ( 'NONE', *, *, #88675, .F. ) ;
#75938 = ORIENTED_EDGE ( 'NONE', *, *, #103968, .F. ) ;
#75939 = ORIENTED_EDGE ( 'NONE', *, *, #109675, .F. ) ;
#75940 = LINE ( 'NONE', #64351, #122833 ) ;
#75941 = CARTESIAN_POINT ( 'NONE',  ( 12.71159235450332048, 3.061616997868378211E-16, -2.500000000000001332 ) ) ;
#75942 = ADVANCED_FACE ( 'NONE', ( #67067 ), #57635, .T. ) ;
#75943 = LINE ( 'NONE', #9199, #95891 ) ;
#75944 = DIRECTION ( 'NONE',  ( 0.7071067811865487940, -0.7071067811865463515, 0.000000000000000000 ) ) ;
#75945 = CARTESIAN_POINT ( 'NONE',  ( 8.700255128608413102, -27.71228299555199825, 4.000000000000000000 ) ) ;
#75946 = LINE ( 'NONE', #119417, #99316 ) ;
#75947 = CARTESIAN_POINT ( 'NONE',  ( 32.66709685856476852, -3.055000000000000160, -5.291415217122921177 ) ) ;
#75948 = LINE ( 'NONE', #78102, #35164 ) ;
#75949 = PLANE ( 'NONE',  #139218 ) ;
#75950 = VERTEX_POINT ( 'NONE', #67816 ) ;
#75951 = LINE ( 'NONE', #119422, #90305 ) ;
#75952 = EDGE_CURVE ( 'NONE', #106121, #132680, #112006, .T. ) ;
#75953 = ORIENTED_EDGE ( 'NONE', *, *, #13172, .F. ) ;
#75954 = DIRECTION ( 'NONE',  ( 0.7071067811865487940, -0.7071067811865463515, 0.000000000000000000 ) ) ;
#75955 = ORIENTED_EDGE ( 'NONE', *, *, #79741, .T. ) ;
#75956 = VECTOR ( 'NONE', #129241, 1000.000000000000114 ) ;
#75957 = CARTESIAN_POINT ( 'NONE',  ( 16.82816939922341959, 9.759292476615618384, 4.000000000000000000 ) ) ;
#75959 = VERTEX_POINT ( 'NONE', #11944 ) ;
#75958 = DIRECTION ( 'NONE',  ( 0.7071067811865487940, -0.7071067811865463515, 0.000000000000000000 ) ) ;
#75960 = DIRECTION ( 'NONE',  ( -0.3543493200069162685, -0.000000000000000000, -0.9351131265310288487 ) ) ;
#75961 = EDGE_CURVE ( 'NONE', #4187, #28997, #90227, .T. ) ;
#75962 = ORIENTED_EDGE ( 'NONE', *, *, #107835, .F. ) ;
#75964 = VECTOR ( 'NONE', #53045, 1000.000000000000000 ) ;
#75963 = PLANE ( 'NONE',  #55461 ) ;
#75965 = ORIENTED_EDGE ( 'NONE', *, *, #118737, .T. ) ;
#75966 = PLANE ( 'NONE',  #90620 ) ;
#75967 = ORIENTED_EDGE ( 'NONE', *, *, #41839, .T. ) ;
#75968 = CARTESIAN_POINT ( 'NONE',  ( 27.99999999999999645, -49.14999999999999147, -49.92499999999968452 ) ) ;
#75969 = ADVANCED_FACE ( 'NONE', ( #59768 ), #106067, .T. ) ;
#75970 = CARTESIAN_POINT ( 'NONE',  ( 115.8708603837962414, 6.884901960086289741, -3.974999999999993427 ) ) ;
#75971 = CARTESIAN_POINT ( 'NONE',  ( 49.51669371712954870, 7.950000000000000178, -2.130196079827421318 ) ) ;
#75972 =( BOUNDED_CURVE ( )  B_SPLINE_CURVE ( 3, ( #125014, #82256, #70676, #15502 ),
 .UNSPECIFIED., .F., .T. ) 
 B_SPLINE_CURVE_WITH_KNOTS ( ( 4, 4 ),
 ( 5.143245962375964986, 6.645403452391246191 ),
 .UNSPECIFIED. ) 
 CURVE ( )  GEOMETRIC_REPRESENTATION_ITEM ( )  RATIONAL_B_SPLINE_CURVE ( ( 1.000000000000000000, 0.8206354192515240564, 0.8206354192515240564, 1.000000000000000000 ) ) 
 REPRESENTATION_ITEM ( '' )  );
#75973 = CARTESIAN_POINT ( 'NONE',  ( -8.999999999999952038, -22.22500000000000142, 4.412002311789987807 ) ) ;
#75974 = CARTESIAN_POINT ( 'NONE',  ( 18.01107201284014536, 4.333342374871280669E-31, 2.500000000000000444 ) ) ;
#75975 = DIRECTION ( 'NONE',  ( 3.115803279706882722E-16, -1.000000000000000000, 0.000000000000000000 ) ) ;
#75976 = LINE ( 'NONE', #120890, #20691 ) ;
#75977 = CARTESIAN_POINT ( 'NONE',  ( 5.687500000000000000, 4.461849672132297329, -4.461849672132302658 ) ) ;
#75978 = CARTESIAN_POINT ( 'NONE',  ( 17.77040314143522082, -7.934999999999988951, 2.126176841940957907 ) ) ;
#75979 = AXIS2_PLACEMENT_3D ( 'NONE', #126179, #81265, #125468 ) ;
#75980 = FILL_AREA_STYLE_COLOUR ( '', #104494 ) ;
#75981 = CARTESIAN_POINT ( 'NONE',  ( -31.49999999999977973, 14.14708470758588099, -0.5283514160165838636 ) ) ;
#75982 = VERTEX_POINT ( 'NONE', #6033 ) ;
#75984 = VERTEX_POINT ( 'NONE', #61233 ) ;
#75983 = STYLED_ITEM ( 'NONE', ( #83832 ), #37829 ) ;
#75985 = DIRECTION ( 'NONE',  ( 1.000000000000000000, 0.000000000000000000, 0.000000000000000000 ) ) ;
#75986 = ORIENTED_EDGE ( 'NONE', *, *, #72625, .F. ) ;
#75987 = PRODUCT_DEFINITION_SHAPE ( 'NONE', 'NONE',  #143563 ) ;
#75988 = ADVANCED_FACE ( 'NONE', ( #127885 ), #16959, .F. ) ;
#75989 = CARTESIAN_POINT ( 'NONE',  ( 5.510786437626906675, -27.52281430457051314, 5.000000000000000000 ) ) ;
#75990 = LINE ( 'NONE', #20873, #143501 ) ;
#75991 = CARTESIAN_POINT ( 'NONE',  ( 129.2310344399266739, -47.51495700085919083, -36.79359617903136837 ) ) ;
#75992 = VERTEX_POINT ( 'NONE', #27106 ) ;
#75993 = DIRECTION ( 'NONE',  ( -0.000000000000000000, -0.000000000000000000, 1.000000000000000000 ) ) ;
#75994 = CARTESIAN_POINT ( 'NONE',  ( -38.99451991528749062, 28.92564299267965211, 4.000000000000000000 ) ) ;
#75995 = DIRECTION ( 'NONE',  ( 0.7071067811865487940, 0.7071067811865463515, 0.000000000000000000 ) ) ;
#75996 = EDGE_CURVE ( 'NONE', #55245, #96439, #126416, .T. ) ;
#75997 = DIRECTION ( 'NONE',  ( -1.000000000000000000, -0.000000000000000000, -0.000000000000000000 ) ) ;
#75999 = ORIENTED_EDGE ( 'NONE', *, *, #131812, .F. ) ;
#75998 = DIRECTION ( 'NONE',  ( 0.7071067811865487940, 0.7071067811865463515, 0.000000000000000000 ) ) ;
#76000 = FACE_OUTER_BOUND ( 'NONE', #57069, .T. ) ;
#76001 = CARTESIAN_POINT ( 'NONE',  ( 70.12500000000000000, -7.950000000000000178, -4.867971026610729436E-16 ) ) ;
#76002 = CARTESIAN_POINT ( 'NONE',  ( 28.00000000000002487, -49.14999999999999147, -34.92499999999976978 ) ) ;
#76003 = DIRECTION ( 'NONE',  ( 0.7071067811865487940, 0.7071067811865463515, 0.000000000000000000 ) ) ;
#76004 = CARTESIAN_POINT ( 'NONE',  ( 34.45011844616451668, -7.483719188362419672, 5.000000000000000888 ) ) ;
#76005 = EDGE_LOOP ( 'NONE', ( #107298, #81669, #116827, #93895 ) ) ;
#76006 = ORIENTED_EDGE ( 'NONE', *, *, #81179, .T. ) ;
#76007 = ORIENTED_EDGE ( 'NONE', *, *, #66793, .F. ) ;
#76008 = CARTESIAN_POINT ( 'NONE',  ( 93.33376352523144703, 6.110000000000001208, 1.122388791418549305E-15 ) ) ;
#76009 =( GEOMETRIC_REPRESENTATION_CONTEXT ( 3 ) GLOBAL_UNCERTAINTY_ASSIGNED_CONTEXT ( ( #102567 ) ) GLOBAL_UNIT_ASSIGNED_CONTEXT ( ( #21150, #41467, #108844 ) ) REPRESENTATION_CONTEXT ( 'NONE', 'WORKASPACE' ) );
#76010 = ORIENTED_EDGE ( 'NONE', *, *, #1846, .F. ) ;
#76011 = CARTESIAN_POINT ( 'NONE',  ( 15.48921356237309510, -27.52281430457066236, 5.000000000000000000 ) ) ;
#76012 = ADVANCED_FACE ( 'NONE', ( #81535 ), #4580, .T. ) ;
#76013 = FACE_OUTER_BOUND ( 'NONE', #88207, .T. ) ;
#76014 = ORIENTED_EDGE ( 'NONE', *, *, #49898, .F. ) ;
#76015 = DIRECTION ( 'NONE',  ( 0.7071067811865487940, 0.7071067811865463515, -0.000000000000000000 ) ) ;
#76016 = CARTESIAN_POINT ( 'NONE',  ( 26.99999999999980815, 2.966399257802232459, 5.000000000000000000 ) ) ;
#76017 = CARTESIAN_POINT ( 'NONE',  ( 97.47459685856478018, 1.637169565754164058, -6.109999999999996767 ) ) ;
#76018 = ORIENTED_EDGE ( 'NONE', *, *, #105693, .F. ) ;
#76019 = VECTOR ( 'NONE', #137098, 1000.000000000000000 ) ;
#76020 = EDGE_CURVE ( 'NONE', #88426, #128563, #28562, .T. ) ;
#76021 = CARTESIAN_POINT ( 'NONE',  ( -68.99451991528748351, 28.92564299267986172, 4.000000000000000000 ) ) ;
#76022 = DIRECTION ( 'NONE',  ( -0.7071067811865486830, -0.7071067811865464625, 0.000000000000000000 ) ) ;
#76023 = AXIS2_PLACEMENT_3D ( 'NONE', #40417, #26662, #16468 ) ;
#76024 = VECTOR ( 'NONE', #74705, 1000.000000000000000 ) ;
#76025 = ORIENTED_EDGE ( 'NONE', *, *, #106180, .F. ) ;
#76026 = ORIENTED_EDGE ( 'NONE', *, *, #34863, .F. ) ;
#76027 = VECTOR ( 'NONE', #4658, 999.9999999999998863 ) ;
#76028 = EDGE_CURVE ( 'NONE', #110799, #64904, #82241, .T. ) ;
#76029 = VERTEX_POINT ( 'NONE', #27828 ) ;
#76030 = LINE ( 'NONE', #42712, #141724 ) ;
#76031 = VECTOR ( 'NONE', #34391, 1000.000000000000000 ) ;
#76032 = EDGE_CURVE ( 'NONE', #79781, #3412, #93093, .T. ) ;
#76033 = DIRECTION ( 'NONE',  ( 0.3543493200069162685, -0.000000000000000000, -0.9351131265310288487 ) ) ;
#76034 = CARTESIAN_POINT ( 'NONE',  ( 16.40040314143521982, -7.934999999999988951, 2.126176841940957907 ) ) ;
#76035 = DIRECTION ( 'NONE',  ( -0.6830127018922181881, 0.6830127018922202975, -0.2588190451025214056 ) ) ;
#76036 = VECTOR ( 'NONE', #115990, 1000.000000000000000 ) ;
#76037 = AXIS2_PLACEMENT_3D ( 'NONE', #136862, #81808, #38273 ) ;
#76038 = PLANE ( 'NONE',  #75729 ) ;
#76039 =( BOUNDED_CURVE ( )  B_SPLINE_CURVE ( 3, ( #79074, #15172, #80480, #25350 ),
 .UNSPECIFIED., .F., .T. ) 
 B_SPLINE_CURVE_WITH_KNOTS ( ( 4, 4 ),
 ( 1.208578181583240374, 1.359146454359457135 ),
 .UNSPECIFIED. ) 
 CURVE ( )  GEOMETRIC_REPRESENTATION_ITEM ( )  RATIONAL_B_SPLINE_CURVE ( ( 1.000000000000000000, 0.9981116584018949744, 0.9981116584018949744, 1.000000000000000000 ) ) 
 REPRESENTATION_ITEM ( '' )  );
#76040 = DIRECTION ( 'NONE',  ( 0.7071067811865487940, 0.7071067811865463515, 0.000000000000000000 ) ) ;
#76041 = ORIENTED_EDGE ( 'NONE', *, *, #4508, .T. ) ;
#76043 = EDGE_LOOP ( 'NONE', ( #142051, #118071, #120271, #62642 ) ) ;
#76042 = ADVANCED_FACE ( 'NONE', ( #48165 ), #62656, .T. ) ;
#76044 = PLANE ( 'NONE',  #3953 ) ;
#76045 = VERTEX_POINT ( 'NONE', #105377 ) ;
#76046 = ORIENTED_EDGE ( 'NONE', *, *, #61589, .F. ) ;
#76047 = VECTOR ( 'NONE', #41518, 1000.000000000000227 ) ;
#76048 = ADVANCED_FACE ( 'NONE', ( #6739 ), #116269, .F. ) ;
#76049 = VECTOR ( 'NONE', #107157, 1000.000000000000227 ) ;
#76050 = CARTESIAN_POINT ( 'NONE',  ( 15.06442625288295822, 7.619305877646135094, 4.652854425660932769 ) ) ;
#76051 = ORIENTED_EDGE ( 'NONE', *, *, #42391, .F. ) ;
#76052 = CARTESIAN_POINT ( 'NONE',  ( -4.171830600776445408, -8.240707523384198652, 4.000000000000000000 ) ) ;
#76053 = DIRECTION ( 'NONE',  ( -1.000000000000000000, -0.000000000000000000, -0.000000000000000000 ) ) ;
#76054 = DIRECTION ( 'NONE',  ( -0.000000000000000000, 0.3543493200069153248, 0.9351131265310292928 ) ) ;
#76055 = CARTESIAN_POINT ( 'NONE',  ( 36.18398860626899705, 28.73617430169812437, 5.000000000000000000 ) ) ;
#76056 = EDGE_CURVE ( 'NONE', #45188, #84616, #134902, .T. ) ;
#76057 = CARTESIAN_POINT ( 'NONE',  ( 0.000000000000000000, 0.000000000000000000, 5.000000000000000000 ) ) ;
#76058 = ORIENTED_EDGE ( 'NONE', *, *, #20812, .F. ) ;
#76059 = AXIS2_PLACEMENT_3D ( 'NONE', #132317, #98239, #56902 ) ;
#76060 = SURFACE_STYLE_USAGE ( .BOTH. , #107930 ) ;
#76061 = VECTOR ( 'NONE', #141327, 1000.000000000000000 ) ;
#76062 = ORIENTED_EDGE ( 'NONE', *, *, #101240, .F. ) ;
#76063 = FACE_OUTER_BOUND ( 'NONE', #985, .T. ) ;
#76064 = EDGE_LOOP ( 'NONE', ( #41323, #93483, #116505, #123319 ) ) ;
#76065 = DIRECTION ( 'NONE',  ( -0.7071067811865486830, -0.7071067811865464625, 0.000000000000000000 ) ) ;
#76066 = ORIENTED_EDGE ( 'NONE', *, *, #3855, .T. ) ;
#76067 = DIRECTION ( 'NONE',  ( 0.7071067811865487940, 0.7071067811865463515, -0.000000000000000000 ) ) ;
#76068 = EDGE_LOOP ( 'NONE', ( #5763, #84818, #87095, #58660 ) ) ;
#76069 = ORIENTED_EDGE ( 'NONE', *, *, #48435, .F. ) ;
#76070 = ORIENTED_EDGE ( 'NONE', *, *, #191, .F. ) ;
#76071 = LINE ( 'NONE', #123162, #30407 ) ;
#76072 = LINE ( 'NONE', #31853, #133195 ) ;
#76073 = DIRECTION ( 'NONE',  ( 0.7071067811865487940, 0.7071067811865463515, 0.000000000000000000 ) ) ;
#76074 = DIRECTION ( 'NONE',  ( 0.6830127018922181881, 0.6830127018922202975, -0.2588190451025214056 ) ) ;
#76075 = CARTESIAN_POINT ( 'NONE',  ( 126.2920968585647614, -5.291415217122921177, 3.054999999999999272 ) ) ;
#76076 = DIRECTION ( 'NONE',  ( -0.7071067811865486830, 0.7071067811865464625, 0.000000000000000000 ) ) ;
#76077 = EDGE_CURVE ( 'NONE', #139208, #82074, #83674, .T. ) ;
#76078 = DIRECTION ( 'NONE',  ( 0.6830127018922181881, 0.6830127018922202975, -0.2588190451025214056 ) ) ;
#76079 = DIRECTION ( 'NONE',  ( -0.3543493200069162685, -0.000000000000000000, -0.9351131265310288487 ) ) ;
#76080 = AXIS2_PLACEMENT_3D ( 'NONE', #49750, #73619, #74344 ) ;
#76082 = ADVANCED_FACE ( 'NONE', ( #49624 ), #93799, .F. ) ;
#76081 = AXIS2_PLACEMENT_3D ( 'NONE', #126402, #17626, #61899 ) ;
#76083 = EDGE_CURVE ( 'NONE', #141976, #56643, #113532, .T. ) ;
#76084 = DIRECTION ( 'NONE',  ( -0.6830127018922181881, 0.6830127018922202975, -0.2588190451025214056 ) ) ;
#76085 = PLANE ( 'NONE',  #13490 ) ;
#76086 = DIRECTION ( 'NONE',  ( 0.6830127018922180770, -0.6830127018922204085, -0.2588190451025213501 ) ) ;
#76087 = ORIENTED_EDGE ( 'NONE', *, *, #23147, .F. ) ;
#76088 = ORIENTED_EDGE ( 'NONE', *, *, #21110, .T. ) ;
#76089 = EDGE_LOOP ( 'NONE', ( #66004, #12255, #89620, #10419 ) ) ;
#76090 = CARTESIAN_POINT ( 'NONE',  ( -27.48921356237309155, -27.52281430457074762, 5.000000000000000000 ) ) ;
#76091 = ORIENTED_EDGE ( 'NONE', *, *, #47365, .T. ) ;
#76092 = ADVANCED_FACE ( 'NONE', ( #36561 ), #80804, .F. ) ;
#76093 = VERTEX_POINT ( 'NONE', #37287 ) ;
#76094 = CARTESIAN_POINT ( 'NONE',  ( 0.000000000000000000, 0.000000000000000000, 5.000000000000000000 ) ) ;
#76095 = CARTESIAN_POINT ( 'NONE',  ( 21.76000000000000156, 9.521314400968980422E-16, 0.000000000000000000 ) ) ;
#76096 = EDGE_CURVE ( 'NONE', #20803, #19753, #38712, .T. ) ;
#76097 = EDGE_CURVE ( 'NONE', #47758, #93680, #53897, .T. ) ;
#76098 = CARTESIAN_POINT ( 'NONE',  ( 26.99999999999981171, -13.44781430457069149, 5.000000000000000000 ) ) ;
#76099 = ORIENTED_EDGE ( 'NONE', *, *, #51157, .F. ) ;
#76100 = LINE ( 'NONE', #99241, #132085 ) ;
#76101 = ORIENTED_EDGE ( 'NONE', *, *, #13323, .T. ) ;
#76102 = LINE ( 'NONE', #20988, #56170 ) ;
#76103 = DIRECTION ( 'NONE',  ( -0.000000000000000000, -0.3543493200069152693, 0.9351131265310292928 ) ) ;
#76104 = EDGE_CURVE ( 'NONE', #34254, #56788, #6102, .T. ) ;
#76105 = CARTESIAN_POINT ( 'NONE',  ( 21.06706980810188412, 2.126176841940952134, -7.934999999999993392 ) ) ;
#76106 = ORIENTED_EDGE ( 'NONE', *, *, #4311, .F. ) ;
#76107 = CARTESIAN_POINT ( 'NONE',  ( 91.78709685856478018, 3.054999999999997939, 5.291415217122920289 ) ) ;
#76108 = ADVANCED_FACE ( 'NONE', ( #119803 ), #119115, .F. ) ;
#76109 = LINE ( 'NONE', #31887, #43623 ) ;
#76110 = CARTESIAN_POINT ( 'NONE',  ( 52.40027281130056735, -49.14999999999999147, -40.57187971032006857 ) ) ;
#76111 = PLANE ( 'NONE',  #2496 ) ;
#76112 = EDGE_LOOP ( 'NONE', ( #137082, #52109, #8465, #100442 ) ) ;
#76113 = DIRECTION ( 'NONE',  ( -0.000000000000000000, 0.3543493200069153248, 0.9351131265310292928 ) ) ;
#76114 = ORIENTED_EDGE ( 'NONE', *, *, #22794, .F. ) ;
#76115 = CARTESIAN_POINT ( 'NONE',  ( -62.99451991528749772, 28.92564299267982264, 4.000000000000000000 ) ) ;
#76116 = VERTEX_POINT ( 'NONE', #42302 ) ;
#76117 = CARTESIAN_POINT ( 'NONE',  ( -6.706123077391903387, 22.22500000000000142, 4.000000000000000000 ) ) ;
#76118 = CARTESIAN_POINT ( 'NONE',  ( 34.92499999999998295, -1.199905483972814713, 4.759050581649325373 ) ) ;
#76119 = EDGE_CURVE ( 'NONE', #111653, #37807, #20494, .T. ) ;
#76120 = CARTESIAN_POINT ( 'NONE',  ( 34.49999999999976552, 18.05432934483075513, 4.994342998332162331 ) ) ;
#76121 = CARTESIAN_POINT ( 'NONE',  ( 5.148183550381419948, 17.25929247661554200, 8.802941693769213316 ) ) ;
#76122 = EDGE_LOOP ( 'NONE', ( #16439, #89385, #133672, #123197 ) ) ;
#76123 = DIRECTION ( 'NONE',  ( 0.7071067811865487940, -0.7071067811865463515, 0.000000000000000000 ) ) ;
#76124 = CARTESIAN_POINT ( 'NONE',  ( 10.82816939922345512, 3.759292476615674783, 4.000000000000000000 ) ) ;
#76125 = DIRECTION ( 'NONE',  ( -0.6830127018922180770, -0.6830127018922204085, -0.2588190451025213501 ) ) ;
#76126 = ORIENTED_EDGE ( 'NONE', *, *, #116159, .F. ) ;
#76127 = DIRECTION ( 'NONE',  ( 1.369518533665900312E-16, -1.000000000000000000, 0.000000000000000000 ) ) ;
#76128 = EDGE_CURVE ( 'NONE', #133461, #7223, #11624, .T. ) ;
#76129 = VECTOR ( 'NONE', #130831, 1000.000000000000000 ) ;
#76130 = VECTOR ( 'NONE', #56369, 1000.000000000000000 ) ;
#76131 = AXIS2_PLACEMENT_3D ( 'NONE', #27714, #116153, #118276 ) ;
#76132 = CARTESIAN_POINT ( 'NONE',  ( -2.999999999999975131, -10.44781430457071991, 5.000000000000000000 ) ) ;
#76133 = EDGE_LOOP ( 'NONE', ( #8585, #9846, #38463, #105079 ) ) ;
#76134 = VECTOR ( 'NONE', #39885, 1000.000000000000000 ) ;
#76136 = ORIENTED_EDGE ( 'NONE', *, *, #129750, .T. ) ;
#76135 = LINE ( 'NONE', #120301, #67224 ) ;
#76137 = EDGE_LOOP ( 'NONE', ( #73016, #133353, #6684, #48608, #110095, #83035 ) ) ;
#76138 = CARTESIAN_POINT ( 'NONE',  ( -26.91685193227052864, 21.75929247661549581, 7.311836541447990001 ) ) ;
#76140 = EDGE_CURVE ( 'NONE', #42229, #31468, #65039, .T. ) ;
#76139 = DIRECTION ( 'NONE',  ( 0.7071067811865487940, -0.7071067811865463515, 0.000000000000000000 ) ) ;
#76141 =( GEOMETRIC_REPRESENTATION_CONTEXT ( 3 ) GLOBAL_UNCERTAINTY_ASSIGNED_CONTEXT ( ( #78095 ) ) GLOBAL_UNIT_ASSIGNED_CONTEXT ( ( #105656, #50594, #136886 ) ) REPRESENTATION_CONTEXT ( 'NONE', 'WORKASPACE' ) );
#76142 = VERTEX_POINT ( 'NONE', #43006 ) ;
#76143 = CARTESIAN_POINT ( 'NONE',  ( 45.18398860626900415, 28.73617430169818832, 5.000000000000000000 ) ) ;
#76144 = VECTOR ( 'NONE', #87893, 1000.000000000000000 ) ;
#76145 = LINE ( 'NONE', #52927, #45232 ) ;
#76146 = ADVANCED_FACE ( 'NONE', ( #9619 ), #52424, .F. ) ;
#76147 = LINE ( 'NONE', #109481, #104064 ) ;
#76148 = CARTESIAN_POINT ( 'NONE',  ( 0.1600000000000010858, -4.972023319592707047, -6.193256324377186317 ) ) ;
#76149 = CARTESIAN_POINT ( 'NONE',  ( -33.18398860626899705, 28.73617430169810305, 5.000000000000000000 ) ) ;
#76150 = DIRECTION ( 'NONE',  ( 0.3543493200069162685, -0.000000000000000000, -0.9351131265310288487 ) ) ;
#76151 = PRESENTATION_STYLE_ASSIGNMENT (( #31928 ) ) ;
#76152 = DIRECTION ( 'NONE',  ( 0.3543493200069162685, -0.000000000000000000, -0.9351131265310288487 ) ) ;
#76153 = CARTESIAN_POINT ( 'NONE',  ( -34.92500000000001137, 22.22500000000000142, 4.500000000000000888 ) ) ;
#76154 = DIRECTION ( 'NONE',  ( 0.7071067811865486830, -0.7071067811865464625, -0.000000000000000000 ) ) ;
#76155 = VECTOR ( 'NONE', #19816, 1000.000000000000000 ) ;
#76156 = ADVANCED_FACE ( 'NONE', ( #95936 ), #98091, .T. ) ;
#76157 = CARTESIAN_POINT ( 'NONE',  ( 24.41159235450331977, -3.851859888774471706E-31, 2.500000000000001332 ) ) ;
#76158 = CARTESIAN_POINT ( 'NONE',  ( -7.140000000000001457, -35.62922597241578160, -11.84864515520818706 ) ) ;
#76159 = VERTEX_POINT ( 'NONE', #141598 ) ;
#76160 = EDGE_LOOP ( 'NONE', ( #38548, #49740, #109969, #20041 ) ) ;
#76161 = ORIENTED_EDGE ( 'NONE', *, *, #98575, .T. ) ;
#76162 = CARTESIAN_POINT ( 'NONE',  ( 97.68750000000000000, -5.819803920172573086, 5.819803920172572198 ) ) ;
#76163 = VECTOR ( 'NONE', #53325, 1000.000000000000000 ) ;
#76164 = ORIENTED_EDGE ( 'NONE', *, *, #121954, .F. ) ;
#76165 = VERTEX_POINT ( 'NONE', #40174 ) ;
#76166 = ORIENTED_EDGE ( 'NONE', *, *, #7270, .F. ) ;
#76167 = FACE_OUTER_BOUND ( 'NONE', #13726, .T. ) ;
#76168 = VECTOR ( 'NONE', #82067, 1000.000000000000000 ) ;
#76169 = CARTESIAN_POINT ( 'NONE',  ( 34.91764015037181679, 21.81495039010401982, 4.089230673112391301 ) ) ;
#76170 = VERTEX_POINT ( 'NONE', #139491 ) ;
#76171 = VECTOR ( 'NONE', #16420, 1000.000000000000000 ) ;
#76172 = DIRECTION ( 'NONE',  ( -0.000000000000000000, -1.000000000000000000, -0.000000000000000000 ) ) ;
#76173 = VECTOR ( 'NONE', #69381, 1000.000000000000000 ) ;
#76174 = DIRECTION ( 'NONE',  ( 0.6830127018922181881, 0.6830127018922202975, -0.2588190451025214056 ) ) ;
#76175 = CIRCLE ( 'NONE', #36825, 2.500000000000000888 ) ;
#76176 = DIRECTION ( 'NONE',  ( -1.000000000000000000, -1.224606353822377258E-16, -0.000000000000000000 ) ) ;
#76177 = DIRECTION ( 'NONE',  ( -0.6830127018922180770, -0.6830127018922204085, -0.2588190451025213501 ) ) ;
#76178 = ORIENTED_EDGE ( 'NONE', *, *, #40989, .T. ) ;
#76179 = DIRECTION ( 'NONE',  ( 0.7071067811865487940, -0.7071067811865463515, 0.000000000000000000 ) ) ;
#76180 = CARTESIAN_POINT ( 'NONE',  ( -21.15612307739224462, -22.22499999999999432, 4.000000000000000000 ) ) ;
#76181 = CARTESIAN_POINT ( 'NONE',  ( 16.49999999999989697, 10.46639925780215918, 5.000000000000000000 ) ) ;
#76182 = MECHANICAL_DESIGN_GEOMETRIC_PRESENTATION_REPRESENTATION (  '', ( #140934 ), #101614 ) ;
#76183 = CARTESIAN_POINT ( 'NONE',  ( 27.99999999999999645, 9.521314400968980422E-16, 0.000000000000000000 ) ) ;
#76184 = FACE_OUTER_BOUND ( 'NONE', #8072, .T. ) ;
#76185 = DIRECTION ( 'NONE',  ( 0.7071067811865486830, -0.7071067811865464625, -0.000000000000000000 ) ) ;
#76186 = AXIS2_PLACEMENT_3D ( 'NONE', #115240, #139211, #128327 ) ;
#76187 = CARTESIAN_POINT ( 'NONE',  ( 29.39169371712956291, 2.130196079827421762, 7.950000000000001066 ) ) ;
#76188 = CARTESIAN_POINT ( 'NONE',  ( 19.04500000000000171, 3.130000000000007887, -23.88381690219165776 ) ) ;
#76189 = ORIENTED_EDGE ( 'NONE', *, *, #89045, .F. ) ;
#76190 = VERTEX_POINT ( 'NONE', #64037 ) ;
#76191 = CARTESIAN_POINT ( 'NONE',  ( 124.6879301918981042, 6.110000000000002984, -1.637169565754156730 ) ) ;
#76192 = ORIENTED_EDGE ( 'NONE', *, *, #31380, .T. ) ;
#76193 = CARTESIAN_POINT ( 'NONE',  ( 20.19999999999999929, -2.055000000000000160, 0.000000000000000000 ) ) ;
#76194 = FACE_OUTER_BOUND ( 'NONE', #134177, .T. ) ;
#76195 = DIRECTION ( 'NONE',  ( -0.7071067811865486830, 0.7071067811865464625, 0.000000000000000000 ) ) ;
#76196 = LINE ( 'NONE', #52284, #9870 ) ;
#76197 = CARTESIAN_POINT ( 'NONE',  ( 11.99999999999992184, -1.068876922607797209, 4.000000000000000000 ) ) ;
#76198 = CARTESIAN_POINT ( 'NONE',  ( 125.6204301918981088, 3.055000000000001936, -5.291415217122916737 ) ) ;
#76199 = VERTEX_POINT ( 'NONE', #108203 ) ;
#76200 = EDGE_LOOP ( 'NONE', ( #54711, #28462, #80538, #2304 ) ) ;
#76201 = DIRECTION ( 'NONE',  ( -0.7071067811865486830, -0.7071067811865464625, 0.000000000000000000 ) ) ;
#76202 = CARTESIAN_POINT ( 'NONE',  ( 0.000000000000000000, 0.000000000000000000, 5.000000000000000000 ) ) ;
#76203 = EDGE_CURVE ( 'NONE', #51263, #98176, #8863, .T. ) ;
#76204 = CARTESIAN_POINT ( 'NONE',  ( 29.24139925780183091, 21.72500000000000853, 5.000000000000000000 ) ) ;
#76205 = ORIENTED_EDGE ( 'NONE', *, *, #139798, .F. ) ;
#76206 = CARTESIAN_POINT ( 'NONE',  ( 42.58376352523143993, -6.110000000000001208, -3.741295971395164515E-16 ) ) ;
#76207 = ADVANCED_FACE ( 'NONE', ( #86512 ), #142325, .F. ) ;
#76208 = ORIENTED_EDGE ( 'NONE', *, *, #2673, .F. ) ;
#76209 = CARTESIAN_POINT ( 'NONE',  ( -11.99451991528749417, 28.92564299267946382, 4.000000000000000000 ) ) ;
#76210 = LINE ( 'NONE', #53004, #113289 ) ;
#76211 = CARTESIAN_POINT ( 'NONE',  ( 10.49999999999993250, -11.94781430457070392, 5.000000000000000000 ) ) ;
#76212 = DIRECTION ( 'NONE',  ( 0.000000000000000000, -1.000000000000000000, 0.000000000000000000 ) ) ;
#76213 = EDGE_CURVE ( 'NONE', #69257, #98086, #51744, .T. ) ;
#76214 = ADVANCED_FACE ( 'NONE', ( #29954 ), #79238, .F. ) ;
#76215 = CARTESIAN_POINT ( 'NONE',  ( 42.05793019189811588, 6.110000000000000320, -1.637169565754156064 ) ) ;
#76216 = ORIENTED_EDGE ( 'NONE', *, *, #136318, .T. ) ;
#76217 = EDGE_CURVE ( 'NONE', #116804, #101800, #13187, .T. ) ;
#76218 = DIRECTION ( 'NONE',  ( 0.7071067811865486830, -0.7071067811865464625, -0.000000000000000000 ) ) ;
#76219 = ORIENTED_EDGE ( 'NONE', *, *, #29357, .F. ) ;
#76220 = ORIENTED_EDGE ( 'NONE', *, *, #141162, .F. ) ;
#76221 = ORIENTED_EDGE ( 'NONE', *, *, #22610, .F. ) ;
#76222 = EDGE_CURVE ( 'NONE', #26483, #56060, #24798, .T. ) ;
#76223 = LINE ( 'NONE', #142212, #103063 ) ;
#76224 = DIRECTION ( 'NONE',  ( -0.6830127018922181881, 0.6830127018922202975, -0.2588190451025214056 ) ) ;
#76225 = UNCERTAINTY_MEASURE_WITH_UNIT (LENGTH_MEASURE( 1.000000000000000082E-05 ), #3279, 'distance_accuracy_value', 'NONE');
#76226 = ORIENTED_EDGE ( 'NONE', *, *, #111769, .F. ) ;
#76227 = CARTESIAN_POINT ( 'NONE',  ( -34.49999999999976552, 6.054329344830883031, 4.994342998332166772 ) ) ;
#76228 = CARTESIAN_POINT ( 'NONE',  ( -5.999999999999951150, -6.033600742197678279, 5.000000000000000000 ) ) ;
#76229 = CARTESIAN_POINT ( 'NONE',  ( -12.70000000000000284, -40.42999999999999261, 19.06900128115121973 ) ) ;
#76231 = EDGE_CURVE ( 'NONE', #54018, #136335, #78483, .T. ) ;
#76230 = AXIS2_PLACEMENT_3D ( 'NONE', #53823, #130673, #97261 ) ;
#76232 = AXIS2_PLACEMENT_3D ( 'NONE', #13792, #79124, #34887 ) ;
#76233 = VECTOR ( 'NONE', #54810, 999.9999999999998863 ) ;
#76234 = DIRECTION ( 'NONE',  ( 0.7071067811865487940, -0.7071067811865463515, 0.000000000000000000 ) ) ;
#76235 = AXIS2_PLACEMENT_3D ( 'NONE', #118667, #7744, #107073 ) ;
#76236 = FACE_BOUND ( 'NONE', #58282, .T. ) ;
#76237 = ORIENTED_EDGE ( 'NONE', *, *, #119431, .F. ) ;
#76238 = DIRECTION ( 'NONE',  ( 0.6830127018922181881, 0.6830127018922202975, -0.2588190451025214056 ) ) ;
#76239 = CARTESIAN_POINT ( 'NONE',  ( -63.18398860626900415, 28.73617430169831621, 5.000000000000000000 ) ) ;
#76240 = CARTESIAN_POINT ( 'NONE',  ( 26.20666063542134339, 21.75929247661549581, 4.998822639870700968 ) ) ;
#76241 = ORIENTED_EDGE ( 'NONE', *, *, #124575, .F. ) ;
#76242 = LINE ( 'NONE', #13090, #122170 ) ;
#76243 = VERTEX_POINT ( 'NONE', #90800 ) ;
#76245 = ORIENTED_EDGE ( 'NONE', *, *, #121097, .F. ) ;
#76244 = EDGE_CURVE ( 'NONE', #107481, #23113, #134297, .T. ) ;
#76246 = VECTOR ( 'NONE', #8680, 1000.000000000000000 ) ;
#76247 = CARTESIAN_POINT ( 'NONE',  ( -32.99999999999977263, -13.97847968911263195, -0.1324546996127563547 ) ) ;
#76248 = VERTEX_POINT ( 'NONE', #1588 ) ;
#76249 = CARTESIAN_POINT ( 'NONE',  ( 51.82876352523144448, 0.000000000000000000, -6.109999999999998543 ) ) ;
#76250 = ORIENTED_EDGE ( 'NONE', *, *, #122522, .T. ) ;
#76251 = PLANE ( 'NONE',  #20968 ) ;
#76252 = DIRECTION ( 'NONE',  ( 0.7071067811865486830, -0.7071067811865464625, -0.000000000000000000 ) ) ;
#76253 = EDGE_CURVE ( 'NONE', #22057, #45954, #121253, .T. ) ;
#76254 = ORIENTED_EDGE ( 'NONE', *, *, #79132, .F. ) ;
#76255 = CARTESIAN_POINT ( 'NONE',  ( 151.4000000000000057, -16.48000000000005016, 0.000000000000000000 ) ) ;
#76256 = DIRECTION ( 'NONE',  ( -1.000000000000000000, -0.000000000000000000, -0.000000000000000000 ) ) ;
#76257 = AXIS2_PLACEMENT_3D ( 'NONE', #78500, #53918, #44469 ) ;
#76258 =( BOUNDED_CURVE ( )  B_SPLINE_CURVE ( 2, ( #134525, #66411, #34483, #54821, #99002, #143238, #78000, #43936, #110582, #11261, #114855, #4631, #82986 ),
 .UNSPECIFIED., .F., .F. ) 
 B_SPLINE_CURVE_WITH_KNOTS ( ( 3, 2, 2, 2, 2, 2, 3 ),
 ( 0.03607035673769710266, 0.03611111111111108690, 0.03888888888888748091, 0.04166666666666386798, 0.04444444444444026199, 0.04722222222221665600, 0.04999999999999305000 ),
 .UNSPECIFIED. ) 
 CURVE ( )  GEOMETRIC_REPRESENTATION_ITEM ( )  RATIONAL_B_SPLINE_CURVE ( ( 0.9990148257276658672, 0.9995000782242919879, 1.000000000000000000, 0.9659258262890683122, 1.000000000000000000, 0.9659258262890683122, 1.000000000000000000, 0.9659258262890683122, 1.000000000000000000, 0.9659258262890683122, 1.000000000000000000, 0.9659258262891535773, 0.9999999999999147349 ) ) 
 REPRESENTATION_ITEM ( '' )  );
#76259 = EDGE_CURVE ( 'NONE', #92905, #49830, #69611, .T. ) ;
#76260 = ADVANCED_FACE ( 'NONE', ( #100234 ), #885, .F. ) ;
#76261 = CARTESIAN_POINT ( 'NONE',  ( 116.5000000000000000, 0.000000000000000000, -7.950000000000000178 ) ) ;
#76262 = CARTESIAN_POINT ( 'NONE',  ( -34.92500000000002558, 18.66246187583879035, 4.000000000000000000 ) ) ;
#76263 = DIRECTION ( 'NONE',  ( 0.3543493200069162685, -0.000000000000000000, -0.9351131265310288487 ) ) ;
#76264 = DIRECTION ( 'NONE',  ( -0.7071067811865486830, 0.7071067811865464625, 0.000000000000000000 ) ) ;
#76265 = DIRECTION ( 'NONE',  ( -0.7071067811865486830, 0.7071067811865464625, 0.000000000000000000 ) ) ;
#76266 = VERTEX_POINT ( 'NONE', #89349 ) ;
#76267 = VERTEX_POINT ( 'NONE', #57462 ) ;
#76268 = ORIENTED_EDGE ( 'NONE', *, *, #75753, .F. ) ;
#76269 = AXIS2_PLACEMENT_3D ( 'NONE', #71385, #84419, #4616 ) ;
#76270 = PLANE ( 'NONE',  #116775 ) ;
#76271 = CARTESIAN_POINT ( 'NONE',  ( 75.29974487139158157, -27.71228299555258445, 4.000000000000000000 ) ) ;
#76272 = ORIENTED_EDGE ( 'NONE', *, *, #94898, .T. ) ;
#76274 = EDGE_CURVE ( 'NONE', #102939, #15705, #66187, .T. ) ;
#76273 = VECTOR ( 'NONE', #35886, 1000.000000000000000 ) ;
#76275 = AXIS2_PLACEMENT_3D ( 'NONE', #75437, #34082, #76888 ) ;
#76276 = ORIENTED_EDGE ( 'NONE', *, *, #68566, .T. ) ;
#76277 = PLANE ( 'NONE',  #39745 ) ;
#76278 = DIRECTION ( 'NONE',  ( -1.000000000000000000, -0.000000000000000000, -0.000000000000000000 ) ) ;
#76279 = EDGE_CURVE ( 'NONE', #131061, #63704, #22623, .T. ) ;
#76280 = VECTOR ( 'NONE', #23208, 1000.000000000000000 ) ;
#76281 = CARTESIAN_POINT ( 'NONE',  ( 24.56840764549667355, 9.139736423841732040E-16, 0.000000000000000000 ) ) ;
#76282 = VERTEX_POINT ( 'NONE', #56771 ) ;
#76283 = VECTOR ( 'NONE', #80984, 1000.000000000000000 ) ;
#76284 = CARTESIAN_POINT ( 'NONE',  ( -21.70701326429289324, -21.74070752338406010, 4.999753212805221558 ) ) ;
#76285 = AXIS2_PLACEMENT_3D ( 'NONE', #110299, #34204, #100872 ) ;
#76286 = DIRECTION ( 'NONE',  ( -1.000000000000000000, -1.224606353822377258E-16, -0.000000000000000000 ) ) ;
#76287 = CARTESIAN_POINT ( 'NONE',  ( 15.37956980810188767, 3.967499999999998916, 6.871911579029510442 ) ) ;
#76288 = DIRECTION ( 'NONE',  ( 0.7071067811865487940, 0.7071067811865463515, 0.000000000000000000 ) ) ;
#76289 = ORIENTED_EDGE ( 'NONE', *, *, #6680, .F. ) ;
#76290 = CARTESIAN_POINT ( 'NONE',  ( 120.3704301918981230, -3.055000000000001936, 5.291415217122918513 ) ) ;
#76291 = EDGE_CURVE ( 'NONE', #71113, #3366, #112528, .T. ) ;
#76292 = DIRECTION ( 'NONE',  ( 0.3543493200069162685, -0.000000000000000000, -0.9351131265310288487 ) ) ;
#76293 = FACE_OUTER_BOUND ( 'NONE', #34360, .T. ) ;
#76294 = STYLED_ITEM ( 'NONE', ( #71319 ), #20929 ) ;
#76296 = ORIENTED_EDGE ( 'NONE', *, *, #54153, .F. ) ;
#76295 = CARTESIAN_POINT ( 'NONE',  ( 30.18398860626900060, 28.73617430169808173, 5.000000000000000000 ) ) ;
#76297 = CARTESIAN_POINT ( 'NONE',  ( 66.28752705046289861, 0.000000000000000000, -7.949999999999998401 ) ) ;
#76298 = ORIENTED_EDGE ( 'NONE', *, *, #37641, .T. ) ;
#76299 = DIRECTION ( 'NONE',  ( 1.000000000000000000, 0.000000000000000000, 0.000000000000000000 ) ) ;
#76300 = ADVANCED_FACE ( 'NONE', ( #66890 ), #32855, .F. ) ;
#76301 = DIRECTION ( 'NONE',  ( -0.6830127018922180770, -0.6830127018922204085, -0.2588190451025213501 ) ) ;
#76302 = DIRECTION ( 'NONE',  ( -0.000000000000000000, -0.3543493200069152693, 0.9351131265310292928 ) ) ;
#76303 = EDGE_LOOP ( 'NONE', ( #34193, #86995, #2960, #102823 ) ) ;
#76304 = DIRECTION ( 'NONE',  ( 0.6830127018922181881, 0.6830127018922202975, -0.2588190451025214056 ) ) ;
#76305 = CARTESIAN_POINT ( 'NONE',  ( -19.93618820135885272, -3.270000000000008455, -36.39086428169088094 ) ) ;
#76306 = EDGE_LOOP ( 'NONE', ( #94329, #107635, #20226, #100605 ) ) ;
#76307 = DIRECTION ( 'NONE',  ( -0.6830127018922181881, 0.6830127018922202975, -0.2588190451025214056 ) ) ;
#76308 = CARTESIAN_POINT ( 'NONE',  ( 6.852250093007166143, 3.061616997868383634E-16, -2.500000000000000444 ) ) ;
#76309 = EDGE_LOOP ( 'NONE', ( #41093, #82134, #106007, #24076 ) ) ;
#76310 = CARTESIAN_POINT ( 'NONE',  ( 0.000000000000000000, -21.72500000000000142, 4.500000000000000888 ) ) ;
#76312 = ORIENTED_EDGE ( 'NONE', *, *, #45197, .T. ) ;
#76311 = FACE_OUTER_BOUND ( 'NONE', #52795, .T. ) ;
#76313 = ORIENTED_EDGE ( 'NONE', *, *, #86854, .F. ) ;
#76314 = CARTESIAN_POINT ( 'NONE',  ( 20.90156419391750475, 11.25929247661559884, 10.79108189686412089 ) ) ;
#76315 = PLANE ( 'NONE',  #78431 ) ;
#76316 = EDGE_LOOP ( 'NONE', ( #32923, #128973, #135487, #81878, #62850 ) ) ;
#76317 = LINE ( 'NONE', #120479, #48220 ) ;
#76318 = EDGE_CURVE ( 'NONE', #38372, #133141, #10342, .T. ) ;
#76319 = LINE ( 'NONE', #42986, #8914 ) ;
#76320 = CARTESIAN_POINT ( 'NONE',  ( -25.49999999999982947, 10.94296225409024537, -9.576120664313316766 ) ) ;
#76321 = EDGE_LOOP ( 'NONE', ( #54403, #35944, #10299, #79636, #80766, #50638, #137420 ) ) ;
#76322 = FACE_OUTER_BOUND ( 'NONE', #234, .T. ) ;
#76323 = CARTESIAN_POINT ( 'NONE',  ( 4.358242975411375397, 15.75929247661555799, 19.34181609438698857 ) ) ;
#76324 = LINE ( 'NONE', #132867, #77189 ) ;
#76325 =( NAMED_UNIT ( * ) SI_UNIT ( $, .STERADIAN. ) SOLID_ANGLE_UNIT ( ) );
#76326 = CARTESIAN_POINT ( 'NONE',  ( 40.30793019189810877, -6.109999999999999432, 1.637169565754158507 ) ) ;
#76327 = CARTESIAN_POINT ( 'NONE',  ( 23.63159235450331863, -2.500000000000000000, 3.061616997868384127E-16 ) ) ;
#76328 = ORIENTED_EDGE ( 'NONE', *, *, #21381, .T. ) ;
#76329 = ORIENTED_EDGE ( 'NONE', *, *, #52801, .F. ) ;
#76330 = LINE ( 'NONE', #57450, #55799 ) ;
#76331 = VERTEX_POINT ( 'NONE', #11034 ) ;
#76332 = ORIENTED_EDGE ( 'NONE', *, *, #130789, .F. ) ;
#76333 = DIRECTION ( 'NONE',  ( 0.7071067811865487940, 0.7071067811865463515, 0.000000000000000000 ) ) ;
#76334 = CARTESIAN_POINT ( 'NONE',  ( 9.591592354503321260, -2.500000000000000444, 3.061616997868384620E-16 ) ) ;
#76335 = AXIS2_PLACEMENT_3D ( 'NONE', #26871, #4337, #71121 ) ;
#76336 = CIRCLE ( 'NONE', #111062, 2.500000000000000444 ) ;
#76337 = VECTOR ( 'NONE', #74146, 1000.000000000000000 ) ;
#76338 = ORIENTED_EDGE ( 'NONE', *, *, #101258, .F. ) ;
#76339 = CARTESIAN_POINT ( 'NONE',  ( 128.8287635252314658, 0.000000000000000000, -6.109999999999998543 ) ) ;
#76340 = VECTOR ( 'NONE', #3133, 1000.000000000000000 ) ;
#76341 = DIRECTION ( 'NONE',  ( 0.7071067811865486830, -0.7071067811865464625, -0.000000000000000000 ) ) ;
#76342 = LINE ( 'NONE', #118392, #84720 ) ;
#76343 = ORIENTED_EDGE ( 'NONE', *, *, #59902, .F. ) ;
#76344 = CARTESIAN_POINT ( 'NONE',  ( -8.999999999999932498, 2.587461875839218273, 4.000000000000000000 ) ) ;
#76345 = CARTESIAN_POINT ( 'NONE',  ( 60.18398860626900415, 28.73617430169829490, 5.000000000000000000 ) ) ;
#76346 = CARTESIAN_POINT ( 'NONE',  ( -21.48921356237309155, -27.52281430457070499, 5.000000000000000000 ) ) ;
#76347 = VECTOR ( 'NONE', #110871, 1000.000000000000000 ) ;
#76348 = DIRECTION ( 'NONE',  ( -0.3543493200069162685, -0.000000000000000000, -0.9351131265310288487 ) ) ;
#76349 = PLANE ( 'NONE',  #75217 ) ;
#76350 = CARTESIAN_POINT ( 'NONE',  ( 31.49999999999977973, -19.91253812416055169, 4.000000000000000000 ) ) ;
#76351 = DIRECTION ( 'NONE',  ( -0.6830127018922180770, -0.6830127018922204085, -0.2588190451025213501 ) ) ;
#76352 = CARTESIAN_POINT ( 'NONE',  ( 56.66252705046289151, 7.949999999999998401, 1.460391307983218338E-15 ) ) ;
#76353 = DIRECTION ( 'NONE',  ( -0.7071067811865486830, -0.7071067811865464625, 0.000000000000000000 ) ) ;
#76354 = LINE ( 'NONE', #21248, #20666 ) ;
#76355 = AXIS2_PLACEMENT_3D ( 'NONE', #138350, #58708, #60088 ) ;
#76356 = ORIENTED_EDGE ( 'NONE', *, *, #2032, .T. ) ;
#76357 = EDGE_LOOP ( 'NONE', ( #78211, #26064, #7328, #111960, #125226 ) ) ;
#76358 = CARTESIAN_POINT ( 'NONE',  ( 58.02083333333331439, 7.949999999999999289, 2.130196079827431532 ) ) ;
#76359 = DIRECTION ( 'NONE',  ( -0.000000000000000000, 0.000000000000000000, 1.000000000000000000 ) ) ;
#76360 = FACE_OUTER_BOUND ( 'NONE', #122311, .T. ) ;
#76361 = CIRCLE ( 'NONE', #13809, 8.000000000000001776 ) ;
#76362 = DIRECTION ( 'NONE',  ( 0.7071067811865487940, 0.7071067811865463515, 0.000000000000000000 ) ) ;
#76363 = EDGE_LOOP ( 'NONE', ( #124556, #54380, #119225, #110935 ) ) ;
#76364 = CARTESIAN_POINT ( 'NONE',  ( -0.1743029876375435661, -1.312104359949140431, 3.997104869979374531 ) ) ;
#76365 = DIRECTION ( 'NONE',  ( -0.000000000000000000, 0.000000000000000000, 1.000000000000000000 ) ) ;
#76366 = CIRCLE ( 'NONE', #92472, 2.500000000000000444 ) ;
#76367 = CARTESIAN_POINT ( 'NONE',  ( 50.75043019189810423, 3.055000000000002824, -5.291415217122919401 ) ) ;
#76368 = VERTEX_POINT ( 'NONE', #124120 ) ;
#76369 = FILL_AREA_STYLE_COLOUR ( '', #119681 ) ;
#76370 = ORIENTED_EDGE ( 'NONE', *, *, #62660, .F. ) ;
#76371 = ORIENTED_EDGE ( 'NONE', *, *, #72231, .T. ) ;
#76372 = LINE ( 'NONE', #66921, #72467 ) ;
#76373 = VECTOR ( 'NONE', #67101, 1000.000000000000227 ) ;
#76374 = VECTOR ( 'NONE', #126953, 999.9999999999998863 ) ;
#76375 = FACE_OUTER_BOUND ( 'NONE', #34495, .T. ) ;
#76376 = VECTOR ( 'NONE', #120885, 999.9999999999998863 ) ;
#76377 = EDGE_CURVE ( 'NONE', #119974, #136740, #132889, .T. ) ;
#76378 = LINE ( 'NONE', #7518, #78740 ) ;
#76379 = ORIENTED_EDGE ( 'NONE', *, *, #49308, .F. ) ;
#76380 = CARTESIAN_POINT ( 'NONE',  ( 0.000000000000000000, 0.000000000000000000, 5.000000000000000000 ) ) ;
#76381 = DIRECTION ( 'NONE',  ( -0.7071067811865486830, -0.7071067811865464625, -0.000000000000000000 ) ) ;
#76382 = ADVANCED_FACE ( 'NONE', ( #69047 ), #67636, .F. ) ;
#76383 = ADVANCED_FACE ( 'NONE', ( #12490 ), #18626, .T. ) ;
#76385 = VERTEX_POINT ( 'NONE', #45872 ) ;
#76384 = FACE_OUTER_BOUND ( 'NONE', #99185, .T. ) ;
#76386 = VECTOR ( 'NONE', #14314, 1000.000000000000000 ) ;
#76387 = CARTESIAN_POINT ( 'NONE',  ( 83.41709685856477563, 3.054999999999998828, 5.291415217122922066 ) ) ;
#76388 = CARTESIAN_POINT ( 'NONE',  ( 69.48921356237309510, -27.52281430457103895, 5.000000000000000000 ) ) ;
#76389 = CARTESIAN_POINT ( 'NONE',  ( 17.22560490425083657, -2.499999999999996447, 0.000000000000000000 ) ) ;
#76390 = DIRECTION ( 'NONE',  ( -0.000000000000000000, -0.3543493200069152693, 0.9351131265310292928 ) ) ;
#76391 = VECTOR ( 'NONE', #108221, 1000.000000000000000 ) ;
#76392 = CARTESIAN_POINT ( 'NONE',  ( -11.29298673570688649, -21.74070752338406720, 4.999753212805217117 ) ) ;
#76393 = CARTESIAN_POINT ( 'NONE',  ( 29.99999999999978328, 11.58746187583914100, 4.000000000000000000 ) ) ;
#76394 = ADVANCED_FACE ( 'NONE', ( #38546 ), #39270, .F. ) ;
#76395 = ADVANCED_FACE ( 'NONE', ( #91507 ), #138576, .F. ) ;
#76396 = ORIENTED_EDGE ( 'NONE', *, *, #143472, .F. ) ;
#76397 = DIRECTION ( 'NONE',  ( -0.000000000000000000, 0.000000000000000000, 1.000000000000000000 ) ) ;
#76398 = CARTESIAN_POINT ( 'NONE',  ( 68.89126352523142316, -4.472830434245839371, -4.472830434245839371 ) ) ;
#76399 = CARTESIAN_POINT ( 'NONE',  ( -21.70710678118639336, 14.25929247661557575, 5.000000000000000000 ) ) ;
#76400 = EDGE_CURVE ( 'NONE', #78627, #27619, #113645, .T. ) ;
#76401 = DIRECTION ( 'NONE',  ( 0.7071067811865486830, -0.7071067811865464625, -0.000000000000000000 ) ) ;
#76402 = DIRECTION ( 'NONE',  ( 0.000000000000000000, 0.000000000000000000, -1.000000000000000000 ) ) ;
#76403 = VERTEX_POINT ( 'NONE', #37106 ) ;
#76404 = VERTEX_POINT ( 'NONE', #135718 ) ;
#76405 = VECTOR ( 'NONE', #2845, 999.9999999999998863 ) ;
#76406 = EDGE_CURVE ( 'NONE', #63781, #140124, #81360, .T. ) ;
#76407 = DIRECTION ( 'NONE',  ( 0.000000000000000000, 0.000000000000000000, 1.000000000000000000 ) ) ;
#76408 = CARTESIAN_POINT ( 'NONE',  ( 17.57538274164440040, -2.608983483842240325, 5.000000000000000000 ) ) ;
#76409 = ORIENTED_EDGE ( 'NONE', *, *, #117555, .F. ) ;
#76410 = ADVANCED_FACE ( 'NONE', ( #26245 ), #103088, .F. ) ;
#76411 = ORIENTED_EDGE ( 'NONE', *, *, #48661, .F. ) ;
#76412 = DIRECTION ( 'NONE',  ( -0.7071067811865487940, 0.7071067811865463515, 0.000000000000000000 ) ) ;
#76413 = ORIENTED_EDGE ( 'NONE', *, *, #43027, .T. ) ;
#76414 = LINE ( 'NONE', #77146, #5183 ) ;
#76415 = PLANE ( 'NONE',  #126618 ) ;
#76416 = VECTOR ( 'NONE', #5973, 999.9999999999998863 ) ;
#76417 = EDGE_CURVE ( 'NONE', #87140, #78214, #125132, .T. ) ;
#76418 = LINE ( 'NONE', #77833, #125298 ) ;
#76419 = FACE_BOUND ( 'NONE', #132549, .T. ) ;
#76420 = DIRECTION ( 'NONE',  ( -1.000000000000000000, 0.000000000000000000, 0.000000000000000000 ) ) ;
#76421 = CARTESIAN_POINT ( 'NONE',  ( 14.87852683662844022, -20.24070752338407431, 7.412974875817756271 ) ) ;
#76422 = DIRECTION ( 'NONE',  ( 0.3543493200069162685, -0.000000000000000000, -0.9351131265310288487 ) ) ;
#76424 = ORIENTED_EDGE ( 'NONE', *, *, #69830, .T. ) ;
#76423 = CARTESIAN_POINT ( 'NONE',  ( 52.28752705046288440, 0.000000000000000000, -7.949999999999998401 ) ) ;
#76425 = EDGE_CURVE ( 'NONE', #75431, #53287, #70509, .T. ) ;
#76426 = FACE_OUTER_BOUND ( 'NONE', #95916, .T. ) ;
#76427 = ORIENTED_EDGE ( 'NONE', *, *, #48773, .T. ) ;
#76428 = ORIENTED_EDGE ( 'NONE', *, *, #126807, .T. ) ;
#76429 = CARTESIAN_POINT ( 'NONE',  ( 87.84959685856478018, 6.109999999999996767, 1.637169565754163836 ) ) ;
#76430 = ORIENTED_EDGE ( 'NONE', *, *, #72997, .T. ) ;
#76431 = LINE ( 'NONE', #62703, #105514 ) ;
#76432 = CARTESIAN_POINT ( 'NONE',  ( 2.277185695429367662, -21.72499999999999432, 5.000000000000000000 ) ) ;
#76433 = ADVANCED_FACE ( 'NONE', ( #36403 ), #83492, .T. ) ;
#76434 = VERTEX_POINT ( 'NONE', #58203 ) ;
#76435 = DIRECTION ( 'NONE',  ( 0.7071067811865486830, -0.7071067811865464625, -0.000000000000000000 ) ) ;
#76436 = DIRECTION ( 'NONE',  ( -0.000000000000000000, 0.000000000000000000, 1.000000000000000000 ) ) ;
#76437 = EDGE_CURVE ( 'NONE', #31525, #56636, #4406, .T. ) ;
#76438 = CARTESIAN_POINT ( 'NONE',  ( -34.92500000000001137, -22.22500000000000142, 4.000000000000000000 ) ) ;
#76439 = VECTOR ( 'NONE', #131742, 1000.000000000000114 ) ;
#76440 = DIRECTION ( 'NONE',  ( -0.7071067811865487940, 0.7071067811865463515, -0.000000000000000000 ) ) ;
#76441 = DIRECTION ( 'NONE',  ( 0.000000000000000000, 1.000000000000000000, 1.286409696682840916E-16 ) ) ;
#76442 = ADVANCED_FACE ( 'NONE', ( #48710 ), #30350, .T. ) ;
#76443 = CARTESIAN_POINT ( 'NONE',  ( -15.70612307739185276, 22.22500000000000142, 4.000000000000000000 ) ) ;
#76444 = DIRECTION ( 'NONE',  ( -0.7071067811865487940, 0.7071067811865463515, -0.000000000000000000 ) ) ;
#76446 = EDGE_LOOP ( 'NONE', ( #7293, #71102, #118270, #96210 ) ) ;
#76445 = VECTOR ( 'NONE', #66936, 1000.000000000000000 ) ;
#76447 = VECTOR ( 'NONE', #46543, 1000.000000000000000 ) ;
#76448 = VECTOR ( 'NONE', #111615, 1000.000000000000000 ) ;
#76449 = DIRECTION ( 'NONE',  ( 1.000000000000000000, 8.854317741964955179E-16, 0.000000000000000000 ) ) ;
#76450 = ORIENTED_EDGE ( 'NONE', *, *, #54527, .T. ) ;
#76451 = CARTESIAN_POINT ( 'NONE',  ( 122.2875270504628844, 0.000000000000000000, -7.949999999999998401 ) ) ;
#76452 = ADVANCED_FACE ( 'NONE', ( #71918 ), #5875, .F. ) ;
#76453 = LINE ( 'NONE', #34359, #86038 ) ;
#76454 = EDGE_CURVE ( 'NONE', #124853, #103174, #90590, .T. ) ;
#76455 =( GEOMETRIC_REPRESENTATION_CONTEXT ( 3 ) GLOBAL_UNCERTAINTY_ASSIGNED_CONTEXT ( ( #5489 ) ) GLOBAL_UNIT_ASSIGNED_CONTEXT ( ( #69508, #136877, #16501 ) ) REPRESENTATION_CONTEXT ( 'NONE', 'WORKASPACE' ) );
#76456 = VERTEX_POINT ( 'NONE', #61064 ) ;
#76457 = VERTEX_POINT ( 'NONE', #82085 ) ;
#76458 = CARTESIAN_POINT ( 'NONE',  ( 36.31293019189809712, -1.637169565754159617, -6.110000000000001208 ) ) ;
#76459 = VERTEX_POINT ( 'NONE', #80632 ) ;
#76460 = CIRCLE ( 'NONE', #74073, 2.500000000000000888 ) ;
#76461 = CARTESIAN_POINT ( 'NONE',  ( 45.77083333333332149, -7.949999999999998401, -2.130196079827426203 ) ) ;
#76462 = EDGE_CURVE ( 'NONE', #13854, #19029, #113955, .T. ) ;
#76463 = CARTESIAN_POINT ( 'NONE',  ( 90.20419371712957002, -6.884901960086285300, -3.975000000000000089 ) ) ;
#76464 = CARTESIAN_POINT ( 'NONE',  ( 21.62913961620377279, 5.278424836066147208, 3.047499999999990550 ) ) ;
#76465 = CARTESIAN_POINT ( 'NONE',  ( 7.952899274893373338, 10.68804939725090541, -26.53793298327174455 ) ) ;
#76466 = ORIENTED_EDGE ( 'NONE', *, *, #87301, .T. ) ;
#76467 = EDGE_CURVE ( 'NONE', #33777, #92406, #26941, .T. ) ;
#76468 = CARTESIAN_POINT ( 'NONE',  ( 33.18398860626899705, 28.73617430169810305, 5.000000000000000000 ) ) ;
#76469 = VERTEX_POINT ( 'NONE', #13903 ) ;
#76470 = CARTESIAN_POINT ( 'NONE',  ( 11.99999999999991296, 16.93112307739200872, 4.000000000000000000 ) ) ;
#76471 = AXIS2_PLACEMENT_3D ( 'NONE', #68881, #45706, #33413 ) ;
#76472 = DIRECTION ( 'NONE',  ( -1.000000000000000000, 0.000000000000000000, 0.000000000000000000 ) ) ;
#76474 = VERTEX_POINT ( 'NONE', #47338 ) ;
#76473 = PLANE ( 'NONE',  #142072 ) ;
#76475 = VERTEX_POINT ( 'NONE', #124832 ) ;
#76476 = CARTESIAN_POINT ( 'NONE',  ( -33.79289321881321939, 3.759292476615681888, 5.000000000000000000 ) ) ;
#76477 = CARTESIAN_POINT ( 'NONE',  ( 6.183988606268994381, 28.73617430169791476, 5.000000000000000000 ) ) ;
#76478 = FACE_OUTER_BOUND ( 'NONE', #129460, .T. ) ;
#76479 = ORIENTED_EDGE ( 'NONE', *, *, #99468, .F. ) ;
#76480 = VECTOR ( 'NONE', #54629, 999.9999999999998863 ) ;
#76481 = DIRECTION ( 'NONE',  ( -0.6830127018922181881, 0.6830127018922202975, -0.2588190451025214056 ) ) ;
#76482 = ORIENTED_EDGE ( 'NONE', *, *, #26386, .F. ) ;
#76483 = ORIENTED_EDGE ( 'NONE', *, *, #140049, .F. ) ;
#76484 = VERTEX_POINT ( 'NONE', #71191 ) ;
#76486 = CARTESIAN_POINT ( 'NONE',  ( -8.510786437626906675, -27.52281430457049183, 5.000000000000000000 ) ) ;
#76485 = AXIS2_PLACEMENT_3D ( 'NONE', #68518, #38020, #112701 ) ;
#76487 = PLANE ( 'NONE',  #34851 ) ;
#76488 = CARTESIAN_POINT ( 'NONE',  ( 30.48921356237309510, -27.52281430457076894, 5.000000000000000000 ) ) ;
#76489 = VECTOR ( 'NONE', #35557, 1000.000000000000000 ) ;
#76490 = DIRECTION ( 'NONE',  ( 0.2419218955996628451, 0.000000000000000000, -0.9702957262759975832 ) ) ;
#76491 = LINE ( 'NONE', #19928, #109561 ) ;
#76492 = EDGE_CURVE ( 'NONE', #93995, #73867, #115339, .T. ) ;
#76493 = CARTESIAN_POINT ( 'NONE',  ( 0.000000000000000000, 2.375000000000000000, -4.320000000000002061 ) ) ;
#76494 = ORIENTED_EDGE ( 'NONE', *, *, #19635, .F. ) ;
#76495 = AXIS2_PLACEMENT_3D ( 'NONE', #108520, #21561, #133201 ) ;
#76496 = CARTESIAN_POINT ( 'NONE',  ( 97.20419371712955581, -6.884901960086285300, -3.975000000000000089 ) ) ;
#76497 = ORIENTED_EDGE ( 'NONE', *, *, #107634, .T. ) ;
#76498 = DIRECTION ( 'NONE',  ( 1.000000000000000000, 1.224606353822377258E-16, 0.000000000000000000 ) ) ;
#76499 = CARTESIAN_POINT ( 'NONE',  ( -63.48921356237309510, -27.52281430457099631, 5.000000000000000000 ) ) ;
#76500 = LINE ( 'NONE', #19937, #64688 ) ;
#76501 = ORIENTED_EDGE ( 'NONE', *, *, #8540, .T. ) ;
#76502 = VECTOR ( 'NONE', #19870, 1000.000000000000000 ) ;
#76503 = DIRECTION ( 'NONE',  ( 1.000000000000000000, 0.000000000000000000, 0.000000000000000000 ) ) ;
#76504 = LINE ( 'NONE', #128885, #62684 ) ;
#76505 = PLANE ( 'NONE',  #46772 ) ;
#76506 = VERTEX_POINT ( 'NONE', #84897 ) ;
#76507 = ORIENTED_EDGE ( 'NONE', *, *, #44170, .F. ) ;
#76508 = CARTESIAN_POINT ( 'NONE',  ( 12.19999999999999574, -40.43000000000000682, -39.50000000000000000 ) ) ;
#76509 = AXIS2_PLACEMENT_3D ( 'NONE', #65491, #54595, #100233 ) ;
#76510 = FACE_OUTER_BOUND ( 'NONE', #32661, .T. ) ;
#76511 = CARTESIAN_POINT ( 'NONE',  ( 53.06250000000000000, -5.819803920172573086, -5.819803920172573974 ) ) ;
#76512 = DIRECTION ( 'NONE',  ( 0.7071067811865486830, -0.7071067811865464625, -0.000000000000000000 ) ) ;
#76513 = CARTESIAN_POINT ( 'NONE',  ( 68.45376352523143737, -6.109999999999999432, -3.741295971395163529E-16 ) ) ;
#76514 = ADVANCED_FACE ( 'NONE', ( #116808 ), #86345, .F. ) ;
#76515 = CARTESIAN_POINT ( 'NONE',  ( 8.897059064271770623, 2.055000000000001048, 0.000000000000000000 ) ) ;
#76516 = LINE ( 'NONE', #54758, #20679 ) ;
#76517 = EDGE_CURVE ( 'NONE', #89322, #99498, #142161, .T. ) ;
#76518 = LINE ( 'NONE', #141772, #95092 ) ;
#76519 = CARTESIAN_POINT ( 'NONE',  ( -39.29974487139159578, -27.71228299555233576, 4.000000000000000000 ) ) ;
#76520 = ORIENTED_EDGE ( 'NONE', *, *, #73788, .F. ) ;
#76521 = CARTESIAN_POINT ( 'NONE',  ( -27.29974487139158512, -27.71228299555225405, 4.000000000000000000 ) ) ;
#76522 = EDGE_LOOP ( 'NONE', ( #40045, #131116, #9745, #16556 ) ) ;
#76523 = VECTOR ( 'NONE', #78984, 1000.000000000000000 ) ;
#76524 = DIRECTION ( 'NONE',  ( -0.7071067811865486830, -0.7071067811865464625, 0.000000000000000000 ) ) ;
#76525 = VERTEX_POINT ( 'NONE', #131263 ) ;
#76526 = DIRECTION ( 'NONE',  ( -0.000000000000000000, 0.000000000000000000, 1.000000000000000000 ) ) ;
#76527 = CARTESIAN_POINT ( 'NONE',  ( -36.29974487139159578, -27.71228299555231445, 4.000000000000000000 ) ) ;
#76528 = CARTESIAN_POINT ( 'NONE',  ( 8.999999999999932498, 19.93112307739198386, 4.000000000000000000 ) ) ;
#76529 = EDGE_CURVE ( 'NONE', #124509, #142351, #41386, .T. ) ;
#76530 = CARTESIAN_POINT ( 'NONE',  ( -31.92499999999997584, -6.270000000000012008, -40.00000000000000000 ) ) ;
#76531 = PLANE ( 'NONE',  #38002 ) ;
#76532 = ORIENTED_EDGE ( 'NONE', *, *, #54761, .T. ) ;
#76533 = ORIENTED_EDGE ( 'NONE', *, *, #28548, .T. ) ;
#76534 = DIRECTION ( 'NONE',  ( 0.7071067811865486830, -0.7071067811865464625, -0.000000000000000000 ) ) ;
#76535 = FACE_BOUND ( 'NONE', #68381, .T. ) ;
#76536 = UNCERTAINTY_MEASURE_WITH_UNIT (LENGTH_MEASURE( 1.000000000000000082E-05 ), #56860, 'distance_accuracy_value', 'NONE');
#76537 = AXIS2_PLACEMENT_3D ( 'NONE', #3207, #24954, #133748 ) ;
#76538 = CARTESIAN_POINT ( 'NONE',  ( -11.99999999999992184, 13.93112307739204603, 4.000000000000000000 ) ) ;
#76539 = CARTESIAN_POINT ( 'NONE',  ( 15.50413961620377279, -3.047499999999994547, 5.278424836066145431 ) ) ;
#76540 = CARTESIAN_POINT ( 'NONE',  ( 86.55836038379621300, -7.949999999999997513, -2.130196079827425759 ) ) ;
#76541 = DIRECTION ( 'NONE',  ( 0.6830127018922181881, 0.6830127018922202975, -0.2588190451025214056 ) ) ;
#76542 = CARTESIAN_POINT ( 'NONE',  ( 34.92499999999998295, -10.19990548397272256, 4.759050581649326261 ) ) ;
#76543 = ORIENTED_EDGE ( 'NONE', *, *, #23950, .T. ) ;
#76544 = CARTESIAN_POINT ( 'NONE',  ( 83.97916666666665719, -7.950000000000001066, 2.130196079827424427 ) ) ;
#76545 = CARTESIAN_POINT ( 'NONE',  ( 21.29974487139158512, -27.71228299555221142, 4.000000000000000000 ) ) ;
#76546 = DIRECTION ( 'NONE',  ( 0.7071067811865486830, -0.7071067811865464625, -0.000000000000000000 ) ) ;
#76547 = CARTESIAN_POINT ( 'NONE',  ( -10.49999999999992184, 19.39370406404966118, 1.459788787078225569 ) ) ;
#76548 = EDGE_LOOP ( 'NONE', ( #112726, #105926, #10747, #21469 ) ) ;
#76549 = AXIS2_PLACEMENT_3D ( 'NONE', #119957, #20670, #9798 ) ;
#76550 = CARTESIAN_POINT ( 'NONE',  ( 5.691592354503320905, 2.500000000000001332, 0.000000000000000000 ) ) ;
#76551 = ORIENTED_EDGE ( 'NONE', *, *, #42812, .F. ) ;
#76552 = VECTOR ( 'NONE', #83725, 1000.000000000000000 ) ;
#76553 = CARTESIAN_POINT ( 'NONE',  ( 78.89626352523143282, 4.472830434245840259, -4.472830434245839371 ) ) ;
#76554 = EDGE_LOOP ( 'NONE', ( #139344, #2523, #137443, #83567 ) ) ;
#76555 = EDGE_CURVE ( 'NONE', #99234, #143251, #48892, .T. ) ;
#76556 = VECTOR ( 'NONE', #23863, 999.9999999999998863 ) ;
#76557 = AXIS2_PLACEMENT_3D ( 'NONE', #119428, #130353, #97704 ) ;
#76558 = VECTOR ( 'NONE', #82538, 1000.000000000000000 ) ;
#76559 = AXIS2_PLACEMENT_3D ( 'NONE', #116836, #17512, #74051 ) ;
#76560 = CARTESIAN_POINT ( 'NONE',  ( -39.18398860626899705, 28.73617430169814568, 5.000000000000000000 ) ) ;
#76562 = CARTESIAN_POINT ( 'NONE',  ( -36.18398860626899705, 28.73617430169812437, 5.000000000000000000 ) ) ;
#76561 = AXIS2_PLACEMENT_3D ( 'NONE', #24377, #36668, #68625 ) ;
#76563 = DIRECTION ( 'NONE',  ( -0.000000000000000000, -0.3543493200069152693, 0.9351131265310292928 ) ) ;
#76564 = LINE ( 'NONE', #77290, #57870 ) ;
#76565 = CARTESIAN_POINT ( 'NONE',  ( 55.45418156660456788, -52.10373894832328290, 40.45955814675563289 ) ) ;
#76566 = EDGE_CURVE ( 'NONE', #79108, #60521, #130564, .T. ) ;
#76568 = ORIENTED_EDGE ( 'NONE', *, *, #21118, .T. ) ;
#76567 = CARTESIAN_POINT ( 'NONE',  ( -42.48921356237308800, -27.52281430457085065, 5.000000000000000000 ) ) ;
#76569 = LINE ( 'NONE', #66397, #46181 ) ;
#76570 = DIRECTION ( 'NONE',  ( 1.000000000000000000, 0.000000000000000000, 0.000000000000000000 ) ) ;
#76571 = CARTESIAN_POINT ( 'NONE',  ( 2.999999999999993783, 2.587461875839212944, 4.000000000000000000 ) ) ;
#76572 = VECTOR ( 'NONE', #134865, 1000.000000000000000 ) ;
#76573 = CARTESIAN_POINT ( 'NONE',  ( 17.81601139373099940, 28.73617430169775133, 5.000000000000000000 ) ) ;
#76574 = ORIENTED_EDGE ( 'NONE', *, *, #36798, .T. ) ;
#76576 = VERTEX_POINT ( 'NONE', #40692 ) ;
#76575 = EDGE_CURVE ( 'NONE', #65577, #68093, #84221, .T. ) ;
#76577 = EDGE_CURVE ( 'NONE', #120738, #53245, #118215, .T. ) ;
#76578 = CARTESIAN_POINT ( 'NONE',  ( 62.70876352523143993, -7.482591942790329030E-16, 6.110000000000001208 ) ) ;
#76579 = VERTEX_POINT ( 'NONE', #119635 ) ;
#76580 = EDGE_CURVE ( 'NONE', #58068, #34917, #74030, .T. ) ;
#76581 = FACE_OUTER_BOUND ( 'NONE', #43403, .T. ) ;
#76582 = CARTESIAN_POINT ( 'NONE',  ( -34.49999999999976552, 0.05432934483094037370, 4.994342998332168548 ) ) ;
#76583 = ADVANCED_FACE ( 'NONE', ( #18921 ), #29093, .T. ) ;
#76584 = AXIS2_PLACEMENT_3D ( 'NONE', #55637, #3358, #66514 ) ;
#76585 = SURFACE_STYLE_FILL_AREA ( #32346 ) ;
#76586 = VERTEX_POINT ( 'NONE', #7312 ) ;
#76587 = ORIENTED_EDGE ( 'NONE', *, *, #132431, .T. ) ;
#76588 = ADVANCED_FACE ( 'NONE', ( #20332 ), #64576, .F. ) ;
#76589 = PLANE ( 'NONE',  #23694 ) ;
#76590 = CARTESIAN_POINT ( 'NONE',  ( 12.86840764549667604, 9.139736423841732040E-16, 0.000000000000000000 ) ) ;
#76591 = VECTOR ( 'NONE', #129339, 999.9999999999998863 ) ;
#76592 = EDGE_CURVE ( 'NONE', #106721, #116046, #21133, .T. ) ;
#76593 = VERTEX_POINT ( 'NONE', #95769 ) ;
#76594 = AXIS2_PLACEMENT_3D ( 'NONE', #48796, #137229, #37930 ) ;
#76595 = CARTESIAN_POINT ( 'NONE',  ( -18.38945826904184599, 9.109118024354394549, 4.348864708961791337 ) ) ;
#76596 = VECTOR ( 'NONE', #104503, 1000.000000000000000 ) ;
#76597 = CARTESIAN_POINT ( 'NONE',  ( 1.353980332882009252, -0.3999999999999997446, -2.467792535850613866 ) ) ;
#76598 = FACE_OUTER_BOUND ( 'NONE', #130623, .T. ) ;
#76599 = VECTOR ( 'NONE', #129430, 1000.000000000000227 ) ;
#76600 = EDGE_LOOP ( 'NONE', ( #130647, #141798, #65425, #10917 ) ) ;
#76601 = EDGE_CURVE ( 'NONE', #110589, #125118, #6572, .T. ) ;
#76602 = ADVANCED_FACE ( 'NONE', ( #50848 ), #139316, .T. ) ;
#76603 = FACE_BOUND ( 'NONE', #43462, .T. ) ;
#76604 = CONICAL_SURFACE ( 'NONE', #4798, 2.500000000000000444, 0.9599310885968830309 ) ;
#76605 = DIRECTION ( 'NONE',  ( 0.000000000000000000, 1.000000000000000000, 0.000000000000000000 ) ) ;
#76606 = DIRECTION ( 'NONE',  ( -0.7071067811865487940, 0.7071067811865463515, -0.000000000000000000 ) ) ;
#76607 = CARTESIAN_POINT ( 'NONE',  ( 60.64583333333332860, 2.130196079827431976, -7.949999999999998401 ) ) ;
#76608 = DIRECTION ( 'NONE',  ( -0.7071067811865486830, -0.7071067811865464625, -0.000000000000000000 ) ) ;
#76609 = EDGE_CURVE ( 'NONE', #32796, #10266, #108754, .T. ) ;
#76610 = CARTESIAN_POINT ( 'NONE',  ( 1.199999999999999956, -0.6000000000000001998, 4.543283425070392845 ) ) ;
#76611 = EDGE_LOOP ( 'NONE', ( #111291, #26798, #75479, #88350 ) ) ;
#76612 = AXIS2_PLACEMENT_3D ( 'NONE', #10501, #143174, #21406 ) ;
#76613 = EDGE_LOOP ( 'NONE', ( #118341, #142337, #26519, #81753 ) ) ;
#76614 = CARTESIAN_POINT ( 'NONE',  ( 108.1204301918981230, 3.055000000000001936, -5.291415217122916737 ) ) ;
#76615 = ORIENTED_EDGE ( 'NONE', *, *, #97105, .F. ) ;
#76616 = ORIENTED_EDGE ( 'NONE', *, *, #32598, .T. ) ;
#76617 = VECTOR ( 'NONE', #61743, 1000.000000000000227 ) ;
#76618 = CARTESIAN_POINT ( 'NONE',  ( 183.4386084925739340, -49.19295221407111995, 41.21232802153470942 ) ) ;
#76619 = DIRECTION ( 'NONE',  ( 0.7071067811865487940, -0.7071067811865463515, 0.000000000000000000 ) ) ;
#76620 = DIRECTION ( 'NONE',  ( 0.6830127018922180770, -0.6830127018922204085, -0.2588190451025213501 ) ) ;
#76621 = ORIENTED_EDGE ( 'NONE', *, *, #101411, .T. ) ;
#76622 = DIRECTION ( 'NONE',  ( -0.6830127018922180770, -0.6830127018922204085, -0.2588190451025213501 ) ) ;
#76623 = CARTESIAN_POINT ( 'NONE',  ( 12.48921356237309155, -27.52281430457064104, 5.000000000000000000 ) ) ;
#76625 = DIRECTION ( 'NONE',  ( -0.7071067811865487940, 0.7071067811865463515, 0.000000000000000000 ) ) ;
#76624 = CARTESIAN_POINT ( 'NONE',  ( 34.92499999999998295, 17.81665438641027777, 4.500000000000000888 ) ) ;
#76626 = ADVANCED_FACE ( 'NONE', ( #97924 ), #63188, .F. ) ;
#76627 = LINE ( 'NONE', #9141, #127227 ) ;
#76628 = VECTOR ( 'NONE', #36690, 1000.000000000000000 ) ;
#76629 = DIRECTION ( 'NONE',  ( 6.895928203464619851E-15, 0.6666666666666692942, 0.7453559924999275665 ) ) ;
#76630 = VERTEX_POINT ( 'NONE', #140692 ) ;
#76631 = CARTESIAN_POINT ( 'NONE',  ( 20.99451991528748707, 28.92564299267952777, 4.000000000000000000 ) ) ;
#76632 = LINE ( 'NONE', #122967, #90495 ) ;
#76633 = VERTEX_POINT ( 'NONE', #101478 ) ;
#76634 = ORIENTED_EDGE ( 'NONE', *, *, #53845, .T. ) ;
#76635 = EDGE_LOOP ( 'NONE', ( #86396, #27454, #104780, #111844 ) ) ;
#76636 = CARTESIAN_POINT ( 'NONE',  ( 65.62543019189810423, 5.291415217122919401, 3.055000000000002824 ) ) ;
#76637 = EDGE_LOOP ( 'NONE', ( #4644, #55642, #82923, #114428, #10369 ) ) ;
#76638 = AXIS2_PLACEMENT_3D ( 'NONE', #44221, #100013, #111593 ) ;
#76639 = EDGE_CURVE ( 'NONE', #15951, #44387, #33418, .T. ) ;
#76640 = DIRECTION ( 'NONE',  ( 0.7071067811865487940, -0.7071067811865463515, 0.000000000000000000 ) ) ;
#76641 = CARTESIAN_POINT ( 'NONE',  ( 0.1916396162037724282, 6.094999999999988205, -1.633150327867694651 ) ) ;
#76642 = CARTESIAN_POINT ( 'NONE',  ( 102.9587635252314470, 0.000000000000000000, -6.110000000000001208 ) ) ;
#76643 = CARTESIAN_POINT ( 'NONE',  ( 31.00193056682077142, -22.22500000000000142, 4.500000000000000888 ) ) ;
#76644 = ADVANCED_FACE ( 'NONE', ( #13027 ), #133418, .T. ) ;
#76645 = ORIENTED_EDGE ( 'NONE', *, *, #135614, .T. ) ;
#76646 = CARTESIAN_POINT ( 'NONE',  ( 42.29974487139158157, -27.71228299555235708, 4.000000000000000000 ) ) ;
#76647 = AXIS2_PLACEMENT_3D ( 'NONE', #113000, #2811, #56552 ) ;
#76648 = DIRECTION ( 'NONE',  ( 1.000000000000000000, 0.000000000000000000, 0.000000000000000000 ) ) ;
#76649 = LINE ( 'NONE', #9927, #23631 ) ;
#76651 = LINE ( 'NONE', #21533, #26683 ) ;
#76650 = VECTOR ( 'NONE', #135976, 1000.000000000000227 ) ;
#76653 = EDGE_LOOP ( 'NONE', ( #73252, #62236, #36143, #115203 ) ) ;
#76652 = VECTOR ( 'NONE', #120205, 1000.000000000000000 ) ;
#76654 = LINE ( 'NONE', #44008, #50677 ) ;
#76655 = EDGE_CURVE ( 'NONE', #19199, #98173, #66034, .T. ) ;
#76656 = VERTEX_POINT ( 'NONE', #10871 ) ;
#76657 = VERTEX_POINT ( 'NONE', #2128 ) ;
#76658 = ORIENTED_EDGE ( 'NONE', *, *, #14540, .T. ) ;
#76659 = CARTESIAN_POINT ( 'NONE',  ( 120.0787635252314516, -7.482591942790325086E-16, 6.109999999999998543 ) ) ;
#76660 = AXIS2_PLACEMENT_3D ( 'NONE', #24264, #56922, #1745 ) ;
#76661 = EDGE_LOOP ( 'NONE', ( #57186, #77442, #35632, #48728 ) ) ;
#76662 = VECTOR ( 'NONE', #12641, 1000.000000000000000 ) ;
#76663 = VECTOR ( 'NONE', #128445, 999.9999999999998863 ) ;
#76664 = AXIS2_PLACEMENT_3D ( 'NONE', #130685, #121195, #32799 ) ;
#76665 = CARTESIAN_POINT ( 'NONE',  ( 8.423184310185783730, 4.584330080086930965E-16, 0.000000000000000000 ) ) ;
#76666 = ADVANCED_FACE ( 'NONE', ( #65324 ), #721, .F. ) ;
#76667 = LINE ( 'NONE', #22227, #138945 ) ;
#76668 = ORIENTED_EDGE ( 'NONE', *, *, #89746, .T. ) ;
#76669 = CARTESIAN_POINT ( 'NONE',  ( -5.277185695429377432, -21.72500000000000853, 5.000000000000000000 ) ) ;
#76671 = VERTEX_POINT ( 'NONE', #55869 ) ;
#76670 = VECTOR ( 'NONE', #58585, 1000.000000000000000 ) ;
#76672 = CARTESIAN_POINT ( 'NONE',  ( 9.749569808101886892, 3.967499999999998916, 6.871911579029510442 ) ) ;
#76673 = EDGE_CURVE ( 'NONE', #13309, #32684, #121788, .T. ) ;
#76674 = CARTESIAN_POINT ( 'NONE',  ( -8.994519915287490619, 28.92564299267944250, 4.000000000000000000 ) ) ;
#76675 = VECTOR ( 'NONE', #59842, 1000.000000000000000 ) ;
#76676 = CARTESIAN_POINT ( 'NONE',  ( 39.06250000000000000, -5.819803920172573086, -5.819803920172573974 ) ) ;
#76677 = ORIENTED_EDGE ( 'NONE', *, *, #28506, .T. ) ;
#76678 = ORIENTED_EDGE ( 'NONE', *, *, #57926, .T. ) ;
#76679 = EDGE_LOOP ( 'NONE', ( #127850, #80687, #140853, #34235 ) ) ;
#76680 = AXIS2_PLACEMENT_3D ( 'NONE', #29762, #139999, #7288 ) ;
#76681 = CARTESIAN_POINT ( 'NONE',  ( -12.19999999999999929, -60.26999999999998892, -39.50000000000000000 ) ) ;
#76682 = UNCERTAINTY_MEASURE_WITH_UNIT (LENGTH_MEASURE( 1.000000000000000082E-05 ), #58354, 'distance_accuracy_value', 'NONE');
#76683 = LINE ( 'NONE', #120857, #68220 ) ;
#76684 = FACE_OUTER_BOUND ( 'NONE', #38465, .T. ) ;
#76685 = VECTOR ( 'NONE', #74091, 999.9999999999998863 ) ;
#76686 = AXIS2_PLACEMENT_3D ( 'NONE', #3920, #2513, #133094 ) ;
#76687 = LINE ( 'NONE', #85375, #143313 ) ;
#76688 = ADVANCED_FACE ( 'NONE', ( #66723 ), #44278, .F. ) ;
#76689 = CARTESIAN_POINT ( 'NONE',  ( 33.25043019189810423, 3.055000000000002824, -5.291415217122919401 ) ) ;
#76690 = PLANE ( 'NONE',  #134720 ) ;
#76691 = LINE ( 'NONE', #21573, #106783 ) ;
#76692 = CONICAL_SURFACE ( 'NONE', #65096, 2.055000000000001048, 0.9599310885968758145 ) ;
#76693 = ORIENTED_EDGE ( 'NONE', *, *, #24659, .F. ) ;
#76694 = LINE ( 'NONE', #97696, #83393 ) ;
#76695 = VERTEX_POINT ( 'NONE', #90628 ) ;
#76697 = VECTOR ( 'NONE', #24781, 1000.000000000000227 ) ;
#76696 = DIRECTION ( 'NONE',  ( 0.000000000000000000, 0.000000000000000000, 1.000000000000000000 ) ) ;
#76698 = ORIENTED_EDGE ( 'NONE', *, *, #63054, .T. ) ;
#76699 = PLANE ( 'NONE',  #20568 ) ;
#76701 = ORIENTED_EDGE ( 'NONE', *, *, #67174, .F. ) ;
#76700 = DIRECTION ( 'NONE',  ( -0.7071067811865486830, -0.7071067811865464625, 0.000000000000000000 ) ) ;
#76702 = VECTOR ( 'NONE', #57277, 1000.000000000000227 ) ;
#76703 = EDGE_CURVE ( 'NONE', #54005, #109319, #31950, .T. ) ;
#76704 = CARTESIAN_POINT ( 'NONE',  ( 15.79289321881335084, 9.759292476615625489, 5.000000000000000000 ) ) ;
#76705 = VERTEX_POINT ( 'NONE', #34107 ) ;
#76706 = FILL_AREA_STYLE ('',( #57094 ) ) ;
#76707 = EDGE_LOOP ( 'NONE', ( #5423, #67325, #6292, #9241 ) ) ;
#76708 = CARTESIAN_POINT ( 'NONE',  ( -66.48921356237309510, -27.52281430457101763, 5.000000000000000000 ) ) ;
#76709 = UNCERTAINTY_MEASURE_WITH_UNIT (LENGTH_MEASURE( 1.000000000000000082E-05 ), #90263, 'distance_accuracy_value', 'NONE');
#76710 = ORIENTED_EDGE ( 'NONE', *, *, #49536, .F. ) ;
#76711 = PRODUCT_RELATED_PRODUCT_CATEGORY ( 'part', '', ( #118763 ) ) ;
#76712 = CARTESIAN_POINT ( 'NONE',  ( 6.707013264292989163, -21.74070752338407075, 4.999753212805213565 ) ) ;
#76713 = CARTESIAN_POINT ( 'NONE',  ( 108.1416937171295700, -2.130196079827424871, -7.949999999999999289 ) ) ;
#76714 = CARTESIAN_POINT ( 'NONE',  ( 50.53752705046289861, -9.735942053221456900E-16, 7.949999999999998401 ) ) ;
#76715 = AXIS2_PLACEMENT_3D ( 'NONE', #88178, #33120, #33805 ) ;
#76716 = SURFACE_STYLE_USAGE ( .BOTH. , #32476 ) ;
#76717 = FACE_OUTER_BOUND ( 'NONE', #92090, .T. ) ;
#76718 = DIRECTION ( 'NONE',  ( -0.000000000000000000, -0.3543493200069152693, 0.9351131265310292928 ) ) ;
#76719 = DIRECTION ( 'NONE',  ( 0.7071067811865486830, -0.7071067811865464625, -0.000000000000000000 ) ) ;
#76720 = CARTESIAN_POINT ( 'NONE',  ( 2.479166666666666963, 6.094999999999988205, -1.633150327867694651 ) ) ;
#76721 = CARTESIAN_POINT ( 'NONE',  ( 15.58290314143522082, 3.967499999999992699, -6.871911579029513994 ) ) ;
#76723 = AXIS2_PLACEMENT_3D ( 'NONE', #126733, #27422, #86835 ) ;
#76722 = CARTESIAN_POINT ( 'NONE',  ( -7.828169399223476432, -8.240707523384205757, 4.000000000000000000 ) ) ;
#76724 = DIRECTION ( 'NONE',  ( -0.6830127018922181881, 0.6830127018922202975, -0.2588190451025214056 ) ) ;
#76725 = ORIENTED_EDGE ( 'NONE', *, *, #114829, .F. ) ;
#76726 = ORIENTED_EDGE ( 'NONE', *, *, #110186, .T. ) ;
#76727 = LINE ( 'NONE', #120154, #99916 ) ;
#76728 = ORIENTED_EDGE ( 'NONE', *, *, #137422, .T. ) ;
#76729 = LINE ( 'NONE', #46244, #131352 ) ;
#76731 = VECTOR ( 'NONE', #63838, 1000.000000000000000 ) ;
#76730 = DIRECTION ( 'NONE',  ( -0.000000000000000000, -0.000000000000000000, 1.000000000000000000 ) ) ;
#76732 = CARTESIAN_POINT ( 'NONE',  ( -22.49999999999983302, 22.08746187583901843, 4.000000000000000000 ) ) ;
#76733 = EDGE_LOOP ( 'NONE', ( #125388, #117860, #74449, #120215 ) ) ;
#76734 = DIRECTION ( 'NONE',  ( -0.7071067811865486830, -0.7071067811865464625, 0.000000000000000000 ) ) ;
#76735 =( BOUNDED_CURVE ( )  B_SPLINE_CURVE ( 3, ( #117134, #59936, #139658, #4763 ),
 .UNSPECIFIED., .F., .F. ) 
 B_SPLINE_CURVE_WITH_KNOTS ( ( 4, 4 ),
 ( 5.143245962375964986, 6.645403452391247079 ),
 .UNSPECIFIED. ) 
 CURVE ( )  GEOMETRIC_REPRESENTATION_ITEM ( )  RATIONAL_B_SPLINE_CURVE ( ( 1.000000000000000000, 0.8206354192515239454, 0.8206354192515239454, 1.000000000000000000 ) ) 
 REPRESENTATION_ITEM ( '' )  );
#76736 = PLANE ( 'NONE',  #69644 ) ;
#76737 = FACE_OUTER_BOUND ( 'NONE', #117781, .T. ) ;
#76738 = PRESENTATION_STYLE_ASSIGNMENT (( #108576 ) ) ;
#76740 = ORIENTED_EDGE ( 'NONE', *, *, #127452, .T. ) ;
#76739 = CARTESIAN_POINT ( 'NONE',  ( 12.71159235450332048, 9.902892378096218942E-16, 0.000000000000000000 ) ) ;
#76741 = PLANE ( 'NONE',  #88303 ) ;
#76742 = AXIS2_PLACEMENT_3D ( 'NONE', #1427, #100071, #12325 ) ;
#76743 = DIRECTION ( 'NONE',  ( -0.000000000000000000, 1.000000000000000000, 2.242629915582283412E-16 ) ) ;
#76744 = DIRECTION ( 'NONE',  ( -1.000000000000000000, -1.224606353822377258E-16, -0.000000000000000000 ) ) ;
#76745 = DIRECTION ( 'NONE',  ( -0.000000000000000000, 0.000000000000000000, 1.000000000000000000 ) ) ;
#76746 = EDGE_LOOP ( 'NONE', ( #9763, #114852, #96999, #27024 ) ) ;
#76747 = VERTEX_POINT ( 'NONE', #54445 ) ;
#76748 = ORIENTED_EDGE ( 'NONE', *, *, #3398, .F. ) ;
#76749 = EDGE_CURVE ( 'NONE', #123646, #17485, #110199, .T. ) ;
#76750 = CARTESIAN_POINT ( 'NONE',  ( 95.22959685856474721, -6.110000000000000320, -1.637169565754161393 ) ) ;
#76751 = ORIENTED_EDGE ( 'NONE', *, *, #43922, .T. ) ;
#76752 = EDGE_CURVE ( 'NONE', #32290, #38181, #99318, .T. ) ;
#76753 = CARTESIAN_POINT ( 'NONE',  ( 126.2665610010944874, -48.52444309369082731, 36.09967824800328628 ) ) ;
#76754 = EDGE_CURVE ( 'NONE', #18784, #97146, #98619, .T. ) ;
#76755 = LINE ( 'NONE', #120934, #40851 ) ;
#76756 = ORIENTED_EDGE ( 'NONE', *, *, #73313, .T. ) ;
#76757 = VECTOR ( 'NONE', #108346, 1000.000000000000000 ) ;
#76758 = ADVANCED_FACE ( 'NONE', ( #131991 ), #45016, .F. ) ;
#76759 = PLANE ( 'NONE',  #99972 ) ;
#76760 = LINE ( 'NONE', #74608, #58271 ) ;
#76761 = AXIS2_PLACEMENT_3D ( 'NONE', #3812, #136507, #92281 ) ;
#76762 = VECTOR ( 'NONE', #88729, 1000.000000000000000 ) ;
#76763 = CARTESIAN_POINT ( 'NONE',  ( 85.37043019189812298, -3.055000000000001492, 5.291415217122917625 ) ) ;
#76764 = EDGE_LOOP ( 'NONE', ( #35624, #107405, #44537, #42252 ) ) ;
#76765 = DIRECTION ( 'NONE',  ( -0.000000000000000000, -0.3543493200069152693, 0.9351131265310292928 ) ) ;
#76766 = VECTOR ( 'NONE', #33374, 1000.000000000000000 ) ;
#76767 = CIRCLE ( 'NONE', #51291, 5.968999999999998529 ) ;
#76768 = CARTESIAN_POINT ( 'NONE',  ( -34.92500000000001137, 11.71849043720411032, 4.759050581649336920 ) ) ;
#76769 = VECTOR ( 'NONE', #75272, 999.9999999999998863 ) ;
#76770 = VECTOR ( 'NONE', #139872, 1000.000000000000000 ) ;
#76771 = ORIENTED_EDGE ( 'NONE', *, *, #137897, .F. ) ;
#76772 = EDGE_LOOP ( 'NONE', ( #74618, #104272 ) ) ;
#76773 = ADVANCED_FACE ( 'NONE', ( #84215 ), #88488, .F. ) ;
#76774 = ORIENTED_EDGE ( 'NONE', *, *, #116942, .F. ) ;
#76775 = LINE ( 'NONE', #107905, #37618 ) ;
#76776 = ADVANCED_FACE ( 'NONE', ( #134130 ), #89194, .F. ) ;
#76777 = PLANE ( 'NONE',  #31628 ) ;
#76778 = CARTESIAN_POINT ( 'NONE',  ( 14.94206980810188590, 7.934999999999992504, 2.126176841940951689 ) ) ;
#76779 = DIRECTION ( 'NONE',  ( 0.7071067811865486830, -0.7071067811865464625, -0.000000000000000000 ) ) ;
#76780 = AXIS2_PLACEMENT_3D ( 'NONE', #32148, #29991, #97370 ) ;
#76781 = CARTESIAN_POINT ( 'NONE',  ( 159.7320121765528711, 26.96999999999993847, 34.92499999999998295 ) ) ;
#76782 = EDGE_CURVE ( 'NONE', #95164, #123516, #56609, .T. ) ;
#76783 = FACE_OUTER_BOUND ( 'NONE', #37775, .T. ) ;
#76784 = EDGE_LOOP ( 'NONE', ( #95582, #111013, #20127, #121938 ) ) ;
#76785 = EDGE_LOOP ( 'NONE', ( #24383, #96371, #103355, #119919 ) ) ;
#76786 = VECTOR ( 'NONE', #21324, 1000.000000000000000 ) ;
#76787 = DIRECTION ( 'NONE',  ( -0.7071067811865486830, -0.7071067811865464625, 0.000000000000000000 ) ) ;
#76788 = ORIENTED_EDGE ( 'NONE', *, *, #110926, .F. ) ;
#76789 = EDGE_LOOP ( 'NONE', ( #115371, #22603, #82702, #48563, #115280, #16020 ) ) ;
#76790 = EDGE_CURVE ( 'NONE', #21344, #13457, #132209, .T. ) ;
#76791 = VECTOR ( 'NONE', #106501, 1000.000000000000000 ) ;
#76792 = VECTOR ( 'NONE', #39679, 1000.000000000000000 ) ;
#76793 = LINE ( 'NONE', #130444, #65950 ) ;
#76794 = ORIENTED_EDGE ( 'NONE', *, *, #83811, .T. ) ;
#76795 = CARTESIAN_POINT ( 'NONE',  ( 52.60764783923757193, -49.05583548141699879, 39.86617647058822200 ) ) ;
#76796 = DIRECTION ( 'NONE',  ( -0.000000000000000000, 0.000000000000000000, 1.000000000000000000 ) ) ;
#76797 = VECTOR ( 'NONE', #67560, 1000.000000000000000 ) ;
#76798 = CARTESIAN_POINT ( 'NONE',  ( 1.045157733366657071, -21.74070752338406010, 21.72585301388584611 ) ) ;
#76799 = EDGE_CURVE ( 'NONE', #54290, #19121, #72033, .T. ) ;
#76800 = CARTESIAN_POINT ( 'NONE',  ( -8.999999999999925393, -19.44781430457063465, 5.000000000000000000 ) ) ;
#76801 = VECTOR ( 'NONE', #49961, 1000.000000000000000 ) ;
#76802 = DIRECTION ( 'NONE',  ( -1.000000000000000000, -0.000000000000000000, -0.000000000000000000 ) ) ;
#76803 = ORIENTED_EDGE ( 'NONE', *, *, #65433, .T. ) ;
#76804 = DIRECTION ( 'NONE',  ( -0.7071067811865487940, 0.7071067811865463515, -0.000000000000000000 ) ) ;
#76805 = ORIENTED_EDGE ( 'NONE', *, *, #77919, .T. ) ;
#76806 = CARTESIAN_POINT ( 'NONE',  ( 22.55334942336767767, 2.259292476615690770, 14.86850063742348915 ) ) ;
#76807 = ORIENTED_EDGE ( 'NONE', *, *, #142991, .F. ) ;
#76808 = FACE_OUTER_BOUND ( 'NONE', #15709, .T. ) ;
#76809 = ORIENTED_EDGE ( 'NONE', *, *, #113509, .T. ) ;
#76810 = LINE ( 'NONE', #120982, #71390 ) ;
#76811 = ORIENTED_EDGE ( 'NONE', *, *, #131432, .F. ) ;
#76812 = ORIENTED_EDGE ( 'NONE', *, *, #29567, .T. ) ;
#76813 = EDGE_LOOP ( 'NONE', ( #60059, #114971, #116483, #38981 ) ) ;
#76814 = EDGE_CURVE ( 'NONE', #27100, #86567, #36934, .T. ) ;
#76815 = DIRECTION ( 'NONE',  ( -0.7071067811865486830, 0.7071067811865464625, 0.000000000000000000 ) ) ;
#76816 = DIRECTION ( 'NONE',  ( -0.000000000000000000, -0.3543493200069152693, 0.9351131265310292928 ) ) ;
#76817 = CARTESIAN_POINT ( 'NONE',  ( -51.18398860626899705, 28.73617430169823095, 5.000000000000000000 ) ) ;
#76818 = CARTESIAN_POINT ( 'NONE',  ( 124.8337635252314470, 6.110000000000001208, 1.122388791418549305E-15 ) ) ;
#76819 = PLANE ( 'NONE',  #116866 ) ;
#76820 = PRODUCT ( 'MAS-695', 'MAS-695', '', ( #38088 ) ) ;
#76821 = CARTESIAN_POINT ( 'NONE',  ( -34.92500000000001137, -22.22500000000000142, 4.000000000000000000 ) ) ;
#76823 = CARTESIAN_POINT ( 'NONE',  ( -63.29974487139158867, -27.71228299555250274, 4.000000000000000000 ) ) ;
#76822 = AXIS2_PLACEMENT_3D ( 'NONE', #130592, #74050, #118237 ) ;
#76824 = VECTOR ( 'NONE', #112508, 1000.000000000000000 ) ;
#76825 = DIRECTION ( 'NONE',  ( -0.6830127018922181881, 0.6830127018922202975, -0.2588190451025214056 ) ) ;
#76826 = SURFACE_STYLE_USAGE ( .BOTH. , #56521 ) ;
#76827 = CARTESIAN_POINT ( 'NONE',  ( -14.51078643762690490, -27.52281430457045275, 5.000000000000000000 ) ) ;
#76828 = DIRECTION ( 'NONE',  ( 0.7071067811865487940, -0.7071067811865463515, 0.000000000000000000 ) ) ;
#76829 = ADVANCED_FACE ( 'NONE', ( #70338 ), #16601, .F. ) ;
#76830 = AXIS2_PLACEMENT_3D ( 'NONE', #102123, #123887, #24542 ) ;
#76831 = ORIENTED_EDGE ( 'NONE', *, *, #64266, .F. ) ;
#76832 = ORIENTED_EDGE ( 'NONE', *, *, #118328, .T. ) ;
#76833 = ORIENTED_EDGE ( 'NONE', *, *, #76982, .F. ) ;
#76834 = AXIS2_PLACEMENT_3D ( 'NONE', #136534, #5995, #14771 ) ;
#76835 = DIRECTION ( 'NONE',  ( -0.3543493200069163240, -0.000000000000000000, -0.9351131265310288487 ) ) ;
#76836 = VERTEX_POINT ( 'NONE', #47172 ) ;
#76837 = ORIENTED_EDGE ( 'NONE', *, *, #92445, .F. ) ;
#76838 = CARTESIAN_POINT ( 'NONE',  ( 23.99999999999983302, 13.55218569542903140, 5.000000000000000000 ) ) ;
#76839 = CARTESIAN_POINT ( 'NONE',  ( 107.5583603837962414, -7.949999999999996625, -2.130196079827426203 ) ) ;
#76840 = EDGE_CURVE ( 'NONE', #19458, #34970, #68887, .T. ) ;
#76841 = LINE ( 'NONE', #21712, #935 ) ;
#76842 = CARTESIAN_POINT ( 'NONE',  ( -47.99451991528749062, 28.92564299267971251, 4.000000000000000000 ) ) ;
#76843 = ORIENTED_EDGE ( 'NONE', *, *, #117609, .T. ) ;
#76844 = PLANE ( 'NONE',  #27855 ) ;
#76845 = VECTOR ( 'NONE', #51556, 999.9999999999998863 ) ;
#76846 = VERTEX_POINT ( 'NONE', #13733 ) ;
#76847 =( NAMED_UNIT ( * ) SI_UNIT ( $, .STERADIAN. ) SOLID_ANGLE_UNIT ( ) );
#76848 = CARTESIAN_POINT ( 'NONE',  ( 18.58790314143521982, 6.871911579029515771, 3.967499999999989146 ) ) ;
#76849 = ORIENTED_EDGE ( 'NONE', *, *, #34176, .F. ) ;
#76850 = CARTESIAN_POINT ( 'NONE',  ( 86.24543019189812298, -5.291415217122919401, -3.055000000000000604 ) ) ;
#76851 = DIRECTION ( 'NONE',  ( -0.000000000000000000, -0.3543493200069152693, 0.9351131265310292928 ) ) ;
#76852 = DIRECTION ( 'NONE',  ( 1.000000000000000000, 0.000000000000000000, -0.000000000000000000 ) ) ;
#76853 = CARTESIAN_POINT ( 'NONE',  ( -27.52400138585429445, 22.03583458319438293, 4.979811245910086726 ) ) ;
#76854 = ORIENTED_EDGE ( 'NONE', *, *, #102361, .T. ) ;
#76855 = ORIENTED_EDGE ( 'NONE', *, *, #47697, .T. ) ;
#76856 = ORIENTED_EDGE ( 'NONE', *, *, #48538, .F. ) ;
#76857 = DIRECTION ( 'NONE',  ( 0.000000000000000000, 1.000000000000000000, 0.000000000000000000 ) ) ;
#76858 = CARTESIAN_POINT ( 'NONE',  ( 6.328169399223490643, 20.25929247661551003, 4.000000000000000000 ) ) ;
#76859 = CARTESIAN_POINT ( 'NONE',  ( 18.32816939922340183, -12.74070752338415247, 4.000000000000000000 ) ) ;
#76860 = VECTOR ( 'NONE', #17619, 999.9999999999998863 ) ;
#76862 = LINE ( 'NONE', #55813, #98316 ) ;
#76861 = VECTOR ( 'NONE', #5089, 999.9999999999998863 ) ;
#76863 = DIRECTION ( 'NONE',  ( -0.6830127018922180770, -0.6830127018922204085, -0.2588190451025213501 ) ) ;
#76864 = ORIENTED_EDGE ( 'NONE', *, *, #114822, .F. ) ;
#76865 = VECTOR ( 'NONE', #35998, 999.9999999999998863 ) ;
#76866 = CARTESIAN_POINT ( 'NONE',  ( 29.99999999999978328, -5.527737879153164613, -7.983877177622441756 ) ) ;
#76867 = AXIS2_PLACEMENT_3D ( 'NONE', #34889, #121147, #33474 ) ;
#76868 = EDGE_CURVE ( 'NONE', #62391, #100092, #92841, .T. ) ;
#76869 = LINE ( 'NONE', #12279, #76766 ) ;
#76870 = CARTESIAN_POINT ( 'NONE',  ( 6.183988606268994381, 28.73617430169791476, 5.000000000000000000 ) ) ;
#76871 = ORIENTED_EDGE ( 'NONE', *, *, #128583, .T. ) ;
#76872 = FILL_AREA_STYLE_COLOUR ( '', #21226 ) ;
#76873 = VECTOR ( 'NONE', #23723, 1000.000000000000000 ) ;
#76874 = CONICAL_SURFACE ( 'NONE', #86050, 2.500000000000000444, 0.9599310885968830309 ) ;
#76875 = CARTESIAN_POINT ( 'NONE',  ( -45.29974487139158867, -27.71228299555237840, 4.000000000000000000 ) ) ;
#76876 = ORIENTED_EDGE ( 'NONE', *, *, #43646, .T. ) ;
#76877 = EDGE_CURVE ( 'NONE', #137404, #34663, #80472, .T. ) ;
#76879 = ORIENTED_EDGE ( 'NONE', *, *, #32505, .F. ) ;
#76878 = CARTESIAN_POINT ( 'NONE',  ( 51.18398860626899705, 28.73617430169823095, 5.000000000000000000 ) ) ;
#76880 = ORIENTED_EDGE ( 'NONE', *, *, #43450, .T. ) ;
#76881 = EDGE_CURVE ( 'NONE', #140719, #119697, #118025, .T. ) ;
#76882 = LINE ( 'NONE', #134092, #53944 ) ;
#76883 = DIRECTION ( 'NONE',  ( -0.7071067811865486830, -0.7071067811865464625, -0.000000000000000000 ) ) ;
#76884 = ORIENTED_EDGE ( 'NONE', *, *, #88274, .T. ) ;
#76885 = DIRECTION ( 'NONE',  ( 0.6830127018922181881, 0.6830127018922202975, -0.2588190451025214056 ) ) ;
#76886 = LINE ( 'NONE', #74736, #31329 ) ;
#76887 = DIRECTION ( 'NONE',  ( 0.3543493200069162685, -0.000000000000000000, -0.9351131265310288487 ) ) ;
#76888 = DIRECTION ( 'NONE',  ( 1.000000000000000000, 0.000000000000000000, 0.000000000000000000 ) ) ;
#76889 = CARTESIAN_POINT ( 'NONE',  ( 30.75000000000000000, -9.735942053221458872E-16, 7.950000000000000178 ) ) ;
#76890 = CARTESIAN_POINT ( 'NONE',  ( 57.18398860626899705, 28.73617430169827358, 5.000000000000000000 ) ) ;
#76891 = DIRECTION ( 'NONE',  ( 0.6830127018922180770, -0.6830127018922204085, -0.2588190451025213501 ) ) ;
#76892 = FACE_OUTER_BOUND ( 'NONE', #44577, .T. ) ;
#76893 = LINE ( 'NONE', #97903, #87322 ) ;
#76894 = CARTESIAN_POINT ( 'NONE',  ( -7.940000000000007496, -35.76999999999998892, -10.00000000000000178 ) ) ;
#76895 = LINE ( 'NONE', #121068, #66853 ) ;
#76896 = CARTESIAN_POINT ( 'NONE',  ( -34.45011844616455221, 7.516280811637403581, 5.000000000000000888 ) ) ;
#76897 = DIRECTION ( 'NONE',  ( 0.7071067811865487940, 0.7071067811865463515, 0.000000000000000000 ) ) ;
#76898 = VERTEX_POINT ( 'NONE', #139125 ) ;
#76899 = EDGE_CURVE ( 'NONE', #71320, #57800, #107181, .T. ) ;
#76900 = VECTOR ( 'NONE', #140420, 1000.000000000000000 ) ;
#76901 = ORIENTED_EDGE ( 'NONE', *, *, #141278, .T. ) ;
#76902 = CARTESIAN_POINT ( 'NONE',  ( 104.5416666666666714, -3.975000000000002753, 6.884901960086286188 ) ) ;
#76903 = VECTOR ( 'NONE', #76412, 1000.000000000000000 ) ;
#76904 = ORIENTED_EDGE ( 'NONE', *, *, #24651, .T. ) ;
#76905 = ORIENTED_EDGE ( 'NONE', *, *, #141990, .F. ) ;
#76906 = AXIS2_PLACEMENT_3D ( 'NONE', #82013, #47264, #94263 ) ;
#76907 = EDGE_LOOP ( 'NONE', ( #129745, #123156, #106362, #121989 ) ) ;
#76908 = LINE ( 'NONE', #40686, #110524 ) ;
#76909 = DIRECTION ( 'NONE',  ( 0.6830127018922181881, 0.6830127018922202975, -0.2588190451025214056 ) ) ;
#76910 = AXIS2_PLACEMENT_3D ( 'NONE', #95413, #56057, #12503 ) ;
#76911 = ORIENTED_EDGE ( 'NONE', *, *, #95394, .F. ) ;
#76912 = CARTESIAN_POINT ( 'NONE',  ( -21.29974487139158512, -27.71228299555221142, 4.000000000000000000 ) ) ;
#76913 = CARTESIAN_POINT ( 'NONE',  ( -51.48921356237309510, -27.52281430457091460, 5.000000000000000000 ) ) ;
#76914 = DIRECTION ( 'NONE',  ( -1.000000000000000000, -0.000000000000000000, -0.000000000000000000 ) ) ;
#76915 = ORIENTED_EDGE ( 'NONE', *, *, #140662, .F. ) ;
#76916 = DIRECTION ( 'NONE',  ( 0.7071067811865486830, -0.7071067811865464625, -0.000000000000000000 ) ) ;
#76917 = CARTESIAN_POINT ( 'NONE',  ( 0.000000000000000000, 0.000000000000000000, 5.000000000000000000 ) ) ;
#76919 = VECTOR ( 'NONE', #59515, 1000.000000000000000 ) ;
#76918 = CARTESIAN_POINT ( 'NONE',  ( -0.7067925072407263976, 20.25929247661552068, 20.83292124670814971 ) ) ;
#76920 = FACE_OUTER_BOUND ( 'NONE', #126998, .T. ) ;
#76921 = CARTESIAN_POINT ( 'NONE',  ( 20.51078643762690490, -27.52281430457041012, 5.000000000000000000 ) ) ;
#76922 = CARTESIAN_POINT ( 'NONE',  ( 32.74586038379622011, 3.974999999999996980, 6.884901960086287964 ) ) ;
#76923 = DIRECTION ( 'NONE',  ( 0.7071067811865487940, 0.7071067811865463515, -0.000000000000000000 ) ) ;
#76924 = VERTEX_POINT ( 'NONE', #95594 ) ;
#76925 = ORIENTED_EDGE ( 'NONE', *, *, #138226, .F. ) ;
#76926 = EDGE_CURVE ( 'NONE', #8478, #12275, #18730, .T. ) ;
#76927 = CARTESIAN_POINT ( 'NONE',  ( 123.9587635252314470, 0.000000000000000000, -6.110000000000001208 ) ) ;
#76928 = ORIENTED_EDGE ( 'NONE', *, *, #125237, .T. ) ;
#76929 = FACE_OUTER_BOUND ( 'NONE', #109746, .T. ) ;
#76930 = EDGE_CURVE ( 'NONE', #15696, #27121, #66382, .T. ) ;
#76931 = VECTOR ( 'NONE', #40389, 999.9999999999998863 ) ;
#76932 = CARTESIAN_POINT ( 'NONE',  ( -24.18398860626899705, 28.73617430169804265, 5.000000000000000000 ) ) ;
#76933 = VECTOR ( 'NONE', #131235, 1000.000000000000000 ) ;
#76934 = FACE_OUTER_BOUND ( 'NONE', #33170, .T. ) ;
#76935 = EDGE_CURVE ( 'NONE', #81702, #81966, #135928, .T. ) ;
#76936 = EDGE_CURVE ( 'NONE', #133451, #14507, #96275, .T. ) ;
#76937 = PLANE ( 'NONE',  #25876 ) ;
#76938 = CARTESIAN_POINT ( 'NONE',  ( 50.99451991528749062, 28.92564299267973738, 4.000000000000000000 ) ) ;
#76939 = CARTESIAN_POINT ( 'NONE',  ( 115.1204301918981230, 3.055000000000001936, -5.291415217122916737 ) ) ;
#76940 = ORIENTED_EDGE ( 'NONE', *, *, #58747, .F. ) ;
#76941 = ORIENTED_EDGE ( 'NONE', *, *, #123131, .T. ) ;
#76942 = VECTOR ( 'NONE', #18871, 1000.000000000000000 ) ;
#76943 = DIRECTION ( 'NONE',  ( 1.000000000000000000, 0.000000000000000000, 0.000000000000000000 ) ) ;
#76944 = LINE ( 'NONE', #108070, #140408 ) ;
#76945 = ORIENTED_EDGE ( 'NONE', *, *, #120725, .T. ) ;
#76946 = EDGE_LOOP ( 'NONE', ( #77299, #95333, #100835, #130046 ) ) ;
#76948 = EDGE_CURVE ( 'NONE', #62248, #76248, #30344, .T. ) ;
#76947 = CARTESIAN_POINT ( 'NONE',  ( 38.06293019189810423, 1.637169565754157174, 6.110000000000002984 ) ) ;
#76949 = VERTEX_POINT ( 'NONE', #105733 ) ;
#76950 = DIRECTION ( 'NONE',  ( 0.7071067811865486830, -0.7071067811865464625, -0.000000000000000000 ) ) ;
#76951 = EDGE_CURVE ( 'NONE', #113958, #33777, #140520, .T. ) ;
#76952 = CARTESIAN_POINT ( 'NONE',  ( -55.65468426143998215, -25.33999999999998920, 13.17925390838734323 ) ) ;
#76953 = VECTOR ( 'NONE', #66196, 1000.000000000000227 ) ;
#76954 = EDGE_CURVE ( 'NONE', #62751, #66606, #107872, .T. ) ;
#76955 = CARTESIAN_POINT ( 'NONE',  ( 37.24543019189811588, -5.291415217122918513, -3.055000000000000160 ) ) ;
#76956 = ORIENTED_EDGE ( 'NONE', *, *, #105983, .T. ) ;
#76957 = CARTESIAN_POINT ( 'NONE',  ( 10.06000000000000050, 9.521314400968980422E-16, 0.000000000000000000 ) ) ;
#76958 = ORIENTED_EDGE ( 'NONE', *, *, #73067, .F. ) ;
#76959 = ORIENTED_EDGE ( 'NONE', *, *, #95678, .T. ) ;
#76961 = EDGE_CURVE ( 'NONE', #84037, #123150, #128940, .T. ) ;
#76960 = VECTOR ( 'NONE', #119432, 1000.000000000000227 ) ;
#76962 = AXIS2_PLACEMENT_3D ( 'NONE', #10118, #87686, #3498 ) ;
#76963 = EDGE_LOOP ( 'NONE', ( #32970, #102870, #85736, #93629 ) ) ;
#76964 = AXIS2_PLACEMENT_3D ( 'NONE', #138440, #39128, #127558 ) ;
#76965 = AXIS2_PLACEMENT_3D ( 'NONE', #136701, #114918, #49737 ) ;
#76966 = AXIS2_PLACEMENT_3D ( 'NONE', #11478, #55756, #99957 ) ;
#76967 = PLANE ( 'NONE',  #123254 ) ;
#76968 = ORIENTED_EDGE ( 'NONE', *, *, #46994, .F. ) ;
#76969 = CARTESIAN_POINT ( 'NONE',  ( -28.39656807105339453, -14.24070752338413648, 19.24067776001719210 ) ) ;
#76971 = CARTESIAN_POINT ( 'NONE',  ( 16.49999999999988987, -10.91253812416064406, 4.000000000000000000 ) ) ;
#76970 = VECTOR ( 'NONE', #110386, 1000.000000000000227 ) ;
#76972 = EDGE_CURVE ( 'NONE', #56350, #140092, #109085, .T. ) ;
#76973 = CIRCLE ( 'NONE', #111710, 3.000000000000000000 ) ;
#76974 = DIRECTION ( 'NONE',  ( -1.000000000000000000, -0.000000000000000000, 0.000000000000000000 ) ) ;
#76975 = CARTESIAN_POINT ( 'NONE',  ( 27.22000000000000242, -2.055000000000000160, 0.000000000000000000 ) ) ;
#76976 = FACE_BOUND ( 'NONE', #37571, .T. ) ;
#76977 = EDGE_LOOP ( 'NONE', ( #58864, #382, #46164 ) ) ;
#76978 = DIRECTION ( 'NONE',  ( -0.7071067811865486830, -0.7071067811865464625, 0.000000000000000000 ) ) ;
#76979 = CARTESIAN_POINT ( 'NONE',  ( -5.292893218813420120, -15.74070752338412760, 5.000000000000000000 ) ) ;
#76980 = CARTESIAN_POINT ( 'NONE',  ( 14.42840764549667476, -2.500000000000000888, 0.000000000000000000 ) ) ;
#76981 = ORIENTED_EDGE ( 'NONE', *, *, #10094, .F. ) ;
#76982 = EDGE_CURVE ( 'NONE', #6466, #31236, #77281, .T. ) ;
#76983 = CARTESIAN_POINT ( 'NONE',  ( -2.510786437626908008, -27.52281430457053446, 5.000000000000000000 ) ) ;
#76984 = ORIENTED_EDGE ( 'NONE', *, *, #132325, .F. ) ;
#76985 = EDGE_CURVE ( 'NONE', #26598, #128893, #73855, .T. ) ;
#76986 = ORIENTED_EDGE ( 'NONE', *, *, #10941, .F. ) ;
#76987 =( NAMED_UNIT ( * ) SI_UNIT ( $, .STERADIAN. ) SOLID_ANGLE_UNIT ( ) );
#76988 = ORIENTED_EDGE ( 'NONE', *, *, #84644, .F. ) ;
#76989 = EDGE_CURVE ( 'NONE', #70885, #121450, #128248, .T. ) ;
#76990 = CARTESIAN_POINT ( 'NONE',  ( 48.62043019189811588, 3.055000000000001936, -5.291415217122916737 ) ) ;
#76991 = VERTEX_POINT ( 'NONE', #17998 ) ;
#76992 = CARTESIAN_POINT ( 'NONE',  ( -29.20666063542132207, 21.75929247661549226, 4.998822639870711626 ) ) ;
#76993 = DIRECTION ( 'NONE',  ( 0.000000000000000000, 0.000000000000000000, 1.000000000000000000 ) ) ;
#76994 = LINE ( 'NONE', #109579, #118190 ) ;
#76995 = ORIENTED_EDGE ( 'NONE', *, *, #35308, .T. ) ;
#76996 = VECTOR ( 'NONE', #138121, 1000.000000000000000 ) ;
#76997 = FACE_OUTER_BOUND ( 'NONE', #54367, .T. ) ;
#76998 = CARTESIAN_POINT ( 'NONE',  ( 1.042387978378689573, 4.202752102959690472E-16, 0.000000000000000000 ) ) ;
#76999 = DIRECTION ( 'NONE',  ( 0.7071067811865487940, 0.7071067811865463515, 0.000000000000000000 ) ) ;
#77000 = CIRCLE ( 'NONE', #14470, 2.500000000000000444 ) ;
#77001 = PLANE ( 'NONE',  #65587 ) ;
#77002 = CARTESIAN_POINT ( 'NONE',  ( -8.999999999999932498, -3.033600742197707145, 5.000000000000000000 ) ) ;
#77003 = ORIENTED_EDGE ( 'NONE', *, *, #24289, .F. ) ;
#77004 = ORIENTED_EDGE ( 'NONE', *, *, #70888, .F. ) ;
#77005 = ORIENTED_EDGE ( 'NONE', *, *, #94890, .T. ) ;
#77006 = AXIS2_PLACEMENT_3D ( 'NONE', #122520, #100785, #35572 ) ;
#77007 = DIRECTION ( 'NONE',  ( 0.7071067811865486830, -0.7071067811865464625, -0.000000000000000000 ) ) ;
#77008 = DIRECTION ( 'NONE',  ( -0.7071067811865486830, -0.7071067811865464625, -0.000000000000000000 ) ) ;
#77009 = VERTEX_POINT ( 'NONE', #106435 ) ;
#77010 = ORIENTED_EDGE ( 'NONE', *, *, #39956, .F. ) ;
#77011 = CARTESIAN_POINT ( 'NONE',  ( 164.1998387378793893, 26.96999999999993491, -34.37854159432827572 ) ) ;
#77012 = CARTESIAN_POINT ( 'NONE',  ( 0.000000000000000000, 0.000000000000000000, 5.000000000000000000 ) ) ;
#77013 = DIRECTION ( 'NONE',  ( 0.7071067811865486830, -0.7071067811865464625, -0.000000000000000000 ) ) ;
#77014 = VERTEX_POINT ( 'NONE', #143212 ) ;
#77015 = DIRECTION ( 'NONE',  ( -0.3543493200069162685, -0.000000000000000000, -0.9351131265310288487 ) ) ;
#77016 = CARTESIAN_POINT ( 'NONE',  ( 16.76840764549667639, 3.061616997868385113E-16, -2.500000000000001332 ) ) ;
#77017 = CARTESIAN_POINT ( 'NONE',  ( 19.17123647476855197, 0.000000000000000000, 7.934999999999990727 ) ) ;
#77018 = CARTESIAN_POINT ( 'NONE',  ( 21.29159235450332233, 9.902892378096218942E-16, 0.000000000000000000 ) ) ;
#77019 = EDGE_LOOP ( 'NONE', ( #90790, #22253, #37167, #4765 ) ) ;
#77020 = CARTESIAN_POINT ( 'NONE',  ( 116.1412635252314374, 4.472830434245837594, 4.472830434245841147 ) ) ;
#77021 = CARTESIAN_POINT ( 'NONE',  ( 33.18398860626899705, 28.73617430169810305, 5.000000000000000000 ) ) ;
#77022 = VECTOR ( 'NONE', #90276, 1000.000000000000227 ) ;
#77023 = CARTESIAN_POINT ( 'NONE',  ( -34.42499999999997584, -21.76999999999999247, -0.5000000000000000000 ) ) ;
#77025 = EDGE_LOOP ( 'NONE', ( #41610, #18799, #89954, #58542 ) ) ;
#77024 = LINE ( 'NONE', #67577, #95791 ) ;
#77027 = VECTOR ( 'NONE', #7674, 999.9999999999998863 ) ;
#77026 = FACE_OUTER_BOUND ( 'NONE', #33837, .T. ) ;
#77028 = ORIENTED_EDGE ( 'NONE', *, *, #120717, .T. ) ;
#77029 = LINE ( 'NONE', #46564, #19649 ) ;
#77030 = DIRECTION ( 'NONE',  ( -0.7071067811865486830, 0.7071067811865464625, 0.000000000000000000 ) ) ;
#77031 = CARTESIAN_POINT ( 'NONE',  ( 7.499999999999947597, 12.43112307739205846, 4.000000000000000000 ) ) ;
#77032 = ORIENTED_EDGE ( 'NONE', *, *, #85898, .F. ) ;
#77033 = CARTESIAN_POINT ( 'NONE',  ( 25.39999999999999858, 7.464222240803104598E-16, -6.094999999999989093 ) ) ;
#77034 = CARTESIAN_POINT ( 'NONE',  ( -25.49999999999982947, 16.18958161055400069, -11.56426086740816928 ) ) ;
#77035 = VERTEX_POINT ( 'NONE', #39832 ) ;
#77036 = CIRCLE ( 'NONE', #120971, 0.5000000000000004441 ) ;
#77037 = LINE ( 'NONE', #21904, #50899 ) ;
#77038 = LINE ( 'NONE', #109629, #83997 ) ;
#77039 = ORIENTED_EDGE ( 'NONE', *, *, #5643, .T. ) ;
#77040 = CARTESIAN_POINT ( 'NONE',  ( 2.816011393730999401, 28.73617430169785436, 5.000000000000000000 ) ) ;
#77041 = ADVANCED_FACE ( 'NONE', ( #11231 ), #43914, .F. ) ;
#77043 = VERTEX_POINT ( 'NONE', #94160 ) ;
#77042 = LINE ( 'NONE', #56008, #108670 ) ;
#77045 = ORIENTED_EDGE ( 'NONE', *, *, #76222, .F. ) ;
#77044 = EDGE_CURVE ( 'NONE', #69770, #43467, #127518, .T. ) ;
#77046 = VECTOR ( 'NONE', #118954, 1000.000000000000227 ) ;
#77047 = DIRECTION ( 'NONE',  ( 0.6830127018922181881, 0.6830127018922202975, -0.2588190451025214056 ) ) ;
#77048 = DIRECTION ( 'NONE',  ( -0.3543493200069162685, -0.000000000000000000, -0.9351131265310288487 ) ) ;
#77049 = ORIENTED_EDGE ( 'NONE', *, *, #123629, .F. ) ;
#77050 = CARTESIAN_POINT ( 'NONE',  ( 17.22560490425083657, 3.821174125832445049E-16, 0.000000000000000000 ) ) ;
#77051 = DIRECTION ( 'NONE',  ( -0.000000000000000000, -0.3543493200069152693, 0.9351131265310292928 ) ) ;
#77052 = CARTESIAN_POINT ( 'NONE',  ( 24.29974487139158867, -27.71228299555223273, 4.000000000000000000 ) ) ;
#77053 = VERTEX_POINT ( 'NONE', #61582 ) ;
#77054 = EDGE_CURVE ( 'NONE', #36043, #32966, #73164, .T. ) ;
#77055 = CARTESIAN_POINT ( 'NONE',  ( 30.79289321881324426, 15.75929247661555976, 5.000000000000000000 ) ) ;
#77056 = DIRECTION ( 'NONE',  ( -0.7071067811865486830, -0.7071067811865464625, 0.000000000000000000 ) ) ;
#77057 = LINE ( 'NONE', #120486, #3056 ) ;
#77058 = VECTOR ( 'NONE', #67595, 999.9999999999998863 ) ;
#77059 = STYLED_ITEM ( 'NONE', ( #16086 ), #68458 ) ;
#77060 = CARTESIAN_POINT ( 'NONE',  ( 37.53709685856478018, -3.054999999999999272, -5.291415217122919401 ) ) ;
#77061 = DIRECTION ( 'NONE',  ( 1.000000000000000000, 0.000000000000000000, 0.000000000000000000 ) ) ;
#77062 = VECTOR ( 'NONE', #119754, 1000.000000000000000 ) ;
#77063 = EDGE_CURVE ( 'NONE', #100461, #58911, #84052, .T. ) ;
#77064 = AXIS2_PLACEMENT_3D ( 'NONE', #122778, #12583, #23465 ) ;
#77065 = VERTEX_POINT ( 'NONE', #113421 ) ;
#77066 = ORIENTED_EDGE ( 'NONE', *, *, #109631, .T. ) ;
#77067 = LINE ( 'NONE', #24089, #37366 ) ;
#77068 = ORIENTED_EDGE ( 'NONE', *, *, #86135, .T. ) ;
#77069 = VERTEX_POINT ( 'NONE', #46071 ) ;
#77070 = VECTOR ( 'NONE', #125206, 999.9999999999998863 ) ;
#77071 = CARTESIAN_POINT ( 'NONE',  ( 11.99999999999991651, 2.966399257802230682, 5.000000000000000000 ) ) ;
#77072 = CARTESIAN_POINT ( 'NONE',  ( -15.18398860626900237, 28.73617430169797871, 5.000000000000000000 ) ) ;
#77073 = EDGE_CURVE ( 'NONE', #47703, #29768, #69928, .T. ) ;
#77074 = VERTEX_POINT ( 'NONE', #67841 ) ;
#77075 = DIRECTION ( 'NONE',  ( -0.7071067811865486830, -0.7071067811865464625, 0.000000000000000000 ) ) ;
#77076 = CARTESIAN_POINT ( 'NONE',  ( 19.04500000000000881, 3.130000000000007887, -2.396719511207313368E-16 ) ) ;
#77077 = PLANE ( 'NONE',  #99541 ) ;
#77078 = DIRECTION ( 'NONE',  ( -0.6830127018922180770, -0.6830127018922204085, -0.2588190451025213501 ) ) ;
#77079 = CARTESIAN_POINT ( 'NONE',  ( 117.6879301918981184, 6.110000000000002984, -1.637169565754156730 ) ) ;
#77080 = ORIENTED_EDGE ( 'NONE', *, *, #10457, .F. ) ;
#77081 = FACE_OUTER_BOUND ( 'NONE', #17807, .T. ) ;
#77082 = CARTESIAN_POINT ( 'NONE',  ( -50.99451991528749062, 28.92564299267973738, 4.000000000000000000 ) ) ;
#77083 = EDGE_CURVE ( 'NONE', #120068, #7267, #135905, .T. ) ;
#77084 = LINE ( 'NONE', #45879, #114401 ) ;
#77085 = CARTESIAN_POINT ( 'NONE',  ( -62.99451991528749772, 28.92564299267982264, 4.000000000000000000 ) ) ;
#77086 = LINE ( 'NONE', #43711, #121444 ) ;
#77087 = LINE ( 'NONE', #9629, #93160 ) ;
#77088 = DIRECTION ( 'NONE',  ( -1.000000000000000000, 0.000000000000000000, 0.000000000000000000 ) ) ;
#77089 = CARTESIAN_POINT ( 'NONE',  ( 61.03752705046289151, -9.735942053221456900E-16, 7.949999999999998401 ) ) ;
#77090 = PLANE ( 'NONE',  #32928 ) ;
#77092 = FACE_OUTER_BOUND ( 'NONE', #89844, .T. ) ;
#77091 = VECTOR ( 'NONE', #107673, 1000.000000000000000 ) ;
#77093 = VERTEX_POINT ( 'NONE', #12680 ) ;
#77094 = VERTEX_POINT ( 'NONE', #24291 ) ;
#77095 = CARTESIAN_POINT ( 'NONE',  ( 45.47916666666665719, -7.950000000000001066, 2.130196079827424427 ) ) ;
#77096 = CARTESIAN_POINT ( 'NONE',  ( 27.29974487139158512, -27.71228299555225405, 4.000000000000000000 ) ) ;
#77097 = ADVANCED_FACE ( 'NONE', ( #25706 ), #36580, .T. ) ;
#77098 = CARTESIAN_POINT ( 'NONE',  ( 3.005480084712505828, 28.92564299267936079, 4.000000000000000000 ) ) ;
#77099 = ORIENTED_EDGE ( 'NONE', *, *, #51236, .F. ) ;
#77100 = CARTESIAN_POINT ( 'NONE',  ( 45.18398860626900415, 28.73617430169818832, 5.000000000000000000 ) ) ;
#77101 = AXIS2_PLACEMENT_3D ( 'NONE', #82508, #128166, #6305 ) ;
#77103 = ADVANCED_FACE ( 'NONE', ( #33767 ), #30457, .T. ) ;
#77102 = DIRECTION ( 'NONE',  ( -0.000000000000000000, -0.3543493200069152693, 0.9351131265310292928 ) ) ;
#77104 = ADVANCED_FACE ( 'NONE', ( #14106 ), #124311, .T. ) ;
#77105 = CARTESIAN_POINT ( 'NONE',  ( 35.14626352523143993, -4.472830434245840259, 4.472830434245839371 ) ) ;
#77106 = VECTOR ( 'NONE', #19925, 1000.000000000000227 ) ;
#77107 = ORIENTED_EDGE ( 'NONE', *, *, #32275, .T. ) ;
#77108 = DIRECTION ( 'NONE',  ( -1.000000000000000000, 0.000000000000000000, 0.000000000000000000 ) ) ;
#77109 = ORIENTED_EDGE ( 'NONE', *, *, #124211, .T. ) ;
#77110 = ORIENTED_EDGE ( 'NONE', *, *, #113838, .F. ) ;
#77111 = AXIS2_PLACEMENT_3D ( 'NONE', #65155, #120178, #32511 ) ;
#77112 = CARTESIAN_POINT ( 'NONE',  ( 5.999999999999956479, -7.068876922607745250, 4.000000000000000000 ) ) ;
#77113 = EDGE_CURVE ( 'NONE', #82515, #70432, #37392, .T. ) ;
#77114 = LINE ( 'NONE', #8214, #103249 ) ;
#77115 = CARTESIAN_POINT ( 'NONE',  ( 34.82816939922329880, -17.24070752338409562, 4.000000000000000000 ) ) ;
#77116 = CARTESIAN_POINT ( 'NONE',  ( 66.48921356237309510, -27.52281430457101763, 5.000000000000000000 ) ) ;
#77117 = EDGE_LOOP ( 'NONE', ( #100093, #103917, #82480, #21853 ) ) ;
#77118 = ADVANCED_FACE ( 'NONE', ( #88859 ), #90999, .F. ) ;
#77119 = DIRECTION ( 'NONE',  ( 0.000000000000000000, 1.000000000000000000, 0.000000000000000000 ) ) ;
#77121 = VERTEX_POINT ( 'NONE', #135223 ) ;
#77120 = CARTESIAN_POINT ( 'NONE',  ( 9.087472949537108491, -6.094999999999989981, 3.732111120401553285E-16 ) ) ;
#77122 = CARTESIAN_POINT ( 'NONE',  ( 78.31293019189811844, -1.637169565754159617, -6.110000000000001208 ) ) ;
#77123 = EDGE_CURVE ( 'NONE', #73032, #26933, #79439, .T. ) ;
#77124 = CARTESIAN_POINT ( 'NONE',  ( 14.70692117890024697, 4.584330080086930965E-16, 0.000000000000000000 ) ) ;
#77125 = CARTESIAN_POINT ( 'NONE',  ( 0.000000000000000000, 0.000000000000000000, 0.000000000000000000 ) ) ;
#77126 = LINE ( 'NONE', #65544, #30053 ) ;
#77127 = VECTOR ( 'NONE', #126746, 1000.000000000000000 ) ;
#77128 = VERTEX_POINT ( 'NONE', #56256 ) ;
#77129 = ADVANCED_FACE ( 'NONE', ( #1083 ), #69238, .T. ) ;
#77130 = FACE_OUTER_BOUND ( 'NONE', #125196, .T. ) ;
#77131 = CARTESIAN_POINT ( 'NONE',  ( 63.93293019189812298, 1.637169565754156508, 6.110000000000000320 ) ) ;
#77132 = LINE ( 'NONE', #66239, #27885 ) ;
#77133 = VECTOR ( 'NONE', #113283, 1000.000000000000000 ) ;
#77134 = CARTESIAN_POINT ( 'NONE',  ( -18.15612307739227660, -22.22499999999999432, 4.000000000000000000 ) ) ;
#77135 = CARTESIAN_POINT ( 'NONE',  ( 54.48921356237310221, -27.52281430457093236, 5.000000000000000000 ) ) ;
#77136 = ORIENTED_EDGE ( 'NONE', *, *, #71843, .F. ) ;
#77137 = ORIENTED_EDGE ( 'NONE', *, *, #61436, .T. ) ;
#77138 = CIRCLE ( 'NONE', #61007, 6.000000000000000000 ) ;
#77139 = CARTESIAN_POINT ( 'NONE',  ( 9.370933818357753964, 3.821174125832445049E-16, 0.000000000000000000 ) ) ;
#77140 = EDGE_CURVE ( 'NONE', #124621, #36518, #102584, .T. ) ;
#77141 = ORIENTED_EDGE ( 'NONE', *, *, #121744, .F. ) ;
#77142 =( BOUNDED_CURVE ( )  B_SPLINE_CURVE ( 3, ( #140057, #128459, #41426, #52302 ),
 .UNSPECIFIED., .F., .F. ) 
 B_SPLINE_CURVE_WITH_KNOTS ( ( 4, 4 ),
 ( 5.005968288816727174, 5.074607125596338086 ),
 .UNSPECIFIED. ) 
 CURVE ( )  GEOMETRIC_REPRESENTATION_ITEM ( )  RATIONAL_B_SPLINE_CURVE ( ( 1.000000000000000000, 0.9996074310407765395, 0.9996074310407765395, 1.000000000000000000 ) ) 
 REPRESENTATION_ITEM ( '' )  );
#77143 = VERTEX_POINT ( 'NONE', #45366 ) ;
#77144 = LINE ( 'NONE', #98155, #60667 ) ;
#77145 = VERTEX_POINT ( 'NONE', #80831 ) ;
#77146 = CARTESIAN_POINT ( 'NONE',  ( -30.18398860626900060, 28.73617430169808173, 5.000000000000000000 ) ) ;
#77147 = DIRECTION ( 'NONE',  ( -1.000000000000000000, -1.224606353822377258E-16, -0.000000000000000000 ) ) ;
#77148 = AXIS2_PLACEMENT_3D ( 'NONE', #135699, #56753, #36385 ) ;
#77149 =( BOUNDED_CURVE ( )  B_SPLINE_CURVE ( 3, ( #100963, #1618, #112563, #101678 ),
 .UNSPECIFIED., .F., .F. ) 
 B_SPLINE_CURVE_WITH_KNOTS ( ( 4, 4 ),
 ( 4.712388980384689674, 6.283185307179586232 ),
 .UNSPECIFIED. ) 
 CURVE ( )  GEOMETRIC_REPRESENTATION_ITEM ( )  RATIONAL_B_SPLINE_CURVE ( ( 1.000000000000000000, 0.8047378541243649375, 0.8047378541243649375, 1.000000000000000000 ) ) 
 REPRESENTATION_ITEM ( '' )  );
#77150 = CARTESIAN_POINT ( 'NONE',  ( 0.9387690737794645024, 0.3999999999999995781, 2.166563419957292957 ) ) ;
#77151 = FACE_BOUND ( 'NONE', #50066, .T. ) ;
#77152 = FACE_OUTER_BOUND ( 'NONE', #131087, .T. ) ;
#77153 = DIRECTION ( 'NONE',  ( -0.000000000000000000, -0.000000000000000000, 1.000000000000000000 ) ) ;
#77154 = CIRCLE ( 'NONE', #88731, 2.500000000000000444 ) ;
#77155 = CARTESIAN_POINT ( 'NONE',  ( 0.000000000000000000, 0.000000000000000000, 0.000000000000000000 ) ) ;
#77156 = ORIENTED_EDGE ( 'NONE', *, *, #130827, .T. ) ;
#77157 = PLANE ( 'NONE',  #106552 ) ;
#77158 = EDGE_LOOP ( 'NONE', ( #98837, #5460, #107198, #74734 ) ) ;
#77159 = ADVANCED_FACE ( 'NONE', ( #67093 ), #111277, .F. ) ;
#77160 = EDGE_CURVE ( 'NONE', #7890, #85293, #42062, .T. ) ;
#77161 = ORIENTED_EDGE ( 'NONE', *, *, #128289, .F. ) ;
#77162 = CARTESIAN_POINT ( 'NONE',  ( 73.26626352523143737, 4.472830434245838482, -4.472830434245837594 ) ) ;
#77163 = ORIENTED_EDGE ( 'NONE', *, *, #106659, .F. ) ;
#77164 = DIRECTION ( 'NONE',  ( -1.000000000000000000, -1.224606353822377258E-16, -0.000000000000000000 ) ) ;
#77165 = DIRECTION ( 'NONE',  ( 0.6830127018922181881, 0.6830127018922202975, -0.2588190451025214056 ) ) ;
#77166 = ORIENTED_EDGE ( 'NONE', *, *, #41911, .T. ) ;
#77167 = DIRECTION ( 'NONE',  ( -0.7071067811865486830, 0.7071067811865464625, 0.000000000000000000 ) ) ;
#77168 = VECTOR ( 'NONE', #104999, 1000.000000000000114 ) ;
#77169 = VECTOR ( 'NONE', #50061, 1000.000000000000000 ) ;
#77170 = CARTESIAN_POINT ( 'NONE',  ( 121.8958333333333286, -2.130196079827399558, 7.950000000000016165 ) ) ;
#77171 = DIRECTION ( 'NONE',  ( -0.000000000000000000, -0.000000000000000000, -1.000000000000000000 ) ) ;
#77172 = CARTESIAN_POINT ( 'NONE',  ( 52.60764783923757193, -52.00875322212550600, 39.33676470588235219 ) ) ;
#77173 = LINE ( 'NONE', #8964, #32020 ) ;
#77174 = FACE_OUTER_BOUND ( 'NONE', #97774, .T. ) ;
#77175 = DIRECTION ( 'NONE',  ( -0.3543493200069163240, 0.000000000000000000, -0.9351131265310288487 ) ) ;
#77176 = ORIENTED_EDGE ( 'NONE', *, *, #69066, .F. ) ;
#77177 = AXIS2_PLACEMENT_3D ( 'NONE', #50262, #138704, #39388 ) ;
#77178 = AXIS2_PLACEMENT_3D ( 'NONE', #13428, #14879, #101174 ) ;
#77179 = LINE ( 'NONE', #120618, #9792 ) ;
#77180 = ORIENTED_EDGE ( 'NONE', *, *, #71181, .F. ) ;
#77181 = CARTESIAN_POINT ( 'NONE',  ( 31.92500000000001492, -3.269999999999992468, -37.00000000000000000 ) ) ;
#77182 = VECTOR ( 'NONE', #140777, 1000.000000000000227 ) ;
#77183 = ORIENTED_EDGE ( 'NONE', *, *, #133552, .T. ) ;
#77184 = ORIENTED_EDGE ( 'NONE', *, *, #64760, .T. ) ;
#77185 = CARTESIAN_POINT ( 'NONE',  ( 28.43793019189810423, -6.110000000000001208, 1.637169565754158951 ) ) ;
#77186 = ORIENTED_EDGE ( 'NONE', *, *, #44479, .T. ) ;
#77187 = DIRECTION ( 'NONE',  ( -0.7071067811865486830, 0.7071067811865464625, 0.000000000000000000 ) ) ;
#77188 = CARTESIAN_POINT ( 'NONE',  ( -2.700255128608413990, -27.71228299555204089, 4.000000000000000000 ) ) ;
#77189 = VECTOR ( 'NONE', #78466, 1000.000000000000000 ) ;
#77190 = CARTESIAN_POINT ( 'NONE',  ( 23.52497294953710849, -4.461849672132299993, -4.461849672132299105 ) ) ;
#77191 = LINE ( 'NONE', #79350, #107434 ) ;
#77192 = ORIENTED_EDGE ( 'NONE', *, *, #51685, .F. ) ;
#77193 = DIRECTION ( 'NONE',  ( -0.000000000000000000, 0.000000000000000000, 1.000000000000000000 ) ) ;
#77194 = ORIENTED_EDGE ( 'NONE', *, *, #98533, .T. ) ;
#77196 = EDGE_CURVE ( 'NONE', #111882, #15565, #112029, .T. ) ;
#77195 =( NAMED_UNIT ( * ) PLANE_ANGLE_UNIT ( ) SI_UNIT ( $, .RADIAN. ) );
#77197 = PLANE ( 'NONE',  #28967 ) ;
#77199 = ORIENTED_EDGE ( 'NONE', *, *, #95577, .F. ) ;
#77198 = DIRECTION ( 'NONE',  ( 0.6830127018922181881, 0.6830127018922202975, -0.2588190451025214056 ) ) ;
#77200 = ORIENTED_EDGE ( 'NONE', *, *, #141052, .F. ) ;
#77201 = DIRECTION ( 'NONE',  ( -0.6830127018922181881, 0.6830127018922202975, -0.2588190451025214056 ) ) ;
#77202 = CARTESIAN_POINT ( 'NONE',  ( -12.20000000000000107, -34.51840020119762187, 17.97447928118982929 ) ) ;
#77203 = VECTOR ( 'NONE', #20622, 1000.000000000000000 ) ;
#77204 = ORIENTED_EDGE ( 'NONE', *, *, #135385, .T. ) ;
#77205 = DIRECTION ( 'NONE',  ( -0.000000000000000000, 0.000000000000000000, 1.000000000000000000 ) ) ;
#77206 = ORIENTED_EDGE ( 'NONE', *, *, #14967, .T. ) ;
#77207 = VECTOR ( 'NONE', #100360, 1000.000000000000000 ) ;
#77208 = CARTESIAN_POINT ( 'NONE',  ( 12.18398860626900060, 28.73617430169795739, 5.000000000000000000 ) ) ;
#77209 = CARTESIAN_POINT ( 'NONE',  ( 34.92499999999998295, 11.81665438641033106, 4.500000000000000888 ) ) ;
#77210 = PLANE ( 'NONE',  #50795 ) ;
#77211 = CARTESIAN_POINT ( 'NONE',  ( 8.811592354503320124, -5.777789833161707559E-31, 2.500000000000001332 ) ) ;
#77213 = VECTOR ( 'NONE', #135850, 999.9999999999998863 ) ;
#77212 = CARTESIAN_POINT ( 'NONE',  ( 48.18398860626899705, 28.73617430169820608, 5.000000000000000000 ) ) ;
#77214 = EDGE_CURVE ( 'NONE', #63923, #25547, #46761, .T. ) ;
#77215 = CARTESIAN_POINT ( 'NONE',  ( 5.292893218813423672, -12.74070752338415247, 5.000000000000000000 ) ) ;
#77216 = DIRECTION ( 'NONE',  ( 1.000000000000000000, 1.224606353822377258E-16, 0.000000000000000000 ) ) ;
#77217 = EDGE_CURVE ( 'NONE', #99583, #75231, #50331, .T. ) ;
#77219 = ORIENTED_EDGE ( 'NONE', *, *, #8112, .F. ) ;
#77218 = EDGE_CURVE ( 'NONE', #28732, #9245, #59789, .T. ) ;
#77220 = DIRECTION ( 'NONE',  ( 0.3543493200069162685, -0.000000000000000000, -0.9351131265310288487 ) ) ;
#77221 = ORIENTED_EDGE ( 'NONE', *, *, #141493, .T. ) ;
#77222 = LINE ( 'NONE', #31548, #21634 ) ;
#77224 = EDGE_CURVE ( 'NONE', #33411, #19554, #14830, .T. ) ;
#77223 = VECTOR ( 'NONE', #48974, 1000.000000000000114 ) ;
#77225 = EDGE_CURVE ( 'NONE', #70402, #137770, #127154, .T. ) ;
#77226 = CARTESIAN_POINT ( 'NONE',  ( 26.40000000000000568, -16.48000000000005016, -33.92499999999998295 ) ) ;
#77227 = DIRECTION ( 'NONE',  ( 1.000000000000000000, 0.000000000000000000, 0.000000000000000000 ) ) ;
#77229 = ORIENTED_EDGE ( 'NONE', *, *, #35869, .T. ) ;
#77228 = AXIS2_PLACEMENT_3D ( 'NONE', #71485, #7621, #16344 ) ;
#77230 = CARTESIAN_POINT ( 'NONE',  ( 21.18398860626899349, 28.73617430169802134, 5.000000000000000000 ) ) ;
#77231 = CARTESIAN_POINT ( 'NONE',  ( 16.49999999999988276, -17.56887692260763956, 4.000000000000000000 ) ) ;
#77232 = LINE ( 'NONE', #66342, #120790 ) ;
#77233 = ORIENTED_EDGE ( 'NONE', *, *, #22533, .F. ) ;
#77234 = EDGE_CURVE ( 'NONE', #111457, #103339, #26434, .T. ) ;
#77235 = DIRECTION ( 'NONE',  ( 0.6830127018922180770, -0.6830127018922204085, -0.2588190451025213501 ) ) ;
#77236 = CARTESIAN_POINT ( 'NONE',  ( 111.6875000000000000, -5.819803920172573974, 5.819803920172573086 ) ) ;
#77237 = LINE ( 'NONE', #55460, #35398 ) ;
#77238 = PRESENTATION_LAYER_ASSIGNMENT (  '', '', ( #111990 ) ) ;
#77239 = FILL_AREA_STYLE_COLOUR ( '', #123858 ) ;
#77240 = PLANE ( 'NONE',  #69072 ) ;
#77241 = CARTESIAN_POINT ( 'NONE',  ( 62.18293019189812298, -1.637169565754159173, -6.109999999999999432 ) ) ;
#77242 = FACE_OUTER_BOUND ( 'NONE', #59473, .T. ) ;
#77243 = EDGE_CURVE ( 'NONE', #75031, #10935, #16985, .T. ) ;
#77244 = LINE ( 'NONE', #45330, #131841 ) ;
#77245 = CARTESIAN_POINT ( 'NONE',  ( -1.499999999999987566, 0.4497235411627421575, -5.599840258123544245 ) ) ;
#77246 = LINE ( 'NONE', #22095, #69624 ) ;
#77247 = ORIENTED_EDGE ( 'NONE', *, *, #103549, .T. ) ;
#77248 = CARTESIAN_POINT ( 'NONE',  ( 31.17183060077625356, 12.75929247661558286, 4.000000000000000000 ) ) ;
#77249 = ORIENTED_EDGE ( 'NONE', *, *, #136603, .F. ) ;
#77250 = STYLED_ITEM ( 'NONE', ( #46749 ), #81158 ) ;
#77251 = CARTESIAN_POINT ( 'NONE',  ( -20.99999999999985789, -8.151047557385087572, -8.977947279169748995 ) ) ;
#77252 = LINE ( 'NONE', #43174, #56947 ) ;
#77253 = EDGE_CURVE ( 'NONE', #36177, #77939, #109196, .T. ) ;
#77254 = DIRECTION ( 'NONE',  ( -0.000000000000000000, 1.000000000000000000, -0.000000000000000000 ) ) ;
#77255 = DIRECTION ( 'NONE',  ( -1.000000000000000000, 0.000000000000000000, 0.000000000000000000 ) ) ;
#77256 = LINE ( 'NONE', #33741, #69366 ) ;
#77257 = CARTESIAN_POINT ( 'NONE',  ( -34.45011844616454511, 13.51628081163733874, 5.000000000000000888 ) ) ;
#77258 = DIRECTION ( 'NONE',  ( -0.000000000000000000, 0.000000000000000000, 1.000000000000000000 ) ) ;
#77259 = EDGE_LOOP ( 'NONE', ( #83189, #135690, #27664, #25562 ) ) ;
#77261 = ORIENTED_EDGE ( 'NONE', *, *, #128318, .F. ) ;
#77260 = AXIS2_PLACEMENT_3D ( 'NONE', #142533, #120010, #43220 ) ;
#77262 = LINE ( 'NONE', #121430, #74190 ) ;
#77263 = EDGE_CURVE ( 'NONE', #5121, #142121, #136604, .T. ) ;
#77264 = DIRECTION ( 'NONE',  ( 0.3543493200069163240, 0.000000000000000000, -0.9351131265310288487 ) ) ;
#77265 = DIRECTION ( 'NONE',  ( 0.000000000000000000, 0.000000000000000000, 1.000000000000000000 ) ) ;
#77266 = CARTESIAN_POINT ( 'NONE',  ( 86.85002705046289861, -5.819803920172572198, -5.819803920172572198 ) ) ;
#77267 = LINE ( 'NONE', #109855, #143485 ) ;
#77268 = VECTOR ( 'NONE', #68619, 1000.000000000000000 ) ;
#77269 = LINE ( 'NONE', #52613, #76163 ) ;
#77270 = ORIENTED_EDGE ( 'NONE', *, *, #34201, .F. ) ;
#77271 = CARTESIAN_POINT ( 'NONE',  ( 71.87500000000000000, 7.950000000000000178, 1.460391307983218535E-15 ) ) ;
#77272 = CARTESIAN_POINT ( 'NONE',  ( 25.49999999999982947, -20.94781430457061333, 5.000000000000000000 ) ) ;
#77273 = LINE ( 'NONE', #85971, #92391 ) ;
#77274 = PLANE ( 'NONE',  #19647 ) ;
#77275 = EDGE_CURVE ( 'NONE', #36187, #79492, #61938, .T. ) ;
#77276 = VERTEX_POINT ( 'NONE', #48913 ) ;
#77277 = AXIS2_PLACEMENT_3D ( 'NONE', #130992, #52686, #20772 ) ;
#77278 = DIRECTION ( 'NONE',  ( -0.000000000000000000, 0.3543493200069153248, 0.9351131265310292928 ) ) ;
#77279 = ADVANCED_FACE ( 'NONE', ( #6059 ), #48185, .T. ) ;
#77280 = ORIENTED_EDGE ( 'NONE', *, *, #59863, .T. ) ;
#77281 = LINE ( 'NONE', #121452, #44241 ) ;
#77282 = CARTESIAN_POINT ( 'NONE',  ( 76.41709685856476142, 3.054999999999998828, 5.291415217122922066 ) ) ;
#77283 = EDGE_CURVE ( 'NONE', #105795, #61439, #126644, .T. ) ;
#77284 = DIRECTION ( 'NONE',  ( -0.7071067811865486830, -0.7071067811865464625, 0.000000000000000000 ) ) ;
#77285 = ORIENTED_EDGE ( 'NONE', *, *, #81199, .F. ) ;
#77286 = DIRECTION ( 'NONE',  ( 0.6830127018922181881, 0.6830127018922202975, -0.2588190451025214056 ) ) ;
#77287 = EDGE_CURVE ( 'NONE', #31893, #135641, #72844, .T. ) ;
#77288 = CARTESIAN_POINT ( 'NONE',  ( 3.299744871391591339, -27.71228299555208352, 4.000000000000000000 ) ) ;
#77289 = DIRECTION ( 'NONE',  ( 0.7071067811865487940, 0.7071067811865463515, -0.000000000000000000 ) ) ;
#77290 = CARTESIAN_POINT ( 'NONE',  ( 42.29974487139158157, -27.71228299555235708, 4.000000000000000000 ) ) ;
#77291 = PLANE ( 'NONE',  #81040 ) ;
#77293 = ORIENTED_EDGE ( 'NONE', *, *, #10680, .T. ) ;
#77292 = CARTESIAN_POINT ( 'NONE',  ( 127.0000000000000000, 1.664417612029487348, 6.163512901498443775 ) ) ;
#77294 =( REPRESENTATION_RELATIONSHIP ('NONE','NONE', #69070, #88538 ) REPRESENTATION_RELATIONSHIP_WITH_TRANSFORMATION ( #22011 )SHAPE_REPRESENTATION_RELATIONSHIP( ) );
#77295 = CARTESIAN_POINT ( 'NONE',  ( -15.12147316337138214, -20.24070752338408141, 7.412974875817823772 ) ) ;
#77296 = CARTESIAN_POINT ( 'NONE',  ( -21.46160355370557582, -9.740707523384180888, 17.74957260769605938 ) ) ;
#77297 = AXIS2_PLACEMENT_3D ( 'NONE', #6646, #119019, #119702 ) ;
#77298 = DIRECTION ( 'NONE',  ( -0.7071067811865486830, -0.7071067811865464625, 0.000000000000000000 ) ) ;
#77299 = ORIENTED_EDGE ( 'NONE', *, *, #96963, .T. ) ;
#77300 = ORIENTED_EDGE ( 'NONE', *, *, #27077, .F. ) ;
#77301 = CARTESIAN_POINT ( 'NONE',  ( 63.00043019189810423, -3.055000000000002380, 5.291415217122920289 ) ) ;
#77302 = VECTOR ( 'NONE', #121063, 1000.000000000000000 ) ;
#77303 = EDGE_LOOP ( 'NONE', ( #134146, #95247, #50790, #131952 ) ) ;
#77304 = EDGE_CURVE ( 'NONE', #96600, #41872, #7357, .T. ) ;
#77305 = CARTESIAN_POINT ( 'NONE',  ( 21.79289321881330466, 12.75929247661559351, 5.000000000000000000 ) ) ;
#77306 = CARTESIAN_POINT ( 'NONE',  ( -20.99999999999985079, -0.2811185226894475919, -5.995736974527464902 ) ) ;
#77307 = CARTESIAN_POINT ( 'NONE',  ( -34.42500000000001137, -22.22500000000000142, 5.000000000000000000 ) ) ;
#77308 = PLANE ( 'NONE',  #10921 ) ;
#77309 = DIRECTION ( 'NONE',  ( 1.000000000000000000, -0.000000000000000000, 0.000000000000000000 ) ) ;
#77310 = ORIENTED_EDGE ( 'NONE', *, *, #18036, .T. ) ;
#77311 = EDGE_LOOP ( 'NONE', ( #64131, #96861, #62181, #107658 ) ) ;
#77312 = DIRECTION ( 'NONE',  ( -0.7071067811865487940, 0.7071067811865463515, -0.000000000000000000 ) ) ;
#77313 = DIRECTION ( 'NONE',  ( 0.7071067811865486830, -0.7071067811865464625, -0.000000000000000000 ) ) ;
#77314 = VECTOR ( 'NONE', #24913, 1000.000000000000000 ) ;
#77315 = VERTEX_POINT ( 'NONE', #114832 ) ;
#77316 = EDGE_CURVE ( 'NONE', #87614, #131559, #15508, .T. ) ;
#77317 = VECTOR ( 'NONE', #47287, 1000.000000000000000 ) ;
#77319 = AXIS2_PLACEMENT_3D ( 'NONE', #86543, #100264, #64065 ) ;
#77318 = DIRECTION ( 'NONE',  ( 0.3543493200069162685, -0.000000000000000000, -0.9351131265310288487 ) ) ;
#77320 = CARTESIAN_POINT ( 'NONE',  ( -0.1839886062690032631, 28.73617430169787568, 5.000000000000000000 ) ) ;
#77321 = DIRECTION ( 'NONE',  ( 0.000000000000000000, 1.000000000000000000, 0.000000000000000000 ) ) ;
#77322 = ORIENTED_EDGE ( 'NONE', *, *, #88400, .F. ) ;
#77323 = VECTOR ( 'NONE', #137753, 1000.000000000000000 ) ;
#77324 = EDGE_CURVE ( 'NONE', #62339, #79834, #5363, .T. ) ;
#77325 = DIRECTION ( 'NONE',  ( -0.7071067811865486830, 0.7071067811865464625, 0.000000000000000000 ) ) ;
#77326 = LINE ( 'NONE', #119337, #22266 ) ;
#77327 = DIRECTION ( 'NONE',  ( -0.7071067811865486830, -0.7071067811865464625, 0.000000000000000000 ) ) ;
#77328 = PLANE ( 'NONE',  #89972 ) ;
#77330 = VECTOR ( 'NONE', #50469, 1000.000000000000000 ) ;
#77329 = LINE ( 'NONE', #58450, #64239 ) ;
#77331 =( BOUNDED_CURVE ( )  B_SPLINE_CURVE ( 2, ( #86462, #110308, #31360, #130689, #107475, #63986, #118340, #108156, #75581, #119751, #43651, #97275, #76297 ),
 .UNSPECIFIED., .F., .T. ) 
 B_SPLINE_CURVE_WITH_KNOTS ( ( 3, 2, 2, 2, 2, 2, 3 ),
 ( 0.5833333333333333703, 0.5861111111111111382, 0.5888888888888889062, 0.5916666666666666741, 0.5944444444444444420, 0.5972222222222222099, 0.5999999999999999778 ),
 .UNSPECIFIED. ) 
 CURVE ( )  GEOMETRIC_REPRESENTATION_ITEM ( )  RATIONAL_B_SPLINE_CURVE ( ( 1.000000000000000000, 0.9659258262890683122, 1.000000000000000000, 0.9659258262890683122, 1.000000000000000000, 0.9659258262890683122, 1.000000000000000000, 0.9659258262890683122, 1.000000000000000000, 0.9659258262890683122, 1.000000000000000000, 0.9659258262890683122, 1.000000000000000000 ) ) 
 REPRESENTATION_ITEM ( '' )  );
#77332 = VECTOR ( 'NONE', #84125, 999.9999999999998863 ) ;
#77333 = DIRECTION ( 'NONE',  ( 1.000000000000000000, 1.224606353822377258E-16, 0.000000000000000000 ) ) ;
#77334 = ORIENTED_EDGE ( 'NONE', *, *, #4471, .T. ) ;
#77335 = EDGE_CURVE ( 'NONE', #3406, #126947, #82959, .T. ) ;
#77336 = VECTOR ( 'NONE', #122428, 1000.000000000000227 ) ;
#77337 = ORIENTED_EDGE ( 'NONE', *, *, #1709, .F. ) ;
#77338 = CARTESIAN_POINT ( 'NONE',  ( 100.0995968585647944, -6.109999999999997655, -1.637169565754160283 ) ) ;
#77339 = ORIENTED_EDGE ( 'NONE', *, *, #83627, .F. ) ;
#77340 = ORIENTED_EDGE ( 'NONE', *, *, #95735, .F. ) ;
#77341 = AXIS2_PLACEMENT_3D ( 'NONE', #70131, #94666, #39624 ) ;
#77342 = FACE_OUTER_BOUND ( 'NONE', #78989, .T. ) ;
#77343 = EDGE_CURVE ( 'NONE', #32288, #130620, #61042, .T. ) ;
#77344 = CARTESIAN_POINT ( 'NONE',  ( 13.04515773336657780, -21.74070752338407075, 21.72585301388587808 ) ) ;
#77346 = EDGE_CURVE ( 'NONE', #22185, #19349, #138554, .T. ) ;
#77345 = LINE ( 'NONE', #99032, #123589 ) ;
#77347 = ORIENTED_EDGE ( 'NONE', *, *, #49440, .T. ) ;
#77348 = CARTESIAN_POINT ( 'NONE',  ( -48.48921356237309510, -27.52281430457089328, 5.000000000000000000 ) ) ;
#77349 = LINE ( 'NONE', #27022, #98253 ) ;
#77350 = DIRECTION ( 'NONE',  ( 0.7071067811865487940, -0.7071067811865463515, 0.000000000000000000 ) ) ;
#77352 = FACE_OUTER_BOUND ( 'NONE', #94781, .T. ) ;
#77351 = DIRECTION ( 'NONE',  ( -0.000000000000000000, 0.3543493200069153248, 0.9351131265310292928 ) ) ;
#77353 = CARTESIAN_POINT ( 'NONE',  ( 2.000000000000256239, -6.019044215166783118, 0.9592349742722835471 ) ) ;
#77354 =( GEOMETRIC_REPRESENTATION_CONTEXT ( 3 ) GLOBAL_UNCERTAINTY_ASSIGNED_CONTEXT ( ( #25688 ) ) GLOBAL_UNIT_ASSIGNED_CONTEXT ( ( #69170, #91621, #23500 ) ) REPRESENTATION_CONTEXT ( 'NONE', 'WORKASPACE' ) );
#77355 = CARTESIAN_POINT ( 'NONE',  ( 1.152381814940565130, 0.6684352261620748470, 3.831050770371648984 ) ) ;
#77356 = ORIENTED_EDGE ( 'NONE', *, *, #451, .F. ) ;
#77357 = CARTESIAN_POINT ( 'NONE',  ( 88.06249999999998579, -5.819803920172573086, -5.819803920172573974 ) ) ;
#77358 = CARTESIAN_POINT ( 'NONE',  ( 0.000000000000000000, 0.000000000000000000, 5.000000000000000000 ) ) ;
#77359 = ORIENTED_EDGE ( 'NONE', *, *, #130494, .T. ) ;
#77360 = ORIENTED_EDGE ( 'NONE', *, *, #135797, .T. ) ;
#77361 = ADVANCED_FACE ( 'NONE', ( #96428 ), #39794, .T. ) ;
#77362 = VERTEX_POINT ( 'NONE', #72629 ) ;
#77363 = CARTESIAN_POINT ( 'NONE',  ( 68.25043019189810423, 3.055000000000002824, -5.291415217122919401 ) ) ;
#77364 = EDGE_LOOP ( 'NONE', ( #43827, #39541, #60099, #96383 ) ) ;
#77365 = CARTESIAN_POINT ( 'NONE',  ( 0.000000000000000000, -21.76999999999999247, -39.50000000000000000 ) ) ;
#77366 = VECTOR ( 'NONE', #80749, 1000.000000000000000 ) ;
#77367 = CARTESIAN_POINT ( 'NONE',  ( 0.04580628287043911340, 5.278424836066143655, -3.047499999999997655 ) ) ;
#77368 = CARTESIAN_POINT ( 'NONE',  ( 96.68793019189811844, 6.110000000000002984, -1.637169565754156730 ) ) ;
#77369 = CARTESIAN_POINT ( 'NONE',  ( 30.98911971346031180, -22.02621442084248216, 4.990779571109225543 ) ) ;
#77370 = ORIENTED_EDGE ( 'NONE', *, *, #59022, .F. ) ;
#77371 = DIRECTION ( 'NONE',  ( 0.000000000000000000, 0.000000000000000000, 1.000000000000000000 ) ) ;
#77372 = CARTESIAN_POINT ( 'NONE',  ( 1.499999999999997780, 7.466399257802191158, 5.000000000000000000 ) ) ;
#77373 = VECTOR ( 'NONE', #41458, 1000.000000000000000 ) ;
#77374 = CARTESIAN_POINT ( 'NONE',  ( 12.00548008471251293, 28.92564299267929684, 4.000000000000000000 ) ) ;
#77375 = CARTESIAN_POINT ( 'NONE',  ( 0.000000000000000000, 0.000000000000000000, 5.000000000000000000 ) ) ;
#77376 = EDGE_LOOP ( 'NONE', ( #77163, #126515, #31634, #65685 ) ) ;
#77377 = CARTESIAN_POINT ( 'NONE',  ( 30.79333936457826937, 21.75929247661550647, 4.998822639870708073 ) ) ;
#77378 = ORIENTED_EDGE ( 'NONE', *, *, #69339, .T. ) ;
#77379 = VERTEX_POINT ( 'NONE', #39984 ) ;
#77380 = ORIENTED_EDGE ( 'NONE', *, *, #62018, .T. ) ;
#77381 = CARTESIAN_POINT ( 'NONE',  ( 125.3287635252314516, 0.000000000000000000, -6.109999999999998543 ) ) ;
#77382 = ADVANCED_FACE ( 'NONE', ( #129805 ), #39250, .F. ) ;
#77383 = CARTESIAN_POINT ( 'NONE',  ( 10.17183060077640810, 3.759292476615685441, 4.000000000000000000 ) ) ;
#77384 = CARTESIAN_POINT ( 'NONE',  ( 19.17183060077634238, -11.24070752338416490, 4.000000000000000000 ) ) ;
#77386 = EDGE_CURVE ( 'NONE', #88378, #70323, #140000, .T. ) ;
#77385 = EDGE_CURVE ( 'NONE', #45976, #22044, #27629, .T. ) ;
#77387 = ORIENTED_EDGE ( 'NONE', *, *, #62067, .F. ) ;
#77388 = CARTESIAN_POINT ( 'NONE',  ( 52.51203195997707951, -49.11957940092399610, 40.22172306649563467 ) ) ;
#77389 = VERTEX_POINT ( 'NONE', #5858 ) ;
#77390 = EDGE_CURVE ( 'NONE', #103866, #129269, #74012, .T. ) ;
#77391 = EDGE_CURVE ( 'NONE', #19406, #75708, #38524, .T. ) ;
#77392 = VECTOR ( 'NONE', #11040, 1000.000000000000000 ) ;
#77393 = CARTESIAN_POINT ( 'NONE',  ( 13.97873647476855119, -5.808823158059033709, 5.808823158059035485 ) ) ;
#77394 = CARTESIAN_POINT ( 'NONE',  ( 30.18398860626900060, 28.73617430169808173, 5.000000000000000000 ) ) ;
#77395 = EDGE_CURVE ( 'NONE', #44308, #112461, #17470, .T. ) ;
#77396 = DIRECTION ( 'NONE',  ( 0.7071067811865487940, 0.7071067811865463515, -0.000000000000000000 ) ) ;
#77397 = CARTESIAN_POINT ( 'NONE',  ( -12.47512612785037689, 14.25929247661557397, 9.797011795316608485 ) ) ;
#77398 = ORIENTED_EDGE ( 'NONE', *, *, #24340, .F. ) ;
#77399 = VERTEX_POINT ( 'NONE', #83463 ) ;
#77400 = ADVANCED_FACE ( 'NONE', ( #62434 ), #73307, .T. ) ;
#77401 = ORIENTED_EDGE ( 'NONE', *, *, #34040, .F. ) ;
#77402 = SURFACE_STYLE_FILL_AREA ( #65822 ) ;
#77403 = FACE_OUTER_BOUND ( 'NONE', #36483, .T. ) ;
#77404 = EDGE_CURVE ( 'NONE', #54347, #132587, #82750, .T. ) ;
#77405 = CARTESIAN_POINT ( 'NONE',  ( -18.79289321881332597, -11.24070752338416668, 5.000000000000000000 ) ) ;
#77406 = DIRECTION ( 'NONE',  ( -0.000000000000000000, 0.000000000000000000, 1.000000000000000000 ) ) ;
#77407 = ADVANCED_FACE ( 'NONE', ( #6548 ), #63164, .T. ) ;
#77408 = DIRECTION ( 'NONE',  ( -1.000000000000000000, -1.224606353822377258E-16, -0.000000000000000000 ) ) ;
#77409 = COLOUR_RGB ( '', 0.31764706, 0.68627451, 0.89019608) ;
#77410 = DIRECTION ( 'NONE',  ( 0.7071067811865487940, 0.7071067811865463515, 0.000000000000000000 ) ) ;
#77411 = DIRECTION ( 'NONE',  ( 0.3543493200069163240, 0.000000000000000000, 0.9351131265310288487 ) ) ;
#77412 = PLANE ( 'NONE',  #23491 ) ;
#77413 = EDGE_LOOP ( 'NONE', ( #132836, #92072, #24012, #52873 ) ) ;
#77414 = DIRECTION ( 'NONE',  ( 1.000000000000000000, 0.000000000000000000, 0.000000000000000000 ) ) ;
#77415 = ORIENTED_EDGE ( 'NONE', *, *, #22805, .F. ) ;
#77416 = DIRECTION ( 'NONE',  ( 0.7071067811865487940, 0.7071067811865463515, 0.000000000000000000 ) ) ;
#77417 = ORIENTED_EDGE ( 'NONE', *, *, #120535, .T. ) ;
#77418 = EDGE_CURVE ( 'NONE', #136567, #16596, #8007, .T. ) ;
#77419 = CARTESIAN_POINT ( 'NONE',  ( 17.83747294953710494, 6.094999999999989981, -1.119633336120465690E-15 ) ) ;
#77421 = VERTEX_POINT ( 'NONE', #106591 ) ;
#77420 = FACE_OUTER_BOUND ( 'NONE', #103991, .T. ) ;
#77422 = VECTOR ( 'NONE', #60263, 1000.000000000000227 ) ;
#77423 = CARTESIAN_POINT ( 'NONE',  ( -17.70025512860841488, -27.71228299555193786, 4.000000000000000000 ) ) ;
#77424 = EDGE_LOOP ( 'NONE', ( #97249, #13526, #52279, #101179 ) ) ;
#77425 = PRESENTATION_STYLE_ASSIGNMENT (( #134650 ) ) ;
#77426 = VERTEX_POINT ( 'NONE', #7289 ) ;
#77427 = DIRECTION ( 'NONE',  ( 1.201410254241279878E-16, -1.000000000000000000, 0.000000000000000000 ) ) ;
#77428 = ORIENTED_EDGE ( 'NONE', *, *, #55838, .F. ) ;
#77429 = EDGE_CURVE ( 'NONE', #139966, #124257, #95750, .T. ) ;
#77430 = VECTOR ( 'NONE', #5807, 1000.000000000000000 ) ;
#77431 = FACE_OUTER_BOUND ( 'NONE', #63099, .T. ) ;
#77432 = CARTESIAN_POINT ( 'NONE',  ( 117.0375270504628986, -9.735942053221456900E-16, 7.949999999999998401 ) ) ;
#77433 = SURFACE_STYLE_USAGE ( .BOTH. , #67999 ) ;
#77434 = CARTESIAN_POINT ( 'NONE',  ( -27.70710678118634362, -18.74070752338409207, 5.000000000000000000 ) ) ;
#77435 = SURFACE_SIDE_STYLE ('',( #133233 ) ) ;
#77436 = DIRECTION ( 'NONE',  ( -1.000000000000000000, -3.115803279706882722E-16, 0.000000000000000000 ) ) ;
#77437 = DIRECTION ( 'NONE',  ( -0.7071067811865487940, 0.7071067811865463515, 0.000000000000000000 ) ) ;
#77438 = CARTESIAN_POINT ( 'NONE',  ( 12.10416666666666607, -1.633150327867691987, -6.094999999999989093 ) ) ;
#77439 = CARTESIAN_POINT ( 'NONE',  ( 18.93706980810188867, 2.126176841940952134, -7.934999999999992504 ) ) ;
#77440 = FACE_OUTER_BOUND ( 'NONE', #107550, .T. ) ;
#77441 = CARTESIAN_POINT ( 'NONE',  ( -33.48921356237309510, -27.52281430457078670, 5.000000000000000000 ) ) ;
#77442 = ORIENTED_EDGE ( 'NONE', *, *, #79555, .T. ) ;
#77443 = VERTEX_POINT ( 'NONE', #129087 ) ;
#77444 = AXIS2_PLACEMENT_3D ( 'NONE', #97439, #65592, #87307 ) ;
#77445 = DIRECTION ( 'NONE',  ( 0.7071067811865486830, -0.7071067811865464625, -0.000000000000000000 ) ) ;
#77446 = EDGE_LOOP ( 'NONE', ( #140045, #60775, #131157, #52485 ) ) ;
#77447 = EDGE_CURVE ( 'NONE', #108671, #78331, #18899, .T. ) ;
#77448 = DIRECTION ( 'NONE',  ( 0.000000000000000000, 0.000000000000000000, 1.000000000000000000 ) ) ;
#77449 = CARTESIAN_POINT ( 'NONE',  ( 29.29298673570674438, -21.74070752338405654, 4.999753212805219782 ) ) ;
#77450 = DIRECTION ( 'NONE',  ( 0.7071067811865486830, -0.7071067811865464625, -0.000000000000000000 ) ) ;
#77451 = CARTESIAN_POINT ( 'NONE',  ( 128.0481121284643962, -51.19676978474259954, -38.21513923099703902 ) ) ;
#77452 = ORIENTED_EDGE ( 'NONE', *, *, #117429, .F. ) ;
#77453 = LINE ( 'NONE', #79619, #93818 ) ;
#77454 = DIRECTION ( 'NONE',  ( -0.6830127018922181881, 0.6830127018922202975, -0.2588190451025214056 ) ) ;
#77455 = ADVANCED_FACE ( 'NONE', ( #41360 ), #106803, .T. ) ;
#77456 = DIRECTION ( 'NONE',  ( 0.7071067811865487940, 0.7071067811865463515, -0.000000000000000000 ) ) ;
#77457 =( NAMED_UNIT ( * ) SI_UNIT ( $, .STERADIAN. ) SOLID_ANGLE_UNIT ( ) );
#77458 = FACE_OUTER_BOUND ( 'NONE', #10763, .T. ) ;
#77460 = ORIENTED_EDGE ( 'NONE', *, *, #57217, .F. ) ;
#77459 = DIRECTION ( 'NONE',  ( -0.7071067811865486830, 0.7071067811865464625, 0.000000000000000000 ) ) ;
#77461 = LINE ( 'NONE', #99146, #67811 ) ;
#77462 = CARTESIAN_POINT ( 'NONE',  ( -71.99451991528749772, 28.92564299267988304, 4.000000000000000000 ) ) ;
#77463 = LINE ( 'NONE', #121626, #22408 ) ;
#77464 = FACE_OUTER_BOUND ( 'NONE', #9506, .T. ) ;
#77465 = VERTEX_POINT ( 'NONE', #141398 ) ;
#77466 = ORIENTED_EDGE ( 'NONE', *, *, #107976, .T. ) ;
#77467 = ORIENTED_EDGE ( 'NONE', *, *, #115028, .F. ) ;
#77468 = CARTESIAN_POINT ( 'NONE',  ( 96.54209685856477563, 5.291415217122923842, -3.054999999999996163 ) ) ;
#77469 = ORIENTED_EDGE ( 'NONE', *, *, #20389, .T. ) ;
#77470 = ADVANCED_FACE ( 'NONE', ( #33399 ), #31929, .F. ) ;
#77471 = DIRECTION ( 'NONE',  ( -1.000000000000000000, -0.000000000000000000, -0.000000000000000000 ) ) ;
#77472 = LINE ( 'NONE', #97760, #128801 ) ;
#77473 = ORIENTED_EDGE ( 'NONE', *, *, #48435, .T. ) ;
#77474 = CARTESIAN_POINT ( 'NONE',  ( 8.500000000000000000, -2.055000000000000160, 0.000000000000000000 ) ) ;
#77476 = VECTOR ( 'NONE', #131888, 1000.000000000000000 ) ;
#77475 = CARTESIAN_POINT ( 'NONE',  ( 48.54166666666666430, -3.975000000000002753, 6.884901960086286188 ) ) ;
#77477 = CARTESIAN_POINT ( 'NONE',  ( 85.95376352523145158, -6.109999999999998543, -3.741295971395162543E-16 ) ) ;
#77478 = ORIENTED_EDGE ( 'NONE', *, *, #98881, .T. ) ;
#77479 = CARTESIAN_POINT ( 'NONE',  ( -14.99999999999989519, -7.068876922607736368, 4.000000000000000000 ) ) ;
#77480 = CARTESIAN_POINT ( 'NONE',  ( 6.540657738503846907, 4.202752102959690472E-16, 0.000000000000000000 ) ) ;
#77481 = VERTEX_POINT ( 'NONE', #9415 ) ;
#77482 = EDGE_LOOP ( 'NONE', ( #106559, #3796, #136122, #55896 ) ) ;
#77483 = EDGE_CURVE ( 'NONE', #81979, #23623, #8688, .T. ) ;
#77484 = ORIENTED_EDGE ( 'NONE', *, *, #141290, .F. ) ;
#77485 = FACE_OUTER_BOUND ( 'NONE', #85040, .T. ) ;
#77486 = EDGE_CURVE ( 'NONE', #99307, #566, #11566, .T. ) ;
#77487 = FACE_OUTER_BOUND ( 'NONE', #136239, .T. ) ;
#77488 = CARTESIAN_POINT ( 'NONE',  ( 19.46290314143521982, -3.967499999999994476, 6.871911579029513106 ) ) ;
#77489 = CARTESIAN_POINT ( 'NONE',  ( 23.99999999999984723, -16.44781430457065241, 5.000000000000000000 ) ) ;
#77490 = VECTOR ( 'NONE', #40788, 1000.000000000000227 ) ;
#77491 = CARTESIAN_POINT ( 'NONE',  ( -25.49999999999982236, 13.56627193232212392, -10.57019076586074391 ) ) ;
#77492 = CARTESIAN_POINT ( 'NONE',  ( 34.42499999999998295, 11.97718569542927014, 5.000000000000000000 ) ) ;
#77493 = DIRECTION ( 'NONE',  ( -0.7071067811865486830, 0.7071067811865464625, 0.000000000000000000 ) ) ;
#77494 = AXIS2_PLACEMENT_3D ( 'NONE', #63885, #31253, #53725 ) ;
#77495 = EDGE_CURVE ( 'NONE', #136084, #39996, #142141, .T. ) ;
#77496 = ORIENTED_EDGE ( 'NONE', *, *, #3092, .F. ) ;
#77497 = ORIENTED_EDGE ( 'NONE', *, *, #50418, .T. ) ;
#77498 = AXIS2_PLACEMENT_3D ( 'NONE', #111259, #100418, #89526 ) ;
#77499 = CARTESIAN_POINT ( 'NONE',  ( -20.18650864602349060, -15.74070752338412404, 8.904080028138988467 ) ) ;
#77500 = VERTEX_POINT ( 'NONE', #31229 ) ;
#77501 = ORIENTED_EDGE ( 'NONE', *, *, #113153, .T. ) ;
#77502 = ADVANCED_FACE ( 'NONE', ( #66705 ), #20311, .F. ) ;
#77504 = EDGE_CURVE ( 'NONE', #31910, #56980, #99295, .T. ) ;
#77503 = DIRECTION ( 'NONE',  ( 0.7071067811865487940, 0.7071067811865463515, 0.000000000000000000 ) ) ;
#77505 = VERTEX_POINT ( 'NONE', #42826 ) ;
#77506 = VECTOR ( 'NONE', #16004, 999.9999999999998863 ) ;
#77507 = CARTESIAN_POINT ( 'NONE',  ( -26.99999999999981526, -13.39766691384885711, -10.96608748226459618 ) ) ;
#77508 = LINE ( 'NONE', #55028, #43909 ) ;
#77509 = DIRECTION ( 'NONE',  ( -0.5735764363510507113, 0.8191520442889885789, 1.003171929053520926E-16 ) ) ;
#77510 = DIRECTION ( 'NONE',  ( -0.000000000000000000, 0.000000000000000000, 1.000000000000000000 ) ) ;
#77511 = LINE ( 'NONE', #109391, #79085 ) ;
#77512 = ORIENTED_EDGE ( 'NONE', *, *, #118260, .F. ) ;
#77513 = FACE_OUTER_BOUND ( 'NONE', #117957, .T. ) ;
#77514 = ORIENTED_EDGE ( 'NONE', *, *, #16859, .F. ) ;
#77515 = CARTESIAN_POINT ( 'NONE',  ( 28.49999999999980460, 18.05218569542898521, 5.000000000000000000 ) ) ;
#77516 = ORIENTED_EDGE ( 'NONE', *, *, #141495, .T. ) ;
#77517 = LINE ( 'NONE', #134759, #83906 ) ;
#77518 = EDGE_CURVE ( 'NONE', #131139, #92065, #131973, .T. ) ;
#77519 = ORIENTED_EDGE ( 'NONE', *, *, #95363, .F. ) ;
#77520 = PLANE ( 'NONE',  #4141 ) ;
#77521 = ORIENTED_EDGE ( 'NONE', *, *, #53833, .T. ) ;
#77522 = ORIENTED_EDGE ( 'NONE', *, *, #33738, .T. ) ;
#77523 = ORIENTED_EDGE ( 'NONE', *, *, #56396, .T. ) ;
#77524 = DIRECTION ( 'NONE',  ( 0.6830127018922180770, -0.6830127018922204085, -0.2588190451025213501 ) ) ;
#77525 = LINE ( 'NONE', #78955, #8132 ) ;
#77526 = VECTOR ( 'NONE', #44403, 1000.000000000000000 ) ;
#77527 = VECTOR ( 'NONE', #107125, 999.9999999999998863 ) ;
#77528 = DIRECTION ( 'NONE',  ( 0.000000000000000000, 0.000000000000000000, 1.000000000000000000 ) ) ;
#77529 = PLANE ( 'NONE',  #70414 ) ;
#77530 = DIRECTION ( 'NONE',  ( -0.3543493200069163240, 0.000000000000000000, -0.9351131265310288487 ) ) ;
#77531 = CARTESIAN_POINT ( 'NONE',  ( -0.3281693992235219515, -6.740707523384212863, 4.000000000000000000 ) ) ;
#77532 = VECTOR ( 'NONE', #43422, 1000.000000000000227 ) ;
#77533 = CARTESIAN_POINT ( 'NONE',  ( 63.29974487139158867, -27.71228299555250274, 4.000000000000000000 ) ) ;
#77534 = LINE ( 'NONE', #76823, #92189 ) ;
#77535 = CARTESIAN_POINT ( 'NONE',  ( 34.60428828362104525, 22.19175015946030172, 4.000000000000000000 ) ) ;
#77536 = DIRECTION ( 'NONE',  ( -0.6830127018922181881, 0.6830127018922202975, -0.2588190451025214056 ) ) ;
#77537 = VERTEX_POINT ( 'NONE', #143540 ) ;
#77538 = DIRECTION ( 'NONE',  ( -0.000000000000000000, -0.3543493200069152693, 0.9351131265310292928 ) ) ;
#77539 = CARTESIAN_POINT ( 'NONE',  ( 7.139999999999992575, -35.14999999999999858, -40.00000000000000000 ) ) ;
#77540 = ORIENTED_EDGE ( 'NONE', *, *, #82299, .T. ) ;
#77541 = ORIENTED_EDGE ( 'NONE', *, *, #104332, .T. ) ;
#77542 = ORIENTED_EDGE ( 'NONE', *, *, #50166, .F. ) ;
#77543 = CARTESIAN_POINT ( 'NONE',  ( -5.999999999999953815, 13.55218569542903317, 5.000000000000000000 ) ) ;
#77544 = ORIENTED_EDGE ( 'NONE', *, *, #17622, .F. ) ;
#77545 = ORIENTED_EDGE ( 'NONE', *, *, #121689, .T. ) ;
#77546 = CARTESIAN_POINT ( 'NONE',  ( -36.29974487139159578, -27.71228299555231445, 4.000000000000000000 ) ) ;
#77547 = CARTESIAN_POINT ( 'NONE',  ( 106.8291937171295700, -3.975000000000001865, 6.884901960086284411 ) ) ;
#77548 = LINE ( 'NONE', #121716, #56583 ) ;
#77549 = CARTESIAN_POINT ( 'NONE',  ( 28.49999999999981171, 16.18958161055405753, -11.56426086740805204 ) ) ;
#77550 = ORIENTED_EDGE ( 'NONE', *, *, #102084, .T. ) ;
#77551 = DIRECTION ( 'NONE',  ( -0.7071067811865487940, 0.7071067811865463515, 0.000000000000000000 ) ) ;
#77552 = EDGE_LOOP ( 'NONE', ( #85793, #137630, #84396, #105183 ) ) ;
#77553 = LINE ( 'NONE', #97855, #9644 ) ;
#77554 = ADVANCED_FACE ( 'NONE', ( #119615 ), #118926, .F. ) ;
#77555 = CARTESIAN_POINT ( 'NONE',  ( 16.98373647476855197, -5.808823158059035485, -5.808823158059033709 ) ) ;
#77556 = ORIENTED_EDGE ( 'NONE', *, *, #65769, .F. ) ;
#77557 = CARTESIAN_POINT ( 'NONE',  ( 81.14126352523143737, 4.472830434245837594, 4.472830434245841147 ) ) ;
#77558 = ADVANCED_FACE ( 'NONE', ( #110180 ), #5055, .F. ) ;
#77559 = CARTESIAN_POINT ( 'NONE',  ( 5.949495903232621785, -9.500232149547882088, -0.2856502682321572784 ) ) ;
#77560 = ADVANCED_FACE ( 'NONE', ( #131240 ), #55845, .F. ) ;
#77561 = CARTESIAN_POINT ( 'NONE',  ( 2.999999999999978240, -8.731860332648835765, -2.120594902707531926 ) ) ;
#77562 = ORIENTED_EDGE ( 'NONE', *, *, #134174, .T. ) ;
#77563 = ORIENTED_EDGE ( 'NONE', *, *, #111097, .F. ) ;
#77564 = EDGE_CURVE ( 'NONE', #50064, #51894, #66016, .T. ) ;
#77565 = ORIENTED_EDGE ( 'NONE', *, *, #54012, .F. ) ;
#77566 = CARTESIAN_POINT ( 'NONE',  ( 21.29974487139158512, -27.71228299555221142, 4.000000000000000000 ) ) ;
#77567 = CARTESIAN_POINT ( 'NONE',  ( -6.994446791092093669E-14, -39.92999999999999261, 19.06900128115121618 ) ) ;
#77568 = CARTESIAN_POINT ( 'NONE',  ( -15.75860074219783513, 21.72499999999999432, 5.000000000000000000 ) ) ;
#77569 = EDGE_CURVE ( 'NONE', #94043, #33680, #64554, .T. ) ;
#77570 = CARTESIAN_POINT ( 'NONE',  ( 75.48921356237309510, -27.52281430457107803, 5.000000000000000000 ) ) ;
#77572 = VERTEX_POINT ( 'NONE', #88468 ) ;
#77571 = VECTOR ( 'NONE', #31687, 1000.000000000000000 ) ;
#77573 = EDGE_CURVE ( 'NONE', #113402, #50766, #98602, .T. ) ;
#77574 = LINE ( 'NONE', #121742, #120693 ) ;
#77575 = CARTESIAN_POINT ( 'NONE',  ( -26.99999999999981171, 13.55218569542903495, 5.000000000000000000 ) ) ;
#77576 = VERTEX_POINT ( 'NONE', #142832 ) ;
#77577 = CARTESIAN_POINT ( 'NONE',  ( -34.53569095963128177, 22.21392809009763170, 4.239552123775272463 ) ) ;
#77578 = DIRECTION ( 'NONE',  ( -0.7071067811865487940, 0.7071067811865463515, -0.000000000000000000 ) ) ;
#77579 = ORIENTED_EDGE ( 'NONE', *, *, #112427, .T. ) ;
#77580 = EDGE_CURVE ( 'NONE', #125243, #73980, #55120, .T. ) ;
#77582 = ORIENTED_EDGE ( 'NONE', *, *, #36153, .F. ) ;
#77581 = PLANE ( 'NONE',  #9211 ) ;
#77583 = ORIENTED_EDGE ( 'NONE', *, *, #72275, .F. ) ;
#77584 = EDGE_CURVE ( 'NONE', #7658, #124601, #21768, .T. ) ;
#77585 = CARTESIAN_POINT ( 'NONE',  ( -9.461603553705650427, -9.740707523384173783, 17.74957260769608780 ) ) ;
#77586 = CARTESIAN_POINT ( 'NONE',  ( 14.29289321881336150, -9.740707523384182664, 5.000000000000000000 ) ) ;
#77587 = ORIENTED_EDGE ( 'NONE', *, *, #123480, .F. ) ;
#77588 = CARTESIAN_POINT ( 'NONE',  ( -31.49999999999976552, -1.912538124160739095, 4.000000000000000000 ) ) ;
#77589 = EDGE_CURVE ( 'NONE', #24379, #107684, #89174, .T. ) ;
#77590 = LINE ( 'NONE', #111625, #128503 ) ;
#77591 = VECTOR ( 'NONE', #17168, 1000.000000000000000 ) ;
#77592 = LINE ( 'NONE', #57995, #18347 ) ;
#77593 = FACE_OUTER_BOUND ( 'NONE', #21937, .T. ) ;
#77595 = DIRECTION ( 'NONE',  ( -0.000000000000000000, -0.3543493200069152693, 0.9351131265310292928 ) ) ;
#77594 = COLOUR_RGB ( '', 0.72549020, 0.75294118, 0.79215686) ;
#77596 = CARTESIAN_POINT ( 'NONE',  ( -34.49999999999975842, 3.431123077392154830, 4.000000000000000000 ) ) ;
#77597 = PLANE ( 'NONE',  #139789 ) ;
#77598 = DIRECTION ( 'NONE',  ( -0.3543493200069163240, -0.000000000000000000, -0.9351131265310288487 ) ) ;
#77599 = CARTESIAN_POINT ( 'NONE',  ( 17.18706980810188867, -2.126176841940956130, 7.934999999999991616 ) ) ;
#77600 = DIRECTION ( 'NONE',  ( -0.7071067811865486830, -0.7071067811865464625, -0.000000000000000000 ) ) ;
#77601 = CARTESIAN_POINT ( 'NONE',  ( 11.99999999999991296, -5.527737879153178824, -7.983877177622400012 ) ) ;
#77602 = LINE ( 'NONE', #111638, #104379 ) ;
#77603 = CARTESIAN_POINT ( 'NONE',  ( -7.140000000000001457, -35.69931899287965393, -11.97485302731578294 ) ) ;
#77604 = ORIENTED_EDGE ( 'NONE', *, *, #130696, .F. ) ;
#77605 = ORIENTED_EDGE ( 'NONE', *, *, #83351, .F. ) ;
#77606 = CARTESIAN_POINT ( 'NONE',  ( 104.3958333333333428, -2.130196079827427091, 7.949999999999999289 ) ) ;
#77607 = ORIENTED_EDGE ( 'NONE', *, *, #36775, .F. ) ;
#77608 = AXIS2_PLACEMENT_3D ( 'NONE', #105705, #82564, #39054 ) ;
#77609 = ORIENTED_EDGE ( 'NONE', *, *, #97733, .F. ) ;
#77610 = VERTEX_POINT ( 'NONE', #134108 ) ;
#77611 = EDGE_CURVE ( 'NONE', #7821, #130956, #124643, .T. ) ;
#77612 = CARTESIAN_POINT ( 'NONE',  ( 22.25000000000000000, 0.000000000000000000, 1.749999999999999778 ) ) ;
#77613 = CARTESIAN_POINT ( 'NONE',  ( 88.93750000000000000, 5.819803920172574863, -5.819803920172573086 ) ) ;
#77614 = ORIENTED_EDGE ( 'NONE', *, *, #136879, .F. ) ;
#77615 = CARTESIAN_POINT ( 'NONE',  ( 2.924914550060625285, 4.584330080086930965E-16, 0.000000000000000000 ) ) ;
#77616 = LINE ( 'NONE', #121786, #134451 ) ;
#77617 = CARTESIAN_POINT ( 'NONE',  ( 14.08979869950237074, -1.618973607074033483, -36.99999999997771738 ) ) ;
#77618 = CARTESIAN_POINT ( 'NONE',  ( 38.99451991528749062, 28.92564299267965211, 4.000000000000000000 ) ) ;
#77619 = ORIENTED_EDGE ( 'NONE', *, *, #52238, .F. ) ;
#77620 = DIRECTION ( 'NONE',  ( 0.7071067811865487940, 0.7071067811865463515, 0.000000000000000000 ) ) ;
#77621 = DIRECTION ( 'NONE',  ( 0.6830127018922181881, 0.6830127018922202975, -0.2588190451025214056 ) ) ;
#77622 = CARTESIAN_POINT ( 'NONE',  ( -34.75611968250422024, 16.70565069852389328, 4.955485411084898928 ) ) ;
#77623 = CARTESIAN_POINT ( 'NONE',  ( 34.92499999999998295, 22.22500000000000142, 4.000000000000000000 ) ) ;
#77624 = DIRECTION ( 'NONE',  ( 0.7071067811865487940, 0.7071067811865463515, -0.000000000000000000 ) ) ;
#77625 = DIRECTION ( 'NONE',  ( -0.000000000000000000, 1.000000000000000000, 1.091707662666338270E-16 ) ) ;
#77626 = EDGE_CURVE ( 'NONE', #44075, #88739, #114467, .T. ) ;
#77627 = VECTOR ( 'NONE', #130572, 1000.000000000000227 ) ;
#77628 = LINE ( 'NONE', #121098, #97772 ) ;
#77629 = VECTOR ( 'NONE', #16322, 1000.000000000000000 ) ;
#77630 = ORIENTED_EDGE ( 'NONE', *, *, #106837, .T. ) ;
#77631 = ORIENTED_EDGE ( 'NONE', *, *, #33306, .T. ) ;
#77632 = VECTOR ( 'NONE', #133170, 1000.000000000000000 ) ;
#77633 = CARTESIAN_POINT ( 'NONE',  ( 119.1462635252314470, -4.472830434245840259, 4.472830434245839371 ) ) ;
#77634 = VERTEX_POINT ( 'NONE', #26056 ) ;
#77635 = VECTOR ( 'NONE', #83598, 1000.000000000000000 ) ;
#77636 = VECTOR ( 'NONE', #126793, 1000.000000000000227 ) ;
#77637 = EDGE_CURVE ( 'NONE', #133910, #47388, #14458, .T. ) ;
#77638 = LINE ( 'NONE', #100087, #31691 ) ;
#77639 = CARTESIAN_POINT ( 'NONE',  ( 28.00000000000002487, -52.14999999999999147, -34.92499999999976978 ) ) ;
#77640 = DIRECTION ( 'NONE',  ( -0.7071067811865486830, 0.7071067811865464625, 0.000000000000000000 ) ) ;
#77641 = CARTESIAN_POINT ( 'NONE',  ( 34.92499999999998295, -22.22500000000000142, 4.500000000000000888 ) ) ;
#77642 = CARTESIAN_POINT ( 'NONE',  ( 117.7454301918981230, -5.291415217122918513, -3.055000000000000160 ) ) ;
#77643 = VERTEX_POINT ( 'NONE', #101457 ) ;
#77644 = EDGE_CURVE ( 'NONE', #56258, #6222, #57283, .T. ) ;
#77645 = ORIENTED_EDGE ( 'NONE', *, *, #102443, .T. ) ;
#77646 = DIRECTION ( 'NONE',  ( 0.7071067811865487940, -0.7071067811865463515, 0.000000000000000000 ) ) ;
#77647 = CARTESIAN_POINT ( 'NONE',  ( 97.83333333333332860, -6.884901960086287964, 3.974999999999998312 ) ) ;
#77648 = ORIENTED_EDGE ( 'NONE', *, *, #87936, .F. ) ;
#77649 = VERTEX_POINT ( 'NONE', #102906 ) ;
#77650 = CARTESIAN_POINT ( 'NONE',  ( 39.22959685856475431, -6.110000000000000320, -1.637169565754161393 ) ) ;
#77651 = EDGE_CURVE ( 'NONE', #54868, #32290, #4219, .T. ) ;
#77652 = ORIENTED_EDGE ( 'NONE', *, *, #46958, .T. ) ;
#77653 = PLANE ( 'NONE',  #9751 ) ;
#77654 = LINE ( 'NONE', #110937, #33942 ) ;
#77655 = CARTESIAN_POINT ( 'NONE',  ( 122.6835989386367771, -49.14999999999999147, -40.92499999999998295 ) ) ;
#77656 = CARTESIAN_POINT ( 'NONE',  ( 28.20376352523144803, 6.109999999999998543, 1.122388791418548911E-15 ) ) ;
#77657 = ORIENTED_EDGE ( 'NONE', *, *, #115857, .T. ) ;
#77658 = CARTESIAN_POINT ( 'NONE',  ( -28.88982677111770059, -22.22500000000000853, 4.785647885939353863 ) ) ;
#77659 = VERTEX_POINT ( 'NONE', #58737 ) ;
#77660 = ORIENTED_EDGE ( 'NONE', *, *, #36437, .T. ) ;
#77661 = ORIENTED_EDGE ( 'NONE', *, *, #58646, .T. ) ;
#77662 = CARTESIAN_POINT ( 'NONE',  ( 0.1630955410174104447, 0.4000000000000001332, -2.152173700565807479 ) ) ;
#77663 = DIRECTION ( 'NONE',  ( -0.7071067811865486830, -0.7071067811865464625, -0.000000000000000000 ) ) ;
#77664 = ADVANCED_FACE ( 'NONE', ( #134845 ), #113038, .T. ) ;
#77665 = ORIENTED_EDGE ( 'NONE', *, *, #10425, .F. ) ;
#77666 = LINE ( 'NONE', #120392, #11199 ) ;
#77667 = DIRECTION ( 'NONE',  ( 0.7071067811865486830, -0.7071067811865464625, -0.000000000000000000 ) ) ;
#77668 = FILL_AREA_STYLE ('',( #23987 ) ) ;
#77669 = CARTESIAN_POINT ( 'NONE',  ( -0.7071067811865398012, 5.259292476615665457, 5.000000000000000000 ) ) ;
#77670 = EDGE_CURVE ( 'NONE', #95691, #3259, #118503, .T. ) ;
#77671 = FACE_BOUND ( 'NONE', #109846, .T. ) ;
#77672 = VERTEX_POINT ( 'NONE', #25318 ) ;
#77673 = LINE ( 'NONE', #45773, #31820 ) ;
#77674 = PLANE ( 'NONE',  #139375 ) ;
#77676 = ADVANCED_FACE ( 'NONE', ( #2105 ), #90602, .T. ) ;
#77675 = DIRECTION ( 'NONE',  ( -0.7071067811865486830, 0.7071067811865464625, 0.000000000000000000 ) ) ;
#77677 = EDGE_LOOP ( 'NONE', ( #103739, #89411, #65819, #84928 ) ) ;
#77678 = CARTESIAN_POINT ( 'NONE',  ( 26.70025512860841488, -27.71228299555187391, 4.000000000000000000 ) ) ;
#77679 = ORIENTED_EDGE ( 'NONE', *, *, #26607, .T. ) ;
#77680 = ORIENTED_EDGE ( 'NONE', *, *, #97081, .T. ) ;
#77681 = CARTESIAN_POINT ( 'NONE',  ( -3.328169399223503966, -18.74070752338408852, 4.000000000000000000 ) ) ;
#77682 = ORIENTED_EDGE ( 'NONE', *, *, #30816, .F. ) ;
#77683 = VECTOR ( 'NONE', #127168, 1000.000000000000000 ) ;
#77684 = CARTESIAN_POINT ( 'NONE',  ( 44.53709685856478728, -3.054999999999998828, -5.291415217122919401 ) ) ;
#77685 = ORIENTED_EDGE ( 'NONE', *, *, #57566, .F. ) ;
#77686 = DIRECTION ( 'NONE',  ( 0.6830127018922180770, -0.6830127018922204085, -0.2588190451025213501 ) ) ;
#77687 = FILL_AREA_STYLE ('',( #10254 ) ) ;
#77688 = CARTESIAN_POINT ( 'NONE',  ( 33.48921356237309510, -27.52281430457078670, 5.000000000000000000 ) ) ;
#77689 = ORIENTED_EDGE ( 'NONE', *, *, #58023, .T. ) ;
#77690 = CARTESIAN_POINT ( 'NONE',  ( -12.20000000000000284, -40.42999999999999261, 19.06900128115121973 ) ) ;
#77691 = CARTESIAN_POINT ( 'NONE',  ( 2.999999999999999112, -7.600000000000055600, -28.92499999999998650 ) ) ;
#77692 = EDGE_CURVE ( 'NONE', #106843, #112433, #35540, .T. ) ;
#77693 = VECTOR ( 'NONE', #83857, 1000.000000000000114 ) ;
#77694 = CARTESIAN_POINT ( 'NONE',  ( 8.999999999999937828, -13.97847968911259464, -0.1324546996126583220 ) ) ;
#77695 = CARTESIAN_POINT ( 'NONE',  ( 33.18398860626899705, 28.73617430169810305, 5.000000000000000000 ) ) ;
#77696 = CARTESIAN_POINT ( 'NONE',  ( 0.000000000000000000, 0.000000000000000000, 5.000000000000000000 ) ) ;
#77697 = CARTESIAN_POINT ( 'NONE',  ( 44.99451991528749772, 28.92564299267969474, 4.000000000000000000 ) ) ;
#77698 = EDGE_LOOP ( 'NONE', ( #53107, #106195, #3104, #90788, #60899 ) ) ;
#77699 = VERTEX_POINT ( 'NONE', #123952 ) ;
#77700 = ORIENTED_EDGE ( 'NONE', *, *, #86390, .T. ) ;
#77701 = CARTESIAN_POINT ( 'NONE',  ( 5.816011393731002066, 28.73617430169783304, 5.000000000000000000 ) ) ;
#77702 = DIRECTION ( 'NONE',  ( 0.6830127018922181881, 0.6830127018922202975, -0.2588190451025214056 ) ) ;
#77703 = ORIENTED_EDGE ( 'NONE', *, *, #33126, .F. ) ;
#77704 = EDGE_LOOP ( 'NONE', ( #56295, #83155, #54214, #108724 ) ) ;
#77705 = LINE ( 'NONE', #24029, #42008 ) ;
#77706 = DIRECTION ( 'NONE',  ( 0.000000000000000000, -1.000000000000000000, 0.000000000000000000 ) ) ;
#77707 = CARTESIAN_POINT ( 'NONE',  ( 39.29974487139159578, -27.71228299555233576, 4.000000000000000000 ) ) ;
#77708 = VERTEX_POINT ( 'NONE', #102196 ) ;
#77709 = CARTESIAN_POINT ( 'NONE',  ( 78.48921356237309510, -27.52281430457109934, 5.000000000000000000 ) ) ;
#77710 = CIRCLE ( 'NONE', #29159, 2.500000000000000444 ) ;
#77711 = FACE_OUTER_BOUND ( 'NONE', #72120, .T. ) ;
#77712 = CARTESIAN_POINT ( 'NONE',  ( 31.12956980810189478, -3.967499999999998028, -6.871911579029511330 ) ) ;
#77714 = EDGE_CURVE ( 'NONE', #117130, #17670, #3546, .T. ) ;
#77713 = AXIS2_PLACEMENT_3D ( 'NONE', #1775, #136611, #47528 ) ;
#77715 = FACE_OUTER_BOUND ( 'NONE', #61944, .T. ) ;
#77716 = ORIENTED_EDGE ( 'NONE', *, *, #42617, .T. ) ;
#77717 = CARTESIAN_POINT ( 'NONE',  ( 107.0995968585648086, -6.109999999999998543, -1.637169565754160727 ) ) ;
#77718 = VECTOR ( 'NONE', #143097, 1000.000000000000000 ) ;
#77719 = EDGE_CURVE ( 'NONE', #14349, #36041, #121140, .T. ) ;
#77720 = DIRECTION ( 'NONE',  ( -0.000000000000000000, -0.000000000000000000, 1.000000000000000000 ) ) ;
#77721 = FACE_OUTER_BOUND ( 'NONE', #120850, .T. ) ;
#77723 = EDGE_LOOP ( 'NONE', ( #64871, #41976, #75365, #66570 ) ) ;
#77722 = CARTESIAN_POINT ( 'NONE',  ( -15.00548008471250228, 28.92564299267927552, 4.000000000000000000 ) ) ;
#77724 = DIRECTION ( 'NONE',  ( -0.7071067811865486830, -0.7071067811865464625, -0.000000000000000000 ) ) ;
#77725 = ORIENTED_EDGE ( 'NONE', *, *, #81155, .T. ) ;
#77726 = VECTOR ( 'NONE', #130350, 999.9999999999998863 ) ;
#77727 = FACE_OUTER_BOUND ( 'NONE', #87368, .T. ) ;
#77728 = DIRECTION ( 'NONE',  ( -0.7071067811865487940, 0.7071067811865463515, -0.000000000000000000 ) ) ;
#77729 = ADVANCED_FACE ( 'NONE', ( #70147 ), #112191, .T. ) ;
#77730 = EDGE_CURVE ( 'NONE', #43949, #27998, #136062, .T. ) ;
#77731 = DIRECTION ( 'NONE',  ( 2.781805975412906507E-17, 0.3543493200069153248, 0.9351131265310292928 ) ) ;
#77732 = ORIENTED_EDGE ( 'NONE', *, *, #46011, .F. ) ;
#77733 = ADVANCED_BREP_SHAPE_REPRESENTATION ( '', ( #94738, #127880 ), #33203 ) ;
#77734 = LINE ( 'NONE', #101599, #115922 ) ;
#77735 = CARTESIAN_POINT ( 'NONE',  ( 19.05000000000000071, 3.174999999999997158, 5.000000000000000000 ) ) ;
#77736 = ORIENTED_EDGE ( 'NONE', *, *, #131938, .F. ) ;
#77737 = CARTESIAN_POINT ( 'NONE',  ( 31.49999999999977973, -15.29013452822851882, 0.3645803511611086511 ) ) ;
#77738 = DIRECTION ( 'NONE',  ( -0.7071067811865487940, 0.7071067811865463515, -0.000000000000000000 ) ) ;
#77739 = ORIENTED_EDGE ( 'NONE', *, *, #76655, .F. ) ;
#77740 = EDGE_CURVE ( 'NONE', #86591, #24725, #91163, .T. ) ;
#77741 = CARTESIAN_POINT ( 'NONE',  ( -34.92500000000001137, 21.72500000000000142, 5.000000000000000000 ) ) ;
#77743 = ORIENTED_EDGE ( 'NONE', *, *, #143270, .T. ) ;
#77742 = DIRECTION ( 'NONE',  ( 0.5735764363510444941, 0.8191520442889929088, 0.000000000000000000 ) ) ;
#77744 = EDGE_CURVE ( 'NONE', #26004, #143241, #123191, .T. ) ;
#77745 = ORIENTED_EDGE ( 'NONE', *, *, #29923, .T. ) ;
#77746 = DIRECTION ( 'NONE',  ( 0.000000000000000000, -1.000000000000000000, 0.000000000000000000 ) ) ;
#77747 = EDGE_LOOP ( 'NONE', ( #124862, #20805, #130666, #15801 ) ) ;
#77749 = EDGE_CURVE ( 'NONE', #61664, #45414, #100598, .T. ) ;
#77748 =( BOUNDED_CURVE ( )  B_SPLINE_CURVE ( 2, ( #4220, #26757, #76539, #12666, #21427, #34438, #23557, #87403, #56239, #33052, #133755, #77953, #22802 ),
 .UNSPECIFIED., .F., .T. ) 
 B_SPLINE_CURVE_WITH_KNOTS ( ( 3, 2, 2, 2, 2, 2, 3 ),
 ( 0.5000000000000000000, 0.5083333333333333037, 0.5166666666666667185, 0.5250000000000001332, 0.5333333333333334370, 0.5416666666666667407, 0.5500000000000001554 ),
 .UNSPECIFIED. ) 
 CURVE ( )  GEOMETRIC_REPRESENTATION_ITEM ( )  RATIONAL_B_SPLINE_CURVE ( ( 1.000000000000000000, 0.9659258262890683122, 1.000000000000000000, 0.9659258262890683122, 1.000000000000000000, 0.9659258262890683122, 1.000000000000000000, 0.9659258262890683122, 1.000000000000000000, 0.9659258262890683122, 1.000000000000000000, 0.9659258262890678681, 1.000000000000000444 ) ) 
 REPRESENTATION_ITEM ( '' )  );
#77750 = SURFACE_SIDE_STYLE ('',( #42274 ) ) ;
#77751 = FACE_OUTER_BOUND ( 'NONE', #88407, .T. ) ;
#77752 = LINE ( 'NONE', #4200, #79258 ) ;
#77753 = VERTEX_POINT ( 'NONE', #58568 ) ;
#77754 = FACE_OUTER_BOUND ( 'NONE', #1183, .T. ) ;
#77755 = DIRECTION ( 'NONE',  ( -1.000000000000000000, -0.000000000000000000, -0.000000000000000000 ) ) ;
#77756 = PLANE ( 'NONE',  #116486 ) ;
#77757 = ADVANCED_FACE ( 'NONE', ( #22980 ), #57113, .F. ) ;
#77758 = DIRECTION ( 'NONE',  ( -0.7071067811865487940, 0.7071067811865463515, -0.000000000000000000 ) ) ;
#77759 = CARTESIAN_POINT ( 'NONE',  ( 26.59959685856477307, -6.109999999999998543, -1.637169565754160727 ) ) ;
#77760 = DIRECTION ( 'NONE',  ( -1.000000000000000000, -1.224606353822377258E-16, -0.000000000000000000 ) ) ;
#77761 = ORIENTED_EDGE ( 'NONE', *, *, #98984, .F. ) ;
#77762 = ORIENTED_EDGE ( 'NONE', *, *, #122820, .T. ) ;
#77763 = DIRECTION ( 'NONE',  ( 0.7071067811865487940, 0.7071067811865463515, 0.000000000000000000 ) ) ;
#77764 = VERTEX_POINT ( 'NONE', #67248 ) ;
#77765 = EDGE_LOOP ( 'NONE', ( #48005, #71769, #26718, #17765 ) ) ;
#77766 = EDGE_CURVE ( 'NONE', #22361, #120155, #90418, .T. ) ;
#77767 = LINE ( 'NONE', #56037, #133538 ) ;
#77768 = CARTESIAN_POINT ( 'NONE',  ( 23.29298673570678346, -21.74070752338406720, 4.999753212805222446 ) ) ;
#77769 = ORIENTED_EDGE ( 'NONE', *, *, #54787, .F. ) ;
#77770 = PLANE ( 'NONE',  #11443 ) ;
#77771 = CARTESIAN_POINT ( 'NONE',  ( 25.40000000000000568, 3.739651257385445238, 5.035049619000475651 ) ) ;
#77772 = FACE_OUTER_BOUND ( 'NONE', #122981, .T. ) ;
#77773 = DIRECTION ( 'NONE',  ( -0.7071067811865486830, 0.7071067811865464625, 0.000000000000000000 ) ) ;
#77774 = CARTESIAN_POINT ( 'NONE',  ( 126.4379301918981042, -6.110000000000001208, 1.637169565754158951 ) ) ;
#77775 = ORIENTED_EDGE ( 'NONE', *, *, #25610, .T. ) ;
#77776 = EDGE_CURVE ( 'NONE', #73203, #88923, #1241, .T. ) ;
#77777 = CARTESIAN_POINT ( 'NONE',  ( -34.49999999999976552, 7.464255608400418573, 4.994342998332163219 ) ) ;
#77778 = DIRECTION ( 'NONE',  ( 0.6830127018922180770, -0.6830127018922204085, -0.2588190451025213501 ) ) ;
#77779 = DIRECTION ( 'NONE',  ( 1.000000000000000000, 0.000000000000000000, 0.000000000000000000 ) ) ;
#77780 = DIRECTION ( 'NONE',  ( -0.6830127018922181881, 0.6830127018922202975, -0.2588190451025214056 ) ) ;
#77781 = DIRECTION ( 'NONE',  ( -0.000000000000000000, 0.3543493200069153248, 0.9351131265310292928 ) ) ;
#77782 = DIRECTION ( 'NONE',  ( 1.000000000000000000, 0.000000000000000000, 0.000000000000000000 ) ) ;
#77783 = CARTESIAN_POINT ( 'NONE',  ( 47.03752705046289151, -9.735942053221456900E-16, 7.949999999999998401 ) ) ;
#77784 = EDGE_CURVE ( 'NONE', #121955, #22749, #35358, .T. ) ;
#77785 = AXIS2_PLACEMENT_3D ( 'NONE', #71762, #135589, #49307 ) ;
#77786 = LINE ( 'NONE', #121966, #90764 ) ;
#77787 = CARTESIAN_POINT ( 'NONE',  ( -18.18398860626898994, 28.73617430169800002, 5.000000000000000000 ) ) ;
#77788 = ORIENTED_EDGE ( 'NONE', *, *, #75952, .F. ) ;
#77789 = VERTEX_POINT ( 'NONE', #3384 ) ;
#77790 = CARTESIAN_POINT ( 'NONE',  ( 40.95833333333333570, 3.974999999999997424, 6.884901960086288852 ) ) ;
#77791 = AXIS2_PLACEMENT_3D ( 'NONE', #51795, #95268, #108981 ) ;
#77792 = PLANE ( 'NONE',  #34457 ) ;
#77793 = CARTESIAN_POINT ( 'NONE',  ( 31.17183060077625001, -17.24070752338410628, 4.000000000000000000 ) ) ;
#77794 = ORIENTED_EDGE ( 'NONE', *, *, #32490, .T. ) ;
#77795 = PLANE ( 'NONE',  #54847 ) ;
#77796 = LINE ( 'NONE', #19116, #60841 ) ;
#77797 = CARTESIAN_POINT ( 'NONE',  ( 37.62543019189811133, 5.291415217122919401, 3.055000000000002824 ) ) ;
#77799 = ORIENTED_EDGE ( 'NONE', *, *, #90005, .F. ) ;
#77798 = VECTOR ( 'NONE', #114125, 1000.000000000000000 ) ;
#77800 = CARTESIAN_POINT ( 'NONE',  ( 0.1600000000000028066, 0.5691893105020771060, -7.934999999999987175 ) ) ;
#77801 = VERTEX_POINT ( 'NONE', #123789 ) ;
#77802 = ORIENTED_EDGE ( 'NONE', *, *, #71416, .T. ) ;
#77803 = DIRECTION ( 'NONE',  ( -0.000000000000000000, 0.000000000000000000, 1.000000000000000000 ) ) ;
#77804 = CARTESIAN_POINT ( 'NONE',  ( 9.208651418775088970, 2.500000000000000444, 0.000000000000000000 ) ) ;
#77805 = PRESENTATION_STYLE_ASSIGNMENT (( #79275 ) ) ;
#77806 = CARTESIAN_POINT ( 'NONE',  ( 21.70710678118638981, -15.74070752338412404, 5.000000000000000000 ) ) ;
#77807 = ORIENTED_EDGE ( 'NONE', *, *, #10153, .T. ) ;
#77808 = CARTESIAN_POINT ( 'NONE',  ( -4.499999999999967137, 3.052185695429136647, 5.000000000000000000 ) ) ;
#77809 = ORIENTED_EDGE ( 'NONE', *, *, #131568, .F. ) ;
#77810 = CARTESIAN_POINT ( 'NONE',  ( 83.27126352523143282, 4.472830434245838482, 4.472830434245842035 ) ) ;
#77811 = CARTESIAN_POINT ( 'NONE',  ( 0.000000000000000000, 0.000000000000000000, 5.000000000000000000 ) ) ;
#77812 =( NAMED_UNIT ( * ) SI_UNIT ( $, .STERADIAN. ) SOLID_ANGLE_UNIT ( ) );
#77813 = CARTESIAN_POINT ( 'NONE',  ( -4.499999999999968914, -4.796895815301026822, -3.611700055028691292 ) ) ;
#77814 = CARTESIAN_POINT ( 'NONE',  ( -66.48921356237309510, -27.52281430457101763, 5.000000000000000000 ) ) ;
#77815 = VECTOR ( 'NONE', #103438, 1000.000000000000000 ) ;
#77816 = VECTOR ( 'NONE', #61946, 999.9999999999998863 ) ;
#77817 = ORIENTED_EDGE ( 'NONE', *, *, #124042, .F. ) ;
#77818 = DIRECTION ( 'NONE',  ( -0.000000000000000000, 0.3543493200069153248, 0.9351131265310292928 ) ) ;
#77819 = CARTESIAN_POINT ( 'NONE',  ( 60.87043019189810877, -3.055000000000001492, 5.291415217122917625 ) ) ;
#77820 = CARTESIAN_POINT ( 'NONE',  ( -25.01459476339044130, 2.945717840782780428, 4.000000000000000000 ) ) ;
#77821 = DIRECTION ( 'NONE',  ( -0.000000000000000000, 0.3543493200069153248, 0.9351131265310291818 ) ) ;
#77822 = CARTESIAN_POINT ( 'NONE',  ( 10.17183060077640100, 0.7592924766157104211, 4.000000000000000000 ) ) ;
#77823 = EDGE_CURVE ( 'NONE', #137750, #53081, #125192, .T. ) ;
#77824 = ORIENTED_EDGE ( 'NONE', *, *, #68805, .T. ) ;
#77825 = AXIS2_PLACEMENT_3D ( 'NONE', #87742, #110884, #111639 ) ;
#77826 = LINE ( 'NONE', #124889, #86321 ) ;
#77827 = SURFACE_SIDE_STYLE ('',( #122011 ) ) ;
#77828 = ORIENTED_EDGE ( 'NONE', *, *, #55397, .T. ) ;
#77829 = DIRECTION ( 'NONE',  ( -0.7071067811865486830, -0.7071067811865464625, -0.000000000000000000 ) ) ;
#77830 = ORIENTED_EDGE ( 'NONE', *, *, #21916, .T. ) ;
#77831 = CARTESIAN_POINT ( 'NONE',  ( 66.48921356237309510, -27.52281430457101763, 5.000000000000000000 ) ) ;
#77832 = DIRECTION ( 'NONE',  ( -0.000000000000000000, 0.000000000000000000, 1.000000000000000000 ) ) ;
#77833 = CARTESIAN_POINT ( 'NONE',  ( 39.48921356237310221, -27.52281430457082934, 5.000000000000000000 ) ) ;
#77834 = ADVANCED_FACE ( 'NONE', ( #85780 ), #141608, .F. ) ;
#77835 = FACE_BOUND ( 'NONE', #9189, .T. ) ;
#77836 = DIRECTION ( 'NONE',  ( 0.7071067811865486830, -0.7071067811865464625, -0.000000000000000000 ) ) ;
#77837 = FACE_OUTER_BOUND ( 'NONE', #52001, .T. ) ;
#77838 = EDGE_CURVE ( 'NONE', #6035, #28590, #57260, .T. ) ;
#77839 = FACE_OUTER_BOUND ( 'NONE', #10964, .T. ) ;
#77841 = VERTEX_POINT ( 'NONE', #130010 ) ;
#77840 = FACE_OUTER_BOUND ( 'NONE', #47887, .T. ) ;
#77842 = DIRECTION ( 'NONE',  ( -1.000000000000000000, -0.000000000000000000, -0.000000000000000000 ) ) ;
#77843 = EDGE_LOOP ( 'NONE', ( #90724, #64210, #21519, #109960 ) ) ;
#77844 = ORIENTED_EDGE ( 'NONE', *, *, #60045, .T. ) ;
#77845 = CARTESIAN_POINT ( 'NONE',  ( 78.80793019189810877, -6.109999999999998543, 1.637169565754158507 ) ) ;
#77846 = ORIENTED_EDGE ( 'NONE', *, *, #21443, .T. ) ;
#77847 = DIRECTION ( 'NONE',  ( 0.000000000000000000, -1.000000000000000000, 0.000000000000000000 ) ) ;
#77848 = EDGE_CURVE ( 'NONE', #32886, #116795, #61415, .T. ) ;
#77849 = DIRECTION ( 'NONE',  ( 0.000000000000000000, 0.000000000000000000, -1.000000000000000000 ) ) ;
#77850 = EDGE_LOOP ( 'NONE', ( #53813, #45568, #4907, #98447 ) ) ;
#77851 = PLANE ( 'NONE',  #106877 ) ;
#77852 = VECTOR ( 'NONE', #44838, 1000.000000000000000 ) ;
#77853 = ADVANCED_FACE ( 'NONE', ( #114987 ), #82414, .T. ) ;
#77854 = DIRECTION ( 'NONE',  ( 0.7071067811865486830, -0.7071067811865464625, -0.000000000000000000 ) ) ;
#77855 = CARTESIAN_POINT ( 'NONE',  ( -21.29974487139158512, -27.71228299555221142, 4.000000000000000000 ) ) ;
#77856 = CARTESIAN_POINT ( 'NONE',  ( 69.48921356237309510, -27.52281430457103895, 5.000000000000000000 ) ) ;
#77858 = PLANE ( 'NONE',  #114445 ) ;
#77857 = DIRECTION ( 'NONE',  ( 0.7071067811865487940, -0.7071067811865463515, 0.000000000000000000 ) ) ;
#77859 = FACE_OUTER_BOUND ( 'NONE', #115142, .T. ) ;
#77860 = CARTESIAN_POINT ( 'NONE',  ( 15.48921356237309510, -27.52281430457066236, 5.000000000000000000 ) ) ;
#77861 = ORIENTED_EDGE ( 'NONE', *, *, #74587, .T. ) ;
#77862 = AXIS2_PLACEMENT_3D ( 'NONE', #125733, #11938, #135196 ) ;
#77863 = ADVANCED_FACE ( 'NONE', ( #72293 ), #140860, .F. ) ;
#77864 = SURFACE_SIDE_STYLE ('',( #126863 ) ) ;
#77865 = ADVANCED_FACE ( 'NONE', ( #26596 ), #79244, .T. ) ;
#77866 = VERTEX_POINT ( 'NONE', #116457 ) ;
#77867 = CARTESIAN_POINT ( 'NONE',  ( 57.18398860626899705, 28.73617430169827358, 5.000000000000000000 ) ) ;
#77868 = CARTESIAN_POINT ( 'NONE',  ( -33.70710678118630454, -18.74070752338409562, 5.000000000000000000 ) ) ;
#77869 = ORIENTED_EDGE ( 'NONE', *, *, #60669, .T. ) ;
#77870 = VERTEX_POINT ( 'NONE', #27287 ) ;
#77871 = ORIENTED_EDGE ( 'NONE', *, *, #65246, .F. ) ;
#77872 = CARTESIAN_POINT ( 'NONE',  ( 69.18398860626899705, 28.73617430169835529, 5.000000000000000000 ) ) ;
#77873 = VERTEX_POINT ( 'NONE', #4062 ) ;
#77874 = CARTESIAN_POINT ( 'NONE',  ( 174.7500000000000000, 7.919999999999947526, 16.57230000000005532 ) ) ;
#77875 = AXIS2_PLACEMENT_3D ( 'NONE', #60590, #138114, #136671 ) ;
#77876 = CARTESIAN_POINT ( 'NONE',  ( -57.18398860626899705, 28.73617430169827358, 5.000000000000000000 ) ) ;
#77877 = CARTESIAN_POINT ( 'NONE',  ( 30.52497294953710494, -4.461849672132299993, -4.461849672132299105 ) ) ;
#77878 = CARTESIAN_POINT ( 'NONE',  ( 0.7307956238753654521, -0.4000000000000004108, 2.467792535850613866 ) ) ;
#77879 = ORIENTED_EDGE ( 'NONE', *, *, #45037, .T. ) ;
#77880 = VECTOR ( 'NONE', #137561, 1000.000000000000227 ) ;
#77881 = FACE_OUTER_BOUND ( 'NONE', #119109, .T. ) ;
#77882 = EDGE_CURVE ( 'NONE', #138848, #16402, #104861, .T. ) ;
#77883 = DIRECTION ( 'NONE',  ( -0.6830127018922181881, 0.6830127018922202975, -0.2588190451025214056 ) ) ;
#77884 = CARTESIAN_POINT ( 'NONE',  ( -3.183988606268992161, 28.73617430169789699, 5.000000000000000000 ) ) ;
#77886 = ORIENTED_EDGE ( 'NONE', *, *, #44212, .F. ) ;
#77885 = DIRECTION ( 'NONE',  ( -0.000000000000000000, 0.000000000000000000, 1.000000000000000000 ) ) ;
#77887 = ORIENTED_EDGE ( 'NONE', *, *, #23922, .T. ) ;
#77888 = LINE ( 'NONE', #22053, #130247 ) ;
#77889 = ADVANCED_FACE ( 'NONE', ( #30719 ), #70837, .F. ) ;
#77890 = ADVANCED_FACE ( 'NONE', ( #49807 ), #90806, .T. ) ;
#77891 = CARTESIAN_POINT ( 'NONE',  ( -9.707013264292978505, -21.74070752338405654, 4.999753212805220670 ) ) ;
#77892 = EDGE_LOOP ( 'NONE', ( #80148, #123980, #109783, #40435 ) ) ;
#77893 = LINE ( 'NONE', #67015, #78209 ) ;
#77894 = CARTESIAN_POINT ( 'NONE',  ( 15.18398860626900237, 28.73617430169797871, 5.000000000000000000 ) ) ;
#77895 = EDGE_LOOP ( 'NONE', ( #132072, #44030, #83934, #67915 ) ) ;
#77896 = VECTOR ( 'NONE', #429, 1000.000000000000227 ) ;
#77897 = DIRECTION ( 'NONE',  ( 0.7071067811865486830, -0.7071067811865464625, -0.000000000000000000 ) ) ;
#77898 = DIRECTION ( 'NONE',  ( 0.7071067811865487940, 0.7071067811865463515, 0.000000000000000000 ) ) ;
#77899 = CARTESIAN_POINT ( 'NONE',  ( 13.46247294953710494, -7.464222240803106570E-16, -6.094999999999989981 ) ) ;
#77900 = DIRECTION ( 'NONE',  ( 0.000000000000000000, 0.000000000000000000, -1.000000000000000000 ) ) ;
#77901 = EDGE_CURVE ( 'NONE', #131775, #73925, #83122, .T. ) ;
#77902 = CARTESIAN_POINT ( 'NONE',  ( -36.48921356237310221, -27.52281430457080802, 5.000000000000000000 ) ) ;
#77903 = DIRECTION ( 'NONE',  ( 0.7071067811865487940, -0.7071067811865463515, 0.000000000000000000 ) ) ;
#77904 = CARTESIAN_POINT ( 'NONE',  ( -36.13499573751600735, 3.759292476615678336, 15.36553568819734572 ) ) ;
#77905 = COLOUR_RGB ( '', 0.72549020, 0.75294118, 0.79215686) ;
#77906 = EDGE_CURVE ( 'NONE', #87440, #82359, #122688, .T. ) ;
#77907 = DIRECTION ( 'NONE',  ( 0.3543493200069162685, -0.000000000000000000, -0.9351131265310288487 ) ) ;
#77908 = ORIENTED_EDGE ( 'NONE', *, *, #139333, .T. ) ;
#77909 = ADVANCED_FACE ( 'NONE', ( #33582 ), #10351, .F. ) ;
#77910 = DIRECTION ( 'NONE',  ( 0.7071067811865486830, -0.7071067811865464625, -0.000000000000000000 ) ) ;
#77911 = ORIENTED_EDGE ( 'NONE', *, *, #79276, .T. ) ;
#77912 = DIRECTION ( 'NONE',  ( 0.7071067811865487940, 0.7071067811865463515, -0.000000000000000000 ) ) ;
#77913 = DIRECTION ( 'NONE',  ( -0.000000000000000000, -0.3543493200069152693, 0.9351131265310292928 ) ) ;
#77914 = AXIS2_PLACEMENT_3D ( 'NONE', #27866, #104711, #5378 ) ;
#77915 = AXIS2_PLACEMENT_3D ( 'NONE', #81581, #69265, #80154 ) ;
#77916 = LINE ( 'NONE', #11172, #3471 ) ;
#77917 = CARTESIAN_POINT ( 'NONE',  ( 20.29289321881331887, 20.25929247661551713, 5.000000000000000000 ) ) ;
#77918 = VECTOR ( 'NONE', #74061, 999.9999999999998863 ) ;
#77919 = EDGE_CURVE ( 'NONE', #109689, #94724, #54605, .T. ) ;
#77920 = ORIENTED_EDGE ( 'NONE', *, *, #70884, .T. ) ;
#77921 = LINE ( 'NONE', #113370, #18334 ) ;
#77922 = CARTESIAN_POINT ( 'NONE',  ( 2.602085213965210642E-15, 19.55218569542897100, 5.000000000000000000 ) ) ;
#77923 = EDGE_CURVE ( 'NONE', #143372, #7797, #12499, .T. ) ;
#77924 = DIRECTION ( 'NONE',  ( -0.7071067811865487940, 0.7071067811865463515, 0.000000000000000000 ) ) ;
#77925 = ORIENTED_EDGE ( 'NONE', *, *, #20982, .T. ) ;
#77926 = CARTESIAN_POINT ( 'NONE',  ( -31.49999999999977973, 6.277155672890242677, -3.510561720658869067 ) ) ;
#77927 = DIRECTION ( 'NONE',  ( 0.7071067811865487940, 0.7071067811865463515, 0.000000000000000000 ) ) ;
#77928 = UNCERTAINTY_MEASURE_WITH_UNIT (LENGTH_MEASURE( 1.000000000000000082E-05 ), #7896, 'distance_accuracy_value', 'NONE');
#77929 = DIRECTION ( 'NONE',  ( 0.000000000000000000, 1.000000000000000000, 0.000000000000000000 ) ) ;
#77930 = AXIS2_PLACEMENT_3D ( 'NONE', #106418, #71715, #139109 ) ;
#77931 = FACE_OUTER_BOUND ( 'NONE', #32273, .T. ) ;
#77932 = EDGE_CURVE ( 'NONE', #50763, #131707, #119812, .T. ) ;
#77933 = CARTESIAN_POINT ( 'NONE',  ( 58.24543019189810877, -5.291415217122919401, -3.055000000000000604 ) ) ;
#77934 = PLANE ( 'NONE',  #132157 ) ;
#77935 = CARTESIAN_POINT ( 'NONE',  ( 16.49230000000001439, 3.130000000000008331, -22.35000000000000142 ) ) ;
#77936 = CARTESIAN_POINT ( 'NONE',  ( 61.46640106136307935, -49.14999999999999147, 40.92499999999998295 ) ) ;
#77937 = CARTESIAN_POINT ( 'NONE',  ( 18.29974487139159223, -27.71228299555219010, 4.000000000000000000 ) ) ;
#77938 = ORIENTED_EDGE ( 'NONE', *, *, #128523, .F. ) ;
#77939 = VERTEX_POINT ( 'NONE', #65502 ) ;
#77940 = LINE ( 'NONE', #97522, #13054 ) ;
#77941 = PLANE ( 'NONE',  #8333 ) ;
#77942 = CARTESIAN_POINT ( 'NONE',  ( 20.81601139373100295, 28.73617430169773002, 5.000000000000000000 ) ) ;
#77943 = DIRECTION ( 'NONE',  ( -0.7071067811865486830, -0.7071067811865464625, 0.000000000000000000 ) ) ;
#77944 = FACE_OUTER_BOUND ( 'NONE', #54264, .T. ) ;
#77945 = DIRECTION ( 'NONE',  ( -0.000000000000000000, 0.000000000000000000, 1.000000000000000000 ) ) ;
#77946 = ORIENTED_EDGE ( 'NONE', *, *, #90825, .F. ) ;
#77947 = ORIENTED_EDGE ( 'NONE', *, *, #100564, .T. ) ;
#77948 = DIRECTION ( 'NONE',  ( -0.6830127018922180770, -0.6830127018922204085, -0.2588190451025213501 ) ) ;
#77949 = CARTESIAN_POINT ( 'NONE',  ( 18.71247294953710494, 0.000000000000000000, 6.094999999999989981 ) ) ;
#77950 = UNCERTAINTY_MEASURE_WITH_UNIT (LENGTH_MEASURE( 1.000000000000000082E-05 ), #117504, 'distance_accuracy_value', 'NONE');
#77951 = EDGE_CURVE ( 'NONE', #31681, #119020, #143026, .T. ) ;
#77952 = CARTESIAN_POINT ( 'NONE',  ( -22.49999999999984368, -8.568876922607728375, 4.000000000000000000 ) ) ;
#77954 = EDGE_CURVE ( 'NONE', #61275, #24150, #88945, .T. ) ;
#77953 = CARTESIAN_POINT ( 'NONE',  ( 16.81663961620377279, -1.633150327867672447, -6.094999999999999751 ) ) ;
#77955 = CARTESIAN_POINT ( 'NONE',  ( 87.28752705046288440, 0.000000000000000000, -7.949999999999998401 ) ) ;
#77957 = EDGE_CURVE ( 'NONE', #116108, #81904, #894, .T. ) ;
#77956 = FACE_OUTER_BOUND ( 'NONE', #107386, .T. ) ;
#77958 = AXIS2_PLACEMENT_3D ( 'NONE', #76095, #97080, #120264 ) ;
#77959 = CARTESIAN_POINT ( 'NONE',  ( 17.06332250466817158, 2.500000000000000444, 0.000000000000000000 ) ) ;
#77960 = ORIENTED_EDGE ( 'NONE', *, *, #138817, .F. ) ;
#77961 = CARTESIAN_POINT ( 'NONE',  ( 69.83333333333332860, -6.884901960086287964, 3.974999999999998312 ) ) ;
#77962 = DIRECTION ( 'NONE',  ( 1.000000000000000000, 0.000000000000000000, 0.000000000000000000 ) ) ;
#77963 = DIRECTION ( 'NONE',  ( -0.7071067811865487940, 0.7071067811865463515, 0.000000000000000000 ) ) ;
#77964 = CARTESIAN_POINT ( 'NONE',  ( 69.18398860626899705, 28.73617430169835529, 5.000000000000000000 ) ) ;
#77965 = VECTOR ( 'NONE', #36260, 1000.000000000000227 ) ;
#77966 = VERTEX_POINT ( 'NONE', #56054 ) ;
#77967 = ADVANCED_FACE ( 'NONE', ( #53907 ), #45182, .F. ) ;
#77968 =( BOUNDED_CURVE ( )  B_SPLINE_CURVE ( 3, ( #89306, #13140, #12442, #87874 ),
 .UNSPECIFIED., .F., .F. ) 
 B_SPLINE_CURVE_WITH_KNOTS ( ( 4, 4 ),
 ( 4.712388980384689674, 6.105785702739209064 ),
 .UNSPECIFIED. ) 
 CURVE ( )  GEOMETRIC_REPRESENTATION_ITEM ( )  RATIONAL_B_SPLINE_CURVE ( ( 1.000000000000000000, 0.8446433258982484205, 0.8446433258982484205, 1.000000000000000000 ) ) 
 REPRESENTATION_ITEM ( '' )  );
#77969 = DIRECTION ( 'NONE',  ( 0.000000000000000000, 0.000000000000000000, 1.000000000000000000 ) ) ;
#77970 = ORIENTED_EDGE ( 'NONE', *, *, #54584, .F. ) ;
#77971 = DIRECTION ( 'NONE',  ( -0.000000000000000000, 0.000000000000000000, 1.000000000000000000 ) ) ;
#77972 = CARTESIAN_POINT ( 'NONE',  ( 66.64626352523144703, -4.472830434245840259, 4.472830434245839371 ) ) ;
#77973 = LINE ( 'NONE', #22821, #6087 ) ;
#77974 = AXIS2_PLACEMENT_3D ( 'NONE', #82763, #4401, #92908 ) ;
#77975 = ORIENTED_EDGE ( 'NONE', *, *, #41029, .T. ) ;
#77976 = CARTESIAN_POINT ( 'NONE',  ( 17.29289321881333308, -3.740707523384244837, 5.000000000000000000 ) ) ;
#77977 =( BOUNDED_CURVE ( )  B_SPLINE_CURVE ( 2, ( #64791, #58052, #53175, #2158, #98819, #87959, #77120, #9666, #20534, #8906, #130045, #10379, #30747 ),
 .UNSPECIFIED., .F., .T. ) 
 B_SPLINE_CURVE_WITH_KNOTS ( ( 3, 2, 2, 2, 2, 2, 3 ),
 ( 0.3000000000000000444, 0.3083333333333334036, 0.3166666666666667074, 0.3250000000000000666, 0.3333333333333333703, 0.3416666666666667296, 0.3500000000000000333 ),
 .UNSPECIFIED. ) 
 CURVE ( )  GEOMETRIC_REPRESENTATION_ITEM ( )  RATIONAL_B_SPLINE_CURVE ( ( 0.9999999999999997780, 0.9659258262890685343, 1.000000000000000000, 0.9659258262890683122, 1.000000000000000000, 0.9659258262890683122, 1.000000000000000000, 0.9659258262890683122, 1.000000000000000000, 0.9659258262890683122, 1.000000000000000000, 0.9659258262890680902, 1.000000000000000222 ) ) 
 REPRESENTATION_ITEM ( '' )  );
#77978 = CARTESIAN_POINT ( 'NONE',  ( -7.499999999999951150, 13.56627193232214523, -10.57019076586070483 ) ) ;
#77979 = DIRECTION ( 'NONE',  ( -0.000000000000000000, 0.3543493200069153248, 0.9351131265310292928 ) ) ;
#77980 = VECTOR ( 'NONE', #106495, 1000.000000000000000 ) ;
#77981 = CARTESIAN_POINT ( 'NONE',  ( 43.58333333333333570, 6.884901960086290629, -3.974999999999994316 ) ) ;
#77982 = CARTESIAN_POINT ( 'NONE',  ( -30.70710678118632231, -15.74070752338412760, 5.000000000000000000 ) ) ;
#77984 = ORIENTED_EDGE ( 'NONE', *, *, #62543, .T. ) ;
#77983 = DIRECTION ( 'NONE',  ( 0.000000000000000000, -1.000000000000000000, 0.000000000000000000 ) ) ;
#77985 = DIRECTION ( 'NONE',  ( 0.7071067811865487940, 0.7071067811865463515, 0.000000000000000000 ) ) ;
#77986 = DIRECTION ( 'NONE',  ( 0.7071067811865487940, 0.7071067811865463515, 0.000000000000000000 ) ) ;
#77987 = LINE ( 'NONE', #46086, #135106 ) ;
#77988 = CARTESIAN_POINT ( 'NONE',  ( -23.70025512860841133, -27.71228299555189523, 4.000000000000000000 ) ) ;
#77989 = ORIENTED_EDGE ( 'NONE', *, *, #3551, .F. ) ;
#77990 = MECHANICAL_DESIGN_GEOMETRIC_PRESENTATION_REPRESENTATION (  '', ( #45615 ), #89558 ) ;
#77991 = ORIENTED_EDGE ( 'NONE', *, *, #82369, .T. ) ;
#77992 = CARTESIAN_POINT ( 'NONE',  ( 68.10459685856474721, 1.637169565754164946, -6.109999999999999432 ) ) ;
#77993 = VERTEX_POINT ( 'NONE', #89358 ) ;
#77994 = VECTOR ( 'NONE', #91045, 999.9999999999998863 ) ;
#77996 = DIRECTION ( 'NONE',  ( 0.7071067811865487940, 0.7071067811865463515, -0.000000000000000000 ) ) ;
#77995 = PRODUCT_DEFINITION_SHAPE ( 'NONE', 'NONE',  #82917 ) ;
#77997 = CARTESIAN_POINT ( 'NONE',  ( -31.82816939922330945, -8.240707523384191546, 4.000000000000000000 ) ) ;
#77998 = LINE ( 'NONE', #68560, #75779 ) ;
#77999 = AXIS2_PLACEMENT_3D ( 'NONE', #119810, #87924, #20500 ) ;
#78000 = CARTESIAN_POINT ( 'NONE',  ( 124.9125270504628986, -7.949999999999998401, -4.867971026610728450E-16 ) ) ;
#78001 = CARTESIAN_POINT ( 'NONE',  ( 54.95833333333332860, 3.974999999999997424, 6.884901960086288852 ) ) ;
#78002 = ORIENTED_EDGE ( 'NONE', *, *, #58024, .T. ) ;
#78003 = ORIENTED_EDGE ( 'NONE', *, *, #81944, .F. ) ;
#78004 = CARTESIAN_POINT ( 'NONE',  ( 21.15294044719737698, 3.061616997868383634E-16, -2.500000000000000444 ) ) ;
#78005 = CARTESIAN_POINT ( 'NONE',  ( -17.43071299949562558, -2.562240267135510230, -33.48616200217535521 ) ) ;
#78006 = ORIENTED_EDGE ( 'NONE', *, *, #44034, .T. ) ;
#78007 = DIRECTION ( 'NONE',  ( 0.000000000000000000, 0.000000000000000000, 1.000000000000000000 ) ) ;
#78008 = CARTESIAN_POINT ( 'NONE',  ( 113.5375270504628986, -9.735942053221456900E-16, 7.949999999999998401 ) ) ;
#78009 = DIRECTION ( 'NONE',  ( -0.7071067811865486830, -0.7071067811865464625, -0.000000000000000000 ) ) ;
#78010 = ORIENTED_EDGE ( 'NONE', *, *, #70993, .F. ) ;
#78011 = EDGE_CURVE ( 'NONE', #44918, #138069, #45882, .T. ) ;
#78012 = VECTOR ( 'NONE', #63578, 1000.000000000000227 ) ;
#78013 = EDGE_CURVE ( 'NONE', #73316, #58598, #77087, .T. ) ;
#78014 = FACE_BOUND ( 'NONE', #127764, .T. ) ;
#78015 = DIRECTION ( 'NONE',  ( -1.000000000000000000, -1.224606353822377258E-16, -0.000000000000000000 ) ) ;
#78016 = DIRECTION ( 'NONE',  ( -0.7071067811865487940, 0.7071067811865463515, 0.000000000000000000 ) ) ;
#78017 = LINE ( 'NONE', #44714, #8802 ) ;
#78018 = CARTESIAN_POINT ( 'NONE',  ( 31.60343192894623954, -14.24070752338412582, 19.24067776001733066 ) ) ;
#78019 = VECTOR ( 'NONE', #10219, 1000.000000000000000 ) ;
#78021 = ADVANCED_FACE ( 'NONE', ( #87926, #44460 ), #67645, .F. ) ;
#78020 = VECTOR ( 'NONE', #110236, 1000.000000000000000 ) ;
#78022 = ADVANCED_FACE ( 'NONE', ( #120517 ), #121962, .F. ) ;
#78023 = LINE ( 'NONE', #135272, #78987 ) ;
#78024 = DIRECTION ( 'NONE',  ( 0.000000000000000000, 1.665334536937735304E-16, -1.000000000000000000 ) ) ;
#78025 = ORIENTED_EDGE ( 'NONE', *, *, #79441, .T. ) ;
#78026 = VECTOR ( 'NONE', #16409, 1000.000000000000000 ) ;
#78027 = ORIENTED_EDGE ( 'NONE', *, *, #56957, .F. ) ;
#78028 = CARTESIAN_POINT ( 'NONE',  ( 101.5579301918981088, 6.110000000000000320, -1.637169565754156064 ) ) ;
#78029 = VERTEX_POINT ( 'NONE', #76350 ) ;
#78030 = ADVANCED_FACE ( 'NONE', ( #132898 ), #78491, .F. ) ;
#78031 = FACE_OUTER_BOUND ( 'NONE', #43438, .T. ) ;
#78032 = VERTEX_POINT ( 'NONE', #21244 ) ;
#78033 = VECTOR ( 'NONE', #24470, 999.9999999999998863 ) ;
#78034 = VECTOR ( 'NONE', #40721, 1000.000000000000000 ) ;
#78035 = DIRECTION ( 'NONE',  ( 0.000000000000000000, 0.000000000000000000, -1.000000000000000000 ) ) ;
#78036 = CARTESIAN_POINT ( 'NONE',  ( 6.758600742197917732, 21.72500000000000142, 5.000000000000000000 ) ) ;
#78037 = EDGE_CURVE ( 'NONE', #24063, #111037, #100939, .T. ) ;
#78038 = PLANE ( 'NONE',  #33261 ) ;
#78039 = ORIENTED_EDGE ( 'NONE', *, *, #9165, .T. ) ;
#78040 = CARTESIAN_POINT ( 'NONE',  ( 1.629999999999999893, 4.202752102959690472E-16, -4.330509084666861676E-16 ) ) ;
#78041 = DIRECTION ( 'NONE',  ( -0.7071067811865486830, 0.7071067811865464625, 0.000000000000000000 ) ) ;
#78042 = CARTESIAN_POINT ( 'NONE',  ( -12.18398860626900060, 28.73617430169795739, 5.000000000000000000 ) ) ;
#78043 = DIRECTION ( 'NONE',  ( -0.3543493200069162685, -0.000000000000000000, -0.9351131265310288487 ) ) ;
#78044 = PLANE ( 'NONE',  #50416 ) ;
#78045 = EDGE_CURVE ( 'NONE', #33966, #115267, #72089, .T. ) ;
#78046 = DIRECTION ( 'NONE',  ( 0.7071067811865487940, 0.7071067811865463515, -0.000000000000000000 ) ) ;
#78047 = VERTEX_POINT ( 'NONE', #87221 ) ;
#78048 = CARTESIAN_POINT ( 'NONE',  ( -0.1839886062690032631, 28.73617430169787568, 5.000000000000000000 ) ) ;
#78049 = CARTESIAN_POINT ( 'NONE',  ( 8.671830600776413434, -6.740707523384218192, 4.000000000000000000 ) ) ;
#78050 = ORIENTED_EDGE ( 'NONE', *, *, #135406, .F. ) ;
#78051 = ORIENTED_EDGE ( 'NONE', *, *, #120168, .T. ) ;
#78052 = ORIENTED_EDGE ( 'NONE', *, *, #19935, .T. ) ;
#78053 = CARTESIAN_POINT ( 'NONE',  ( 53.37543019189811133, -5.291415217122920289, -3.055000000000001492 ) ) ;
#78054 = VECTOR ( 'NONE', #80218, 1000.000000000000000 ) ;
#78055 = EDGE_CURVE ( 'NONE', #49512, #31384, #5167, .T. ) ;
#78056 = ORIENTED_EDGE ( 'NONE', *, *, #92520, .T. ) ;
#78057 = FACE_OUTER_BOUND ( 'NONE', #62725, .T. ) ;
#78058 = VECTOR ( 'NONE', #123658, 1000.000000000000000 ) ;
#78059 = FACE_OUTER_BOUND ( 'NONE', #71124, .T. ) ;
#78060 = CARTESIAN_POINT ( 'NONE',  ( 91.29209685856477563, -5.291415217122921177, 3.054999999999999272 ) ) ;
#78061 = CARTESIAN_POINT ( 'NONE',  ( -14.20710678118644665, 6.759292476615649470, 5.000000000000000000 ) ) ;
#78062 = EDGE_CURVE ( 'NONE', #88361, #141224, #48022, .T. ) ;
#78063 = EDGE_LOOP ( 'NONE', ( #18856, #74168, #76250 ) ) ;
#78064 = DIRECTION ( 'NONE',  ( 0.7071067811865487940, -0.7071067811865463515, 0.000000000000000000 ) ) ;
#78065 = VECTOR ( 'NONE', #11427, 1000.000000000000227 ) ;
#78066 = CARTESIAN_POINT ( 'NONE',  ( 18.63999999999999702, -2.055000000000000160, 2.789133085058098087E-16 ) ) ;
#78067 = VERTEX_POINT ( 'NONE', #79248 ) ;
#78068 = CARTESIAN_POINT ( 'NONE',  ( -34.92500000000001137, 21.72500000000000142, 0.4999999999999995559 ) ) ;
#78070 = ADVANCED_FACE ( 'NONE', ( #104508 ), #83984, .T. ) ;
#78069 = LINE ( 'NONE', #9928, #128525 ) ;
#78071 = ORIENTED_EDGE ( 'NONE', *, *, #50584, .F. ) ;
#78072 = FACE_OUTER_BOUND ( 'NONE', #752, .T. ) ;
#78073 = VERTEX_POINT ( 'NONE', #37859 ) ;
#78074 = EDGE_CURVE ( 'NONE', #99199, #53035, #112537, .T. ) ;
#78075 = EDGE_LOOP ( 'NONE', ( #76879, #33146, #44007, #122056 ) ) ;
#78076 = ORIENTED_EDGE ( 'NONE', *, *, #132025, .T. ) ;
#78078 = VECTOR ( 'NONE', #6387, 1000.000000000000000 ) ;
#78077 = CARTESIAN_POINT ( 'NONE',  ( 125.0370968585647944, -3.054999999999998828, -5.291415217122919401 ) ) ;
#78079 = ADVANCED_FACE ( 'NONE', ( #135045 ), #68364, .T. ) ;
#78080 = FACE_OUTER_BOUND ( 'NONE', #43086, .T. ) ;
#78081 = CARTESIAN_POINT ( 'NONE',  ( 25.49999999999982947, 6.052185695429106893, 5.000000000000000000 ) ) ;
#78082 = PLANE ( 'NONE',  #141483 ) ;
#78083 = ORIENTED_EDGE ( 'NONE', *, *, #9914, .T. ) ;
#78084 = CARTESIAN_POINT ( 'NONE',  ( 12.37456980810188512, 6.871911579029510442, -3.967499999999998916 ) ) ;
#78085 = CARTESIAN_POINT ( 'NONE',  ( -34.92500000000001137, 22.22500000000000142, 4.000000000000000000 ) ) ;
#78086 = DIRECTION ( 'NONE',  ( -0.7071067811865486830, -0.7071067811865464625, 0.000000000000000000 ) ) ;
#78087 = AXIS2_PLACEMENT_3D ( 'NONE', #19696, #131324, #65387 ) ;
#78088 = EDGE_CURVE ( 'NONE', #100625, #140758, #125577, .T. ) ;
#78089 = DIRECTION ( 'NONE',  ( -0.7071067811865487940, 0.7071067811865463515, 0.000000000000000000 ) ) ;
#78090 = ORIENTED_EDGE ( 'NONE', *, *, #9532, .F. ) ;
#78091 = ORIENTED_EDGE ( 'NONE', *, *, #62369, .F. ) ;
#78092 = ORIENTED_EDGE ( 'NONE', *, *, #52798, .T. ) ;
#78093 = DIRECTION ( 'NONE',  ( -0.000000000000000000, 1.137193330093850868E-16, -1.000000000000000000 ) ) ;
#78094 = LINE ( 'NONE', #46202, #23211 ) ;
#78095 = UNCERTAINTY_MEASURE_WITH_UNIT (LENGTH_MEASURE( 1.000000000000000082E-05 ), #105656, 'distance_accuracy_value', 'NONE');
#78096 = DIRECTION ( 'NONE',  ( 0.000000000000000000, 1.065814103640150279E-14, 1.000000000000000000 ) ) ;
#78097 = ADVANCED_FACE ( 'NONE', ( #137158 ), #70517, .F. ) ;
#78098 = CARTESIAN_POINT ( 'NONE',  ( -33.18398860626899705, 28.73617430169810305, 5.000000000000000000 ) ) ;
#78099 = CARTESIAN_POINT ( 'NONE',  ( 7.033036791254640541, 9.050499037475331576, 2.895286894036863679 ) ) ;
#78100 = DIRECTION ( 'NONE',  ( -0.6830127018922180770, -0.6830127018922204085, -0.2588190451025213501 ) ) ;
#78101 = CARTESIAN_POINT ( 'NONE',  ( 27.99999999999999645, -49.14999999999999147, -49.92499999999968452 ) ) ;
#78102 = CARTESIAN_POINT ( 'NONE',  ( 14.12514619309225772, -14.24070752338413648, 9.401115078912624767 ) ) ;
#78103 = CARTESIAN_POINT ( 'NONE',  ( 5.207106781186514155, 18.75929247661552068, 5.000000000000000000 ) ) ;
#78104 = VERTEX_POINT ( 'NONE', #135727 ) ;
#78105 = LINE ( 'NONE', #123760, #104366 ) ;
#78106 = ORIENTED_EDGE ( 'NONE', *, *, #92239, .T. ) ;
#78107 = SURFACE_SIDE_STYLE ('',( #112166 ) ) ;
#78108 = EDGE_LOOP ( 'NONE', ( #67717, #12826, #88521, #9816 ) ) ;
#78109 = LINE ( 'NONE', #82395, #120097 ) ;
#78111 = ORIENTED_EDGE ( 'NONE', *, *, #88611, .T. ) ;
#78110 = CARTESIAN_POINT ( 'NONE',  ( 41.83333333333333570, -6.884901960086287964, 3.974999999999998312 ) ) ;
#78112 = VECTOR ( 'NONE', #15894, 999.9999999999998863 ) ;
#78113 = CARTESIAN_POINT ( 'NONE',  ( -28.26506670282034150, 12.75929247661558286, 18.34774599283962360 ) ) ;
#78114 = LINE ( 'NONE', #110689, #81998 ) ;
#78115 = ORIENTED_EDGE ( 'NONE', *, *, #34613, .F. ) ;
#78116 = LINE ( 'NONE', #22967, #2106 ) ;
#78117 = ORIENTED_EDGE ( 'NONE', *, *, #36114, .T. ) ;
#78118 = CARTESIAN_POINT ( 'NONE',  ( 7.637717201596474048, 4.584330080086930965E-16, 0.000000000000000000 ) ) ;
#78119 = UNCERTAINTY_MEASURE_WITH_UNIT (LENGTH_MEASURE( 1.000000000000000082E-05 ), #138510, 'distance_accuracy_value', 'NONE');
#78120 = ORIENTED_EDGE ( 'NONE', *, *, #8760, .T. ) ;
#78121 = VECTOR ( 'NONE', #30020, 1000.000000000000000 ) ;
#78122 = VECTOR ( 'NONE', #131859, 1000.000000000000000 ) ;
#78123 = DIRECTION ( 'NONE',  ( -0.7071067811865487940, 0.7071067811865463515, -0.000000000000000000 ) ) ;
#78124 = ADVANCED_FACE ( 'NONE', ( #26949 ), #124840, .T. ) ;
#78126 = CARTESIAN_POINT ( 'NONE',  ( 113.1000270504628986, 5.819803920172570422, 5.819803920172574863 ) ) ;
#78125 = VECTOR ( 'NONE', #58041, 999.9999999999998863 ) ;
#78127 = DIRECTION ( 'NONE',  ( -0.6830127018922180770, -0.6830127018922204085, -0.2588190451025213501 ) ) ;
#78128 = DIRECTION ( 'NONE',  ( 0.000000000000000000, 0.000000000000000000, -1.000000000000000000 ) ) ;
#78129 =( LENGTH_UNIT ( ) NAMED_UNIT ( * ) SI_UNIT ( .MILLI., .METRE. ) );
#78130 = PLANE ( 'NONE',  #93615 ) ;
#78131 = DIRECTION ( 'NONE',  ( 0.7071067811865486830, -0.7071067811865464625, -0.000000000000000000 ) ) ;
#78132 = CARTESIAN_POINT ( 'NONE',  ( 18.66666666666666785, -5.278424836066145431, -3.047499999999993658 ) ) ;
#78133 = DIRECTION ( 'NONE',  ( 0.7071067811865487940, 0.7071067811865463515, 0.000000000000000000 ) ) ;
#78134 = AXIS2_PLACEMENT_3D ( 'NONE', #46279, #69441, #1280 ) ;
#78135 = DIRECTION ( 'NONE',  ( 0.3543493200069162685, -0.000000000000000000, -0.9351131265310288487 ) ) ;
#78136 = CARTESIAN_POINT ( 'NONE',  ( 15.18398860626900237, 28.73617430169797871, 5.000000000000000000 ) ) ;
#78137 = EDGE_LOOP ( 'NONE', ( #62039, #7537, #70098, #107513, #63805 ) ) ;
#78138 = ORIENTED_EDGE ( 'NONE', *, *, #128752, .T. ) ;
#78139 = LINE ( 'NONE', #143371, #9654 ) ;
#78140 = ORIENTED_EDGE ( 'NONE', *, *, #39705, .F. ) ;
#78141 = CARTESIAN_POINT ( 'NONE',  ( 91.00043019189810423, -3.055000000000002380, 5.291415217122920289 ) ) ;
#78142 = PLANE ( 'NONE',  #6282 ) ;
#78143 = DIRECTION ( 'NONE',  ( -0.7071067811865487940, 0.7071067811865463515, -0.000000000000000000 ) ) ;
#78144 = FACE_OUTER_BOUND ( 'NONE', #59803, .T. ) ;
#78145 = CARTESIAN_POINT ( 'NONE',  ( 126.7224180521723298, -45.84254607569018702, -35.55177538329009224 ) ) ;
#78146 = VERTEX_POINT ( 'NONE', #35005 ) ;
#78147 = CARTESIAN_POINT ( 'NONE',  ( 1.179999999999999272, 10.00000000000000178, 6.750000000000000888 ) ) ;
#78148 = CARTESIAN_POINT ( 'NONE',  ( 6.981552653643259276, 18.75929247661552424, 20.33588619593441393 ) ) ;
#78149 = PLANE ( 'NONE',  #99714 ) ;
#78150 = CARTESIAN_POINT ( 'NONE',  ( 0.7816268829249468642, 21.74787736706806385, 4.999607392498049308 ) ) ;
#78151 = CARTESIAN_POINT ( 'NONE',  ( 29.99999999999979039, 9.631307414974347836, -9.079085613539472632 ) ) ;
#78153 = EDGE_LOOP ( 'NONE', ( #135932, #36145, #113901, #141077 ) ) ;
#78152 = LINE ( 'NONE', #99888, #1161 ) ;
#78154 = DIRECTION ( 'NONE',  ( 0.000000000000000000, 0.000000000000000000, -1.000000000000000000 ) ) ;
#78155 = VECTOR ( 'NONE', #114753, 1000.000000000000000 ) ;
#78156 = LINE ( 'NONE', #122331, #126331 ) ;
#78157 = LINE ( 'NONE', #89727, #9942 ) ;
#78158 = LINE ( 'NONE', #67281, #15468 ) ;
#78159 =( BOUNDED_CURVE ( )  B_SPLINE_CURVE ( 3, ( #132316, #142460, #64181, #42452 ),
 .UNSPECIFIED., .F., .T. ) 
 B_SPLINE_CURVE_WITH_KNOTS ( ( 4, 4 ),
 ( 1.208578181583233491, 1.359146454359400957 ),
 .UNSPECIFIED. ) 
 CURVE ( )  GEOMETRIC_REPRESENTATION_ITEM ( )  RATIONAL_B_SPLINE_CURVE ( ( 1.000000000000000000, 0.9981116584018960847, 0.9981116584018960847, 1.000000000000000000 ) ) 
 REPRESENTATION_ITEM ( '' )  );
#78160 = DIRECTION ( 'NONE',  ( 0.7071067811865487940, 0.7071067811865463515, 0.000000000000000000 ) ) ;
#78161 = ORIENTED_EDGE ( 'NONE', *, *, #31862, .F. ) ;
#78162 = ORIENTED_EDGE ( 'NONE', *, *, #121882, .F. ) ;
#78163 = ORIENTED_EDGE ( 'NONE', *, *, #60517, .F. ) ;
#78164 = CARTESIAN_POINT ( 'NONE',  ( 90.85459685856477563, -1.637169565754161615, 6.110000000000000320 ) ) ;
#78165 = VECTOR ( 'NONE', #117973, 999.9999999999998863 ) ;
#78166 = ORIENTED_EDGE ( 'NONE', *, *, #62774, .F. ) ;
#78167 = LINE ( 'NONE', #122343, #76386 ) ;
#78168 = DIRECTION ( 'NONE',  ( -0.7071067811865487940, 0.7071067811865463515, -0.000000000000000000 ) ) ;
#78169 = AXIS2_PLACEMENT_3D ( 'NONE', #65729, #88156, #107735 ) ;
#78170 = DIRECTION ( 'NONE',  ( -0.7071067811865486830, -0.7071067811865464625, 0.000000000000000000 ) ) ;
#78171 = CARTESIAN_POINT ( 'NONE',  ( 85.10002705046289861, 5.819803920172570422, 5.819803920172575751 ) ) ;
#78172 = EDGE_LOOP ( 'NONE', ( #133226, #67650, #17852, #79975 ) ) ;
#78173 = CARTESIAN_POINT ( 'NONE',  ( 12.18398860626900060, 28.73617430169795739, 5.000000000000000000 ) ) ;
#78174 = FACE_OUTER_BOUND ( 'NONE', #92967, .T. ) ;
#78175 = DIRECTION ( 'NONE',  ( 0.000000000000000000, 0.000000000000000000, 1.000000000000000000 ) ) ;
#78176 = CARTESIAN_POINT ( 'NONE',  ( 81.43293019189809456, 1.637169565754156508, 6.110000000000000320 ) ) ;
#78177 = VERTEX_POINT ( 'NONE', #26254 ) ;
#78178 = LINE ( 'NONE', #111500, #90657 ) ;
#78179 = EDGE_CURVE ( 'NONE', #140110, #44742, #114660, .T. ) ;
#78180 = DIRECTION ( 'NONE',  ( 0.000000000000000000, 0.000000000000000000, 1.000000000000000000 ) ) ;
#78181 = ORIENTED_EDGE ( 'NONE', *, *, #129645, .F. ) ;
#78182 = ORIENTED_EDGE ( 'NONE', *, *, #111411, .F. ) ;
#78183 = AXIS2_PLACEMENT_3D ( 'NONE', #99037, #21509, #132449 ) ;
#78184 = FACE_OUTER_BOUND ( 'NONE', #137693, .T. ) ;
#78185 = EDGE_CURVE ( 'NONE', #134257, #98588, #3051, .T. ) ;
#78186 = EDGE_CURVE ( 'NONE', #138636, #77870, #101654, .T. ) ;
#78187 = CARTESIAN_POINT ( 'NONE',  ( 36.29974487139159578, -27.71228299555231445, 4.000000000000000000 ) ) ;
#78188 = CARTESIAN_POINT ( 'NONE',  ( 163.1915705344537741, 26.96999999999992781, 34.63378833274251889 ) ) ;
#78189 = DIRECTION ( 'NONE',  ( -0.7071067811865486830, -0.7071067811865464625, -0.000000000000000000 ) ) ;
#78190 = EDGE_CURVE ( 'NONE', #130315, #46312, #113966, .T. ) ;
#78191 = EDGE_CURVE ( 'NONE', #114924, #77276, #58213, .T. ) ;
#78192 = CARTESIAN_POINT ( 'NONE',  ( 81.48921356237309510, -27.52281430457112066, 5.000000000000000000 ) ) ;
#78193 = VERTEX_POINT ( 'NONE', #58934 ) ;
#78194 = AXIS2_PLACEMENT_3D ( 'NONE', #72190, #127975, #83026 ) ;
#78195 = VERTEX_POINT ( 'NONE', #91514 ) ;
#78197 = EDGE_CURVE ( 'NONE', #76630, #23935, #3732, .T. ) ;
#78196 = FACE_OUTER_BOUND ( 'NONE', #54483, .T. ) ;
#78198 = ORIENTED_EDGE ( 'NONE', *, *, #107482, .T. ) ;
#78199 = ORIENTED_EDGE ( 'NONE', *, *, #31210, .F. ) ;
#78200 = ADVANCED_FACE ( 'NONE', ( #59616 ), #4413, .F. ) ;
#78201 = EDGE_CURVE ( 'NONE', #136035, #83916, #105228, .T. ) ;
#78202 = CIRCLE ( 'NONE', #96672, 2.500000000000000888 ) ;
#78203 = CARTESIAN_POINT ( 'NONE',  ( -66.18398860626901126, 28.73617430169833753, 5.000000000000000000 ) ) ;
#78204 = ORIENTED_EDGE ( 'NONE', *, *, #95989, .F. ) ;
#78205 = DIRECTION ( 'NONE',  ( 0.7071067811865487940, 0.7071067811865463515, 0.000000000000000000 ) ) ;
#78206 = CARTESIAN_POINT ( 'NONE',  ( -9.489213562373095101, -27.52281430457062328, 5.000000000000000000 ) ) ;
#78207 = FACE_OUTER_BOUND ( 'NONE', #18247, .T. ) ;
#78208 = FACE_OUTER_BOUND ( 'NONE', #110050, .T. ) ;
#78209 = VECTOR ( 'NONE', #45294, 1000.000000000000000 ) ;
#78210 = DIRECTION ( 'NONE',  ( 0.3543493200069162685, -0.000000000000000000, -0.9351131265310288487 ) ) ;
#78211 = ORIENTED_EDGE ( 'NONE', *, *, #46730, .T. ) ;
#78212 = EDGE_CURVE ( 'NONE', #58576, #90134, #105916, .T. ) ;
#78213 = CARTESIAN_POINT ( 'NONE',  ( 31.92500000000002203, -22.26999999999999247, -37.00000000000000000 ) ) ;
#78214 = VERTEX_POINT ( 'NONE', #16793 ) ;
#78215 = CARTESIAN_POINT ( 'NONE',  ( -32.99999999999976552, -3.485240976185108863, -4.108735105802471921 ) ) ;
#78216 = VERTEX_POINT ( 'NONE', #84229 ) ;
#78217 = CARTESIAN_POINT ( 'NONE',  ( 115.5791937171295558, 3.975000000000002753, -6.884901960086283523 ) ) ;
#78218 = VERTEX_POINT ( 'NONE', #96457 ) ;
#78219 = CARTESIAN_POINT ( 'NONE',  ( 25.97159235450331849, -3.851859888774471706E-31, 2.500000000000001332 ) ) ;
#78220 = ORIENTED_EDGE ( 'NONE', *, *, #126661, .T. ) ;
#78221 = ORIENTED_EDGE ( 'NONE', *, *, #105049, .T. ) ;
#78222 = EDGE_CURVE ( 'NONE', #129512, #53690, #58554, .T. ) ;
#78223 = VECTOR ( 'NONE', #2015, 1000.000000000000000 ) ;
#78224 = ORIENTED_EDGE ( 'NONE', *, *, #93430, .F. ) ;
#78225 = VECTOR ( 'NONE', #100136, 999.9999999999998863 ) ;
#78226 = CARTESIAN_POINT ( 'NONE',  ( -34.92500000000001137, 0.5846064065779844610, -3.200354092940483230 ) ) ;
#78227 = LINE ( 'NONE', #24537, #99213 ) ;
#78228 = DIRECTION ( 'NONE',  ( -0.6830127018922180770, -0.6830127018922204085, -0.2588190451025213501 ) ) ;
#78229 = CARTESIAN_POINT ( 'NONE',  ( 119.8754301918981184, -5.291415217122920289, -3.055000000000001492 ) ) ;
#78230 = DIRECTION ( 'NONE',  ( 0.6830127018922181881, 0.6830127018922202975, -0.2588190451025214056 ) ) ;
#78231 = CARTESIAN_POINT ( 'NONE',  ( 27.48921356237309155, -27.52281430457074762, 5.000000000000000000 ) ) ;
#78232 = DIRECTION ( 'NONE',  ( -0.7071067811865486830, -0.7071067811865464625, 0.000000000000000000 ) ) ;
#78233 = ADVANCED_FACE ( 'NONE', ( #50151 ), #94349, .F. ) ;
#78234 = DIRECTION ( 'NONE',  ( -0.000000000000000000, -0.000000000000000000, -1.000000000000000000 ) ) ;
#78236 = ADVANCED_FACE ( 'NONE', ( #85601 ), #73338, .F. ) ;
#78235 = CARTESIAN_POINT ( 'NONE',  ( -7.499999999999940492, -20.94781430457061333, 5.000000000000000000 ) ) ;
#78237 = VERTEX_POINT ( 'NONE', #62457 ) ;
#78238 = DIRECTION ( 'NONE',  ( 0.7071067811865487940, 0.7071067811865463515, -0.000000000000000000 ) ) ;
#78239 = CARTESIAN_POINT ( 'NONE',  ( -34.92500000000001137, -22.22500000000000142, 4.500000000000000888 ) ) ;
#78240 = DIRECTION ( 'NONE',  ( 0.000000000000000000, 0.000000000000000000, 1.000000000000000000 ) ) ;
#78241 = VERTEX_POINT ( 'NONE', #116816 ) ;
#78242 = EDGE_CURVE ( 'NONE', #125874, #7538, #116095, .T. ) ;
#78243 = ORIENTED_EDGE ( 'NONE', *, *, #129152, .T. ) ;
#78244 = VERTEX_POINT ( 'NONE', #108050 ) ;
#78245 = DIRECTION ( 'NONE',  ( 0.7071067811865487940, 0.7071067811865463515, -0.000000000000000000 ) ) ;
#78246 = EDGE_LOOP ( 'NONE', ( #25781, #58346, #114442, #36829 ) ) ;
#78247 = EDGE_CURVE ( 'NONE', #45102, #117033, #52970, .T. ) ;
#78248 = EDGE_CURVE ( 'NONE', #119991, #34098, #29100, .T. ) ;
#78249 = ORIENTED_EDGE ( 'NONE', *, *, #26150, .T. ) ;
#78250 = CARTESIAN_POINT ( 'NONE',  ( 31.49999999999978684, -7.420205493532869845, -2.617629953481181992 ) ) ;
#78251 = CARTESIAN_POINT ( 'NONE',  ( 107.9958603837962272, -3.974999999999998312, -6.884901960086286188 ) ) ;
#78252 = CARTESIAN_POINT ( 'NONE',  ( -2.999999999999981792, 14.87792677143808362, -11.06722581663440508 ) ) ;
#78253 = LINE ( 'NONE', #132659, #127433 ) ;
#78254 = VERTEX_POINT ( 'NONE', #52273 ) ;
#78255 = CIRCLE ( 'NONE', #15687, 2.500000000000000444 ) ;
#78256 = DIRECTION ( 'NONE',  ( -0.6830127018922181881, 0.6830127018922202975, -0.2588190451025214056 ) ) ;
#78257 = ORIENTED_EDGE ( 'NONE', *, *, #84087, .T. ) ;
#78258 = LINE ( 'NONE', #122440, #120894 ) ;
#78259 = CARTESIAN_POINT ( 'NONE',  ( 15.67123647476855552, 0.000000000000000000, 7.934999999999990727 ) ) ;
#78260 = ORIENTED_EDGE ( 'NONE', *, *, #90309, .T. ) ;
#78261 = CARTESIAN_POINT ( 'NONE',  ( 86.39126352523146579, -4.472830434245839371, -4.472830434245839371 ) ) ;
#78262 = LINE ( 'NONE', #107982, #25085 ) ;
#78263 = EDGE_CURVE ( 'NONE', #68280, #84791, #37602, .T. ) ;
#78264 = CARTESIAN_POINT ( 'NONE',  ( 99.39169371712955581, 2.130196079827421762, 7.950000000000000178 ) ) ;
#78265 = ORIENTED_EDGE ( 'NONE', *, *, #5491, .F. ) ;
#78266 = ORIENTED_EDGE ( 'NONE', *, *, #417, .F. ) ;
#78267 = ORIENTED_EDGE ( 'NONE', *, *, #54144, .F. ) ;
#78268 = CARTESIAN_POINT ( 'NONE',  ( 7.139999999999992575, -35.14999999999999858, -8.278119684037271497 ) ) ;
#78269 = DIRECTION ( 'NONE',  ( -1.000000000000000000, 0.000000000000000000, 0.000000000000000000 ) ) ;
#78270 = DIRECTION ( 'NONE',  ( -0.000000000000000000, 0.3543493200069153248, 0.9351131265310292928 ) ) ;
#78271 = CARTESIAN_POINT ( 'NONE',  ( 0.000000000000000000, 0.000000000000000000, 5.000000000000000000 ) ) ;
#78272 = EDGE_LOOP ( 'NONE', ( #102950, #97329, #45345, #10552, #33937, #13762 ) ) ;
#78273 = DIRECTION ( 'NONE',  ( -0.000000000000000000, -0.3543493200069152693, 0.9351131265310292928 ) ) ;
#78274 = ADVANCED_FACE ( 'NONE', ( #51584 ), #95777, .F. ) ;
#78275 = CARTESIAN_POINT ( 'NONE',  ( 13.17183060077637968, 0.7592924766157086447, 4.000000000000000000 ) ) ;
#78276 = CARTESIAN_POINT ( 'NONE',  ( 23.99999999999983302, 7.931123077392101095, 4.000000000000000000 ) ) ;
#78277 = VERTEX_POINT ( 'NONE', #140024 ) ;
#78278 = CARTESIAN_POINT ( 'NONE',  ( 10.46799328145038821, -2.055000000000000160, 0.000000000000000000 ) ) ;
#78279 = CARTESIAN_POINT ( 'NONE',  ( -54.18398860626899705, 28.73617430169825226, 5.000000000000000000 ) ) ;
#78280 = ORIENTED_EDGE ( 'NONE', *, *, #32609, .F. ) ;
#78283 = ADVANCED_FACE ( 'NONE', ( #39278 ), #83501, .F. ) ;
#78282 = ORIENTED_EDGE ( 'NONE', *, *, #141371, .F. ) ;
#78281 = DIRECTION ( 'NONE',  ( 0.000000000000000000, -1.000000000000000000, 0.000000000000000000 ) ) ;
#78284 = EDGE_LOOP ( 'NONE', ( #61093, #124728, #120497, #118939 ) ) ;
#78285 = DIRECTION ( 'NONE',  ( -0.000000000000000000, 0.3543493200069153248, 0.9351131265310292928 ) ) ;
#78286 = CARTESIAN_POINT ( 'NONE',  ( 51.48921356237309510, -27.52281430457091460, 5.000000000000000000 ) ) ;
#78287 = ORIENTED_EDGE ( 'NONE', *, *, #20569, .F. ) ;
#78288 = LINE ( 'NONE', #67427, #86049 ) ;
#78289 = CARTESIAN_POINT ( 'NONE',  ( 34.49999999999975131, -1.592773361805337906, -6.492772025301308148 ) ) ;
#78290 = CARTESIAN_POINT ( 'NONE',  ( -25.39999999999996305, 0.000000000000000000, 0.000000000000000000 ) ) ;
#78291 = CARTESIAN_POINT ( 'NONE',  ( -13.49999999999990408, 3.653845994658375673, -4.504631822206340175 ) ) ;
#78292 = VECTOR ( 'NONE', #9720, 1000.000000000000000 ) ;
#78293 = CARTESIAN_POINT ( 'NONE',  ( -4.499999999999968914, 12.43112307739206024, 4.000000000000000000 ) ) ;
#78294 = CARTESIAN_POINT ( 'NONE',  ( -33.18398860626899705, 28.73617430169810305, 5.000000000000000000 ) ) ;
#78295 = CARTESIAN_POINT ( 'NONE',  ( -16.49999999999986500, 19.08746187583904685, 4.000000000000000000 ) ) ;
#78296 = CARTESIAN_POINT ( 'NONE',  ( 15.18398860626900237, 28.73617430169797871, 5.000000000000000000 ) ) ;
#78297 = LINE ( 'NONE', #10162, #117731 ) ;
#78298 = CARTESIAN_POINT ( 'NONE',  ( 19.08290314143522437, 3.967499999999992699, -6.871911579029513994 ) ) ;
#78299 = CARTESIAN_POINT ( 'NONE',  ( 2.166236474768552966, 7.934999999999990727, -1.457635852685135314E-15 ) ) ;
#78300 = PLANE ( 'NONE',  #103758 ) ;
#78301 = LINE ( 'NONE', #119620, #68626 ) ;
#78302 = ORIENTED_EDGE ( 'NONE', *, *, #132591, .F. ) ;
#78303 = ADVANCED_FACE ( 'NONE', ( #118223 ), #129118, .F. ) ;
#78304 = EDGE_LOOP ( 'NONE', ( #103258, #63347, #133332, #105150 ) ) ;
#78305 = CARTESIAN_POINT ( 'NONE',  ( 103.3750000000000000, 7.950000000000000178, 1.460391307983218535E-15 ) ) ;
#78306 = EDGE_CURVE ( 'NONE', #56334, #134021, #29796, .T. ) ;
#78307 = ORIENTED_EDGE ( 'NONE', *, *, #105650, .T. ) ;
#78308 = ORIENTED_EDGE ( 'NONE', *, *, #134654, .T. ) ;
#78309 = ORIENTED_EDGE ( 'NONE', *, *, #1232, .T. ) ;
#78310 = LINE ( 'NONE', #89187, #124417 ) ;
#78311 = CARTESIAN_POINT ( 'NONE',  ( -31.49999999999977263, 1.087461875839230707, 4.000000000000000000 ) ) ;
#78312 = ORIENTED_EDGE ( 'NONE', *, *, #45745, .F. ) ;
#78313 = VECTOR ( 'NONE', #25634, 1000.000000000000000 ) ;
#78314 = CARTESIAN_POINT ( 'NONE',  ( -28.49999999999979750, -13.53360074219760101, 5.000000000000000000 ) ) ;
#78315 = PLANE ( 'NONE',  #51140 ) ;
#78316 = CARTESIAN_POINT ( 'NONE',  ( 5.068407645496677105, 9.139736423841732040E-16, 0.000000000000000000 ) ) ;
#78317 = DIRECTION ( 'NONE',  ( -0.7071067811865486830, -0.7071067811865464625, 0.000000000000000000 ) ) ;
#78318 = ORIENTED_EDGE ( 'NONE', *, *, #116781, .F. ) ;
#78319 = ADVANCED_FACE ( 'NONE', ( #18930 ), #41393, .F. ) ;
#78320 = CARTESIAN_POINT ( 'NONE',  ( 19.42650926608378725, -2.782569431601979559, 4.369986656771211564 ) ) ;
#78321 = CARTESIAN_POINT ( 'NONE',  ( 17.50000000000000000, 0.000000000000000000, 6.094999999999989981 ) ) ;
#78322 = CARTESIAN_POINT ( 'NONE',  ( 14.99999999999989519, -15.03360074219758857, 5.000000000000000000 ) ) ;
#78324 = LINE ( 'NONE', #134871, #59124 ) ;
#78323 = AXIS2_PLACEMENT_3D ( 'NONE', #128831, #122776, #119364 ) ;
#78325 = PLANE ( 'NONE',  #70134 ) ;
#78326 = DIRECTION ( 'NONE',  ( 0.7071067811865487940, 0.7071067811865463515, 0.000000000000000000 ) ) ;
#78327 = VECTOR ( 'NONE', #4135, 999.9999999999998863 ) ;
#78328 = CARTESIAN_POINT ( 'NONE',  ( 86.85002705046289861, -5.819803920172573086, -5.819803920172573086 ) ) ;
#78329 = DIRECTION ( 'NONE',  ( -1.000000000000000000, -1.224606353822377258E-16, -0.000000000000000000 ) ) ;
#78330 = VERTEX_POINT ( 'NONE', #19644 ) ;
#78331 = VERTEX_POINT ( 'NONE', #31956 ) ;
#78332 = CARTESIAN_POINT ( 'NONE',  ( 120.4587635252314328, 0.000000000000000000, -6.110000000000001208 ) ) ;
#78333 = EDGE_LOOP ( 'NONE', ( #87940, #2803, #114339, #123849, #76616, #25376 ) ) ;
#78334 = CARTESIAN_POINT ( 'NONE',  ( 3.250000000000000000, -4.999999999999999112, -7.627214432543508948 ) ) ;
#78335 = CARTESIAN_POINT ( 'NONE',  ( 3.183988606268992161, 28.73617430169789699, 5.000000000000000000 ) ) ;
#78336 = DIRECTION ( 'NONE',  ( 0.7071067811865487940, 0.7071067811865463515, 0.000000000000000000 ) ) ;
#78337 = LINE ( 'NONE', #76938, #85836 ) ;
#78338 = CARTESIAN_POINT ( 'NONE',  ( 112.6412635252314658, 4.472830434245836706, 4.472830434245840259 ) ) ;
#78339 = ORIENTED_EDGE ( 'NONE', *, *, #25702, .F. ) ;
#78340 = B_SPLINE_CURVE_WITH_KNOTS ( 'NONE', 3,
 ( #65165, #53556, #99907, #12174, #142702, #109354, #42700, #119487, #31801, #64420, #88336, #131832 ),
 .UNSPECIFIED., .F., .F.,
 ( 4, 2, 2, 2, 2, 4 ),
 ( 0.000000000000000000, 0.001837441947543509788, 0.003674883895087019577, 0.004593604868858774254, 0.005512325842630529799, 0.007349767790174039153 ),
 .UNSPECIFIED. ) ;
#78341 = ORIENTED_EDGE ( 'NONE', *, *, #140656, .F. ) ;
#78342 = DIRECTION ( 'NONE',  ( -0.3543493200069162685, -0.000000000000000000, -0.9351131265310288487 ) ) ;
#78343 = VECTOR ( 'NONE', #106415, 1000.000000000000227 ) ;
#78344 = CARTESIAN_POINT ( 'NONE',  ( 24.48921356237309510, -27.52281430457072631, 5.000000000000000000 ) ) ;
#78345 = AXIS2_PLACEMENT_3D ( 'NONE', #138725, #126394, #18316 ) ;
#78346 = AXIS2_PLACEMENT_3D ( 'NONE', #50058, #137056, #16694 ) ;
#78347 = EDGE_LOOP ( 'NONE', ( #11284, #129281, #66286, #112340 ) ) ;
#78348 = ORIENTED_EDGE ( 'NONE', *, *, #24448, .F. ) ;
#78349 = CARTESIAN_POINT ( 'NONE',  ( 40.39626352523143993, 4.472830434245840259, -4.472830434245839371 ) ) ;
#78350 = VERTEX_POINT ( 'NONE', #88497 ) ;
#78351 = DIRECTION ( 'NONE',  ( -0.6830127018922180770, -0.6830127018922204085, -0.2588190451025213501 ) ) ;
#78352 = ADVANCED_FACE ( 'NONE', ( #109513 ), #78325, .F. ) ;
#78353 = FACE_OUTER_BOUND ( 'NONE', #24439, .T. ) ;
#78354 = EDGE_CURVE ( 'NONE', #118868, #72669, #120345, .T. ) ;
#78355 = CARTESIAN_POINT ( 'NONE',  ( 28.49543019189811233, 5.291415217122916737, 3.055000000000001936 ) ) ;
#78356 = EDGE_CURVE ( 'NONE', #58219, #15180, #21063, .T. ) ;
#78357 = ORIENTED_EDGE ( 'NONE', *, *, #26972, .T. ) ;
#78359 = EDGE_CURVE ( 'NONE', #136020, #137944, #44285, .T. ) ;
#78358 = DIRECTION ( 'NONE',  ( -1.000000000000000000, -1.224606353822377258E-16, -0.000000000000000000 ) ) ;
#78360 = ORIENTED_EDGE ( 'NONE', *, *, #33814, .F. ) ;
#78361 = ORIENTED_EDGE ( 'NONE', *, *, #125439, .T. ) ;
#78362 = VECTOR ( 'NONE', #22373, 1000.000000000000227 ) ;
#78363 = EDGE_LOOP ( 'NONE', ( #43289, #108413, #13558, #13660 ) ) ;
#78364 = ADVANCED_FACE ( 'NONE', ( #108759 ), #97166, .F. ) ;
#78365 =( BOUNDED_CURVE ( )  B_SPLINE_CURVE ( 3, ( #30394, #50722, #128983, #126831 ),
 .UNSPECIFIED., .F., .F. ) 
 B_SPLINE_CURVE_WITH_KNOTS ( ( 4, 4 ),
 ( 4.130769849943813909, 4.183600770845220751 ),
 .UNSPECIFIED. ) 
 CURVE ( )  GEOMETRIC_REPRESENTATION_ITEM ( )  RATIONAL_B_SPLINE_CURVE ( ( 1.000000000000000000, 0.9997674213408587196, 0.9997674213408587196, 1.000000000000000000 ) ) 
 REPRESENTATION_ITEM ( '' )  );
#78366 = VECTOR ( 'NONE', #64914, 1000.000000000000000 ) ;
#78367 = DIRECTION ( 'NONE',  ( -1.400468248933914810E-15, -0.9647414015272155474, 0.2631995976047525887 ) ) ;
#78368 = CARTESIAN_POINT ( 'NONE',  ( 24.18398860626899705, 28.73617430169804265, 5.000000000000000000 ) ) ;
#78369 = VERTEX_POINT ( 'NONE', #67473 ) ;
#78370 = DIRECTION ( 'NONE',  ( 0.3543493200069163240, -0.000000000000000000, 0.9351131265310288487 ) ) ;
#78371 = ADVANCED_FACE ( 'NONE', ( #76184 ), #54451, .T. ) ;
#78372 = CARTESIAN_POINT ( 'NONE',  ( 0.000000000000000000, -8.616843969807042924, 0.000000000000000000 ) ) ;
#78373 = LINE ( 'NONE', #66781, #99170 ) ;
#78374 = CARTESIAN_POINT ( 'NONE',  ( -34.49999999999975131, 13.08746187583910547, 4.000000000000000000 ) ) ;
#78375 = EDGE_CURVE ( 'NONE', #140587, #17685, #116504, .T. ) ;
#78376 = FACE_BOUND ( 'NONE', #29803, .T. ) ;
#78377 = ORIENTED_EDGE ( 'NONE', *, *, #122164, .F. ) ;
#78378 = ADVANCED_FACE ( 'NONE', ( #76920 ), #111664, .T. ) ;
#78379 = LINE ( 'NONE', #56669, #36380 ) ;
#78380 = LINE ( 'NONE', #135615, #92440 ) ;
#78381 = PLANE ( 'NONE',  #76867 ) ;
#78382 = LINE ( 'NONE', #132788, #106416 ) ;
#78383 = ORIENTED_EDGE ( 'NONE', *, *, #100434, .F. ) ;
#78384 = LINE ( 'NONE', #76983, #1787 ) ;
#78385 = EDGE_LOOP ( 'NONE', ( #131251, #70472, #79107, #43262, #5667 ) ) ;
#78386 = ORIENTED_EDGE ( 'NONE', *, *, #33113, .T. ) ;
#78387 = ADVANCED_FACE ( 'NONE', ( #21792 ), #66040, .F. ) ;
#78388 = ORIENTED_EDGE ( 'NONE', *, *, #222, .T. ) ;
#78389 = CARTESIAN_POINT ( 'NONE',  ( 51.53709685856478018, -3.054999999999998828, -5.291415217122919401 ) ) ;
#78390 = VERTEX_POINT ( 'NONE', #33425 ) ;
#78391 = CARTESIAN_POINT ( 'NONE',  ( 22.49999999999986144, 19.08746187583905041, 4.000000000000000000 ) ) ;
#78392 = CARTESIAN_POINT ( 'NONE',  ( 28.00000000000002487, -52.14999999999999147, 34.92500000000003268 ) ) ;
#78393 = ORIENTED_EDGE ( 'NONE', *, *, #47128, .F. ) ;
#78394 = DIRECTION ( 'NONE',  ( 0.000000000000000000, -0.3543493200069152138, 0.9351131265310292928 ) ) ;
#78395 = DIRECTION ( 'NONE',  ( -0.7071067811865486830, -0.7071067811865464625, 0.000000000000000000 ) ) ;
#78396 = CARTESIAN_POINT ( 'NONE',  ( -7.140000000000001457, -34.64999999999999147, 17.49210858042621908 ) ) ;
#78397 = VECTOR ( 'NONE', #83439, 1000.000000000000000 ) ;
#78398 = LINE ( 'NONE', #33491, #120304 ) ;
#78399 = FACE_OUTER_BOUND ( 'NONE', #66339, .T. ) ;
#78400 = LINE ( 'NONE', #88579, #70251 ) ;
#78401 = EDGE_LOOP ( 'NONE', ( #62553, #134736, #62661, #130822 ) ) ;
#78402 = EDGE_CURVE ( 'NONE', #58607, #142587, #110205, .T. ) ;
#78403 = ORIENTED_EDGE ( 'NONE', *, *, #91613, .T. ) ;
#78404 = ORIENTED_EDGE ( 'NONE', *, *, #100655, .F. ) ;
#78405 = EDGE_LOOP ( 'NONE', ( #74347, #6285, #20867, #59838, #132108 ) ) ;
#78406 = DIRECTION ( 'NONE',  ( 0.2399999999999954947, -0.000000000000000000, 0.9707728879609288652 ) ) ;
#78408 = CARTESIAN_POINT ( 'NONE',  ( 0.7071067811865432429, -0.7407075233842822515, 5.000000000000000000 ) ) ;
#78407 = VECTOR ( 'NONE', #67959, 999.9999999999998863 ) ;
#78409 = ORIENTED_EDGE ( 'NONE', *, *, #134903, .F. ) ;
#78410 = VECTOR ( 'NONE', #78370, 1000.000000000000227 ) ;
#78411 = ORIENTED_EDGE ( 'NONE', *, *, #60587, .T. ) ;
#78412 = CARTESIAN_POINT ( 'NONE',  ( 166.0610720213131799, 26.96999999999993847, -33.43488148127461557 ) ) ;
#78413 = VECTOR ( 'NONE', #78808, 1000.000000000000000 ) ;
#78414 = CARTESIAN_POINT ( 'NONE',  ( -4.828169399223491531, 0.7592924766157138627, 4.000000000000000000 ) ) ;
#78415 = ORIENTED_EDGE ( 'NONE', *, *, #84100, .F. ) ;
#78416 = CARTESIAN_POINT ( 'NONE',  ( 7.190181675744438117, -18.74070752338408852, 7.910009926591490270 ) ) ;
#78417 = VECTOR ( 'NONE', #40152, 1000.000000000000227 ) ;
#78418 = EDGE_CURVE ( 'NONE', #42016, #71242, #55147, .T. ) ;
#78419 = PLANE ( 'NONE',  #118515 ) ;
#78420 = CARTESIAN_POINT ( 'NONE',  ( 32.15040314143522693, 7.934999999999989839, -2.126176841940961904 ) ) ;
#78421 = DIRECTION ( 'NONE',  ( -0.7071067811865486830, -0.7071067811865464625, -0.000000000000000000 ) ) ;
#78422 = VERTEX_POINT ( 'NONE', #121794 ) ;
#78424 = CARTESIAN_POINT ( 'NONE',  ( 14.99999999999989697, 16.55218569542899587, 5.000000000000000000 ) ) ;
#78423 = CARTESIAN_POINT ( 'NONE',  ( 114.2454301918981230, -5.291415217122919401, -3.055000000000000604 ) ) ;
#78426 = ADVANCED_FACE ( 'NONE', ( #22473 ), #100077, .T. ) ;
#78425 = DIRECTION ( 'NONE',  ( -0.7071067811865486830, -0.7071067811865464625, 0.000000000000000000 ) ) ;
#78427 = CARTESIAN_POINT ( 'NONE',  ( 0.7928932188134519832, 15.75929247661555976, 5.000000000000000000 ) ) ;
#78428 = DIRECTION ( 'NONE',  ( 0.3543493200069162685, -0.000000000000000000, -0.9351131265310288487 ) ) ;
#78430 = VERTEX_POINT ( 'NONE', #92739 ) ;
#78429 = CARTESIAN_POINT ( 'NONE',  ( 1.358242975411386055, 15.75929247661555799, 19.34181609438699212 ) ) ;
#78431 = AXIS2_PLACEMENT_3D ( 'NONE', #120477, #9590, #29926 ) ;
#78432 = CARTESIAN_POINT ( 'NONE',  ( 0.000000000000000000, 0.000000000000000000, 5.000000000000000000 ) ) ;
#78434 = ORIENTED_EDGE ( 'NONE', *, *, #86084, .T. ) ;
#78433 = MECHANICAL_DESIGN_GEOMETRIC_PRESENTATION_REPRESENTATION (  '', ( #59916 ), #117811 ) ;
#78435 = SURFACE_STYLE_USAGE ( .BOTH. , #142961 ) ;
#78436 = FACE_OUTER_BOUND ( 'NONE', #42256, .T. ) ;
#78437 = FACE_OUTER_BOUND ( 'NONE', #75156, .T. ) ;
#78438 = ORIENTED_EDGE ( 'NONE', *, *, #90649, .F. ) ;
#78439 = LINE ( 'NONE', #101597, #85303 ) ;
#78440 = VECTOR ( 'NONE', #64945, 1000.000000000000000 ) ;
#78441 = EDGE_CURVE ( 'NONE', #44113, #24156, #106300, .T. ) ;
#78442 = DIRECTION ( 'NONE',  ( -0.3543493200069162685, -0.000000000000000000, -0.9351131265310288487 ) ) ;
#78443 = DIRECTION ( 'NONE',  ( -0.7071067811865487940, 0.7071067811865463515, -0.000000000000000000 ) ) ;
#78444 = ORIENTED_EDGE ( 'NONE', *, *, #69469, .F. ) ;
#78445 = AXIS2_PLACEMENT_3D ( 'NONE', #117479, #5139, #61727 ) ;
#78446 = AXIS2_PLACEMENT_3D ( 'NONE', #61081, #94357, #8046 ) ;
#78448 = VECTOR ( 'NONE', #73125, 1000.000000000000227 ) ;
#78447 = DIRECTION ( 'NONE',  ( 0.6830127018922180770, -0.6830127018922204085, -0.2588190451025213501 ) ) ;
#78449 = ORIENTED_EDGE ( 'NONE', *, *, #102081, .T. ) ;
#78450 = AXIS2_PLACEMENT_3D ( 'NONE', #141944, #74539, #118723 ) ;
#78451 = DIRECTION ( 'NONE',  ( -0.000000000000000000, 0.3543493200069153248, 0.9351131265310292928 ) ) ;
#78454 = EDGE_CURVE ( 'NONE', #11112, #123460, #36250, .T. ) ;
#78453 = ORIENTED_EDGE ( 'NONE', *, *, #88420, .F. ) ;
#78452 = CARTESIAN_POINT ( 'NONE',  ( -33.70710678118631165, 8.259292476615643253, 5.000000000000000000 ) ) ;
#78455 = ORIENTED_EDGE ( 'NONE', *, *, #53280, .T. ) ;
#78456 = CARTESIAN_POINT ( 'NONE',  ( 6.671778046239097648, 12.72213433738527932, -25.13690993948508279 ) ) ;
#78457 = CARTESIAN_POINT ( 'NONE',  ( 33.18398860626899705, 28.73617430169810305, 5.000000000000000000 ) ) ;
#78458 = ORIENTED_EDGE ( 'NONE', *, *, #64998, .F. ) ;
#78459 = VECTOR ( 'NONE', #46915, 1000.000000000000000 ) ;
#78460 = CARTESIAN_POINT ( 'NONE',  ( -39.48921356237310221, -27.52281430457082934, 5.000000000000000000 ) ) ;
#78461 = CARTESIAN_POINT ( 'NONE',  ( -26.72174548431410912, 8.259292476615641476, 11.78515199841144145 ) ) ;
#78462 = DIRECTION ( 'NONE',  ( -1.000000000000000000, 4.620891819070403647E-14, 0.000000000000000000 ) ) ;
#78463 = ORIENTED_EDGE ( 'NONE', *, *, #34768, .T. ) ;
#78464 = CARTESIAN_POINT ( 'NONE',  ( 16.99806943317890529, -22.22500000000000142, 4.500000000000000888 ) ) ;
#78465 = LINE ( 'NONE', #124811, #97583 ) ;
#78466 = DIRECTION ( 'NONE',  ( -0.7071067811865486830, -0.7071067811865464625, 0.000000000000000000 ) ) ;
#78467 = VECTOR ( 'NONE', #123582, 1000.000000000000000 ) ;
#78468 = CARTESIAN_POINT ( 'NONE',  ( -2.510786437626908008, -27.52281430457053446, 5.000000000000000000 ) ) ;
#78469 = CARTESIAN_POINT ( 'NONE',  ( 28.05793019189811233, 6.110000000000001208, -1.637169565754156286 ) ) ;
#78470 = PLANE ( 'NONE',  #9475 ) ;
#78471 = ORIENTED_EDGE ( 'NONE', *, *, #53910, .F. ) ;
#78472 = ORIENTED_EDGE ( 'NONE', *, *, #68580, .T. ) ;
#78473 = EDGE_CURVE ( 'NONE', #41252, #64397, #70345, .T. ) ;
#78474 = VERTEX_POINT ( 'NONE', #71031 ) ;
#78475 = ORIENTED_EDGE ( 'NONE', *, *, #118944, .F. ) ;
#78476 = ORIENTED_EDGE ( 'NONE', *, *, #1687, .F. ) ;
#78477 = CARTESIAN_POINT ( 'NONE',  ( -25.49999999999981526, -17.94781430457063820, 5.000000000000000000 ) ) ;
#78478 = CARTESIAN_POINT ( 'NONE',  ( -20.99999999999984368, 14.58746187583908771, 4.000000000000000000 ) ) ;
#78479 = VERTEX_POINT ( 'NONE', #15171 ) ;
#78480 = FACE_OUTER_BOUND ( 'NONE', #25460, .T. ) ;
#78481 = DIRECTION ( 'NONE',  ( -0.000000000000000000, 0.000000000000000000, 1.000000000000000000 ) ) ;
#78482 = CARTESIAN_POINT ( 'NONE',  ( 0.000000000000000000, 0.000000000000000000, 5.000000000000000000 ) ) ;
#78483 = LINE ( 'NONE', #46619, #23286 ) ;
#78484 = CARTESIAN_POINT ( 'NONE',  ( 120.7504301918981184, 3.055000000000002824, -5.291415217122919401 ) ) ;
#78485 = VERTEX_POINT ( 'NONE', #80479 ) ;
#78486 = EDGE_CURVE ( 'NONE', #132165, #27437, #79073, .T. ) ;
#78487 = CARTESIAN_POINT ( 'NONE',  ( 7.499999999999951150, -14.94781430457067906, 5.000000000000000000 ) ) ;
#78488 = PLANE ( 'NONE',  #24073 ) ;
#78489 = DIRECTION ( 'NONE',  ( 0.7071067811865487940, 0.7071067811865463515, 0.000000000000000000 ) ) ;
#78490 = FACE_OUTER_BOUND ( 'NONE', #62483, .T. ) ;
#78491 = PLANE ( 'NONE',  #118610 ) ;
#78492 = CARTESIAN_POINT ( 'NONE',  ( 25.36246187583883582, 22.22500000000000853, 4.000000000000000000 ) ) ;
#78493 = CARTESIAN_POINT ( 'NONE',  ( 44.55836038379621300, -7.949999999999997513, -2.130196079827425759 ) ) ;
#78494 = LINE ( 'NONE', #143029, #44525 ) ;
#78495 = DIRECTION ( 'NONE',  ( 0.6830127018922181881, 0.6830127018922202975, -0.2588190451025214056 ) ) ;
#78496 = ORIENTED_EDGE ( 'NONE', *, *, #88142, .F. ) ;
#78497 = ORIENTED_EDGE ( 'NONE', *, *, #85028, .T. ) ;
#78498 = CARTESIAN_POINT ( 'NONE',  ( 44.16666666666665719, 6.884901960086285300, 3.975000000000003642 ) ) ;
#78499 = CARTESIAN_POINT ( 'NONE',  ( -30.32816939922331656, -0.7407075233842770334, 4.000000000000000000 ) ) ;
#78500 = CARTESIAN_POINT ( 'NONE',  ( -6.183988606268994381, 28.73617430169791476, 5.000000000000000000 ) ) ;
#78501 = ORIENTED_EDGE ( 'NONE', *, *, #101835, .F. ) ;
#78502 = DIRECTION ( 'NONE',  ( 0.6830127018922180770, -0.6830127018922204085, -0.2588190451025213501 ) ) ;
#78503 = EDGE_CURVE ( 'NONE', #39995, #15337, #45720, .T. ) ;
#78504 = CARTESIAN_POINT ( 'NONE',  ( 45.48921356237309510, -27.52281430457087197, 5.000000000000000000 ) ) ;
#78505 = CARTESIAN_POINT ( 'NONE',  ( 40.39626352523143993, 4.472830434245840259, -4.472830434245839371 ) ) ;
#78506 = VERTEX_POINT ( 'NONE', #2137 ) ;
#78507 = CARTESIAN_POINT ( 'NONE',  ( -34.45011844616454511, -4.483719188362475627, 5.000000000000000888 ) ) ;
#78508 = VERTEX_POINT ( 'NONE', #56618 ) ;
#78509 = ORIENTED_EDGE ( 'NONE', *, *, #26545, .T. ) ;
#78510 = LINE ( 'NONE', #3755, #12480 ) ;
#78511 = VECTOR ( 'NONE', #51114, 1000.000000000000000 ) ;
#78512 = CIRCLE ( 'NONE', #46141, 1.749999999999999778 ) ;
#78513 =( GEOMETRIC_REPRESENTATION_CONTEXT ( 3 ) GLOBAL_UNCERTAINTY_ASSIGNED_CONTEXT ( ( #76709 ) ) GLOBAL_UNIT_ASSIGNED_CONTEXT ( ( #90263, #92392, #79455 ) ) REPRESENTATION_CONTEXT ( 'NONE', 'WORKASPACE' ) );
#78514 = FACE_OUTER_BOUND ( 'NONE', #86847, .T. ) ;
#78515 = LINE ( 'NONE', #121987, #102228 ) ;
#78516 = AXIS2_PLACEMENT_3D ( 'NONE', #83366, #72536, #17380 ) ;
#78517 = DIRECTION ( 'NONE',  ( -1.000000000000000000, -0.000000000000000000, -0.000000000000000000 ) ) ;
#78518 = ORIENTED_EDGE ( 'NONE', *, *, #135014, .T. ) ;
#78519 = LINE ( 'NONE', #15878, #16403 ) ;
#78520 = ORIENTED_EDGE ( 'NONE', *, *, #120226, .T. ) ;
#78521 = DIRECTION ( 'NONE',  ( 0.7071067811865486830, -0.7071067811865464625, -0.000000000000000000 ) ) ;
#78522 = CARTESIAN_POINT ( 'NONE',  ( 152.4000000000000057, 7.919999999999947526, -16.42230000000002832 ) ) ;
#78523 = DIRECTION ( 'NONE',  ( 1.000000000000000000, -2.496005001405478586E-15, -0.000000000000000000 ) ) ;
#78524 = DIRECTION ( 'NONE',  ( 0.000000000000000000, -1.000000000000000000, 0.000000000000000000 ) ) ;
#78525 = DIRECTION ( 'NONE',  ( -0.000000000000000000, 0.3543493200069153248, 0.9351131265310292928 ) ) ;
#78526 = LINE ( 'NONE', #36448, #85510 ) ;
#78527 = VECTOR ( 'NONE', #143531, 1000.000000000000227 ) ;
#78528 = EDGE_CURVE ( 'NONE', #80339, #28555, #14485, .T. ) ;
#78529 = EDGE_LOOP ( 'NONE', ( #33009, #109224, #80756, #81584, #121400, #93855 ) ) ;
#78530 =( BOUNDED_CURVE ( )  B_SPLINE_CURVE ( 3, ( #18480, #61357, #27967, #39578 ),
 .UNSPECIFIED., .F., .T. ) 
 B_SPLINE_CURVE_WITH_KNOTS ( ( 4, 4 ),
 ( 4.446051736530344911, 4.712388980384676351 ),
 .UNSPECIFIED. ) 
 CURVE ( )  GEOMETRIC_REPRESENTATION_ITEM ( )  RATIONAL_B_SPLINE_CURVE ( ( 1.000000000000000000, 0.9940974367313476501, 0.9940974367313476501, 1.000000000000000000 ) ) 
 REPRESENTATION_ITEM ( '' )  );
#78531 = CARTESIAN_POINT ( 'NONE',  ( 0.000000000000000000, 0.000000000000000000, 5.000000000000000000 ) ) ;
#78532 = CARTESIAN_POINT ( 'NONE',  ( 59.70376352523145158, 6.109999999999998543, 1.122388791418548911E-15 ) ) ;
#78533 = EDGE_CURVE ( 'NONE', #141976, #66880, #22065, .T. ) ;
#78535 = EDGE_CURVE ( 'NONE', #113749, #114341, #136980, .T. ) ;
#78534 = FACE_OUTER_BOUND ( 'NONE', #71148, .T. ) ;
#78536 = CARTESIAN_POINT ( 'NONE',  ( 6.183988606268994381, 28.73617430169791476, 5.000000000000000000 ) ) ;
#78537 = ORIENTED_EDGE ( 'NONE', *, *, #34550, .T. ) ;
#78538 = AXIS2_PLACEMENT_3D ( 'NONE', #124803, #25469, #42102 ) ;
#78539 = CARTESIAN_POINT ( 'NONE',  ( 18.18398860626898994, 28.73617430169800002, 5.000000000000000000 ) ) ;
#78540 = ORIENTED_EDGE ( 'NONE', *, *, #42409, .F. ) ;
#78541 = EDGE_CURVE ( 'NONE', #40388, #57093, #37686, .T. ) ;
#78542 = VECTOR ( 'NONE', #70672, 1000.000000000000000 ) ;
#78543 = DIRECTION ( 'NONE',  ( -0.000000000000000000, 0.3543493200069153248, 0.9351131265310292928 ) ) ;
#78544 = ORIENTED_EDGE ( 'NONE', *, *, #121412, .T. ) ;
#78545 = DIRECTION ( 'NONE',  ( 0.7071067811865487940, 0.7071067811865463515, -0.000000000000000000 ) ) ;
#78546 = LINE ( 'NONE', #952, #64146 ) ;
#78547 = DIRECTION ( 'NONE',  ( 0.6830127018922181881, 0.6830127018922202975, -0.2588190451025214056 ) ) ;
#78548 =( GEOMETRIC_REPRESENTATION_CONTEXT ( 3 ) GLOBAL_UNCERTAINTY_ASSIGNED_CONTEXT ( ( #65113 ) ) GLOBAL_UNIT_ASSIGNED_CONTEXT ( ( #87432, #99711, #30173 ) ) REPRESENTATION_CONTEXT ( 'NONE', 'WORKASPACE' ) );
#78549 = VECTOR ( 'NONE', #82238, 1000.000000000000000 ) ;
#78551 = VECTOR ( 'NONE', #22775, 1000.000000000000227 ) ;
#78550 = CARTESIAN_POINT ( 'NONE',  ( -22.49999999999984013, -2.568876922607784774, 4.000000000000000000 ) ) ;
#78552 = EDGE_CURVE ( 'NONE', #61902, #103852, #34826, .T. ) ;
#78553 = FACE_BOUND ( 'NONE', #55546, .T. ) ;
#78554 = EDGE_CURVE ( 'NONE', #71583, #10019, #102495, .T. ) ;
#78555 = CARTESIAN_POINT ( 'NONE',  ( 34.92499999999998295, -16.48753812416035203, 4.000000000000000000 ) ) ;
#78556 = CARTESIAN_POINT ( 'NONE',  ( -24.18398860626899705, 28.73617430169804265, 5.000000000000000000 ) ) ;
#78557 = CARTESIAN_POINT ( 'NONE',  ( 27.48921356237309155, -27.52281430457074762, 5.000000000000000000 ) ) ;
#78559 = ORIENTED_EDGE ( 'NONE', *, *, #87304, .F. ) ;
#78558 = CARTESIAN_POINT ( 'NONE',  ( -24.48921356237309510, -27.52281430457072631, 5.000000000000000000 ) ) ;
#78560 = AXIS2_PLACEMENT_3D ( 'NONE', #43354, #42661, #31759 ) ;
#78561 = VECTOR ( 'NONE', #87150, 1000.000000000000000 ) ;
#78562 = LINE ( 'NONE', #32938, #16214 ) ;
#78563 = EDGE_CURVE ( 'NONE', #143251, #47888, #7554, .T. ) ;
#78564 = ORIENTED_EDGE ( 'NONE', *, *, #125500, .T. ) ;
#78565 = ORIENTED_EDGE ( 'NONE', *, *, #32180, .F. ) ;
#78566 = CARTESIAN_POINT ( 'NONE',  ( 71.80793019189810877, -6.109999999999998543, 1.637169565754158507 ) ) ;
#78567 = ORIENTED_EDGE ( 'NONE', *, *, #101761, .T. ) ;
#78568 = FACE_OUTER_BOUND ( 'NONE', #91378, .T. ) ;
#78569 = CARTESIAN_POINT ( 'NONE',  ( 34.42499999999998295, 0.000000000000000000, 4.500000000000000888 ) ) ;
#78570 = ORIENTED_EDGE ( 'NONE', *, *, #139969, .T. ) ;
#78571 = DIRECTION ( 'NONE',  ( -1.000000000000000000, 0.000000000000000000, -0.000000000000000000 ) ) ;
#78572 = EDGE_CURVE ( 'NONE', #82088, #5782, #79797, .T. ) ;
#78573 = CARTESIAN_POINT ( 'NONE',  ( 26.90840764549667696, 2.500000000000003553, 3.061616997868386099E-16 ) ) ;
#78574 = DIRECTION ( 'NONE',  ( -0.7071067811865487940, 0.7071067811865463515, -0.000000000000000000 ) ) ;
#78575 = CARTESIAN_POINT ( 'NONE',  ( 2.700255128608413990, -27.71228299555204089, 4.000000000000000000 ) ) ;
#78576 = FACE_OUTER_BOUND ( 'NONE', #68951, .T. ) ;
#78577 = ORIENTED_EDGE ( 'NONE', *, *, #54485, .T. ) ;
#78578 = EDGE_CURVE ( 'NONE', #92260, #96833, #113069, .T. ) ;
#78579 = ORIENTED_EDGE ( 'NONE', *, *, #126146, .T. ) ;
#78580 = CYLINDRICAL_SURFACE ( 'NONE', #65907, 0.5000000000000004441 ) ;
#78581 = SURFACE_STYLE_FILL_AREA ( #65601 ) ;
#78582 = VERTEX_POINT ( 'NONE', #102931 ) ;
#78583 = VERTEX_POINT ( 'NONE', #3572 ) ;
#78584 = ORIENTED_EDGE ( 'NONE', *, *, #77263, .F. ) ;
#78585 = DIRECTION ( 'NONE',  ( 0.7071067811865486830, -0.7071067811865464625, -0.000000000000000000 ) ) ;
#78586 = CARTESIAN_POINT ( 'NONE',  ( 26.10459685856476852, 1.637169565754164946, -6.109999999999999432 ) ) ;
#78587 = ORIENTED_EDGE ( 'NONE', *, *, #48362, .F. ) ;
#78588 = CARTESIAN_POINT ( 'NONE',  ( 12.09667064187398111, -2.240707523384257716, 15.26439735382755281 ) ) ;
#78589 = EDGE_CURVE ( 'NONE', #77094, #128364, #92031, .T. ) ;
#78590 = FACE_OUTER_BOUND ( 'NONE', #49053, .T. ) ;
#78591 = CARTESIAN_POINT ( 'NONE',  ( 0.9420698081018860082, 7.934999999999993392, 2.126176841940951689 ) ) ;
#78592 = CARTESIAN_POINT ( 'NONE',  ( 15.78777360247684847, 2.639113497459678825, -32.92661230006952877 ) ) ;
#78593 = ORIENTED_EDGE ( 'NONE', *, *, #109642, .F. ) ;
#78594 = DIRECTION ( 'NONE',  ( -0.7071067811865487940, 0.7071067811865463515, -0.000000000000000000 ) ) ;
#78595 = CARTESIAN_POINT ( 'NONE',  ( -36.48921356237310221, -27.52281430457080802, 5.000000000000000000 ) ) ;
#78596 = DIRECTION ( 'NONE',  ( 0.6830127018922181881, 0.6830127018922202975, -0.2588190451025214056 ) ) ;
#78598 = ORIENTED_EDGE ( 'NONE', *, *, #29135, .T. ) ;
#78597 = DIRECTION ( 'NONE',  ( -0.3543493200069162685, -0.000000000000000000, -0.9351131265310288487 ) ) ;
#78599 = ORIENTED_EDGE ( 'NONE', *, *, #114218, .F. ) ;
#78600 =( NAMED_UNIT ( * ) PLANE_ANGLE_UNIT ( ) SI_UNIT ( $, .RADIAN. ) );
#78601 = CARTESIAN_POINT ( 'NONE',  ( 27.32816939922334143, 20.25929247661551003, 4.000000000000000000 ) ) ;
#78602 = EDGE_LOOP ( 'NONE', ( #47883, #113942, #133268, #34876 ) ) ;
#78603 = CARTESIAN_POINT ( 'NONE',  ( -26.99999999999980815, -22.22500000000000142, 4.412002311790036657 ) ) ;
#78604 = CARTESIAN_POINT ( 'NONE',  ( -8.207106781186482181, -5.240707523384228850, 5.000000000000000000 ) ) ;
#78605 = ORIENTED_EDGE ( 'NONE', *, *, #98197, .T. ) ;
#78606 = EDGE_CURVE ( 'NONE', #136324, #133168, #89892, .T. ) ;
#78607 = DIRECTION ( 'NONE',  ( 0.7071067811865486830, -0.7071067811865464625, -0.000000000000000000 ) ) ;
#78608 = CARTESIAN_POINT ( 'NONE',  ( 27.39583333333332504, -2.130196079827427091, 7.949999999999998401 ) ) ;
#78609 = CARTESIAN_POINT ( 'NONE',  ( 12.29974487139158512, -27.71228299555214747, 4.000000000000000000 ) ) ;
#78610 = AXIS2_PLACEMENT_3D ( 'NONE', #37948, #115442, #16135 ) ;
#78611 =( GEOMETRIC_REPRESENTATION_CONTEXT ( 3 ) GLOBAL_UNCERTAINTY_ASSIGNED_CONTEXT ( ( #109985 ) ) GLOBAL_UNIT_ASSIGNED_CONTEXT ( ( #65078, #30279, #44780 ) ) REPRESENTATION_CONTEXT ( 'NONE', 'WORKASPACE' ) );
#78612 = VECTOR ( 'NONE', #53080, 1000.000000000000000 ) ;
#78613 = DIRECTION ( 'NONE',  ( 1.000000000000000000, 1.224606353822377258E-16, 0.000000000000000000 ) ) ;
#78614 = DIRECTION ( 'NONE',  ( -1.000000000000000000, -1.224606353822377258E-16, -0.000000000000000000 ) ) ;
#78615 = DIRECTION ( 'NONE',  ( -0.000000000000000000, 0.000000000000000000, 1.000000000000000000 ) ) ;
#78616 = VECTOR ( 'NONE', #24354, 1000.000000000000227 ) ;
#78617 = CARTESIAN_POINT ( 'NONE',  ( -0.005480084712502889671, 28.92564299267938210, 4.000000000000000000 ) ) ;
#78618 = CARTESIAN_POINT ( 'NONE',  ( -27.83829387547363510, -6.740707523384205757, 16.75550250614860914 ) ) ;
#78620 = EDGE_CURVE ( 'NONE', #139077, #5268, #134138, .T. ) ;
#78619 = ORIENTED_EDGE ( 'NONE', *, *, #110021, .F. ) ;
#78621 = ORIENTED_EDGE ( 'NONE', *, *, #105560, .F. ) ;
#78622 = CARTESIAN_POINT ( 'NONE',  ( 3.489213562373097322, -27.52281430457057709, 5.000000000000000000 ) ) ;
#78623 = CIRCLE ( 'NONE', #53138, 2.500000000000000888 ) ;
#78624 = LINE ( 'NONE', #122837, #138555 ) ;
#78625 = PLANE ( 'NONE',  #45147 ) ;
#78626 = CARTESIAN_POINT ( 'NONE',  ( -34.92500000000001137, -3.281509562795737800, 4.759050581649335143 ) ) ;
#78627 = VERTEX_POINT ( 'NONE', #23946 ) ;
#78628 = VECTOR ( 'NONE', #37622, 1000.000000000000227 ) ;
#78629 = DIRECTION ( 'NONE',  ( -0.7071067811865486830, 0.7071067811865464625, 0.000000000000000000 ) ) ;
#78630 = CARTESIAN_POINT ( 'NONE',  ( -34.92500000000001137, -22.22500000000000142, 4.000000000000000000 ) ) ;
#78631 = ORIENTED_EDGE ( 'NONE', *, *, #77217, .T. ) ;
#78632 = LINE ( 'NONE', #2460, #125214 ) ;
#78633 = CARTESIAN_POINT ( 'NONE',  ( -34.92500000000001137, 21.72500000000000142, 5.000000000000000000 ) ) ;
#78634 = DIRECTION ( 'NONE',  ( -0.000000000000000000, 0.3543493200069153248, 0.9351131265310292928 ) ) ;
#78635 = VECTOR ( 'NONE', #99853, 999.9999999999998863 ) ;
#78636 = VECTOR ( 'NONE', #99132, 1000.000000000000000 ) ;
#78637 = PLANE ( 'NONE',  #89833 ) ;
#78638 = CARTESIAN_POINT ( 'NONE',  ( 59.55793019189812298, 6.110000000000001208, -1.637169565754156286 ) ) ;
#78639 = LINE ( 'NONE', #143172, #53382 ) ;
#78640 = CARTESIAN_POINT ( 'NONE',  ( 12.69999999999999574, -40.43000000000000682, -39.50000000000000000 ) ) ;
#78641 = LINE ( 'NONE', #21407, #27986 ) ;
#78642 = EDGE_CURVE ( 'NONE', #133340, #13138, #28222, .T. ) ;
#78643 = ORIENTED_EDGE ( 'NONE', *, *, #29604, .F. ) ;
#78644 = DIRECTION ( 'NONE',  ( 0.000000000000000000, -0.000000000000000000, 1.000000000000000000 ) ) ;
#78645 = ORIENTED_EDGE ( 'NONE', *, *, #112266, .T. ) ;
#78646 = CARTESIAN_POINT ( 'NONE',  ( 8.292893218813404133, -12.74070752338415247, 5.000000000000000000 ) ) ;
#78647 = VECTOR ( 'NONE', #122727, 999.9999999999998863 ) ;
#78648 = VECTOR ( 'NONE', #137678, 999.9999999999998863 ) ;
#78649 = PLANE ( 'NONE',  #103963 ) ;
#78650 = DIRECTION ( 'NONE',  ( -0.000000000000000000, -0.3543493200069152693, 0.9351131265310292928 ) ) ;
#78651 = LINE ( 'NONE', #33041, #87868 ) ;
#78652 = ADVANCED_FACE ( 'NONE', ( #126792 ), #105739, .F. ) ;
#78653 = CARTESIAN_POINT ( 'NONE',  ( -34.49999999999976552, 13.46425560840034841, 4.994342998332165884 ) ) ;
#78654 = DIRECTION ( 'NONE',  ( -0.7071067811865487940, 0.7071067811865463515, -0.000000000000000000 ) ) ;
#78655 = ORIENTED_EDGE ( 'NONE', *, *, #111043, .T. ) ;
#78657 = ADVANCED_FACE ( 'NONE', ( #116643 ), #27478, .F. ) ;
#78656 = VECTOR ( 'NONE', #129863, 1000.000000000000000 ) ;
#78658 = ORIENTED_EDGE ( 'NONE', *, *, #38670, .F. ) ;
#78659 = CARTESIAN_POINT ( 'NONE',  ( -33.18398860626899705, 28.73617430169810305, 5.000000000000000000 ) ) ;
#78660 = VECTOR ( 'NONE', #116283, 1000.000000000000000 ) ;
#78661 = CARTESIAN_POINT ( 'NONE',  ( -13.77797537283184326, 22.22500000000000142, 13.01339814852647869 ) ) ;
#78662 = PLANE ( 'NONE',  #126950 ) ;
#78663 = CARTESIAN_POINT ( 'NONE',  ( 71.53752705046289861, -9.735942053221456900E-16, 7.949999999999998401 ) ) ;
#78664 = DIRECTION ( 'NONE',  ( 0.6830127018922181881, 0.6830127018922202975, -0.2588190451025214056 ) ) ;
#78665 = PLANE ( 'NONE',  #131729 ) ;
#78666 = EDGE_LOOP ( 'NONE', ( #80858, #123415, #96506, #111322 ) ) ;
#78667 = CARTESIAN_POINT ( 'NONE',  ( 72.89583333333331439, -2.130196079827427091, 7.949999999999999289 ) ) ;
#78668 = ADVANCED_FACE ( 'NONE', ( #84733 ), #18005, .F. ) ;
#78669 = CYLINDRICAL_SURFACE ( 'NONE', #81684, 7.950000000000000178 ) ;
#78670 = LINE ( 'NONE', #122146, #69465 ) ;
#78671 = FACE_OUTER_BOUND ( 'NONE', #7234, .T. ) ;
#78672 = AXIS2_PLACEMENT_3D ( 'NONE', #67066, #111249, #11943 ) ;
#78673 = VERTEX_POINT ( 'NONE', #60153 ) ;
#78674 = ADVANCED_FACE ( 'NONE', ( #73170 ), #40533, .F. ) ;
#78675 = LINE ( 'NONE', #125760, #120802 ) ;
#78676 = DIRECTION ( 'NONE',  ( 1.000000000000000000, 0.000000000000000000, 0.000000000000000000 ) ) ;
#78677 = CARTESIAN_POINT ( 'NONE',  ( 62.27126352523142572, 4.472830434245839371, 4.472830434245842035 ) ) ;
#78678 = ORIENTED_EDGE ( 'NONE', *, *, #80232, .F. ) ;
#78679 = ORIENTED_EDGE ( 'NONE', *, *, #5178, .F. ) ;
#78680 = LINE ( 'NONE', #104528, #132406 ) ;
#78681 = CARTESIAN_POINT ( 'NONE',  ( 27.15612307739222331, -22.22500000000000142, 4.000000000000000000 ) ) ;
#78682 = LINE ( 'NONE', #124320, #27816 ) ;
#78683 = CARTESIAN_POINT ( 'NONE',  ( 14.51078643762690490, -27.52281430457045275, 5.000000000000000000 ) ) ;
#78685 = EDGE_LOOP ( 'NONE', ( #72488, #82675, #93616, #49416 ) ) ;
#78684 = FACE_OUTER_BOUND ( 'NONE', #142005, .T. ) ;
#78686 = DIRECTION ( 'NONE',  ( -1.000000000000000000, -1.224606353822377258E-16, -0.000000000000000000 ) ) ;
#78687 = CARTESIAN_POINT ( 'NONE',  ( -31.80981832425532829, -18.74070752338408852, 7.910009926591581753 ) ) ;
#78688 = CARTESIAN_POINT ( 'NONE',  ( -18.29974487139159223, -27.71228299555219010, 4.000000000000000000 ) ) ;
#78689 = EDGE_CURVE ( 'NONE', #54392, #22559, #94166, .T. ) ;
#78690 = CARTESIAN_POINT ( 'NONE',  ( 32.29289321881323360, -0.7407075233842770334, 5.000000000000000000 ) ) ;
#78691 = ORIENTED_EDGE ( 'NONE', *, *, #122511, .F. ) ;
#78693 = EDGE_CURVE ( 'NONE', #99319, #29884, #84057, .T. ) ;
#78692 = VERTEX_POINT ( 'NONE', #17329 ) ;
#78694 = CARTESIAN_POINT ( 'NONE',  ( 53.52126352523144703, -4.472830434245839371, -4.472830434245840259 ) ) ;
#78695 = EDGE_CURVE ( 'NONE', #16173, #36972, #77154, .T. ) ;
#78696 = ORIENTED_EDGE ( 'NONE', *, *, #7414, .T. ) ;
#78697 = DIRECTION ( 'NONE',  ( 1.000000000000000000, 0.000000000000000000, 0.000000000000000000 ) ) ;
#78698 = EDGE_CURVE ( 'NONE', #17086, #33380, #63015, .T. ) ;
#78699 = CARTESIAN_POINT ( 'NONE',  ( 18.48921356237309510, -27.52281430457068367, 5.000000000000000000 ) ) ;
#78700 = DIRECTION ( 'NONE',  ( 1.000000000000000000, 0.000000000000000000, 0.000000000000000000 ) ) ;
#78701 = LINE ( 'NONE', #47551, #124254 ) ;
#78702 = ORIENTED_EDGE ( 'NONE', *, *, #46954, .T. ) ;
#78703 = VERTEX_POINT ( 'NONE', #85424 ) ;
#78704 = DIRECTION ( 'NONE',  ( 0.3543493200069162685, -0.000000000000000000, -0.9351131265310288487 ) ) ;
#78705 = CARTESIAN_POINT ( 'NONE',  ( -17.53594656315045341, -3.178915670909185032, -35.18142205605356310 ) ) ;
#78706 = ADVANCED_FACE ( 'NONE', ( #74593 ), #39837, .T. ) ;
#78707 = EDGE_CURVE ( 'NONE', #15358, #44633, #117333, .T. ) ;
#78709 = ORIENTED_EDGE ( 'NONE', *, *, #137011, .T. ) ;
#78708 = VECTOR ( 'NONE', #112825, 999.9999999999998863 ) ;
#78710 = LINE ( 'NONE', #1804, #65311 ) ;
#78711 = PLANE ( 'NONE',  #138237 ) ;
#78712 = DIRECTION ( 'NONE',  ( 1.000000000000000000, -0.000000000000000000, -0.000000000000000000 ) ) ;
#78713 = VECTOR ( 'NONE', #104421, 1000.000000000000000 ) ;
#78714 = AXIS2_PLACEMENT_3D ( 'NONE', #129579, #86098, #132496 ) ;
#78715 = AXIS2_PLACEMENT_3D ( 'NONE', #107302, #65263, #29728 ) ;
#78716 = ORIENTED_EDGE ( 'NONE', *, *, #16416, .T. ) ;
#78717 = AXIS2_PLACEMENT_3D ( 'NONE', #105994, #116192, #50235 ) ;
#78718 = EDGE_CURVE ( 'NONE', #88501, #24531, #83319, .T. ) ;
#78719 = FACE_BOUND ( 'NONE', #20822, .T. ) ;
#78720 = ADVANCED_FACE ( 'NONE', ( #129653 ), #106444, .F. ) ;
#78721 = FACE_OUTER_BOUND ( 'NONE', #9078, .T. ) ;
#78722 = DIRECTION ( 'NONE',  ( 1.000000000000000000, 0.000000000000000000, 0.000000000000000000 ) ) ;
#78723 = CARTESIAN_POINT ( 'NONE',  ( -60.48921356237309510, -27.52281430457097500, 5.000000000000000000 ) ) ;
#78724 = AXIS2_PLACEMENT_3D ( 'NONE', #140016, #63187, #82769 ) ;
#78725 = CYLINDRICAL_SURFACE ( 'NONE', #38778, 2.500000000000000444 ) ;
#78726 = CARTESIAN_POINT ( 'NONE',  ( 23.81601139373100295, 28.73617430169770870, 5.000000000000000000 ) ) ;
#78727 = DIRECTION ( 'NONE',  ( -0.9584110683481068538, 0.2313212352929435167, 0.1671487665835038328 ) ) ;
#78728 = ORIENTED_EDGE ( 'NONE', *, *, #1078, .F. ) ;
#78729 = ORIENTED_EDGE ( 'NONE', *, *, #126938, .T. ) ;
#78730 = CARTESIAN_POINT ( 'NONE',  ( 104.3287635252314658, 0.000000000000000000, -6.109999999999998543 ) ) ;
#78731 = ORIENTED_EDGE ( 'NONE', *, *, #50244, .T. ) ;
#78732 = ADVANCED_FACE ( 'NONE', ( #61586 ), #139133, .T. ) ;
#78733 = SURFACE_SIDE_STYLE ('',( #31130 ) ) ;
#78734 = VERTEX_POINT ( 'NONE', #15857 ) ;
#78735 = VECTOR ( 'NONE', #123438, 1000.000000000000114 ) ;
#78736 = VECTOR ( 'NONE', #132551, 1000.000000000000227 ) ;
#78737 = PLANE ( 'NONE',  #111768 ) ;
#78738 = ADVANCED_FACE ( 'NONE', ( #49287 ), #137708, .F. ) ;
#78739 = DIRECTION ( 'NONE',  ( -1.000000000000000000, -1.224606353822377258E-16, -0.000000000000000000 ) ) ;
#78740 = VECTOR ( 'NONE', #41586, 1000.000000000000000 ) ;
#78741 = PLANE ( 'NONE',  #98102 ) ;
#78742 = ORIENTED_EDGE ( 'NONE', *, *, #93437, .T. ) ;
#78743 = CARTESIAN_POINT ( 'NONE',  ( 34.49999999999975842, -17.94567065516886117, 4.994342998332151673 ) ) ;
#78744 = DIRECTION ( 'NONE',  ( 0.7071067811865487940, 0.7071067811865463515, 0.000000000000000000 ) ) ;
#78745 = CARTESIAN_POINT ( 'NONE',  ( 19.49999999999985789, -1.592773361805355226, -6.492772025301275285 ) ) ;
#78746 = CARTESIAN_POINT ( 'NONE',  ( -14.81601139373099585, 28.73617430169776910, 5.000000000000000000 ) ) ;
#78747 = DIRECTION ( 'NONE',  ( -0.6830127018922180770, -0.6830127018922204085, -0.2588190451025213501 ) ) ;
#78748 = VECTOR ( 'NONE', #108377, 1000.000000000000000 ) ;
#78749 = CARTESIAN_POINT ( 'NONE',  ( 27.64169371712955936, -2.130196079827424871, -7.949999999999998401 ) ) ;
#78750 = EDGE_CURVE ( 'NONE', #94433, #135400, #11415, .T. ) ;
#78751 = CARTESIAN_POINT ( 'NONE',  ( -20.51078643762690490, -27.52281430457041012, 5.000000000000000000 ) ) ;
#78752 = ORIENTED_EDGE ( 'NONE', *, *, #106659, .T. ) ;
#78753 = VECTOR ( 'NONE', #59441, 1000.000000000000000 ) ;
#78754 = PLANE ( 'NONE',  #100543 ) ;
#78755 = CARTESIAN_POINT ( 'NONE',  ( -12.69999999999998153, 0.000000000000000000, 0.000000000000000000 ) ) ;
#78756 = ORIENTED_EDGE ( 'NONE', *, *, #6850, .F. ) ;
#78757 = ORIENTED_EDGE ( 'NONE', *, *, #77906, .F. ) ;
#78758 = VECTOR ( 'NONE', #69439, 1000.000000000000000 ) ;
#78759 = ORIENTED_EDGE ( 'NONE', *, *, #25118, .F. ) ;
#78761 = VECTOR ( 'NONE', #58948, 1000.000000000000000 ) ;
#78760 = CARTESIAN_POINT ( 'NONE',  ( 58.62543019189810423, 5.291415217122919401, 3.055000000000002824 ) ) ;
#78762 = EDGE_CURVE ( 'NONE', #81376, #69422, #53969, .T. ) ;
#78763 = ORIENTED_EDGE ( 'NONE', *, *, #5505, .T. ) ;
#78764 = CARTESIAN_POINT ( 'NONE',  ( 17.99999999999987921, 14.96639925780210412, 5.000000000000000000 ) ) ;
#78765 = EDGE_CURVE ( 'NONE', #86499, #86210, #65152, .T. ) ;
#78766 = VECTOR ( 'NONE', #51102, 999.9999999999998863 ) ;
#78767 = CARTESIAN_POINT ( 'NONE',  ( 5.295806282870439752, -5.278424836066144543, 3.047499999999995879 ) ) ;
#78768 = CARTESIAN_POINT ( 'NONE',  ( 92.02126352523143282, -4.472830434245838482, -4.472830434245840259 ) ) ;
#78769 = CARTESIAN_POINT ( 'NONE',  ( -20.70025512860841133, -27.71228299555191654, 4.000000000000000000 ) ) ;
#78770 = VERTEX_POINT ( 'NONE', #20164 ) ;
#78771 = CARTESIAN_POINT ( 'NONE',  ( 30.48921356237309510, -27.52281430457076894, 5.000000000000000000 ) ) ;
#78772 = EDGE_LOOP ( 'NONE', ( #56758, #109957, #5412, #113589, #39696 ) ) ;
#78773 = CARTESIAN_POINT ( 'NONE',  ( 0.1839886062690032631, 28.73617430169787568, 5.000000000000000000 ) ) ;
#78774 = VECTOR ( 'NONE', #41382, 1000.000000000000000 ) ;
#78775 = EDGE_CURVE ( 'NONE', #88325, #72440, #87592, .T. ) ;
#78776 = DIRECTION ( 'NONE',  ( 0.000000000000000000, -0.2631995976047557528, -0.9647414015272147703 ) ) ;
#78777 = ORIENTED_EDGE ( 'NONE', *, *, #38259, .T. ) ;
#78778 = FILL_AREA_STYLE ('',( #25074 ) ) ;
#78779 = FACE_OUTER_BOUND ( 'NONE', #78783, .T. ) ;
#78780 = CARTESIAN_POINT ( 'NONE',  ( 11.67183060077639212, -0.7407075233842701500, 4.000000000000000000 ) ) ;
#78781 = EDGE_LOOP ( 'NONE', ( #139392, #9893, #60334, #71748 ) ) ;
#78782 = PLANE ( 'NONE',  #105998 ) ;
#78783 = EDGE_LOOP ( 'NONE', ( #45270, #129420, #62929, #65198, #72939, #18747 ) ) ;
#78784 = ORIENTED_EDGE ( 'NONE', *, *, #38611, .T. ) ;
#78785 = ORIENTED_EDGE ( 'NONE', *, *, #43496, .F. ) ;
#78786 = DIRECTION ( 'NONE',  ( -1.000000000000000000, -0.000000000000000000, -0.000000000000000000 ) ) ;
#78787 = VECTOR ( 'NONE', #111185, 1000.000000000000227 ) ;
#78788 = CARTESIAN_POINT ( 'NONE',  ( 0.000000000000000000, 0.000000000000000000, 5.000000000000000000 ) ) ;
#78789 = CARTESIAN_POINT ( 'NONE',  ( -28.49999999999979750, 16.77039438581776665, 0.4657186855308382278 ) ) ;
#78790 = LINE ( 'NONE', #34568, #48698 ) ;
#78791 = CARTESIAN_POINT ( 'NONE',  ( 52.39921342269828841, -49.14999999999999147, 40.57473644908944976 ) ) ;
#78792 = EDGE_LOOP ( 'NONE', ( #6560, #130143, #52800, #116439 ) ) ;
#78793 = AXIS2_PLACEMENT_3D ( 'NONE', #43180, #9050, #29418 ) ;
#78794 = CLOSED_SHELL ( 'NONE', ( #133086, #38349, #72546, #13615, #26510, #117793, #136365, #66477, #133701, #72019, #107130, #72264, #47075, #141893, #72200, #92115, #32540, #56651, #114939, #74598, #106085, #139027, #25816, #131675, #47523, #91052, #106917, #55317, #63692, #110241, #65904, #57613, #58768, #84973, #142559, #100104, #54318, #41862, #48749, #26149, #133441, #19464, #143376, #93708, #98629, #133817, #114719, #115617, #106840, #143366, #86209, #129368, #110939, #143506, #139343, #127113, #84438, #15692, #103236, #78835, #58892, #16183, #7388, #99545, #93406, #125643, #141940, #2383, #108794, #105787, #103281, #125244, #125339, #62426, #85041, #77558, #125580, #26443, #93243, #10753, #108151, #92223, #19986, #25167, #110201, #35298, #18081, #105432, #128393, #49885, #78880, #34222, #113957, #138335, #10291, #82686, #82436, #70758, #56487, #59055, #110713, #87051, #131539, #26079, #77097, #7572, #134883, #91109, #24973, #81576, #40615, #106493, #86090, #28613, #100968, #116939, #139757, #107167, #136326, #51857, #39442, #21239, #84766, #103912, #84590, #3417, #129181, #133542, #84585 ) ) ;
#78795 = CARTESIAN_POINT ( 'NONE',  ( 0.000000000000000000, 0.000000000000000000, 5.000000000000000000 ) ) ;
#78796 = CARTESIAN_POINT ( 'NONE',  ( 16.31206980810189222, 7.934999999999993392, 2.126176841940951689 ) ) ;
#78797 = PLANE ( 'NONE',  #9112 ) ;
#78798 = LINE ( 'NONE', #136015, #87711 ) ;
#78799 = FACE_OUTER_BOUND ( 'NONE', #4338, .T. ) ;
#78800 = ORIENTED_EDGE ( 'NONE', *, *, #20444, .T. ) ;
#78801 = ORIENTED_EDGE ( 'NONE', *, *, #99420, .F. ) ;
#78802 = EDGE_CURVE ( 'NONE', #7326, #19604, #110732, .T. ) ;
#78803 = ORIENTED_EDGE ( 'NONE', *, *, #133303, .T. ) ;
#78804 = DIRECTION ( 'NONE',  ( 0.000000000000000000, 0.000000000000000000, 1.000000000000000000 ) ) ;
#78805 = PLANE ( 'NONE',  #53345 ) ;
#78806 = DIRECTION ( 'NONE',  ( -0.000000000000000000, 1.000000000000000000, -0.000000000000000000 ) ) ;
#78807 = VECTOR ( 'NONE', #93246, 1000.000000000000000 ) ;
#78808 = DIRECTION ( 'NONE',  ( 0.7071067811865486830, -0.7071067811865464625, -0.000000000000000000 ) ) ;
#78809 = CARTESIAN_POINT ( 'NONE',  ( 6.851954622386678295, 9.118668024956557261, 2.675793564507496836 ) ) ;
#78810 = AXIS2_PLACEMENT_3D ( 'NONE', #102335, #112477, #13842 ) ;
#78811 = VECTOR ( 'NONE', #134522, 1000.000000000000000 ) ;
#78812 = CARTESIAN_POINT ( 'NONE',  ( 16.49999999999988276, -17.91344420646041158, 1.358650452708503709 ) ) ;
#78813 = DIRECTION ( 'NONE',  ( -1.000000000000000000, -0.000000000000000000, -0.000000000000000000 ) ) ;
#78814 = CARTESIAN_POINT ( 'NONE',  ( 33.18398860626899705, 28.73617430169810305, 5.000000000000000000 ) ) ;
#78815 = DIRECTION ( 'NONE',  ( -0.6830127018922181881, 0.6830127018922202975, -0.2588190451025214056 ) ) ;
#78816 = VERTEX_POINT ( 'NONE', #42686 ) ;
#78817 = DIRECTION ( 'NONE',  ( 0.000000000000000000, 0.000000000000000000, 1.000000000000000000 ) ) ;
#78818 = VECTOR ( 'NONE', #104546, 1000.000000000000000 ) ;
#78819 = ORIENTED_EDGE ( 'NONE', *, *, #122834, .F. ) ;
#78820 = VECTOR ( 'NONE', #106366, 1000.000000000000227 ) ;
#78821 = CIRCLE ( 'NONE', #97191, 2.500000000000000888 ) ;
#78822 = AXIS2_PLACEMENT_3D ( 'NONE', #120855, #67207, #87531 ) ;
#78824 = CARTESIAN_POINT ( 'NONE',  ( 16.55061708910404761, 0.6983515413187854071, -33.57195487390330157 ) ) ;
#78823 = MECHANICAL_DESIGN_GEOMETRIC_PRESENTATION_REPRESENTATION (  '', ( #115811 ), #130052 ) ;
#78825 = ORIENTED_EDGE ( 'NONE', *, *, #108815, .T. ) ;
#78826 =( BOUNDED_CURVE ( )  B_SPLINE_CURVE ( 3, ( #103847, #16880, #49539, #16120 ),
 .UNSPECIFIED., .F., .T. ) 
 B_SPLINE_CURVE_WITH_KNOTS ( ( 4, 4 ),
 ( 5.135034128376270601, 5.164990091338616196 ),
 .UNSPECIFIED. ) 
 CURVE ( )  GEOMETRIC_REPRESENTATION_ITEM ( )  RATIONAL_B_SPLINE_CURVE ( ( 1.000000000000000000, 0.9999252214215840207, 0.9999252214215840207, 1.000000000000000000 ) ) 
 REPRESENTATION_ITEM ( '' )  );
#78827 = CIRCLE ( 'NONE', #27895, 6.094999999999989093 ) ;
#78828 = CARTESIAN_POINT ( 'NONE',  ( 17.69163961620376568, 6.094999999999988205, -1.633150327867694651 ) ) ;
#78830 = VERTEX_POINT ( 'NONE', #66563 ) ;
#78829 = DIRECTION ( 'NONE',  ( -0.000000000000000000, 0.000000000000000000, 1.000000000000000000 ) ) ;
#78831 = EDGE_CURVE ( 'NONE', #30060, #558, #125668, .T. ) ;
#78832 = SURFACE_SIDE_STYLE ('',( #123042 ) ) ;
#78833 = PLANE ( 'NONE',  #102776 ) ;
#78834 = ORIENTED_EDGE ( 'NONE', *, *, #94110, .F. ) ;
#78835 = ADVANCED_FACE ( 'NONE', ( #131817 ), #22293, .T. ) ;
#78836 =( NAMED_UNIT ( * ) SI_UNIT ( $, .STERADIAN. ) SOLID_ANGLE_UNIT ( ) );
#78837 = ORIENTED_EDGE ( 'NONE', *, *, #88654, .F. ) ;
#78838 = LINE ( 'NONE', #36052, #81428 ) ;
#78839 = AXIS2_PLACEMENT_3D ( 'NONE', #32681, #131261, #42134 ) ;
#78840 = ORIENTED_EDGE ( 'NONE', *, *, #57302, .T. ) ;
#78841 = EDGE_CURVE ( 'NONE', #121292, #6949, #44853, .T. ) ;
#78842 = CARTESIAN_POINT ( 'NONE',  ( -26.99451991528749417, 28.92564299267956685, 4.000000000000000000 ) ) ;
#78843 = CARTESIAN_POINT ( 'NONE',  ( 99.10002705046288440, 5.819803920172570422, 5.819803920172574863 ) ) ;
#78844 = PLANE ( 'NONE',  #20852 ) ;
#78845 = CARTESIAN_POINT ( 'NONE',  ( -27.48921356237309155, -27.52281430457074762, 5.000000000000000000 ) ) ;
#78846 = EDGE_LOOP ( 'NONE', ( #41046, #3708, #114702, #23443, #81323 ) ) ;
#78847 = EDGE_CURVE ( 'NONE', #131273, #115014, #21625, .T. ) ;
#78848 = DIRECTION ( 'NONE',  ( 0.000000000000000000, -1.000000000000000000, 0.000000000000000000 ) ) ;
#78849 = CARTESIAN_POINT ( 'NONE',  ( 28.82816939922332722, 6.759292476615644141, 4.000000000000000000 ) ) ;
#78850 = PLANE ( 'NONE',  #115551 ) ;
#78851 = CARTESIAN_POINT ( 'NONE',  ( 11.66666666666666785, -5.278424836066145431, -3.047499999999993658 ) ) ;
#78853 = VECTOR ( 'NONE', #68191, 999.9999999999998863 ) ;
#78852 = CARTESIAN_POINT ( 'NONE',  ( 22.43706980810188867, 2.126176841940952134, -7.934999999999992504 ) ) ;
#78854 = DIRECTION ( 'NONE',  ( -0.7071067811865486830, -0.7071067811865464625, 0.000000000000000000 ) ) ;
#78855 = CARTESIAN_POINT ( 'NONE',  ( 18.18398860626898994, 28.73617430169800002, 5.000000000000000000 ) ) ;
#78856 = ORIENTED_EDGE ( 'NONE', *, *, #113959, .F. ) ;
#78857 = ORIENTED_EDGE ( 'NONE', *, *, #74624, .F. ) ;
#78858 = EDGE_CURVE ( 'NONE', #13678, #57193, #33257, .T. ) ;
#78859 = AXIS2_PLACEMENT_3D ( 'NONE', #38578, #15357, #59642 ) ;
#78860 = LINE ( 'NONE', #13549, #69842 ) ;
#78861 = VERTEX_POINT ( 'NONE', #10708 ) ;
#78862 = VECTOR ( 'NONE', #92815, 1000.000000000000000 ) ;
#78863 = CARTESIAN_POINT ( 'NONE',  ( 98.14626352523144703, -4.472830434245840259, 4.472830434245839371 ) ) ;
#78864 = AXIS2_PLACEMENT_3D ( 'NONE', #111659, #123971, #122512 ) ;
#78865 = FACE_OUTER_BOUND ( 'NONE', #73038, .T. ) ;
#78866 = CARTESIAN_POINT ( 'NONE',  ( 17.85999999999999943, 2.055000000000001492, 0.000000000000000000 ) ) ;
#78867 = DIRECTION ( 'NONE',  ( 0.7071067811865487940, -0.7071067811865463515, 0.000000000000000000 ) ) ;
#78868 = DIRECTION ( 'NONE',  ( 0.7071067811865487940, -0.7071067811865463515, 0.000000000000000000 ) ) ;
#78869 = ORIENTED_EDGE ( 'NONE', *, *, #140665, .F. ) ;
#78870 = EDGE_CURVE ( 'NONE', #78244, #125983, #118779, .T. ) ;
#78871 = VECTOR ( 'NONE', #119789, 999.9999999999998863 ) ;
#78872 = CARTESIAN_POINT ( 'NONE',  ( 28.00000000000002487, -49.14999999999999147, 34.92500000000003268 ) ) ;
#78873 = SURFACE_STYLE_FILL_AREA ( #12151 ) ;
#78874 = DIRECTION ( 'NONE',  ( 0.6830127018922180770, -0.6830127018922204085, -0.2588190451025213501 ) ) ;
#78875 = FACE_OUTER_BOUND ( 'NONE', #138578, .T. ) ;
#78876 = AXIS2_PLACEMENT_3D ( 'NONE', #91123, #124433, #25104 ) ;
#78878 = ORIENTED_EDGE ( 'NONE', *, *, #102063, .F. ) ;
#78877 = FACE_OUTER_BOUND ( 'NONE', #120501, .T. ) ;
#78879 = FACE_OUTER_BOUND ( 'NONE', #127650, .T. ) ;
#78880 = ADVANCED_FACE ( 'NONE', ( #96990 ), #107878, .T. ) ;
#78881 = CARTESIAN_POINT ( 'NONE',  ( 6.940000000000001279, -2.055000000000000160, 2.789133085058098087E-16 ) ) ;
#78882 = CARTESIAN_POINT ( 'NONE',  ( 24.48921356237309510, -27.52281430457072631, 5.000000000000000000 ) ) ;
#78883 = ADVANCED_FACE ( 'NONE', ( #141996 ), #91192, .T. ) ;
#78884 = CARTESIAN_POINT ( 'NONE',  ( 14.99451991528749595, 28.92564299267948513, 4.000000000000000000 ) ) ;
#78885 = LINE ( 'NONE', #34649, #104702 ) ;
#78886 = EDGE_LOOP ( 'NONE', ( #114000, #117369, #131465, #63940 ) ) ;
#78887 = ORIENTED_EDGE ( 'NONE', *, *, #4358, .T. ) ;
#78888 = ORIENTED_EDGE ( 'NONE', *, *, #63217, .T. ) ;
#78889 = CARTESIAN_POINT ( 'NONE',  ( 94.79209685856476142, -5.291415217122921177, 3.054999999999999272 ) ) ;
#78890 = PRESENTATION_LAYER_ASSIGNMENT (  '', '', ( #122841 ) ) ;
#78891 = ORIENTED_EDGE ( 'NONE', *, *, #87004, .T. ) ;
#78892 = CARTESIAN_POINT ( 'NONE',  ( -12.69999999999998153, 3.061616997868383634E-16, -2.500000000000000444 ) ) ;
#78893 = ADVANCED_FACE ( 'NONE', ( #48367 ), #47005, .F. ) ;
#78894 = CYLINDRICAL_SURFACE ( 'NONE', #105853, 2.500000000000000000 ) ;
#78895 = VECTOR ( 'NONE', #120165, 999.9999999999998863 ) ;
#78896 = DIRECTION ( 'NONE',  ( -0.7071067811865487940, 0.7071067811865463515, -0.000000000000000000 ) ) ;
#78897 = CARTESIAN_POINT ( 'NONE',  ( -20.99451991528748707, 28.92564299267952777, 4.000000000000000000 ) ) ;
#78898 = ORIENTED_EDGE ( 'NONE', *, *, #108905, .T. ) ;
#78899 = DIRECTION ( 'NONE',  ( -0.6830127018922181881, 0.6830127018922202975, -0.2588190451025214056 ) ) ;
#78900 = DIRECTION ( 'NONE',  ( 0.000000000000000000, 0.3543493200069153248, 0.9351131265310291818 ) ) ;
#78901 = EDGE_CURVE ( 'NONE', #80773, #140269, #58593, .T. ) ;
#78902 = EDGE_CURVE ( 'NONE', #80281, #45110, #57141, .T. ) ;
#78903 = DIRECTION ( 'NONE',  ( -1.000000000000000000, -1.224606353822377258E-16, -0.000000000000000000 ) ) ;
#78904 = CARTESIAN_POINT ( 'NONE',  ( 86.09959685856478018, -6.109999999999997655, -1.637169565754160283 ) ) ;
#78905 = VERTEX_POINT ( 'NONE', #92560 ) ;
#78906 = LINE ( 'NONE', #102787, #11851 ) ;
#78907 = LINE ( 'NONE', #23792, #74761 ) ;
#78908 = VECTOR ( 'NONE', #44204, 999.9999999999998863 ) ;
#78909 = EDGE_CURVE ( 'NONE', #122922, #72201, #69429, .T. ) ;
#78910 = ORIENTED_EDGE ( 'NONE', *, *, #71640, .F. ) ;
#78911 = VERTEX_POINT ( 'NONE', #114334 ) ;
#78912 = DIRECTION ( 'NONE',  ( 0.6830127018922181881, 0.6830127018922202975, -0.2588190451025214056 ) ) ;
#78913 = EDGE_CURVE ( 'NONE', #40388, #122448, #136088, .T. ) ;
#78914 = CARTESIAN_POINT ( 'NONE',  ( 22.81706980810188767, -2.126176841940956130, 7.934999999999990727 ) ) ;
#78915 = DIRECTION ( 'NONE',  ( -0.7071067811865487940, 0.7071067811865463515, -0.000000000000000000 ) ) ;
#78916 = AXIS2_PLACEMENT_3D ( 'NONE', #126959, #16029, #58925 ) ;
#78917 = CARTESIAN_POINT ( 'NONE',  ( 3.102554694470408325, -48.63825160239813528, -38.47250499286691650 ) ) ;
#78918 = CARTESIAN_POINT ( 'NONE',  ( 15.21247294953710671, 0.000000000000000000, 6.094999999999989981 ) ) ;
#78919 = DIRECTION ( 'NONE',  ( -0.3543493200069162685, -0.000000000000000000, -0.9351131265310288487 ) ) ;
#78920 = ORIENTED_EDGE ( 'NONE', *, *, #50756, .F. ) ;
#78921 = ORIENTED_EDGE ( 'NONE', *, *, #69245, .T. ) ;
#78922 = EDGE_CURVE ( 'NONE', #84015, #5780, #122332, .T. ) ;
#78923 = CARTESIAN_POINT ( 'NONE',  ( -34.82816939922328459, -2.240707523384260824, 4.000000000000000000 ) ) ;
#78924 = ORIENTED_EDGE ( 'NONE', *, *, #114224, .F. ) ;
#78925 = EDGE_LOOP ( 'NONE', ( #135811, #124049, #138736, #19368 ) ) ;
#78927 = ADVANCED_FACE ( 'NONE', ( #123090 ), #45550, .F. ) ;
#78926 = VECTOR ( 'NONE', #16760, 1000.000000000000227 ) ;
#78928 = VECTOR ( 'NONE', #76804, 999.9999999999998863 ) ;
#78929 = VECTOR ( 'NONE', #7726, 1000.000000000000000 ) ;
#78930 = DIRECTION ( 'NONE',  ( -0.3543493200069162685, -0.000000000000000000, -0.9351131265310288487 ) ) ;
#78931 = EDGE_LOOP ( 'NONE', ( #21256, #108746, #54719, #40350, #113971 ) ) ;
#78932 = CARTESIAN_POINT ( 'NONE',  ( 56.37086038379622721, 6.884901960086289741, -3.974999999999993427 ) ) ;
#78933 = DIRECTION ( 'NONE',  ( 1.000000000000000000, 1.224606353822377258E-16, 0.000000000000000000 ) ) ;
#78934 = DIRECTION ( 'NONE',  ( 1.000000000000000000, 0.000000000000000000, 0.000000000000000000 ) ) ;
#78935 = VECTOR ( 'NONE', #121907, 1000.000000000000000 ) ;
#78936 = AXIS2_PLACEMENT_3D ( 'NONE', #132521, #44809, #142643 ) ;
#78937 = VECTOR ( 'NONE', #131587, 1000.000000000000227 ) ;
#78938 = VECTOR ( 'NONE', #97181, 1000.000000000000227 ) ;
#78939 = DIRECTION ( 'NONE',  ( 0.6830127018922180770, -0.6830127018922204085, -0.2588190451025213501 ) ) ;
#78940 = ORIENTED_EDGE ( 'NONE', *, *, #136031, .T. ) ;
#78941 = AXIS2_PLACEMENT_3D ( 'NONE', #5448, #117768, #41676 ) ;
#78942 = CARTESIAN_POINT ( 'NONE',  ( -12.51168605928424249, 6.759292476615645917, 16.35960578974472313 ) ) ;
#78943 = ORIENTED_EDGE ( 'NONE', *, *, #85655, .F. ) ;
#78944 = DIRECTION ( 'NONE',  ( 0.000000000000000000, -1.000000000000000000, 0.000000000000000000 ) ) ;
#78945 = EDGE_LOOP ( 'NONE', ( #36272, #2050, #126869, #30030, #108820, #55224 ) ) ;
#78946 = CARTESIAN_POINT ( 'NONE',  ( -41.99451991528749062, 28.92564299267967343, 4.000000000000000000 ) ) ;
#78947 = ORIENTED_EDGE ( 'NONE', *, *, #21103, .F. ) ;
#78948 = CARTESIAN_POINT ( 'NONE',  ( -31.17183060077625001, 9.759292476615625489, 4.000000000000000000 ) ) ;
#78949 = VERTEX_POINT ( 'NONE', #68715 ) ;
#78950 = ORIENTED_EDGE ( 'NONE', *, *, #98504, .F. ) ;
#78951 = VECTOR ( 'NONE', #61429, 1000.000000000000000 ) ;
#78952 = ORIENTED_EDGE ( 'NONE', *, *, #136249, .F. ) ;
#78953 = ADVANCED_FACE ( 'NONE', ( #123813 ), #113614, .T. ) ;
#78954 = DIRECTION ( 'NONE',  ( -0.6830127018922181881, 0.6830127018922202975, -0.2588190451025214056 ) ) ;
#78955 = CARTESIAN_POINT ( 'NONE',  ( -69.18398860626899705, 28.73617430169835529, 5.000000000000000000 ) ) ;
#78956 = CARTESIAN_POINT ( 'NONE',  ( 17.39159235450332019, 9.902892378096218942E-16, 0.000000000000000000 ) ) ;
#78957 = DIRECTION ( 'NONE',  ( 0.000000000000000000, 0.000000000000000000, 1.000000000000000000 ) ) ;
#78958 = CARTESIAN_POINT ( 'NONE',  ( 119.1462635252314470, -4.472830434245840259, 4.472830434245838482 ) ) ;
#78959 = CARTESIAN_POINT ( 'NONE',  ( -29.99999999999979039, -19.44781430457063465, 5.000000000000000000 ) ) ;
#78960 = VECTOR ( 'NONE', #48061, 1000.000000000000227 ) ;
#78961 = CARTESIAN_POINT ( 'NONE',  ( 24.62910658713767731, 1.050808743928695277, 4.662926800793053772 ) ) ;
#78962 = PLANE ( 'NONE',  #110692 ) ;
#78963 = VECTOR ( 'NONE', #49780, 1000.000000000000000 ) ;
#78964 = CARTESIAN_POINT ( 'NONE',  ( 12.29974487139158512, -27.71228299555214747, 4.000000000000000000 ) ) ;
#78965 = CARTESIAN_POINT ( 'NONE',  ( 33.48921356237309510, -27.52281430457078670, 5.000000000000000000 ) ) ;
#78966 = ORIENTED_EDGE ( 'NONE', *, *, #109956, .T. ) ;
#78967 = AXIS2_PLACEMENT_3D ( 'NONE', #1622, #82620, #56086 ) ;
#78968 = PLANE ( 'NONE',  #48098 ) ;
#78969 = CARTESIAN_POINT ( 'NONE',  ( 34.45011844616451668, 1.516280811637481962, 5.000000000000000888 ) ) ;
#78970 = CARTESIAN_POINT ( 'NONE',  ( 56.99451991528749062, 28.92564299267978001, 4.000000000000000000 ) ) ;
#78971 = ORIENTED_EDGE ( 'NONE', *, *, #124678, .T. ) ;
#78972 = AXIS2_PLACEMENT_3D ( 'NONE', #18629, #62910, #107087 ) ;
#78973 = ORIENTED_EDGE ( 'NONE', *, *, #103620, .F. ) ;
#78974 = DIRECTION ( 'NONE',  ( 0.6830127018922180770, -0.6830127018922204085, -0.2588190451025213501 ) ) ;
#78975 = ORIENTED_EDGE ( 'NONE', *, *, #28124, .T. ) ;
#78976 = AXIS2_PLACEMENT_3D ( 'NONE', #51559, #95753, #141401 ) ;
#78977 = EDGE_LOOP ( 'NONE', ( #102682, #109754, #142713, #133488 ) ) ;
#78978 = DIRECTION ( 'NONE',  ( 0.000000000000000000, 0.000000000000000000, -1.000000000000000000 ) ) ;
#78979 = LINE ( 'NONE', #135489, #64079 ) ;
#78980 = DIRECTION ( 'NONE',  ( -0.3543493200069162685, -0.000000000000000000, -0.9351131265310288487 ) ) ;
#78981 = FACE_OUTER_BOUND ( 'NONE', #8762, .T. ) ;
#78982 = B_SPLINE_CURVE_WITH_KNOTS ( 'NONE', 3,
 ( #69921, #82907, #81497, #35860 ),
 .UNSPECIFIED., .F., .F.,
 ( 4, 4 ),
 ( 0.003913914403404828747, 0.004162342877716045109 ),
 .UNSPECIFIED. ) ;
#78983 = EDGE_LOOP ( 'NONE', ( #31940, #57608, #23876, #134909 ) ) ;
#78984 = DIRECTION ( 'NONE',  ( -1.000000000000000000, -0.000000000000000000, -0.000000000000000000 ) ) ;
#78985 = ORIENTED_EDGE ( 'NONE', *, *, #104390, .T. ) ;
#78986 = LINE ( 'NONE', #12959, #46876 ) ;
#78987 = VECTOR ( 'NONE', #1814, 1000.000000000000000 ) ;
#78988 = CARTESIAN_POINT ( 'NONE',  ( 19.46290314143521982, -3.967499999999994476, 6.871911579029513106 ) ) ;
#78989 = EDGE_LOOP ( 'NONE', ( #101248, #138703, #4307, #100404 ) ) ;
#78990 = CARTESIAN_POINT ( 'NONE',  ( 83.91209685856479439, 5.291415217122922066, -3.054999999999995275 ) ) ;
#78991 = FACE_OUTER_BOUND ( 'NONE', #26840, .T. ) ;
#78992 = DIRECTION ( 'NONE',  ( -0.7071067811865486830, 0.7071067811865464625, 0.000000000000000000 ) ) ;
#78993 = ORIENTED_EDGE ( 'NONE', *, *, #37862, .T. ) ;
#78994 = ORIENTED_EDGE ( 'NONE', *, *, #55880, .T. ) ;
#78995 = ADVANCED_FACE ( 'NONE', ( #112908 ), #67280, .F. ) ;
#78996 = AXIS2_PLACEMENT_3D ( 'NONE', #64968, #75833, #32327 ) ;
#78997 = VERTEX_POINT ( 'NONE', #25905 ) ;
#78998 = DIRECTION ( 'NONE',  ( -1.000000000000000000, -1.224606353822377258E-16, -0.000000000000000000 ) ) ;
#78999 = DIRECTION ( 'NONE',  ( -1.000000000000000000, -1.224606353822377258E-16, -0.000000000000000000 ) ) ;
#79000 = LINE ( 'NONE', #12273, #56648 ) ;
#79001 = AXIS2_PLACEMENT_3D ( 'NONE', #28882, #97693, #129594 ) ;
#79002 = DIRECTION ( 'NONE',  ( -0.5735764363510503783, -0.8191520442889886899, 0.000000000000000000 ) ) ;
#79003 = ORIENTED_EDGE ( 'NONE', *, *, #19855, .F. ) ;
#79004 = CARTESIAN_POINT ( 'NONE',  ( 3.183988606268992161, 28.73617430169789699, 5.000000000000000000 ) ) ;
#79005 = EDGE_CURVE ( 'NONE', #137801, #117180, #1954, .T. ) ;
#79006 = LINE ( 'NONE', #44227, #14221 ) ;
#79008 = VECTOR ( 'NONE', #120078, 1000.000000000000000 ) ;
#79007 = CARTESIAN_POINT ( 'NONE',  ( 27.53159235450332076, 2.500000000000001332, 0.000000000000000000 ) ) ;
#79009 = ADVANCED_FACE ( 'NONE', ( #112214 ), #70174, .F. ) ;
#79010 = VERTEX_POINT ( 'NONE', #136801 ) ;
#79011 = CARTESIAN_POINT ( 'NONE',  ( 14.48334561358944406, 22.22500000000000142, 4.500000000000000888 ) ) ;
#79012 = VECTOR ( 'NONE', #85189, 1000.000000000000000 ) ;
#79013 = CARTESIAN_POINT ( 'NONE',  ( 18.18398860626898994, 28.73617430169800002, 5.000000000000000000 ) ) ;
#79014 = ORIENTED_EDGE ( 'NONE', *, *, #7544, .T. ) ;
#79015 = EDGE_CURVE ( 'NONE', #82088, #122084, #78157, .T. ) ;
#79017 = VERTEX_POINT ( 'NONE', #133951 ) ;
#79016 = CARTESIAN_POINT ( 'NONE',  ( 121.7500000000000000, -9.735942053221458872E-16, 7.950000000000000178 ) ) ;
#79018 = ORIENTED_EDGE ( 'NONE', *, *, #113032, .F. ) ;
#79019 = ADVANCED_FACE ( 'NONE', ( #57849 ), #68034, .T. ) ;
#79020 = EDGE_CURVE ( 'NONE', #87384, #127177, #36087, .T. ) ;
#79021 = FACE_OUTER_BOUND ( 'NONE', #73698, .T. ) ;
#79022 = DIRECTION ( 'NONE',  ( 0.6830127018922181881, 0.6830127018922202975, -0.2588190451025214056 ) ) ;
#79024 = ORIENTED_EDGE ( 'NONE', *, *, #104009, .F. ) ;
#79023 = VECTOR ( 'NONE', #17323, 1000.000000000000000 ) ;
#79025 = FILL_AREA_STYLE_COLOUR ( '', #53566 ) ;
#79026 = ORIENTED_EDGE ( 'NONE', *, *, #89164, .T. ) ;
#79027 =( BOUNDED_CURVE ( )  B_SPLINE_CURVE ( 2, ( #110401, #118433, #51784 ),
 .UNSPECIFIED., .F., .T. ) 
 B_SPLINE_CURVE_WITH_KNOTS ( ( 3, 3 ),
 ( 0.01666666666666434884, 0.01798785857039796043 ),
 .UNSPECIFIED. ) 
 CURVE ( )  GEOMETRIC_REPRESENTATION_ITEM ( )  RATIONAL_B_SPLINE_CURVE ( ( 1.000000000000028422, 0.9837933319240432795, 0.9830033892749372448 ) ) 
 REPRESENTATION_ITEM ( '' )  );
#79028 = EDGE_CURVE ( 'NONE', #28418, #15743, #107632, .T. ) ;
#79029 = EDGE_CURVE ( 'NONE', #29586, #132528, #128058, .T. ) ;
#79030 = DIRECTION ( 'NONE',  ( 0.7071067811865487940, 0.7071067811865463515, 0.000000000000000000 ) ) ;
#79031 = DIRECTION ( 'NONE',  ( -0.7071067811865487940, 0.7071067811865463515, 0.000000000000000000 ) ) ;
#79032 = FACE_OUTER_BOUND ( 'NONE', #104911, .T. ) ;
#79033 = LINE ( 'NONE', #57275, #34566 ) ;
#79034 = CARTESIAN_POINT ( 'NONE',  ( -36.18398860626899705, 28.73617430169812437, 5.000000000000000000 ) ) ;
#79035 = EDGE_CURVE ( 'NONE', #5696, #18494, #49828, .T. ) ;
#79036 = DIRECTION ( 'NONE',  ( 0.3543493200069162685, -0.000000000000000000, -0.9351131265310288487 ) ) ;
#79037 = DIRECTION ( 'NONE',  ( 0.7071067811865487940, 0.7071067811865463515, 0.000000000000000000 ) ) ;
#79038 = DIRECTION ( 'NONE',  ( 2.110369192185896011E-16, -1.000000000000000000, 0.000000000000000000 ) ) ;
#79039 = CARTESIAN_POINT ( 'NONE',  ( 19.37456980810188867, 6.871911579029510442, -3.967499999999998916 ) ) ;
#79040 = CARTESIAN_POINT ( 'NONE',  ( 3.041236474768552966, 0.000000000000000000, 7.934999999999990727 ) ) ;
#79041 = LINE ( 'NONE', #25320, #29669 ) ;
#79042 = VECTOR ( 'NONE', #86286, 1000.000000000000000 ) ;
#79043 = CARTESIAN_POINT ( 'NONE',  ( 0.000000000000000000, 0.000000000000000000, 5.000000000000000000 ) ) ;
#79044 = CARTESIAN_POINT ( 'NONE',  ( -44.99451991528749772, 28.92564299267969474, 4.000000000000000000 ) ) ;
#79045 = ORIENTED_EDGE ( 'NONE', *, *, #46378, .T. ) ;
#79046 = ORIENTED_EDGE ( 'NONE', *, *, #51417, .T. ) ;
#79047 = VECTOR ( 'NONE', #104774, 999.9999999999998863 ) ;
#79049 = ADVANCED_FACE ( 'NONE', ( #29454 ), #28050, .F. ) ;
#79048 = CARTESIAN_POINT ( 'NONE',  ( 100.4583333333333286, 3.974999999999997424, 6.884901960086288852 ) ) ;
#79050 = VECTOR ( 'NONE', #39689, 1000.000000000000227 ) ;
#79051 = ORIENTED_EDGE ( 'NONE', *, *, #113793, .T. ) ;
#79052 = VERTEX_POINT ( 'NONE', #51241 ) ;
#79053 = VERTEX_POINT ( 'NONE', #137532 ) ;
#79054 = CARTESIAN_POINT ( 'NONE',  ( 11.72733514412567857, 3.821174125832445049E-16, 0.000000000000000000 ) ) ;
#79055 = CARTESIAN_POINT ( 'NONE',  ( -8.994519915287490619, 28.92564299267944250, 4.000000000000000000 ) ) ;
#79056 = CONICAL_SURFACE ( 'NONE', #69735, 2.500000000000000888, 0.9599310885968822538 ) ;
#79057 = VECTOR ( 'NONE', #12992, 1000.000000000000000 ) ;
#79058 = FACE_OUTER_BOUND ( 'NONE', #23306, .T. ) ;
#79059 = VERTEX_POINT ( 'NONE', #73019 ) ;
#79060 = FACE_OUTER_BOUND ( 'NONE', #59567, .T. ) ;
#79061 = VECTOR ( 'NONE', #19037, 1000.000000000000000 ) ;
#79062 = CARTESIAN_POINT ( 'NONE',  ( 9.668467411598506089, -18.74070752338409562, 20.73178291233843495 ) ) ;
#79063 = LINE ( 'NONE', #2127, #88149 ) ;
#79064 = CARTESIAN_POINT ( 'NONE',  ( 14.27159235450332098, 9.902892378096218942E-16, 0.000000000000000000 ) ) ;
#79065 = ORIENTED_EDGE ( 'NONE', *, *, #95218, .F. ) ;
#79066 = CARTESIAN_POINT ( 'NONE',  ( 127.0787635252314516, -7.482591942790325086E-16, 6.109999999999998543 ) ) ;
#79067 = CARTESIAN_POINT ( 'NONE',  ( 29.99999999999978684, -13.06887692260767686, 4.000000000000000000 ) ) ;
#79068 = DIRECTION ( 'NONE',  ( 0.7071067811865487940, -0.7071067811865463515, 0.000000000000000000 ) ) ;
#79069 = AXIS2_PLACEMENT_3D ( 'NONE', #123641, #24989, #133777 ) ;
#79070 = DIRECTION ( 'NONE',  ( 0.7071067811865487940, 0.7071067811865463515, 0.000000000000000000 ) ) ;
#79071 = EDGE_CURVE ( 'NONE', #59778, #99826, #93998, .T. ) ;
#79072 = CARTESIAN_POINT ( 'NONE',  ( -69.48921356237309510, -27.52281430457103895, 5.000000000000000000 ) ) ;
#79073 = LINE ( 'NONE', #101484, #127949 ) ;
#79074 = CARTESIAN_POINT ( 'NONE',  ( 34.42499999999998295, 8.977185695429312773, 5.000000000000000000 ) ) ;
#79075 = CARTESIAN_POINT ( 'NONE',  ( 16.76840764549667639, 9.139736423841732040E-16, 0.000000000000000000 ) ) ;
#79076 = ORIENTED_EDGE ( 'NONE', *, *, #49006, .F. ) ;
#79077 = ORIENTED_EDGE ( 'NONE', *, *, #23989, .F. ) ;
#79078 = CARTESIAN_POINT ( 'NONE',  ( 123.0837635252314470, -6.110000000000001208, -3.741295971395164515E-16 ) ) ;
#79079 = VERTEX_POINT ( 'NONE', #37514 ) ;
#79080 = ADVANCED_FACE ( 'NONE', ( #82434 ), #83889, .F. ) ;
#79081 = CARTESIAN_POINT ( 'NONE',  ( -3.707013264293017141, -21.74070752338405299, 4.999753212805222446 ) ) ;
#79082 = CARTESIAN_POINT ( 'NONE',  ( 24.32816939922335209, -21.74070752338406365, 4.000000000000000000 ) ) ;
#79083 = LINE ( 'NONE', #123289, #90679 ) ;
#79084 = DIRECTION ( 'NONE',  ( -0.6830127018922180770, -0.6830127018922204085, -0.2588190451025213501 ) ) ;
#79085 = VECTOR ( 'NONE', #43429, 1000.000000000000000 ) ;
#79086 = EDGE_CURVE ( 'NONE', #9095, #51427, #42519, .T. ) ;
#79087 = VECTOR ( 'NONE', #118051, 1000.000000000000000 ) ;
#79088 = CARTESIAN_POINT ( 'NONE',  ( 112.4954301918981230, 5.291415217122916737, 3.055000000000001936 ) ) ;
#79089 = ORIENTED_EDGE ( 'NONE', *, *, #96020, .F. ) ;
#79090 = ADVANCED_FACE ( 'NONE', ( #109882 ), #121463, .T. ) ;
#79091 = AXIS2_PLACEMENT_3D ( 'NONE', #82179, #103864, #137250 ) ;
#79092 = EDGE_LOOP ( 'NONE', ( #28364, #60221, #66543, #38204 ) ) ;
#79093 = VECTOR ( 'NONE', #20147, 1000.000000000000000 ) ;
#79094 = DIRECTION ( 'NONE',  ( -0.6830127018922181881, 0.6830127018922202975, -0.2588190451025214056 ) ) ;
#79095 = EDGE_CURVE ( 'NONE', #110079, #77841, #135975, .T. ) ;
#79096 = ORIENTED_EDGE ( 'NONE', *, *, #12349, .F. ) ;
#79097 = ORIENTED_EDGE ( 'NONE', *, *, #111270, .T. ) ;
#79098 = ORIENTED_EDGE ( 'NONE', *, *, #140839, .F. ) ;
#79099 = VECTOR ( 'NONE', #37082, 1000.000000000000000 ) ;
#79100 = CARTESIAN_POINT ( 'NONE',  ( -5.671830600776427644, 8.259292476615630818, 4.000000000000000000 ) ) ;
#79101 = PRESENTATION_STYLE_ASSIGNMENT (( #14511 ) ) ;
#79102 = EDGE_CURVE ( 'NONE', #82254, #116108, #19309, .T. ) ;
#79103 = CARTESIAN_POINT ( 'NONE',  ( 18.48921356237309510, -27.52281430457068367, 5.000000000000000000 ) ) ;
#79104 = ORIENTED_EDGE ( 'NONE', *, *, #69355, .F. ) ;
#79105 = EDGE_CURVE ( 'NONE', #13957, #110495, #109167, .T. ) ;
#79106 = CARTESIAN_POINT ( 'NONE',  ( -29.01088028653927964, -22.02621442084247505, 4.990779571109222879 ) ) ;
#79107 = ORIENTED_EDGE ( 'NONE', *, *, #35662, .T. ) ;
#79108 = VERTEX_POINT ( 'NONE', #76571 ) ;
#79109 = AXIS2_PLACEMENT_3D ( 'NONE', #67485, #66748, #23959 ) ;
#79110 = EDGE_LOOP ( 'NONE', ( #131450, #50040, #139428, #54162 ) ) ;
#79111 = AXIS2_PLACEMENT_3D ( 'NONE', #62430, #142828, #130541 ) ;
#79112 = DIRECTION ( 'NONE',  ( -0.7071067811865486830, -0.7071067811865464625, 0.000000000000000000 ) ) ;
#79113 = DIRECTION ( 'NONE',  ( -1.000000000000000000, -0.000000000000000000, -0.000000000000000000 ) ) ;
#79114 = VERTEX_POINT ( 'NONE', #53357 ) ;
#79115 = CARTESIAN_POINT ( 'NONE',  ( -6.489213562373093325, -27.52281430457059841, 5.000000000000000000 ) ) ;
#79116 = AXIS2_PLACEMENT_3D ( 'NONE', #2785, #47084, #91265 ) ;
#79117 = VECTOR ( 'NONE', #39963, 999.9999999999998863 ) ;
#79118 = CARTESIAN_POINT ( 'NONE',  ( 3.328169399223508851, 17.25929247661553489, 4.000000000000000000 ) ) ;
#79119 = DIRECTION ( 'NONE',  ( 0.7071067811865486830, -0.7071067811865464625, -0.000000000000000000 ) ) ;
#79120 = ADVANCED_FACE ( 'NONE', ( #98308 ), #97570, .T. ) ;
#79121 = FACE_BOUND ( 'NONE', #73390, .T. ) ;
#79122 = ORIENTED_EDGE ( 'NONE', *, *, #91985, .F. ) ;
#79123 = CYLINDRICAL_SURFACE ( 'NONE', #101246, 7.950000000000000178 ) ;
#79124 = DIRECTION ( 'NONE',  ( -1.000000000000000000, -1.224606353822377258E-16, -0.000000000000000000 ) ) ;
#79125 = LINE ( 'NONE', #23996, #14325 ) ;
#79126 = VERTEX_POINT ( 'NONE', #9850 ) ;
#79127 = DIRECTION ( 'NONE',  ( 1.000000000000000000, 0.000000000000000000, 0.000000000000000000 ) ) ;
#79128 = VERTEX_POINT ( 'NONE', #41059 ) ;
#79129 = VERTEX_POINT ( 'NONE', #8387 ) ;
#79130 = AXIS2_PLACEMENT_3D ( 'NONE', #28371, #5137, #29765 ) ;
#79131 = EDGE_LOOP ( 'NONE', ( #59779, #132002, #38514, #5144 ) ) ;
#79132 = EDGE_CURVE ( 'NONE', #9583, #94004, #66552, .T. ) ;
#79133 = CARTESIAN_POINT ( 'NONE',  ( 48.03709685856477307, -3.054999999999998828, -5.291415217122919401 ) ) ;
#79134 = EDGE_LOOP ( 'NONE', ( #8926, #10793, #59246, #48003 ) ) ;
#79135 = LINE ( 'NONE', #80545, #141328 ) ;
#79136 = ADVANCED_FACE ( 'NONE', ( #54119 ), #31620, .F. ) ;
#79137 = CARTESIAN_POINT ( 'NONE',  ( -33.18398860626899705, 28.73617430169810305, 5.000000000000000000 ) ) ;
#79138 = ORIENTED_EDGE ( 'NONE', *, *, #23128, .F. ) ;
#79139 = DIRECTION ( 'NONE',  ( -1.000000000000000000, 0.000000000000000000, 0.000000000000000000 ) ) ;
#79140 = VECTOR ( 'NONE', #21556, 1000.000000000000000 ) ;
#79141 = VECTOR ( 'NONE', #128355, 1000.000000000000000 ) ;
#79142 = EDGE_CURVE ( 'NONE', #97043, #62248, #10549, .T. ) ;
#79143 = AXIS2_PLACEMENT_3D ( 'NONE', #41475, #108137, #141524 ) ;
#79144 = AXIS2_PLACEMENT_3D ( 'NONE', #111326, #12010, #56298 ) ;
#79145 = EDGE_CURVE ( 'NONE', #81561, #125811, #96827, .T. ) ;
#79146 = DIRECTION ( 'NONE',  ( -0.000000000000000000, 0.3543493200069153248, 0.9351131265310292928 ) ) ;
#79147 = CARTESIAN_POINT ( 'NONE',  ( -16.41009064519821337, 9.759292476615618384, 11.28811694763775009 ) ) ;
#79148 = CARTESIAN_POINT ( 'NONE',  ( 184.1500000000000057, -3.180000000000061444, -31.92499999999998295 ) ) ;
#79149 = DIRECTION ( 'NONE',  ( -0.6830127018922181881, 0.6830127018922202975, -0.2588190451025214056 ) ) ;
#79150 = ORIENTED_EDGE ( 'NONE', *, *, #81757, .F. ) ;
#79151 = ORIENTED_EDGE ( 'NONE', *, *, #116494, .F. ) ;
#79152 = VECTOR ( 'NONE', #117820, 1000.000000000000000 ) ;
#79153 = MECHANICAL_DESIGN_GEOMETRIC_PRESENTATION_REPRESENTATION (  '', ( #21155 ), #37418 ) ;
#79154 = ORIENTED_EDGE ( 'NONE', *, *, #132332, .F. ) ;
#79155 = AXIS2_PLACEMENT_3D ( 'NONE', #32306, #11949, #56236 ) ;
#79156 = EDGE_LOOP ( 'NONE', ( #95232, #108148, #34507, #77775 ) ) ;
#79157 = CARTESIAN_POINT ( 'NONE',  ( 11.93159235450332112, -3.851859888774471706E-31, 2.500000000000001332 ) ) ;
#79158 = EDGE_LOOP ( 'NONE', ( #86906, #120013, #102426, #55133 ) ) ;
#79159 = PRESENTATION_LAYER_ASSIGNMENT (  '', '', ( #55969 ) ) ;
#79160 = ORIENTED_EDGE ( 'NONE', *, *, #2178, .T. ) ;
#79161 = CARTESIAN_POINT ( 'NONE',  ( 165.1757173328947772, 26.96999999999993847, -33.99520319345304387 ) ) ;
#79162 = EDGE_CURVE ( 'NONE', #116810, #129956, #63565, .T. ) ;
#79163 = CARTESIAN_POINT ( 'NONE',  ( -17.01299345043647548, -0.9444868035624306435, 500000.0000000000582 ) ) ;
#79164 = EDGE_LOOP ( 'NONE', ( #50889, #45130, #117800, #99921, #137794 ) ) ;
#79165 = PRESENTATION_LAYER_ASSIGNMENT (  '', '', ( #115811 ) ) ;
#79166 = DIRECTION ( 'NONE',  ( -0.6830127018922181881, 0.6830127018922202975, -0.2588190451025214056 ) ) ;
#79167 = LINE ( 'NONE', #14578, #125470 ) ;
#79168 = CARTESIAN_POINT ( 'NONE',  ( 25.73373647476855552, 5.808823158059036373, 5.808823158059032821 ) ) ;
#79169 = CARTESIAN_POINT ( 'NONE',  ( 20.51159235450331764, 9.902892378096218942E-16, 0.000000000000000000 ) ) ;
#79170 = ORIENTED_EDGE ( 'NONE', *, *, #133584, .T. ) ;
#79172 = CARTESIAN_POINT ( 'NONE',  ( -11.99999999999991296, 5.966399257802200040, 5.000000000000000000 ) ) ;
#79171 = CARTESIAN_POINT ( 'NONE',  ( 106.5162635252314658, -4.472830434245839371, 4.472830434245839371 ) ) ;
#79173 = CARTESIAN_POINT ( 'NONE',  ( -34.92500000000001137, 22.22500000000000142, 4.000000000000000000 ) ) ;
#79174 = CARTESIAN_POINT ( 'NONE',  ( 12.41161490594822503, 22.22500000000000142, 4.777194822843815913 ) ) ;
#79175 = VERTEX_POINT ( 'NONE', #74423 ) ;
#79176 = CARTESIAN_POINT ( 'NONE',  ( 8.293876922607989144, 22.22500000000000142, 4.000000000000000000 ) ) ;
#79178 = ORIENTED_EDGE ( 'NONE', *, *, #16812, .F. ) ;
#79177 = DIRECTION ( 'NONE',  ( 0.7071067811865487940, 0.7071067811865463515, 0.000000000000000000 ) ) ;
#79179 = DIRECTION ( 'NONE',  ( -0.7071067811865486830, -0.7071067811865464625, 0.000000000000000000 ) ) ;
#79180 = VERTEX_POINT ( 'NONE', #98992 ) ;
#79181 =( LENGTH_UNIT ( ) NAMED_UNIT ( * ) SI_UNIT ( .MILLI., .METRE. ) );
#79182 = PLANE ( 'NONE',  #109415 ) ;
#79183 = CARTESIAN_POINT ( 'NONE',  ( 121.7500000000000000, -9.735942053221458872E-16, 7.950000000000000178 ) ) ;
#79184 = ORIENTED_EDGE ( 'NONE', *, *, #28784, .T. ) ;
#79185 = AXIS2_PLACEMENT_3D ( 'NONE', #66455, #44738, #54176 ) ;
#79186 = DIRECTION ( 'NONE',  ( 1.000000000000000000, 0.000000000000000000, 0.000000000000000000 ) ) ;
#79187 = VECTOR ( 'NONE', #54660, 1000.000000000000227 ) ;
#79188 = LINE ( 'NONE', #24058, #132121 ) ;
#79189 = CARTESIAN_POINT ( 'NONE',  ( -12.18398860626900060, 28.73617430169795739, 5.000000000000000000 ) ) ;
#79190 = ORIENTED_EDGE ( 'NONE', *, *, #45463, .T. ) ;
#79191 = VECTOR ( 'NONE', #115696, 1000.000000000000000 ) ;
#79193 = EDGE_CURVE ( 'NONE', #95370, #92431, #132392, .T. ) ;
#79192 = DIRECTION ( 'NONE',  ( -0.7071067811865486830, -0.7071067811865464625, 0.000000000000000000 ) ) ;
#79194 = ORIENTED_EDGE ( 'NONE', *, *, #48167, .F. ) ;
#79195 = DIRECTION ( 'NONE',  ( 0.7071067811865487940, 0.7071067811865463515, 0.000000000000000000 ) ) ;
#79197 = ORIENTED_EDGE ( 'NONE', *, *, #109440, .F. ) ;
#79196 = DIRECTION ( 'NONE',  ( 0.000000000000000000, 0.000000000000000000, -1.000000000000000000 ) ) ;
#79199 = ADVANCED_FACE ( 'NONE', ( #122167 ), #112736, .F. ) ;
#79198 = EDGE_CURVE ( 'NONE', #99716, #88687, #81401, .T. ) ;
#79200 = ORIENTED_EDGE ( 'NONE', *, *, #41852, .F. ) ;
#79201 = LINE ( 'NONE', #35697, #135263 ) ;
#79202 = LINE ( 'NONE', #24069, #25106 ) ;
#79203 = VECTOR ( 'NONE', #124917, 1000.000000000000000 ) ;
#79204 = ORIENTED_EDGE ( 'NONE', *, *, #121863, .T. ) ;
#79205 = CARTESIAN_POINT ( 'NONE',  ( 30.18398860626900060, 28.73617430169808173, 5.000000000000000000 ) ) ;
#79206 = EDGE_CURVE ( 'NONE', #47599, #50105, #89555, .T. ) ;
#79207 = EDGE_CURVE ( 'NONE', #63837, #29858, #63396, .T. ) ;
#79208 = CARTESIAN_POINT ( 'NONE',  ( 39.18398860626899705, 28.73617430169814568, 5.000000000000000000 ) ) ;
#79209 = FACE_OUTER_BOUND ( 'NONE', #51498, .T. ) ;
#79210 = EDGE_CURVE ( 'NONE', #40163, #79781, #56966, .T. ) ;
#79211 = ORIENTED_EDGE ( 'NONE', *, *, #112253, .F. ) ;
#79212 = FACE_OUTER_BOUND ( 'NONE', #26929, .T. ) ;
#79213 = EDGE_CURVE ( 'NONE', #124237, #97431, #77987, .T. ) ;
#79214 = FACE_OUTER_BOUND ( 'NONE', #40104, .T. ) ;
#79215 = AXIS2_PLACEMENT_3D ( 'NONE', #65892, #110051, #142011 ) ;
#79216 = DIRECTION ( 'NONE',  ( 0.3543493200069162685, -0.000000000000000000, -0.9351131265310288487 ) ) ;
#79217 = DIRECTION ( 'NONE',  ( -0.7071067811865486830, -0.7071067811865464625, -0.000000000000000000 ) ) ;
#79218 = AXIS2_PLACEMENT_3D ( 'NONE', #133924, #24440, #10678 ) ;
#79219 = FACE_OUTER_BOUND ( 'NONE', #56969, .T. ) ;
#79220 = ADVANCED_FACE ( 'NONE', ( #80847 ), #88872, .T. ) ;
#79221 = CARTESIAN_POINT ( 'NONE',  ( -24.48921356237309510, -27.52281430457072631, 5.000000000000000000 ) ) ;
#79222 = EDGE_LOOP ( 'NONE', ( #55074, #25810, #39620, #69034 ) ) ;
#79223 = ORIENTED_EDGE ( 'NONE', *, *, #27965, .F. ) ;
#79224 = VERTEX_POINT ( 'NONE', #35211 ) ;
#79226 = EDGE_CURVE ( 'NONE', #116321, #71945, #1784, .T. ) ;
#79225 =( LENGTH_UNIT ( ) NAMED_UNIT ( * ) SI_UNIT ( .MILLI., .METRE. ) );
#79227 = ORIENTED_EDGE ( 'NONE', *, *, #87884, .T. ) ;
#79228 = ORIENTED_EDGE ( 'NONE', *, *, #132332, .T. ) ;
#79229 = EDGE_LOOP ( 'NONE', ( #83753, #24270, #105655, #56917 ) ) ;
#79230 = CONICAL_SURFACE ( 'NONE', #97697, 2.500000000000000888, 0.9599310885968822538 ) ;
#79231 = CARTESIAN_POINT ( 'NONE',  ( 1.325532373446378864, -3.000483569180001808, -6.075707327269213032 ) ) ;
#79232 = DIRECTION ( 'NONE',  ( -0.000000000000000000, 0.000000000000000000, 1.000000000000000000 ) ) ;
#79233 = ORIENTED_EDGE ( 'NONE', *, *, #29927, .F. ) ;
#79234 = CARTESIAN_POINT ( 'NONE',  ( -17.99999999999987566, 19.93112307739198386, 4.000000000000000000 ) ) ;
#79235 = CARTESIAN_POINT ( 'NONE',  ( 25.40000000000000213, 6.316876854325914614, 3.503673674027464546 ) ) ;
#79236 = EDGE_CURVE ( 'NONE', #68198, #14802, #90262, .T. ) ;
#79237 = DIRECTION ( 'NONE',  ( 0.3543493200069162685, -0.000000000000000000, -0.9351131265310288487 ) ) ;
#79238 = PLANE ( 'NONE',  #32536 ) ;
#79239 = CARTESIAN_POINT ( 'NONE',  ( 123.6670968585647756, -3.055000000000000160, -5.291415217122921177 ) ) ;
#79240 = ORIENTED_EDGE ( 'NONE', *, *, #77418, .T. ) ;
#79241 = DIRECTION ( 'NONE',  ( 1.055184596092948005E-16, -1.000000000000000000, 0.000000000000000000 ) ) ;
#79242 = DIRECTION ( 'NONE',  ( 0.000000000000000000, 0.000000000000000000, 1.000000000000000000 ) ) ;
#79244 = CONICAL_SURFACE ( 'NONE', #53764, 2.500000000000000888, 0.9599310885968822538 ) ;
#79243 = CARTESIAN_POINT ( 'NONE',  ( 6.183988606268994381, 28.73617430169791476, 5.000000000000000000 ) ) ;
#79245 = CARTESIAN_POINT ( 'NONE',  ( 1.219720151767342609, 2.263774094906783052, 6.495225715523759824 ) ) ;
#79246 = PRESENTATION_STYLE_ASSIGNMENT (( #70516 ) ) ;
#79247 = EDGE_CURVE ( 'NONE', #122313, #13983, #35566, .T. ) ;
#79248 = CARTESIAN_POINT ( 'NONE',  ( -17.67183060077634593, -21.74070752338406010, 4.000000000000000000 ) ) ;
#79249 = DIRECTION ( 'NONE',  ( -0.000000000000000000, 0.3543493200069153248, 0.9351131265310292928 ) ) ;
#79250 = CARTESIAN_POINT ( 'NONE',  ( 50.24586038379622011, 3.974999999999996980, 6.884901960086287964 ) ) ;
#79251 = CARTESIAN_POINT ( 'NONE',  ( -30.48921356237309510, -27.52281430457076894, 5.000000000000000000 ) ) ;
#79252 = LINE ( 'NONE', #87931, #11323 ) ;
#79253 = VERTEX_POINT ( 'NONE', #35926 ) ;
#79254 = ORIENTED_EDGE ( 'NONE', *, *, #70983, .F. ) ;
#79255 = CARTESIAN_POINT ( 'NONE',  ( 47.95833333333332860, 3.974999999999997424, 6.884901960086288852 ) ) ;
#79256 = DIRECTION ( 'NONE',  ( -0.000000000000000000, 0.000000000000000000, 1.000000000000000000 ) ) ;
#79257 = VERTEX_POINT ( 'NONE', #22836 ) ;
#79258 = VECTOR ( 'NONE', #87185, 1000.000000000000000 ) ;
#79259 = VECTOR ( 'NONE', #123578, 1000.000000000000000 ) ;
#79260 = VECTOR ( 'NONE', #41245, 1000.000000000000000 ) ;
#79261 = CARTESIAN_POINT ( 'NONE',  ( -0.4282563736389425890, -1.252432624735495326, 3.977822609706378909 ) ) ;
#79262 =( BOUNDED_CURVE ( )  B_SPLINE_CURVE ( 3, ( #139351, #30567, #105941, #63224 ),
 .UNSPECIFIED., .F., .F. ) 
 B_SPLINE_CURVE_WITH_KNOTS ( ( 4, 4 ),
 ( 5.143245962375972091, 6.645403452391247079 ),
 .UNSPECIFIED. ) 
 CURVE ( )  GEOMETRIC_REPRESENTATION_ITEM ( )  RATIONAL_B_SPLINE_CURVE ( ( 1.000000000000000000, 0.8206354192515254997, 0.8206354192515254997, 1.000000000000000000 ) ) 
 REPRESENTATION_ITEM ( '' )  );
#79263 = LINE ( 'NONE', #89375, #139484 ) ;
#79264 = VECTOR ( 'NONE', #107800, 1000.000000000000000 ) ;
#79265 = CIRCLE ( 'NONE', #69947, 2.000000000000001776 ) ;
#79266 = CARTESIAN_POINT ( 'NONE',  ( 34.27126352523143993, 4.472830434245839371, 4.472830434245842035 ) ) ;
#79267 = ORIENTED_EDGE ( 'NONE', *, *, #124702, .F. ) ;
#79268 = ADVANCED_FACE ( 'NONE', ( #134510 ), #56272, .F. ) ;
#79269 = DIRECTION ( 'NONE',  ( -0.7071067811865486830, -0.7071067811865464625, 0.000000000000000000 ) ) ;
#79270 = EDGE_LOOP ( 'NONE', ( #126607, #67283, #93189 ) ) ;
#79271 = VECTOR ( 'NONE', #22816, 1000.000000000000000 ) ;
#79272 = AXIS2_PLACEMENT_3D ( 'NONE', #92921, #26250, #2306 ) ;
#79273 = LINE ( 'NONE', #123474, #118975 ) ;
#79274 = CARTESIAN_POINT ( 'NONE',  ( 18.10180811604841011, 9.068207373850700748, 5.000000000000000000 ) ) ;
#79276 = EDGE_CURVE ( 'NONE', #20488, #48699, #91016, .T. ) ;
#79275 = SURFACE_STYLE_USAGE ( .BOTH. , #88691 ) ;
#79277 = DIRECTION ( 'NONE',  ( -0.6830127018922180770, -0.6830127018922204085, -0.2588190451025213501 ) ) ;
#79278 = ORIENTED_EDGE ( 'NONE', *, *, #130605, .F. ) ;
#79279 = CARTESIAN_POINT ( 'NONE',  ( -24.65671000166197757, 3.759292476615681888, 13.27625715073259904 ) ) ;
#79280 = ORIENTED_EDGE ( 'NONE', *, *, #76782, .T. ) ;
#79281 = DIRECTION ( 'NONE',  ( 0.5735764363510448272, -0.8191520442889927978, 1.003171929053526103E-16 ) ) ;
#79282 = LINE ( 'NONE', #34299, #92480 ) ;
#79283 = CARTESIAN_POINT ( 'NONE',  ( 0.000000000000000000, 9.735942053221458872E-16, -7.950000000000000178 ) ) ;
#79284 = DIRECTION ( 'NONE',  ( -0.7071067811865487940, 0.7071067811865463515, -0.000000000000000000 ) ) ;
#79285 = EDGE_CURVE ( 'NONE', #36518, #1673, #726, .T. ) ;
#79286 = EDGE_LOOP ( 'NONE', ( #88643, #108254, #73247, #113562 ) ) ;
#79287 = DIRECTION ( 'NONE',  ( 0.7071067811865486830, -0.7071067811865464625, -0.000000000000000000 ) ) ;
#79288 = CARTESIAN_POINT ( 'NONE',  ( 55.62043019189812298, 3.055000000000001936, -5.291415217122916737 ) ) ;
#79289 = CARTESIAN_POINT ( 'NONE',  ( -54.18398860626899705, 28.73617430169825226, 5.000000000000000000 ) ) ;
#79290 = ADVANCED_FACE ( 'NONE', ( #24997 ), #121185, .T. ) ;
#79291 = PLANE ( 'NONE',  #80212 ) ;
#79293 = ORIENTED_EDGE ( 'NONE', *, *, #99351, .T. ) ;
#79292 = DIRECTION ( 'NONE',  ( -0.7071067811865487940, 0.7071067811865463515, 0.000000000000000000 ) ) ;
#79294 = ORIENTED_EDGE ( 'NONE', *, *, #8699, .F. ) ;
#79295 = DIRECTION ( 'NONE',  ( -0.3543493200069162685, -0.000000000000000000, -0.9351131265310288487 ) ) ;
#79296 = ORIENTED_EDGE ( 'NONE', *, *, #122470, .F. ) ;
#79297 = VECTOR ( 'NONE', #107617, 999.9999999999998863 ) ;
#79298 = VECTOR ( 'NONE', #78543, 1000.000000000000000 ) ;
#79299 = CARTESIAN_POINT ( 'NONE',  ( 33.40690130215642029, 22.26999999999999957, -13.94180635367735555 ) ) ;
#79300 = ORIENTED_EDGE ( 'NONE', *, *, #97260, .F. ) ;
#79301 = VECTOR ( 'NONE', #87514, 1000.000000000000000 ) ;
#79302 = CARTESIAN_POINT ( 'NONE',  ( 0.000000000000000000, 0.000000000000000000, 5.000000000000000000 ) ) ;
#79303 = DIRECTION ( 'NONE',  ( -0.7071067811865487940, 0.7071067811865463515, 0.000000000000000000 ) ) ;
#79304 = LINE ( 'NONE', #74453, #124952 ) ;
#79305 = VECTOR ( 'NONE', #10191, 999.9999999999998863 ) ;
#79306 = DIRECTION ( 'NONE',  ( 0.6830127018922181881, 0.6830127018922202975, -0.2588190451025214056 ) ) ;
#79307 = EDGE_CURVE ( 'NONE', #967, #92118, #25724, .T. ) ;
#79308 = FACE_BOUND ( 'NONE', #63219, .T. ) ;
#79309 = CARTESIAN_POINT ( 'NONE',  ( 44.99451991528749772, 28.92564299267969474, 4.000000000000000000 ) ) ;
#79310 = EDGE_CURVE ( 'NONE', #46586, #305, #23585, .T. ) ;
#79311 = CARTESIAN_POINT ( 'NONE',  ( 9.489213562373095101, -27.52281430457062328, 5.000000000000000000 ) ) ;
#79312 = DIRECTION ( 'NONE',  ( 0.6830127018922181881, 0.6830127018922202975, -0.2588190451025214056 ) ) ;
#79314 = VERTEX_POINT ( 'NONE', #124327 ) ;
#79313 = DIRECTION ( 'NONE',  ( 0.000000000000000000, 0.000000000000000000, -1.000000000000000000 ) ) ;
#79315 = CARTESIAN_POINT ( 'NONE',  ( 8.423184310185783730, 3.061616997868383634E-16, -2.500000000000000444 ) ) ;
#79316 = ORIENTED_EDGE ( 'NONE', *, *, #42410, .T. ) ;
#79317 = EDGE_LOOP ( 'NONE', ( #68830, #52312, #4455, #7160 ) ) ;
#79318 = CARTESIAN_POINT ( 'NONE',  ( 77.93293019189812298, 1.637169565754156508, 6.110000000000000320 ) ) ;
#79319 = ORIENTED_EDGE ( 'NONE', *, *, #136579, .T. ) ;
#79320 = CARTESIAN_POINT ( 'NONE',  ( -39.48921356237310221, -27.52281430457082934, 5.000000000000000000 ) ) ;
#79321 = EDGE_CURVE ( 'NONE', #14462, #11390, #33780, .T. ) ;
#79322 = AXIS2_PLACEMENT_3D ( 'NONE', #41612, #53954, #76407 ) ;
#79323 = ORIENTED_EDGE ( 'NONE', *, *, #26345, .T. ) ;
#79324 = LINE ( 'NONE', #247, #111543 ) ;
#79325 = VECTOR ( 'NONE', #5355, 1000.000000000000000 ) ;
#79326 = EDGE_CURVE ( 'NONE', #101708, #56732, #45381, .T. ) ;
#79327 = CARTESIAN_POINT ( 'NONE',  ( 123.3541666666666856, -2.130196079827445299, -7.949999999999990408 ) ) ;
#79328 = EDGE_CURVE ( 'NONE', #99670, #6450, #126453, .T. ) ;
#79329 = CARTESIAN_POINT ( 'NONE',  ( -11.99451991528749417, 28.92564299267946382, 4.000000000000000000 ) ) ;
#79330 = CARTESIAN_POINT ( 'NONE',  ( 42.29974487139158157, -27.71228299555235708, 4.000000000000000000 ) ) ;
#79331 = LINE ( 'NONE', #68442, #45844 ) ;
#79332 = DIRECTION ( 'NONE',  ( -0.6830127018922181881, 0.6830127018922202975, -0.2588190451025214056 ) ) ;
#79333 = LINE ( 'NONE', #15409, #36990 ) ;
#79334 = ORIENTED_EDGE ( 'NONE', *, *, #104878, .F. ) ;
#79335 = VECTOR ( 'NONE', #115292, 1000.000000000000000 ) ;
#79336 = VECTOR ( 'NONE', #17352, 1000.000000000000000 ) ;
#79337 = ORIENTED_EDGE ( 'NONE', *, *, #55483, .T. ) ;
#79338 = CARTESIAN_POINT ( 'NONE',  ( 1.828169399223519953, 0.7592924766157069794, 4.000000000000000000 ) ) ;
#79339 = CARTESIAN_POINT ( 'NONE',  ( -29.67183060077625711, -12.74070752338414891, 4.000000000000000000 ) ) ;
#79340 = ORIENTED_EDGE ( 'NONE', *, *, #9108, .F. ) ;
#79341 = VERTEX_POINT ( 'NONE', #51063 ) ;
#79342 = ORIENTED_EDGE ( 'NONE', *, *, #34544, .F. ) ;
#79343 = EDGE_CURVE ( 'NONE', #77443, #91920, #38751, .T. ) ;
#79344 = CARTESIAN_POINT ( 'NONE',  ( 39.18398860626899705, 28.73617430169814568, 5.000000000000000000 ) ) ;
#79345 = AXIS2_PLACEMENT_3D ( 'NONE', #35738, #82092, #24809 ) ;
#79346 = VERTEX_POINT ( 'NONE', #16240 ) ;
#79347 = DIRECTION ( 'NONE',  ( 0.7071067811865487940, 0.7071067811865463515, 0.000000000000000000 ) ) ;
#79348 = CARTESIAN_POINT ( 'NONE',  ( 42.80836038379622011, 7.949999999999996625, 2.130196079827431088 ) ) ;
#79349 = CARTESIAN_POINT ( 'NONE',  ( 0.6504031414352192675, 7.934999999999989839, -2.126176841940961904 ) ) ;
#79350 = CARTESIAN_POINT ( 'NONE',  ( 0.000000000000000000, 9.631307414974321190, -9.079085613539540134 ) ) ;
#79351 = VERTEX_POINT ( 'NONE', #40214 ) ;
#79352 = CARTESIAN_POINT ( 'NONE',  ( 0.000000000000000000, 0.000000000000000000, 5.000000000000000000 ) ) ;
#79353 = DIRECTION ( 'NONE',  ( -0.000000000000000000, 0.3543493200069153248, 0.9351131265310292928 ) ) ;
#79354 = PLANE ( 'NONE',  #40567 ) ;
#79355 = VECTOR ( 'NONE', #66522, 999.9999999999998863 ) ;
#79356 = VECTOR ( 'NONE', #105345, 1000.000000000000000 ) ;
#79358 = ORIENTED_EDGE ( 'NONE', *, *, #71746, .F. ) ;
#79357 = DIRECTION ( 'NONE',  ( 0.3543493200069162685, -0.000000000000000000, -0.9351131265310288487 ) ) ;
#79359 = AXIS2_PLACEMENT_3D ( 'NONE', #24494, #68748, #112932 ) ;
#79360 = ORIENTED_EDGE ( 'NONE', *, *, #70278, .F. ) ;
#79361 = LINE ( 'NONE', #22743, #72796 ) ;
#79362 = DIRECTION ( 'NONE',  ( -1.000000000000000000, -1.224606353822377258E-16, -0.000000000000000000 ) ) ;
#79363 = VECTOR ( 'NONE', #48270, 999.9999999999998863 ) ;
#79364 = LINE ( 'NONE', #24918, #79506 ) ;
#79366 = VERTEX_POINT ( 'NONE', #138795 ) ;
#79365 = VECTOR ( 'NONE', #21682, 999.9999999999998863 ) ;
#79367 = CARTESIAN_POINT ( 'NONE',  ( 25.49999999999982947, 1.030536316426536203, -5.498701923753857024 ) ) ;
#79368 = CARTESIAN_POINT ( 'NONE',  ( 1.353980332882009252, -0.4000000000000004108, 2.467792535850613866 ) ) ;
#79369 = CYLINDRICAL_SURFACE ( 'NONE', #18544, 6.094999999999989093 ) ;
#79370 = PLANE ( 'NONE',  #116522 ) ;
#79371 = VECTOR ( 'NONE', #142346, 1000.000000000000227 ) ;
#79372 = VECTOR ( 'NONE', #125929, 1000.000000000000000 ) ;
#79373 = DIRECTION ( 'NONE',  ( -1.000000000000000000, -0.000000000000000000, -0.000000000000000000 ) ) ;
#79374 = CARTESIAN_POINT ( 'NONE',  ( 17.70025512860841488, -27.71228299555193786, 4.000000000000000000 ) ) ;
#79375 = DIRECTION ( 'NONE',  ( -0.7071067811865487940, 0.7071067811865463515, 0.000000000000000000 ) ) ;
#79376 = LINE ( 'NONE', #81498, #3371 ) ;
#79377 = LINE ( 'NONE', #22756, #36746 ) ;
#79378 = VERTEX_POINT ( 'NONE', #50349 ) ;
#79379 = EDGE_LOOP ( 'NONE', ( #82578, #36464, #75505, #129323 ) ) ;
#79380 = CARTESIAN_POINT ( 'NONE',  ( 34.82816939922329880, 21.75929247661549581, 4.000000000000000000 ) ) ;
#79381 = LINE ( 'NONE', #58352, #37782 ) ;
#79382 =( NAMED_UNIT ( * ) PLANE_ANGLE_UNIT ( ) SI_UNIT ( $, .RADIAN. ) );
#79383 = DIRECTION ( 'NONE',  ( -0.000000000000000000, 0.3543493200069153248, 0.9351131265310292928 ) ) ;
#79384 = ADVANCED_FACE ( 'NONE', ( #48201 ), #29290, .F. ) ;
#79385 = ORIENTED_EDGE ( 'NONE', *, *, #47539, .T. ) ;
#79386 = CIRCLE ( 'NONE', #42314, 1.000000000000000888 ) ;
#79387 = CARTESIAN_POINT ( 'NONE',  ( -3.498163485139541784, -17.24070752338410628, 8.407044977365233152 ) ) ;
#79388 = DIRECTION ( 'NONE',  ( -0.7071067811865486830, -0.7071067811865464625, -0.000000000000000000 ) ) ;
#79389 = LINE ( 'NONE', #98927, #28297 ) ;
#79390 = ADVANCED_FACE ( 'NONE', ( #104712 ), #28605, .F. ) ;
#79391 = EDGE_CURVE ( 'NONE', #482, #75148, #105414, .T. ) ;
#79392 = ORIENTED_EDGE ( 'NONE', *, *, #86165, .F. ) ;
#79393 = CARTESIAN_POINT ( 'NONE',  ( -20.99451991528748707, 28.92564299267952777, 4.000000000000000000 ) ) ;
#79394 = EDGE_CURVE ( 'NONE', #15499, #21301, #48930, .T. ) ;
#79395 = DIRECTION ( 'NONE',  ( 0.000000000000000000, -1.000000000000000000, 0.000000000000000000 ) ) ;
#79396 = DIRECTION ( 'NONE',  ( 0.000000000000000000, -1.000000000000000000, 0.000000000000000000 ) ) ;
#79397 = EDGE_CURVE ( 'NONE', #104700, #122337, #73532, .T. ) ;
#79398 = CARTESIAN_POINT ( 'NONE',  ( 55.62043019189812298, 3.055000000000002380, -5.291415217122917625 ) ) ;
#79399 = AXIS2_PLACEMENT_3D ( 'NONE', #142073, #110810, #44180 ) ;
#79400 = DIRECTION ( 'NONE',  ( -0.7071067811865486830, 0.7071067811865464625, 0.000000000000000000 ) ) ;
#79401 = DIRECTION ( 'NONE',  ( 0.000000000000000000, -1.137193330093851115E-16, 1.000000000000000000 ) ) ;
#79402 = DIRECTION ( 'NONE',  ( 0.6830127018922180770, -0.6830127018922204085, -0.2588190451025213501 ) ) ;
#79403 = AXIS2_PLACEMENT_3D ( 'NONE', #87350, #131566, #32254 ) ;
#79404 = ORIENTED_EDGE ( 'NONE', *, *, #110303, .T. ) ;
#79405 = EDGE_CURVE ( 'NONE', #79734, #21635, #139815, .T. ) ;
#79406 = SURFACE_SIDE_STYLE ('',( #99658 ) ) ;
#79407 = ORIENTED_EDGE ( 'NONE', *, *, #136268, .T. ) ;
#79408 = MECHANICAL_DESIGN_GEOMETRIC_PRESENTATION_REPRESENTATION (  '', ( #19123 ), #26070 ) ;
#79409 = CARTESIAN_POINT ( 'NONE',  ( -35.99451991528749772, 28.92564299267963079, 4.000000000000000000 ) ) ;
#79410 = MECHANICAL_DESIGN_GEOMETRIC_PRESENTATION_REPRESENTATION (  '', ( #93215 ), #111749 ) ;
#79411 = LINE ( 'NONE', #48881, #141029 ) ;
#79412 = CARTESIAN_POINT ( 'NONE',  ( 14.70025512860841133, -27.71228299555195917, 4.000000000000000000 ) ) ;
#79413 = EDGE_CURVE ( 'NONE', #26486, #23088, #39482, .T. ) ;
#79414 = FACE_OUTER_BOUND ( 'NONE', #38681, .T. ) ;
#79415 = EDGE_CURVE ( 'NONE', #136372, #23774, #138067, .T. ) ;
#79416 = LINE ( 'NONE', #33042, #115782 ) ;
#79417 = DIRECTION ( 'NONE',  ( 0.3543493200069162685, -0.000000000000000000, -0.9351131265310288487 ) ) ;
#79418 = ORIENTED_EDGE ( 'NONE', *, *, #70196, .F. ) ;
#79419 = ORIENTED_EDGE ( 'NONE', *, *, #86028, .T. ) ;
#79420 = CARTESIAN_POINT ( 'NONE',  ( 81.18398860626899705, 28.73617430169844056, 5.000000000000000000 ) ) ;
#79421 = UNCERTAINTY_MEASURE_WITH_UNIT (LENGTH_MEASURE( 1.000000000000000082E-05 ), #126590, 'distance_accuracy_value', 'NONE');
#79422 = CARTESIAN_POINT ( 'NONE',  ( -13.63753812416088707, 22.22500000000000142, 4.000000000000000000 ) ) ;
#79423 = EDGE_CURVE ( 'NONE', #46517, #75731, #128153, .T. ) ;
#79424 = CARTESIAN_POINT ( 'NONE',  ( 117.3750000000000000, 7.950000000000000178, 1.460391307983218535E-15 ) ) ;
#79425 = CARTESIAN_POINT ( 'NONE',  ( 74.89169371712957002, 2.130196079827421762, 7.950000000000001066 ) ) ;
#79426 = CARTESIAN_POINT ( 'NONE',  ( 14.39532882439692862, -2.055000000000000160, 2.789133085058097101E-16 ) ) ;
#79427 = LINE ( 'NONE', #123625, #129330 ) ;
#79428 = ORIENTED_EDGE ( 'NONE', *, *, #5463, .T. ) ;
#79429 =( BOUNDED_CURVE ( )  B_SPLINE_CURVE ( 3, ( #13105, #87125, #65403, #55214 ),
 .UNSPECIFIED., .F., .T. ) 
 B_SPLINE_CURVE_WITH_KNOTS ( ( 4, 4 ),
 ( 2.779374508378133601, 4.199602562396783867 ),
 .UNSPECIFIED. ) 
 CURVE ( )  GEOMETRIC_REPRESENTATION_ITEM ( )  RATIONAL_B_SPLINE_CURVE ( ( 1.000000000000000000, 0.8388583629366745953, 0.8388583629366745953, 1.000000000000000000 ) ) 
 REPRESENTATION_ITEM ( '' )  );
#79430 = CARTESIAN_POINT ( 'NONE',  ( 71.00000000000000000, 0.000000000000000000, -7.950000000000000178 ) ) ;
#79431 = CARTESIAN_POINT ( 'NONE',  ( 11.81601139373100651, 28.73617430169779041, 5.000000000000000000 ) ) ;
#79432 = CARTESIAN_POINT ( 'NONE',  ( 29.99451991528749417, 28.92564299267958816, 4.000000000000000000 ) ) ;
#79434 = VECTOR ( 'NONE', #124376, 999.9999999999998863 ) ;
#79433 = CARTESIAN_POINT ( 'NONE',  ( 48.18398860626899705, 28.73617430169820608, 5.000000000000000000 ) ) ;
#79435 = EDGE_CURVE ( 'NONE', #66820, #5794, #17681, .T. ) ;
#79436 = AXIS2_PLACEMENT_3D ( 'NONE', #143204, #43905, #12673 ) ;
#79437 = ORIENTED_EDGE ( 'NONE', *, *, #1687, .T. ) ;
#79438 = PLANE ( 'NONE',  #116262 ) ;
#79439 = LINE ( 'NONE', #24981, #99892 ) ;
#79440 = CARTESIAN_POINT ( 'NONE',  ( 64.45876352523144703, 0.000000000000000000, -6.110000000000001208 ) ) ;
#79441 = EDGE_CURVE ( 'NONE', #45804, #47923, #107321, .T. ) ;
#79442 = ORIENTED_EDGE ( 'NONE', *, *, #73155, .T. ) ;
#79443 = ORIENTED_EDGE ( 'NONE', *, *, #100384, .T. ) ;
#79444 = CONICAL_SURFACE ( 'NONE', #56260, 2.055000000000001048, 0.9599310885968758145 ) ;
#79445 = CARTESIAN_POINT ( 'NONE',  ( 38.99451991528749062, 28.92564299267965211, 4.000000000000000000 ) ) ;
#79446 = SURFACE_STYLE_FILL_AREA ( #135230 ) ;
#79447 = CARTESIAN_POINT ( 'NONE',  ( -42.48921356237308800, -27.52281430457085065, 5.000000000000000000 ) ) ;
#79448 = LINE ( 'NONE', #24299, #25636 ) ;
#79450 = VERTEX_POINT ( 'NONE', #106110 ) ;
#79449 = CARTESIAN_POINT ( 'NONE',  ( 86.16666666666667140, 6.884901960086285300, 3.975000000000003642 ) ) ;
#79451 = DIRECTION ( 'NONE',  ( -0.6830127018922180770, -0.6830127018922204085, -0.2588190451025213501 ) ) ;
#79452 = CARTESIAN_POINT ( 'NONE',  ( 0.000000000000000000, 0.000000000000000000, 5.000000000000000000 ) ) ;
#79453 = AXIS2_PLACEMENT_3D ( 'NONE', #76002, #141242, #120175 ) ;
#79454 = DIRECTION ( 'NONE',  ( -1.000000000000000000, -1.224606353822377258E-16, -0.000000000000000000 ) ) ;
#79455 =( NAMED_UNIT ( * ) SI_UNIT ( $, .STERADIAN. ) SOLID_ANGLE_UNIT ( ) );
#79456 = ORIENTED_EDGE ( 'NONE', *, *, #29215, .T. ) ;
#79457 = EDGE_CURVE ( 'NONE', #35917, #68848, #17001, .T. ) ;
#79458 = ORIENTED_EDGE ( 'NONE', *, *, #91433, .T. ) ;
#79459 = CARTESIAN_POINT ( 'NONE',  ( 54.10459685856476852, 1.637169565754164946, -6.109999999999999432 ) ) ;
#79460 = EDGE_LOOP ( 'NONE', ( #79706, #15344, #79760, #89195 ) ) ;
#79461 = LINE ( 'NONE', #24314, #121634 ) ;
#79462 = CARTESIAN_POINT ( 'NONE',  ( 20.99999999999986144, 14.96639925780210767, 5.000000000000000000 ) ) ;
#79463 = LINE ( 'NONE', #133110, #78058 ) ;
#79464 = ADVANCED_FACE ( 'NONE', ( #26450 ), #139531, .F. ) ;
#79465 = CARTESIAN_POINT ( 'NONE',  ( 15.77004279457781877, 21.73644205237997085, 5.000000000000000888 ) ) ;
#79466 = CARTESIAN_POINT ( 'NONE',  ( -25.39999999999996305, 0.000000000000000000, 2.500000000000000000 ) ) ;
#79467 = ORIENTED_EDGE ( 'NONE', *, *, #3500, .F. ) ;
#79468 = ORIENTED_EDGE ( 'NONE', *, *, #115211, .T. ) ;
#79469 = AXIS2_PLACEMENT_3D ( 'NONE', #65280, #88451, #55097 ) ;
#79470 = CARTESIAN_POINT ( 'NONE',  ( -32.29289321881322650, -12.74070752338415602, 5.000000000000000000 ) ) ;
#79471 = FILL_AREA_STYLE_COLOUR ( '', #28209 ) ;
#79472 = AXIS2_PLACEMENT_3D ( 'NONE', #9569, #117608, #95887 ) ;
#79473 = VECTOR ( 'NONE', #116898, 1000.000000000000000 ) ;
#79474 = EDGE_LOOP ( 'NONE', ( #48138, #84498, #19173, #88737 ) ) ;
#79475 = EDGE_CURVE ( 'NONE', #132213, #80270, #84421, .T. ) ;
#79476 = CARTESIAN_POINT ( 'NONE',  ( 9.489213562373095101, -27.52281430457062328, 5.000000000000000000 ) ) ;
#79478 = LINE ( 'NONE', #135260, #27081 ) ;
#79477 = VECTOR ( 'NONE', #84669, 1000.000000000000000 ) ;
#79479 = DIRECTION ( 'NONE',  ( -0.7071067811865486830, -0.7071067811865464625, 0.000000000000000000 ) ) ;
#79480 = COLOUR_RGB ( '', 0.08235294, 0.09019608, 0.10196078) ;
#79481 = VERTEX_POINT ( 'NONE', #53941 ) ;
#79482 = EDGE_CURVE ( 'NONE', #66625, #9950, #79967, .T. ) ;
#79483 = FACE_BOUND ( 'NONE', #12456, .T. ) ;
#79484 = LINE ( 'NONE', #102627, #124338 ) ;
#79485 = PLANE ( 'NONE',  #113777 ) ;
#79486 = CARTESIAN_POINT ( 'NONE',  ( -18.79289321881332597, -8.240707523384195099, 5.000000000000000000 ) ) ;
#79487 = FACE_OUTER_BOUND ( 'NONE', #76112, .T. ) ;
#79488 = CARTESIAN_POINT ( 'NONE',  ( -71.99451991528749772, 28.92564299267988304, 4.000000000000000000 ) ) ;
#79489 = CARTESIAN_POINT ( 'NONE',  ( 74.86850992298120389, -0.08000000000007086165, -4.716018956497420643E-13 ) ) ;
#79490 = ORIENTED_EDGE ( 'NONE', *, *, #47306, .F. ) ;
#79491 = AXIS2_PLACEMENT_3D ( 'NONE', #5856, #38523, #135010 ) ;
#79492 = VERTEX_POINT ( 'NONE', #130051 ) ;
#79493 = CARTESIAN_POINT ( 'NONE',  ( 102.1412635252314374, 4.472830434245835818, 4.472830434245840259 ) ) ;
#79494 = ORIENTED_EDGE ( 'NONE', *, *, #39045, .T. ) ;
#79495 = FACE_OUTER_BOUND ( 'NONE', #136209, .T. ) ;
#79496 = EDGE_CURVE ( 'NONE', #110666, #45152, #31450, .T. ) ;
#79497 = ORIENTED_EDGE ( 'NONE', *, *, #121287, .F. ) ;
#79498 = FACE_OUTER_BOUND ( 'NONE', #111997, .T. ) ;
#79499 = AXIS2_PLACEMENT_3D ( 'NONE', #124942, #101764, #112646 ) ;
#79500 = DIRECTION ( 'NONE',  ( 1.000000000000000000, 0.000000000000000000, 0.000000000000000000 ) ) ;
#79501 = DIRECTION ( 'NONE',  ( 0.000000000000000000, 0.3543493200069153248, 0.9351131265310291818 ) ) ;
#79502 = ORIENTED_EDGE ( 'NONE', *, *, #39513, .F. ) ;
#79503 = DIRECTION ( 'NONE',  ( -0.000000000000000000, -0.3543493200069152693, 0.9351131265310292928 ) ) ;
#79504 = EDGE_CURVE ( 'NONE', #131250, #31365, #32905, .T. ) ;
#79505 = PLANE ( 'NONE',  #40828 ) ;
#79506 = VECTOR ( 'NONE', #47452, 1000.000000000000000 ) ;
#79507 = CARTESIAN_POINT ( 'NONE',  ( 25.39999999999999503, 7.925800835032758229, -0.5567874546942058744 ) ) ;
#79508 = CARTESIAN_POINT ( 'NONE',  ( 19.10813147593277250, 4.202752102959690472E-16, 0.000000000000000000 ) ) ;
#79509 = CARTESIAN_POINT ( 'NONE',  ( -26.90332935812578086, -2.240707523384264377, 15.26439735382746221 ) ) ;
#79510 = DIRECTION ( 'NONE',  ( -0.7071067811865486830, -0.7071067811865464625, -0.000000000000000000 ) ) ;
#79511 = ORIENTED_EDGE ( 'NONE', *, *, #117361, .T. ) ;
#79512 = CARTESIAN_POINT ( 'NONE',  ( 87.47916666666664298, -7.950000000000000178, 2.130196079827424427 ) ) ;
#79513 = PLANE ( 'NONE',  #46569 ) ;
#79514 = VECTOR ( 'NONE', #134435, 999.9999999999998863 ) ;
#79515 = ORIENTED_EDGE ( 'NONE', *, *, #35035, .T. ) ;
#79516 = ADVANCED_FACE ( 'NONE', ( #87255 ), #67734, .T. ) ;
#79517 = EDGE_LOOP ( 'NONE', ( #69309, #95124, #73545, #1369, #24184 ) ) ;
#79518 = EDGE_CURVE ( 'NONE', #141782, #80772, #143056, .T. ) ;
#79519 = ORIENTED_EDGE ( 'NONE', *, *, #118571, .F. ) ;
#79520 = CARTESIAN_POINT ( 'NONE',  ( 50.16709685856476852, -3.055000000000000160, -5.291415217122921177 ) ) ;
#79521 = VERTEX_POINT ( 'NONE', #21285 ) ;
#79522 = VECTOR ( 'NONE', #101441, 1000.000000000000000 ) ;
#79523 = FACE_OUTER_BOUND ( 'NONE', #38674, .T. ) ;
#79524 = VECTOR ( 'NONE', #43856, 1000.000000000000000 ) ;
#79525 = CARTESIAN_POINT ( 'NONE',  ( 7.629139616203772789, 5.278424836066147208, 3.047499999999990550 ) ) ;
#79526 = CARTESIAN_POINT ( 'NONE',  ( 87.79209685856477563, -5.291415217122921177, 3.054999999999999272 ) ) ;
#79527 = CARTESIAN_POINT ( 'NONE',  ( 28.49999999999981171, -16.91253812416058011, 4.000000000000000000 ) ) ;
#79528 = EDGE_LOOP ( 'NONE', ( #21513, #68043, #12217, #103838 ) ) ;
#79529 = CARTESIAN_POINT ( 'NONE',  ( -29.99999999999978328, 5.966399257802205369, 5.000000000000000000 ) ) ;
#79530 = ORIENTED_EDGE ( 'NONE', *, *, #95559, .T. ) ;
#79531 = PLANE ( 'NONE',  #76561 ) ;
#79532 = CIRCLE ( 'NONE', #40090, 2.500000000000000888 ) ;
#79533 = PLANE ( 'NONE',  #111954 ) ;
#79534 = ORIENTED_EDGE ( 'NONE', *, *, #35081, .T. ) ;
#79535 = EDGE_CURVE ( 'NONE', #118679, #5639, #95971, .T. ) ;
#79536 = DIRECTION ( 'NONE',  ( -0.3543493200069163240, -0.000000000000000000, -0.9351131265310288487 ) ) ;
#79537 = CARTESIAN_POINT ( 'NONE',  ( -6.461603553705668190, -9.740707523384180888, 17.74957260769609135 ) ) ;
#79538 = CARTESIAN_POINT ( 'NONE',  ( 126.6412635252314516, 4.472830434245837594, 4.472830434245841147 ) ) ;
#79539 = ORIENTED_EDGE ( 'NONE', *, *, #98639, .T. ) ;
#79540 = CARTESIAN_POINT ( 'NONE',  ( -36.48921356237310221, -27.52281430457080802, 5.000000000000000000 ) ) ;
#79541 = ORIENTED_EDGE ( 'NONE', *, *, #27514, .F. ) ;
#79542 = ORIENTED_EDGE ( 'NONE', *, *, #65542, .F. ) ;
#79543 = VERTEX_POINT ( 'NONE', #19136 ) ;
#79544 = PLANE ( 'NONE',  #5369 ) ;
#79545 = VECTOR ( 'NONE', #61296, 1000.000000000000000 ) ;
#79546 = DIRECTION ( 'NONE',  ( 0.000000000000000000, 2.556434596176436916E-15, 1.000000000000000000 ) ) ;
#79547 = CARTESIAN_POINT ( 'NONE',  ( -9.183988606268997046, 28.73617430169793607, 5.000000000000000000 ) ) ;
#79548 = DIRECTION ( 'NONE',  ( -0.000000000000000000, -0.3543493200069152693, 0.9351131265310292928 ) ) ;
#79549 = FACE_OUTER_BOUND ( 'NONE', #71552, .T. ) ;
#79550 = VECTOR ( 'NONE', #85259, 1000.000000000000227 ) ;
#79551 = ORIENTED_EDGE ( 'NONE', *, *, #75665, .F. ) ;
#79552 = CARTESIAN_POINT ( 'NONE',  ( 21.48921356237309155, -27.52281430457070499, 5.000000000000000000 ) ) ;
#79553 = CARTESIAN_POINT ( 'NONE',  ( 25.64540314143522082, -2.126176841940958351, -7.934999999999989839 ) ) ;
#79554 = DIRECTION ( 'NONE',  ( 0.7071067811865487940, 0.7071067811865463515, 0.000000000000000000 ) ) ;
#79555 = EDGE_CURVE ( 'NONE', #88426, #142286, #9671, .T. ) ;
#79556 = DIRECTION ( 'NONE',  ( 1.000000000000000000, 0.000000000000000000, 0.000000000000000000 ) ) ;
#79557 = CARTESIAN_POINT ( 'NONE',  ( -33.41687398106825668, 22.27000000000000668, -13.94762968036370054 ) ) ;
#79558 = ORIENTED_EDGE ( 'NONE', *, *, #13265, .F. ) ;
#79559 = EDGE_CURVE ( 'NONE', #136825, #10452, #65541, .T. ) ;
#79560 = ORIENTED_EDGE ( 'NONE', *, *, #16847, .T. ) ;
#79561 = EDGE_LOOP ( 'NONE', ( #137936, #12718, #63798, #38234, #142256 ) ) ;
#79562 = DIRECTION ( 'NONE',  ( 0.7071067811865487940, 0.7071067811865463515, 0.000000000000000000 ) ) ;
#79563 = CARTESIAN_POINT ( 'NONE',  ( 56.99999999999999289, 0.000000000000000000, -7.950000000000000178 ) ) ;
#79564 = UNCERTAINTY_MEASURE_WITH_UNIT (LENGTH_MEASURE( 1.000000000000000082E-05 ), #33390, 'distance_accuracy_value', 'NONE');
#79565 = CARTESIAN_POINT ( 'NONE',  ( 34.92499999999998295, -2.240707523384260824, 4.255531930566177401 ) ) ;
#79566 = CARTESIAN_POINT ( 'NONE',  ( -0.005480084712502889671, 28.92564299267938210, 4.000000000000000000 ) ) ;
#79567 = ADVANCED_FACE ( 'NONE', ( #30001 ), #118435, .F. ) ;
#79569 = EDGE_CURVE ( 'NONE', #14243, #128877, #52466, .T. ) ;
#79568 = DIRECTION ( 'NONE',  ( -0.3543493200069162685, -0.000000000000000000, -0.9351131265310288487 ) ) ;
#79570 = AXIS2_PLACEMENT_3D ( 'NONE', #15938, #127616, #94253 ) ;
#79571 = CARTESIAN_POINT ( 'NONE',  ( -35.00492477221173715, -5.240707523384228850, 12.38332538355504298 ) ) ;
#79572 = CARTESIAN_POINT ( 'NONE',  ( 34.42499999999998295, 16.54139925780187781, 5.000000000000000000 ) ) ;
#79573 = CARTESIAN_POINT ( 'NONE',  ( 39.48921356237310221, -27.52281430457082934, 5.000000000000000000 ) ) ;
#79574 = DIRECTION ( 'NONE',  ( -1.000000000000000000, -1.224606353822377258E-16, -0.000000000000000000 ) ) ;
#79575 = LINE ( 'NONE', #44801, #113586 ) ;
#79576 = VECTOR ( 'NONE', #120373, 1000.000000000000000 ) ;
#79577 = EDGE_LOOP ( 'NONE', ( #18991, #76010, #60251, #34676 ) ) ;
#79578 = CARTESIAN_POINT ( 'NONE',  ( 19.48939575397828960, -0.003013263964889829026, -31.00984187987698704 ) ) ;
#79579 = EDGE_LOOP ( 'NONE', ( #130529, #29310 ) ) ;
#79580 = DIRECTION ( 'NONE',  ( 0.6830127018922181881, 0.6830127018922202975, -0.2588190451025214056 ) ) ;
#79582 = ORIENTED_EDGE ( 'NONE', *, *, #112952, .T. ) ;
#79581 = CARTESIAN_POINT ( 'NONE',  ( 18.71757738642554258, -21.73023691814492864, 5.000000000000000888 ) ) ;
#79583 = EDGE_CURVE ( 'NONE', #33411, #122222, #141645, .T. ) ;
#79584 = EDGE_CURVE ( 'NONE', #17037, #84184, #86554, .T. ) ;
#79585 = CARTESIAN_POINT ( 'NONE',  ( -15.00548008471250228, 28.92564299267927552, 4.000000000000000000 ) ) ;
#79586 = CARTESIAN_POINT ( 'NONE',  ( -34.92500000000001137, -0.1833456135895722428, 4.500000000000000888 ) ) ;
#79587 = ORIENTED_EDGE ( 'NONE', *, *, #133286, .T. ) ;
#79588 = DIRECTION ( 'NONE',  ( 0.000000000000000000, -0.000000000000000000, -1.000000000000000000 ) ) ;
#79589 = VERTEX_POINT ( 'NONE', #119844 ) ;
#79590 = DIRECTION ( 'NONE',  ( 0.7071067811865487940, 0.7071067811865463515, 0.000000000000000000 ) ) ;
#79591 = VERTEX_POINT ( 'NONE', #137732 ) ;
#79592 = VECTOR ( 'NONE', #39350, 999.9999999999998863 ) ;
#79593 = LINE ( 'NONE', #90408, #112452 ) ;
#79594 = EDGE_CURVE ( 'NONE', #139774, #102386, #22665, .T. ) ;
#79595 = CARTESIAN_POINT ( 'NONE',  ( 106.3916937171295700, 2.130196079827421762, 7.950000000000001066 ) ) ;
#79596 = CARTESIAN_POINT ( 'NONE',  ( -12.69999999999998153, 0.000000000000000000, 0.000000000000000000 ) ) ;
#79597 = VECTOR ( 'NONE', #76150, 1000.000000000000227 ) ;
#79598 = CARTESIAN_POINT ( 'NONE',  ( -5.999999999999950262, -16.44781430457066662, 5.000000000000000000 ) ) ;
#79599 = ORIENTED_EDGE ( 'NONE', *, *, #110687, .T. ) ;
#79600 = FILL_AREA_STYLE_COLOUR ( '', #93146 ) ;
#79601 = LINE ( 'NONE', #34612, #70481 ) ;
#79602 = DIRECTION ( 'NONE',  ( 0.7071067811865486830, -0.7071067811865464625, -0.000000000000000000 ) ) ;
#79603 = CARTESIAN_POINT ( 'NONE',  ( 13.85416666666666430, 1.633150327867695095, 6.094999999999988205 ) ) ;
#79604 = DIRECTION ( 'NONE',  ( 0.7071067811865486830, -0.7071067811865464625, -0.000000000000000000 ) ) ;
#79605 = ADVANCED_FACE ( 'NONE', ( #115199 ), #15882, .F. ) ;
#79606 = CARTESIAN_POINT ( 'NONE',  ( 59.99451991528749772, 28.92564299267980132, 4.000000000000000000 ) ) ;
#79607 = ORIENTED_EDGE ( 'NONE', *, *, #116128, .T. ) ;
#79608 = VECTOR ( 'NONE', #97468, 1000.000000000000000 ) ;
#79609 = CARTESIAN_POINT ( 'NONE',  ( -23.99999999999983302, 10.93112307739207267, 4.000000000000000000 ) ) ;
#79610 = ORIENTED_EDGE ( 'NONE', *, *, #80691, .F. ) ;
#79611 = VECTOR ( 'NONE', #99612, 999.9999999999998863 ) ;
#79612 = CARTESIAN_POINT ( 'NONE',  ( 92.02126352523143282, -4.472830434245839371, -4.472830434245840259 ) ) ;
#79613 = FACE_OUTER_BOUND ( 'NONE', #110522, .T. ) ;
#79614 = DIRECTION ( 'NONE',  ( 0.000000000000000000, -0.3543493200069153248, -0.9351131265310291818 ) ) ;
#79615 = EDGE_CURVE ( 'NONE', #134155, #35701, #40727, .T. ) ;
#79616 = CARTESIAN_POINT ( 'NONE',  ( 0.000000000000000000, 0.000000000000000000, 5.000000000000000000 ) ) ;
#79617 = CARTESIAN_POINT ( 'NONE',  ( -63.18398860626900415, 28.73617430169831621, 5.000000000000000000 ) ) ;
#79618 = ORIENTED_EDGE ( 'NONE', *, *, #86685, .T. ) ;
#79619 = CARTESIAN_POINT ( 'NONE',  ( 26.99451991528749417, 28.92564299267956685, 4.000000000000000000 ) ) ;
#79620 = PRESENTATION_STYLE_ASSIGNMENT (( #123080 ) ) ;
#79621 = CIRCLE ( 'NONE', #35615, 2.500000000000000444 ) ;
#79622 = CARTESIAN_POINT ( 'NONE',  ( 27.18398860626900060, 28.73617430169806042, 5.000000000000000000 ) ) ;
#79623 = ORIENTED_EDGE ( 'NONE', *, *, #133756, .F. ) ;
#79624 = CARTESIAN_POINT ( 'NONE',  ( -17.51078643762690845, -27.52281430457043143, 5.000000000000000000 ) ) ;
#79625 = FACE_OUTER_BOUND ( 'NONE', #76977, .T. ) ;
#79628 = ORIENTED_EDGE ( 'NONE', *, *, #126456, .F. ) ;
#79627 = EDGE_CURVE ( 'NONE', #52228, #24833, #60171, .T. ) ;
#79626 = DIRECTION ( 'NONE',  ( -0.000000000000000000, -0.000000000000000000, -1.000000000000000000 ) ) ;
#79630 = ADVANCED_FACE ( 'NONE', ( #99528 ), #81948, .T. ) ;
#79629 = FACE_OUTER_BOUND ( 'NONE', #140513, .T. ) ;
#79631 = CARTESIAN_POINT ( 'NONE',  ( 102.3083603837962130, 7.949999999999996625, 2.130196079827431088 ) ) ;
#79632 = CARTESIAN_POINT ( 'NONE',  ( 9.241694584251812117, 0.7592924766157069794, 14.37146558664980489 ) ) ;
#79633 = CARTESIAN_POINT ( 'NONE',  ( -2.816011393730999401, 28.73617430169785436, 5.000000000000000000 ) ) ;
#79634 = LINE ( 'NONE', #112911, #65528 ) ;
#79635 = VECTOR ( 'NONE', #107609, 1000.000000000000114 ) ;
#79636 = ORIENTED_EDGE ( 'NONE', *, *, #65832, .F. ) ;
#79637 = ADVANCED_FACE ( 'NONE', ( #4267 ), #121997, .F. ) ;
#79638 = ORIENTED_EDGE ( 'NONE', *, *, #17605, .F. ) ;
#79639 = ORIENTED_EDGE ( 'NONE', *, *, #35327, .F. ) ;
#79640 = CARTESIAN_POINT ( 'NONE',  ( 83.56293019189811844, 1.637169565754157174, 6.110000000000002984 ) ) ;
#79641 = VECTOR ( 'NONE', #134786, 1000.000000000000000 ) ;
#79642 = EDGE_LOOP ( 'NONE', ( #50815, #133844, #39919, #81176 ) ) ;
#79643 = CARTESIAN_POINT ( 'NONE',  ( 29.50183651486025482, -17.24070752338410628, 8.407044977365156768 ) ) ;
#79644 = CARTESIAN_POINT ( 'NONE',  ( -34.49999999999975842, 10.46425560840038038, 4.994342998332163219 ) ) ;
#79645 = VECTOR ( 'NONE', #128942, 1000.000000000000000 ) ;
#79646 = DIRECTION ( 'NONE',  ( 0.7071067811865487940, 0.7071067811865463515, 0.000000000000000000 ) ) ;
#79647 = FACE_OUTER_BOUND ( 'NONE', #99193, .T. ) ;
#79648 = ORIENTED_EDGE ( 'NONE', *, *, #141859, .T. ) ;
#79649 = CARTESIAN_POINT ( 'NONE',  ( 102.5000000000000142, 0.000000000000000000, -7.950000000000000178 ) ) ;
#79650 = LINE ( 'NONE', #91213, #92985 ) ;
#79651 = DIRECTION ( 'NONE',  ( -0.000000000000000000, 0.3543493200069153248, 0.9351131265310292928 ) ) ;
#79652 = CARTESIAN_POINT ( 'NONE',  ( 75.30793019189809456, -6.109999999999998543, 1.637169565754158063 ) ) ;
#79653 = ORIENTED_EDGE ( 'NONE', *, *, #130028, .F. ) ;
#79654 = DIRECTION ( 'NONE',  ( -0.6830127018922181881, 0.6830127018922202975, -0.2588190451025214056 ) ) ;
#79655 = VECTOR ( 'NONE', #59730, 1000.000000000000227 ) ;
#79656 = DIRECTION ( 'NONE',  ( -0.000000000000000000, 0.3543493200069153248, 0.9351131265310292928 ) ) ;
#79657 = ORIENTED_EDGE ( 'NONE', *, *, #8865, .F. ) ;
#79658 = ORIENTED_EDGE ( 'NONE', *, *, #73675, .T. ) ;
#79659 = FACE_OUTER_BOUND ( 'NONE', #54823, .T. ) ;
#79660 = CARTESIAN_POINT ( 'NONE',  ( 8.671830600776420539, 14.25929247661558286, 4.000000000000000000 ) ) ;
#79661 = VECTOR ( 'NONE', #109714, 999.9999999999998863 ) ;
#79662 = CARTESIAN_POINT ( 'NONE',  ( 63.29974487139158867, -27.71228299555250274, 4.000000000000000000 ) ) ;
#79663 = CARTESIAN_POINT ( 'NONE',  ( 3.010806948443980779, -48.09618305010688744, -37.50858089739958956 ) ) ;
#79664 = DIRECTION ( 'NONE',  ( -0.000000000000000000, -0.3543493200069152693, 0.9351131265310292928 ) ) ;
#79665 = CARTESIAN_POINT ( 'NONE',  ( 54.18398860626899705, 28.73617430169825226, 5.000000000000000000 ) ) ;
#79666 = VECTOR ( 'NONE', #143480, 1000.000000000000000 ) ;
#79667 = ORIENTED_EDGE ( 'NONE', *, *, #22688, .F. ) ;
#79668 = VERTEX_POINT ( 'NONE', #197 ) ;
#79669 = CARTESIAN_POINT ( 'NONE',  ( -27.18398860626900060, 28.73617430169806042, 5.000000000000000000 ) ) ;
#79670 = ORIENTED_EDGE ( 'NONE', *, *, #130389, .T. ) ;
#79671 = ADVANCED_FACE ( 'NONE', ( #114519 ), #134339, .F. ) ;
#79672 = ORIENTED_EDGE ( 'NONE', *, *, #85559, .F. ) ;
#79673 = VECTOR ( 'NONE', #10594, 1000.000000000000000 ) ;
#79674 = DIRECTION ( 'NONE',  ( 0.7071067811865487940, 0.7071067811865463515, 0.000000000000000000 ) ) ;
#79675 = ORIENTED_EDGE ( 'NONE', *, *, #134544, .F. ) ;
#79676 = CARTESIAN_POINT ( 'NONE',  ( 57.53752705046289151, -9.735942053221456900E-16, 7.949999999999998401 ) ) ;
#79677 = FACE_OUTER_BOUND ( 'NONE', #37050, .T. ) ;
#79678 = DIRECTION ( 'NONE',  ( 0.000000000000000000, -1.000000000000000000, 0.000000000000000000 ) ) ;
#79679 = DIRECTION ( 'NONE',  ( -0.7071067811865486830, -0.7071067811865464625, 0.000000000000000000 ) ) ;
#79680 = VERTEX_POINT ( 'NONE', #133623 ) ;
#79681 = DIRECTION ( 'NONE',  ( 0.6830127018922180770, -0.6830127018922204085, -0.2588190451025213501 ) ) ;
#79682 = ORIENTED_EDGE ( 'NONE', *, *, #108769, .T. ) ;
#79683 = EDGE_CURVE ( 'NONE', #129879, #31472, #28385, .T. ) ;
#79684 = FACE_OUTER_BOUND ( 'NONE', #17990, .T. ) ;
#79685 = ORIENTED_EDGE ( 'NONE', *, *, #3640, .T. ) ;
#79686 = LINE ( 'NONE', #143445, #16815 ) ;
#79687 = ORIENTED_EDGE ( 'NONE', *, *, #29576, .F. ) ;
#79689 = EDGE_CURVE ( 'NONE', #40406, #82818, #36962, .T. ) ;
#79688 = CARTESIAN_POINT ( 'NONE',  ( 29.99999999999979039, -1.068876922607804314, 4.000000000000000000 ) ) ;
#79690 = VERTEX_POINT ( 'NONE', #12533 ) ;
#79691 = VERTEX_POINT ( 'NONE', #56810 ) ;
#79692 = VECTOR ( 'NONE', #114897, 999.9999999999998863 ) ;
#79693 = EDGE_LOOP ( 'NONE', ( #103590, #61593, #40681, #20300 ) ) ;
#79694 = CARTESIAN_POINT ( 'NONE',  ( 94.33333333333332860, -6.884901960086287964, 3.974999999999998312 ) ) ;
#79695 = VECTOR ( 'NONE', #138582, 999.9999999999998863 ) ;
#79696 = CARTESIAN_POINT ( 'NONE',  ( 0.7071067811865432429, -9.740707523384182664, 5.000000000000000000 ) ) ;
#79697 = PLANE ( 'NONE',  #3184 ) ;
#79698 = CARTESIAN_POINT ( 'NONE',  ( 120.1670968585647756, -3.055000000000000160, -5.291415217122921177 ) ) ;
#79699 = PLANE ( 'NONE',  #142345 ) ;
#79700 = ADVANCED_FACE ( 'NONE', ( #45911 ), #90095, .F. ) ;
#79701 = CARTESIAN_POINT ( 'NONE',  ( -66.48921356237309510, -27.52281430457101763, 5.000000000000000000 ) ) ;
#79702 = CARTESIAN_POINT ( 'NONE',  ( -25.77325839282151065, -11.24070752338416845, 18.24660765846976673 ) ) ;
#79704 = DIRECTION ( 'NONE',  ( -0.6830127018922181881, 0.6830127018922202975, -0.2588190451025214056 ) ) ;
#79703 = VECTOR ( 'NONE', #56883, 999.9999999999998863 ) ;
#79705 = EDGE_CURVE ( 'NONE', #5082, #9910, #94188, .T. ) ;
#79706 = ORIENTED_EDGE ( 'NONE', *, *, #70247, .T. ) ;
#79707 = DIRECTION ( 'NONE',  ( -0.7071067811865486830, -0.7071067811865464625, -0.000000000000000000 ) ) ;
#79708 = AXIS2_PLACEMENT_3D ( 'NONE', #18863, #54397, #98571 ) ;
#79709 = CARTESIAN_POINT ( 'NONE',  ( -6.005480084712508493, 28.92564299267933947, 4.000000000000000000 ) ) ;
#79710 = AXIS2_PLACEMENT_3D ( 'NONE', #33603, #77803, #22654 ) ;
#79711 = ORIENTED_EDGE ( 'NONE', *, *, #81637, .F. ) ;
#79712 = ORIENTED_EDGE ( 'NONE', *, *, #46836, .F. ) ;
#79713 = LINE ( 'NONE', #68808, #21721 ) ;
#79714 = EDGE_CURVE ( 'NONE', #117294, #105391, #39859, .T. ) ;
#79715 = ORIENTED_EDGE ( 'NONE', *, *, #14329, .T. ) ;
#79716 = AXIS2_PLACEMENT_3D ( 'NONE', #45842, #90772, #100207 ) ;
#79717 = CARTESIAN_POINT ( 'NONE',  ( -31.49999999999977973, -5.568876922607755908, 4.000000000000000000 ) ) ;
#79718 = PLANE ( 'NONE',  #1526 ) ;
#79719 = VECTOR ( 'NONE', #32800, 999.9999999999998863 ) ;
#79720 = DIRECTION ( 'NONE',  ( 1.000000000000000000, 0.000000000000000000, 0.000000000000000000 ) ) ;
#79721 = LINE ( 'NONE', #47099, #134394 ) ;
#79722 = ORIENTED_EDGE ( 'NONE', *, *, #140761, .F. ) ;
#79723 = ORIENTED_EDGE ( 'NONE', *, *, #117727, .F. ) ;
#79725 = VECTOR ( 'NONE', #43446, 1000.000000000000000 ) ;
#79724 = LINE ( 'NONE', #47103, #70040 ) ;
#79726 = VECTOR ( 'NONE', #139040, 999.9999999999998863 ) ;
#79727 = CARTESIAN_POINT ( 'NONE',  ( 26.60873647476855552, -5.808823158059033709, 5.808823158059035485 ) ) ;
#79728 = ORIENTED_EDGE ( 'NONE', *, *, #84535, .T. ) ;
#79729 = CARTESIAN_POINT ( 'NONE',  ( 84.78709685856478018, 3.054999999999997939, 5.291415217122920289 ) ) ;
#79730 = DIRECTION ( 'NONE',  ( -1.000000000000000000, -0.000000000000000000, -0.000000000000000000 ) ) ;
#79731 = FACE_OUTER_BOUND ( 'NONE', #36670, .T. ) ;
#79732 = EDGE_LOOP ( 'NONE', ( #120039, #39458, #137164, #105310 ) ) ;
#79733 = EDGE_CURVE ( 'NONE', #126893, #22921, #116666, .T. ) ;
#79734 = VERTEX_POINT ( 'NONE', #7886 ) ;
#79735 = VERTEX_POINT ( 'NONE', #27499 ) ;
#79736 = DIRECTION ( 'NONE',  ( 0.9659258262890703106, 3.169619151431672497E-17, 0.2588190451025131900 ) ) ;
#79737 = CARTESIAN_POINT ( 'NONE',  ( -23.99999999999982592, -16.02097659208072855, -11.96015758381202865 ) ) ;
#79738 = LINE ( 'NONE', #137646, #63573 ) ;
#79739 = DIRECTION ( 'NONE',  ( -0.7071067811865487940, 0.7071067811865463515, 0.000000000000000000 ) ) ;
#79740 = EDGE_LOOP ( 'NONE', ( #44675, #44492, #51496, #120473 ) ) ;
#79741 = EDGE_CURVE ( 'NONE', #96308, #49442, #28954, .T. ) ;
#79742 = EDGE_CURVE ( 'NONE', #24873, #93367, #105077, .T. ) ;
#79743 = CARTESIAN_POINT ( 'NONE',  ( -27.32816939922334143, -15.74070752338412049, 4.000000000000000000 ) ) ;
#79744 = CARTESIAN_POINT ( 'NONE',  ( 9.183988606268997046, 28.73617430169793607, 5.000000000000000000 ) ) ;
#79745 = CARTESIAN_POINT ( 'NONE',  ( -42.29974487139158157, -27.71228299555235708, 4.000000000000000000 ) ) ;
#79746 = EDGE_LOOP ( 'NONE', ( #4937, #139823, #67819, #95331 ) ) ;
#79747 = AXIS2_PLACEMENT_3D ( 'NONE', #15106, #37613, #47801 ) ;
#79749 = EDGE_CURVE ( 'NONE', #121955, #126191, #73193, .T. ) ;
#79748 = FACE_OUTER_BOUND ( 'NONE', #49029, .T. ) ;
#79750 = ORIENTED_EDGE ( 'NONE', *, *, #123501, .T. ) ;
#79752 = VERTEX_POINT ( 'NONE', #51432 ) ;
#79751 = CARTESIAN_POINT ( 'NONE',  ( 57.42758194782751247, -45.84254607569121021, -35.55177538329067488 ) ) ;
#79754 = VERTEX_POINT ( 'NONE', #127549 ) ;
#79753 = EDGE_CURVE ( 'NONE', #92724, #13174, #126815, .T. ) ;
#79755 = EDGE_CURVE ( 'NONE', #50562, #91076, #6420, .T. ) ;
#79756 = DIRECTION ( 'NONE',  ( 0.000000000000000000, 0.000000000000000000, -1.000000000000000000 ) ) ;
#79757 = CARTESIAN_POINT ( 'NONE',  ( -54.18398860626899705, 28.73617430169825226, 5.000000000000000000 ) ) ;
#79758 = ORIENTED_EDGE ( 'NONE', *, *, #141396, .F. ) ;
#79759 = CARTESIAN_POINT ( 'NONE',  ( -34.75611968250420603, 8.812934254707275983, 4.955485411084900704 ) ) ;
#79760 = ORIENTED_EDGE ( 'NONE', *, *, #33044, .T. ) ;
#79761 = LINE ( 'NONE', #57993, #116996 ) ;
#79762 = DIRECTION ( 'NONE',  ( 0.7071067811865487940, 0.7071067811865463515, 0.000000000000000000 ) ) ;
#79763 = CARTESIAN_POINT ( 'NONE',  ( -80.99451991528748351, 28.92564299267994699, 4.000000000000000000 ) ) ;
#79764 = EDGE_CURVE ( 'NONE', #135826, #135984, #28243, .T. ) ;
#79765 = CARTESIAN_POINT ( 'NONE',  ( 23.81601139373100295, 28.73617430169770870, 5.000000000000000000 ) ) ;
#79766 = PLANE ( 'NONE',  #111429 ) ;
#79767 = PLANE ( 'NONE',  #25984 ) ;
#79768 = CARTESIAN_POINT ( 'NONE',  ( 29.99999999999979394, -1.447814304570815169, 5.000000000000000000 ) ) ;
#79769 = CARTESIAN_POINT ( 'NONE',  ( 16.45790314143522082, 6.871911579029515771, 3.967499999999989146 ) ) ;
#79770 = DIRECTION ( 'NONE',  ( -0.7071067811865486830, -0.7071067811865464625, 0.000000000000000000 ) ) ;
#79771 = DIRECTION ( 'NONE',  ( -0.3543493200069162685, -0.000000000000000000, -0.9351131265310288487 ) ) ;
#79772 = EDGE_CURVE ( 'NONE', #44308, #40891, #72397, .T. ) ;
#79773 = CARTESIAN_POINT ( 'NONE',  ( -7.446650576632133145, 2.259292476615690770, 14.86850063742356198 ) ) ;
#79774 = DIRECTION ( 'NONE',  ( -0.6830127018922181881, 0.6830127018922202975, -0.2588190451025214056 ) ) ;
#79775 = VERTEX_POINT ( 'NONE', #5738 ) ;
#79776 = VECTOR ( 'NONE', #51994, 1000.000000000000000 ) ;
#79777 = VERTEX_POINT ( 'NONE', #96306 ) ;
#79778 = CARTESIAN_POINT ( 'NONE',  ( 87.62500000000001421, -7.950000000000000178, -4.867971026610729436E-16 ) ) ;
#79779 = ORIENTED_EDGE ( 'NONE', *, *, #131492, .T. ) ;
#79780 = VERTEX_POINT ( 'NONE', #139879 ) ;
#79781 = VERTEX_POINT ( 'NONE', #129674 ) ;
#79782 = CARTESIAN_POINT ( 'NONE',  ( 34.49999999999975131, -5.945670655168991736, 4.994342998332164996 ) ) ;
#79783 = FACE_OUTER_BOUND ( 'NONE', #140938, .T. ) ;
#79784 = FACE_OUTER_BOUND ( 'NONE', #58801, .T. ) ;
#79785 = ORIENTED_EDGE ( 'NONE', *, *, #111046, .T. ) ;
#79786 = CARTESIAN_POINT ( 'NONE',  ( 15.29974487139158867, -27.71228299555216879, 4.000000000000000000 ) ) ;
#79787 = FACE_OUTER_BOUND ( 'NONE', #54413, .T. ) ;
#79788 = CARTESIAN_POINT ( 'NONE',  ( 27.48921356237309155, -27.52281430457074762, 5.000000000000000000 ) ) ;
#79789 = CARTESIAN_POINT ( 'NONE',  ( 126.5612402446580944, 6.599829397831250333, 1.990250523215890688 ) ) ;
#79790 = CARTESIAN_POINT ( 'NONE',  ( 128.5370968585647802, -3.054999999999998828, -5.291415217122919401 ) ) ;
#79791 = DIRECTION ( 'NONE',  ( 0.7071067811865486830, -0.7071067811865464625, -0.000000000000000000 ) ) ;
#79792 = DIRECTION ( 'NONE',  ( -0.7071067811865487940, 0.7071067811865463515, -0.000000000000000000 ) ) ;
#79793 = CARTESIAN_POINT ( 'NONE',  ( -17.70025512860841488, -27.71228299555193786, 4.000000000000000000 ) ) ;
#79794 = ADVANCED_FACE ( 'NONE', ( #71763 ), #74615, .T. ) ;
#79795 = VECTOR ( 'NONE', #56697, 999.9999999999998863 ) ;
#79796 = DIRECTION ( 'NONE',  ( -0.7071067811865486830, -0.7071067811865464625, -0.000000000000000000 ) ) ;
#79797 = LINE ( 'NONE', #91360, #5271 ) ;
#79798 = DIRECTION ( 'NONE',  ( -0.7071067811865486830, 0.7071067811865464625, 0.000000000000000000 ) ) ;
#79799 = CARTESIAN_POINT ( 'NONE',  ( 24.18398860626899705, 28.73617430169804265, 5.000000000000000000 ) ) ;
#79800 =( NAMED_UNIT ( * ) PLANE_ANGLE_UNIT ( ) SI_UNIT ( $, .RADIAN. ) );
#79801 = EDGE_CURVE ( 'NONE', #54679, #69767, #16630, .T. ) ;
#79802 = EDGE_CURVE ( 'NONE', #46380, #27078, #117356, .T. ) ;
#79803 = CIRCLE ( 'NONE', #21881, 2.500000000000000444 ) ;
#79804 = EDGE_LOOP ( 'NONE', ( #61310, #39286, #117872, #54659 ) ) ;
#79805 = ORIENTED_EDGE ( 'NONE', *, *, #140825, .F. ) ;
#79806 = CARTESIAN_POINT ( 'NONE',  ( 108.9379301918981042, -6.110000000000001208, 1.637169565754158951 ) ) ;
#79807 = EDGE_LOOP ( 'NONE', ( #23620, #116053, #42926, #76221, #124303, #19911 ) ) ;
#79808 = VECTOR ( 'NONE', #124839, 1000.000000000000000 ) ;
#79809 = CARTESIAN_POINT ( 'NONE',  ( 100.7500000000000000, -9.735942053221458872E-16, 7.950000000000000178 ) ) ;
#79810 =( NAMED_UNIT ( * ) SI_UNIT ( $, .STERADIAN. ) SOLID_ANGLE_UNIT ( ) );
#79811 = DIRECTION ( 'NONE',  ( -0.7071067811865487940, 0.7071067811865463515, -0.000000000000000000 ) ) ;
#79812 = PLANE ( 'NONE',  #120697 ) ;
#79813 = CARTESIAN_POINT ( 'NONE',  ( 112.9329301918981230, 1.637169565754156508, 6.110000000000000320 ) ) ;
#79814 = VECTOR ( 'NONE', #131761, 1000.000000000000000 ) ;
#79815 = ORIENTED_EDGE ( 'NONE', *, *, #84644, .T. ) ;
#79816 = ORIENTED_EDGE ( 'NONE', *, *, #3479, .F. ) ;
#79817 = CARTESIAN_POINT ( 'NONE',  ( -5.292893218813416567, 2.259292476615692546, 5.000000000000000000 ) ) ;
#79818 = FACE_OUTER_BOUND ( 'NONE', #44613, .T. ) ;
#79819 = ORIENTED_EDGE ( 'NONE', *, *, #53124, .T. ) ;
#79820 = ORIENTED_EDGE ( 'NONE', *, *, #3352, .T. ) ;
#79821 = ORIENTED_EDGE ( 'NONE', *, *, #92658, .F. ) ;
#79822 = CARTESIAN_POINT ( 'NONE',  ( -16.49999999999988276, -11.56887692260769285, 4.000000000000000000 ) ) ;
#79823 = CARTESIAN_POINT ( 'NONE',  ( 2.400403141435219379, -7.934999999999988951, 2.126176841940957907 ) ) ;
#79824 = VECTOR ( 'NONE', #72380, 1000.000000000000114 ) ;
#79825 = AXIS2_PLACEMENT_3D ( 'NONE', #85712, #32067, #9568 ) ;
#79826 = VECTOR ( 'NONE', #130517, 1000.000000000000227 ) ;
#79827 = CARTESIAN_POINT ( 'NONE',  ( 30.82876352523145158, 0.000000000000000000, -6.109999999999998543 ) ) ;
#79828 = ORIENTED_EDGE ( 'NONE', *, *, #130123, .F. ) ;
#79830 = EDGE_LOOP ( 'NONE', ( #14882, #46334, #13148, #92623 ) ) ;
#79829 = VECTOR ( 'NONE', #131864, 999.9999999999998863 ) ;
#79831 = DIRECTION ( 'NONE',  ( -0.000000000000000000, -0.3543493200069152693, 0.9351131265310292928 ) ) ;
#79832 = ORIENTED_EDGE ( 'NONE', *, *, #70739, .F. ) ;
#79833 = VERTEX_POINT ( 'NONE', #83339 ) ;
#79834 = VERTEX_POINT ( 'NONE', #72504 ) ;
#79835 = CARTESIAN_POINT ( 'NONE',  ( 25.49999999999982592, -7.533600742197662292, 5.000000000000000000 ) ) ;
#79836 = VECTOR ( 'NONE', #103318, 1000.000000000000000 ) ;
#79837 = DIRECTION ( 'NONE',  ( -0.7071067811865486830, 0.7071067811865464625, 0.000000000000000000 ) ) ;
#79838 = CARTESIAN_POINT ( 'NONE',  ( -34.92500000000001137, -21.18334561358935986, 4.500000000000000888 ) ) ;
#79839 = ORIENTED_EDGE ( 'NONE', *, *, #127275, .T. ) ;
#79840 = CARTESIAN_POINT ( 'NONE',  ( -34.42500000000001137, 19.54139925780181386, 5.000000000000000000 ) ) ;
#79841 = CARTESIAN_POINT ( 'NONE',  ( 69.18398860626899705, 28.73617430169835529, 5.000000000000000000 ) ) ;
#79842 = FACE_OUTER_BOUND ( 'NONE', #14310, .T. ) ;
#79843 = EDGE_CURVE ( 'NONE', #133751, #11858, #74980, .T. ) ;
#79844 = FACE_BOUND ( 'NONE', #3285, .T. ) ;
#79845 = EDGE_LOOP ( 'NONE', ( #76986, #87031, #65752, #100082 ) ) ;
#79846 = CARTESIAN_POINT ( 'NONE',  ( 42.48921356237308800, -27.52281430457085065, 5.000000000000000000 ) ) ;
#79847 = EDGE_CURVE ( 'NONE', #125405, #87449, #105763, .T. ) ;
#79849 = ADVANCED_FACE ( 'NONE', ( #139160 ), #84080, .F. ) ;
#79848 = DIRECTION ( 'NONE',  ( -1.000000000000000000, -1.224606353822377258E-16, -0.000000000000000000 ) ) ;
#79850 = CARTESIAN_POINT ( 'NONE',  ( -27.70710678118634718, 5.259292476615662792, 5.000000000000000000 ) ) ;
#79851 = VERTEX_POINT ( 'NONE', #107213 ) ;
#79852 = FACE_OUTER_BOUND ( 'NONE', #134699, .T. ) ;
#79853 = ORIENTED_EDGE ( 'NONE', *, *, #50869, .T. ) ;
#79854 = VERTEX_POINT ( 'NONE', #89063 ) ;
#79855 = ORIENTED_EDGE ( 'NONE', *, *, #78831, .T. ) ;
#79856 = EDGE_CURVE ( 'NONE', #14269, #117065, #123615, .T. ) ;
#79857 = EDGE_CURVE ( 'NONE', #103352, #64319, #61135, .T. ) ;
#79858 = CARTESIAN_POINT ( 'NONE',  ( 40.01626352523143737, -4.472830434245838482, 4.472830434245838482 ) ) ;
#79859 = VERTEX_POINT ( 'NONE', #86909 ) ;
#79860 = DIRECTION ( 'NONE',  ( -0.7071067811865486830, -0.7071067811865464625, -0.000000000000000000 ) ) ;
#79861 = CARTESIAN_POINT ( 'NONE',  ( -27.18398860626900060, 28.73617430169806042, 5.000000000000000000 ) ) ;
#79862 = EDGE_CURVE ( 'NONE', #92065, #100356, #120260, .T. ) ;
#79863 = ORIENTED_EDGE ( 'NONE', *, *, #142080, .T. ) ;
#79864 = DIRECTION ( 'NONE',  ( -0.3543493200069162685, -0.000000000000000000, -0.9351131265310288487 ) ) ;
#79865 = LINE ( 'NONE', #45093, #85159 ) ;
#79866 = AXIS2_PLACEMENT_3D ( 'NONE', #89793, #36152, #58666 ) ;
#79867 = EDGE_CURVE ( 'NONE', #76506, #135631, #131839, .T. ) ;
#79868 = SURFACE_STYLE_USAGE ( .BOTH. , #90715 ) ;
#79869 = CARTESIAN_POINT ( 'NONE',  ( 36.18398860626899705, 28.73617430169812437, 5.000000000000000000 ) ) ;
#79870 = DIRECTION ( 'NONE',  ( -1.000000000000000000, -1.224606353822377258E-16, -0.000000000000000000 ) ) ;
#79871 = ORIENTED_EDGE ( 'NONE', *, *, #76703, .F. ) ;
#79872 = EDGE_LOOP ( 'NONE', ( #5149, #71433, #96451, #128678 ) ) ;
#79873 = ORIENTED_EDGE ( 'NONE', *, *, #133989, .T. ) ;
#79874 = ORIENTED_EDGE ( 'NONE', *, *, #99024, .T. ) ;
#79875 = PLANE ( 'NONE',  #7691 ) ;
#79876 = EDGE_CURVE ( 'NONE', #5945, #27927, #134894, .T. ) ;
#79877 = EDGE_LOOP ( 'NONE', ( #57097, #54986, #69103, #58678 ) ) ;
#79878 = ORIENTED_EDGE ( 'NONE', *, *, #42467, .T. ) ;
#79879 = CARTESIAN_POINT ( 'NONE',  ( 164.5340954016161561, 26.96999999999993847, -34.26735321372807164 ) ) ;
#79880 = DIRECTION ( 'NONE',  ( -0.6830127018922180770, -0.6830127018922204085, -0.2588190451025213501 ) ) ;
#79881 = DIRECTION ( 'NONE',  ( 0.7071067811865487940, 0.7071067811865463515, -0.000000000000000000 ) ) ;
#79882 = VERTEX_POINT ( 'NONE', #31807 ) ;
#79883 = DIRECTION ( 'NONE',  ( -0.7071067811865486830, -0.7071067811865464625, 0.000000000000000000 ) ) ;
#79884 = ADVANCED_FACE ( 'NONE', ( #111502 ), #23034, .T. ) ;
#79885 = VERTEX_POINT ( 'NONE', #108606 ) ;
#79886 =( BOUNDED_CURVE ( )  B_SPLINE_CURVE ( 3, ( #73602, #14914, #115623, #62029 ),
 .UNSPECIFIED., .F., .T. ) 
 B_SPLINE_CURVE_WITH_KNOTS ( ( 4, 4 ),
 ( 5.920967161967926273, 7.341195215986592970 ),
 .UNSPECIFIED. ) 
 CURVE ( )  GEOMETRIC_REPRESENTATION_ITEM ( )  RATIONAL_B_SPLINE_CURVE ( ( 1.000000000000000000, 0.8388583629366708205, 0.8388583629366708205, 1.000000000000000000 ) ) 
 REPRESENTATION_ITEM ( '' )  );
#79887 = DIRECTION ( 'NONE',  ( -0.6830127018922181881, 0.6830127018922202975, -0.2588190451025214056 ) ) ;
#79888 = VECTOR ( 'NONE', #101315, 999.9999999999998863 ) ;
#79889 = CARTESIAN_POINT ( 'NONE',  ( 27.92123647476855197, -9.717572351234235426E-16, -7.934999999999990727 ) ) ;
#79890 = DIRECTION ( 'NONE',  ( -0.000000000000000000, 0.000000000000000000, 1.000000000000000000 ) ) ;
#79891 = ORIENTED_EDGE ( 'NONE', *, *, #100005, .F. ) ;
#79893 = DIRECTION ( 'NONE',  ( 0.000000000000000000, -1.000000000000000000, 0.000000000000000000 ) ) ;
#79892 = CARTESIAN_POINT ( 'NONE',  ( 111.4745968585647944, 1.637169565754164280, -6.109999999999997655 ) ) ;
#79894 = CARTESIAN_POINT ( 'NONE',  ( -21.48921356237309155, -27.52281430457070499, 5.000000000000000000 ) ) ;
#79895 = CARTESIAN_POINT ( 'NONE',  ( -23.99451991528749062, 28.92564299267954908, 4.000000000000000000 ) ) ;
#79896 = EDGE_CURVE ( 'NONE', #28591, #108745, #32528, .T. ) ;
#79897 = ORIENTED_EDGE ( 'NONE', *, *, #109620, .F. ) ;
#79898 = CARTESIAN_POINT ( 'NONE',  ( 27.48921356237309155, -27.52281430457074762, 5.000000000000000000 ) ) ;
#79900 = ORIENTED_EDGE ( 'NONE', *, *, #101502, .F. ) ;
#79899 = LINE ( 'NONE', #24747, #112058 ) ;
#79901 = CARTESIAN_POINT ( 'NONE',  ( -22.49999999999984013, -10.04351517176480257, -1.623559851933875198 ) ) ;
#79902 = VERTEX_POINT ( 'NONE', #142709 ) ;
#79903 = DIRECTION ( 'NONE',  ( -0.000000000000000000, -0.3543493200069152693, 0.9351131265310292928 ) ) ;
#79904 = CARTESIAN_POINT ( 'NONE',  ( 0.000000000000000000, 0.000000000000000000, -10.00000000000000000 ) ) ;
#79905 = PLANE ( 'NONE',  #100220 ) ;
#79906 = CARTESIAN_POINT ( 'NONE',  ( -29.99999999999979039, -21.84840872380826937, 2.849755605029536731 ) ) ;
#79907 = EDGE_LOOP ( 'NONE', ( #4373, #75774, #105996, #97865 ) ) ;
#79908 = EDGE_CURVE ( 'NONE', #110472, #61139, #64427, .T. ) ;
#79909 = VECTOR ( 'NONE', #14948, 1000.000000000000000 ) ;
#79910 = EDGE_CURVE ( 'NONE', #96370, #88116, #133283, .T. ) ;
#79911 = PLANE ( 'NONE',  #11714 ) ;
#79912 = CARTESIAN_POINT ( 'NONE',  ( -5.999999999999963585, -10.06887692260771061, 4.000000000000000000 ) ) ;
#79913 = ORIENTED_EDGE ( 'NONE', *, *, #76948, .F. ) ;
#79915 = ADVANCED_FACE ( 'NONE', ( #132584 ), #582, .F. ) ;
#79914 = LINE ( 'NONE', #4368, #30793 ) ;
#79916 = ORIENTED_EDGE ( 'NONE', *, *, #4547, .T. ) ;
#79917 = CARTESIAN_POINT ( 'NONE',  ( -3.098435806082346922, 11.25929247661560240, 10.79108189686406405 ) ) ;
#79919 = ORIENTED_EDGE ( 'NONE', *, *, #101061, .F. ) ;
#79918 = FACE_OUTER_BOUND ( 'NONE', #109421, .T. ) ;
#79920 = ORIENTED_EDGE ( 'NONE', *, *, #14651, .F. ) ;
#79921 = CARTESIAN_POINT ( 'NONE',  ( 4.600000000000001421, 9.521314400968980422E-16, 0.000000000000000000 ) ) ;
#79922 = VERTEX_POINT ( 'NONE', #120944 ) ;
#79923 = CIRCLE ( 'NONE', #82186, 31.92999999999999261 ) ;
#79924 = VECTOR ( 'NONE', #61855, 1000.000000000000000 ) ;
#79925 = EDGE_LOOP ( 'NONE', ( #113779, #68286, #85888, #105090 ) ) ;
#79926 = VECTOR ( 'NONE', #71645, 1000.000000000000000 ) ;
#79927 = EDGE_CURVE ( 'NONE', #106661, #20647, #109291, .T. ) ;
#79928 = DIRECTION ( 'NONE',  ( -0.6830127018922180770, -0.6830127018922204085, -0.2588190451025213501 ) ) ;
#79929 = DIRECTION ( 'NONE',  ( 0.7071067811865487940, 0.7071067811865463515, 0.000000000000000000 ) ) ;
#79930 =( NAMED_UNIT ( * ) PLANE_ANGLE_UNIT ( ) SI_UNIT ( $, .RADIAN. ) );
#79931 = DIRECTION ( 'NONE',  ( -0.7071067811865486830, -0.7071067811865464625, 0.000000000000000000 ) ) ;
#79932 = CARTESIAN_POINT ( 'NONE',  ( 20.99999999999985789, -9.412538124160656494, 4.000000000000000000 ) ) ;
#79933 = ADVANCED_FACE ( 'NONE', ( #44120 ), #137242, .T. ) ;
#79934 = CARTESIAN_POINT ( 'NONE',  ( 0.000000000000000000, -57.15000000000003411, -15.92500000000064730 ) ) ;
#79935 = ORIENTED_EDGE ( 'NONE', *, *, #67268, .T. ) ;
#79936 = ORIENTED_EDGE ( 'NONE', *, *, #23752, .F. ) ;
#79937 = ORIENTED_EDGE ( 'NONE', *, *, #109752, .F. ) ;
#79938 = CARTESIAN_POINT ( 'NONE',  ( 123.7916666666666714, 3.975000000000003642, -6.884901960086285300 ) ) ;
#79939 = ORIENTED_EDGE ( 'NONE', *, *, #117555, .T. ) ;
#79940 = ORIENTED_EDGE ( 'NONE', *, *, #61035, .F. ) ;
#79941 = VERTEX_POINT ( 'NONE', #66588 ) ;
#79942 = CARTESIAN_POINT ( 'NONE',  ( 0.6293903851252851123, -7.359378872481451950, -1.291302361894904660 ) ) ;
#79943 = LINE ( 'NONE', #34256, #16186 ) ;
#79944 = ORIENTED_EDGE ( 'NONE', *, *, #28176, .T. ) ;
#79945 = LINE ( 'NONE', #56767, #41582 ) ;
#79946 = CARTESIAN_POINT ( 'NONE',  ( 25.40000000000000568, 5.131534016557159461, 4.434051995216958808 ) ) ;
#79947 = DIRECTION ( 'NONE',  ( 0.7071067811865486830, -0.7071067811865464625, -0.000000000000000000 ) ) ;
#79948 = CARTESIAN_POINT ( 'NONE',  ( -23.51078643762690490, -27.52281430457038880, 5.000000000000000000 ) ) ;
#79949 = CARTESIAN_POINT ( 'NONE',  ( 120.1670968585647756, -3.055000000000000160, -5.291415217122921177 ) ) ;
#79950 = ORIENTED_EDGE ( 'NONE', *, *, #55378, .T. ) ;
#79951 = EDGE_CURVE ( 'NONE', #129972, #132519, #22316, .T. ) ;
#79952 = LINE ( 'NONE', #2305, #111205 ) ;
#79953 = CARTESIAN_POINT ( 'NONE',  ( -30.78162688292473348, 21.74787736706806385, 4.999607392498049308 ) ) ;
#79954 = DIRECTION ( 'NONE',  ( -0.3543493200069162685, -0.000000000000000000, -0.9351131265310288487 ) ) ;
#79955 = CARTESIAN_POINT ( 'NONE',  ( -26.99451991528749417, 28.92564299267956685, 4.000000000000000000 ) ) ;
#79956 = FACE_OUTER_BOUND ( 'NONE', #30087, .T. ) ;
#79957 = CARTESIAN_POINT ( 'NONE',  ( 17.47599861414538580, 22.03583458319439359, 4.979811245910084949 ) ) ;
#79958 = PLANE ( 'NONE',  #64326 ) ;
#79959 = CARTESIAN_POINT ( 'NONE',  ( 45.87086038379622721, 6.884901960086289741, -3.974999999999993427 ) ) ;
#79960 = CARTESIAN_POINT ( 'NONE',  ( -34.92500000000001137, -22.22500000000000142, 4.500000000000000888 ) ) ;
#79961 = ADVANCED_FACE ( 'NONE', ( #45576 ), #79444, .T. ) ;
#79962 = FACE_OUTER_BOUND ( 'NONE', #123077, .T. ) ;
#79963 = ORIENTED_EDGE ( 'NONE', *, *, #23127, .F. ) ;
#79964 = ORIENTED_EDGE ( 'NONE', *, *, #59702, .T. ) ;
#79965 = CARTESIAN_POINT ( 'NONE',  ( 42.12499999999999289, -7.950000000000000178, -4.867971026610729436E-16 ) ) ;
#79966 = ORIENTED_EDGE ( 'NONE', *, *, #99136, .T. ) ;
#79967 = B_SPLINE_CURVE_WITH_KNOTS ( 'NONE', 3,
 ( #97380, #98138, #40897, #106846 ),
 .UNSPECIFIED., .F., .F.,
 ( 4, 4 ),
 ( 0.009196836153558695173, 0.009397116448368620506 ),
 .UNSPECIFIED. ) ;
#79968 = DIRECTION ( 'NONE',  ( -0.000000000000000000, 0.3543493200069153248, 0.9351131265310292928 ) ) ;
#79969 = ORIENTED_EDGE ( 'NONE', *, *, #135005, .T. ) ;
#79970 = DIRECTION ( 'NONE',  ( -0.7071067811865486830, 0.7071067811865464625, 0.000000000000000000 ) ) ;
#79971 = ADVANCED_FACE ( 'NONE', ( #92586 ), #123119, .T. ) ;
#79972 = FACE_OUTER_BOUND ( 'NONE', #121389, .T. ) ;
#79973 = EDGE_CURVE ( 'NONE', #72893, #129741, #91887, .T. ) ;
#79974 = CARTESIAN_POINT ( 'NONE',  ( 38.06293019189810423, 1.637169565754157174, 6.110000000000002984 ) ) ;
#79975 = ORIENTED_EDGE ( 'NONE', *, *, #84442, .F. ) ;
#79976 = CARTESIAN_POINT ( 'NONE',  ( -21.48921356237309155, -27.52281430457070499, 5.000000000000000000 ) ) ;
#79977 = EDGE_LOOP ( 'NONE', ( #133250, #87913, #4399, #14570 ) ) ;
#79978 = DIRECTION ( 'NONE',  ( -0.000000000000000000, -0.3543493200069152693, 0.9351131265310292928 ) ) ;
#79979 = CARTESIAN_POINT ( 'NONE',  ( 27.24999999999999645, -9.735942053221458872E-16, 7.950000000000000178 ) ) ;
#79980 = DIRECTION ( 'NONE',  ( -0.6830127018922181881, 0.6830127018922202975, -0.2588190451025214056 ) ) ;
#79981 = CARTESIAN_POINT ( 'NONE',  ( -30.18398860626900060, 28.73617430169808173, 5.000000000000000000 ) ) ;
#79982 = ORIENTED_EDGE ( 'NONE', *, *, #83670, .T. ) ;
#79983 = EDGE_CURVE ( 'NONE', #41151, #105272, #81039, .T. ) ;
#79984 = CARTESIAN_POINT ( 'NONE',  ( 6.066782984417857350, -2.500000000000000000, 3.061616997868383634E-16 ) ) ;
#79985 = VERTEX_POINT ( 'NONE', #12888 ) ;
#79986 = DIRECTION ( 'NONE',  ( 1.000000000000000000, 0.000000000000000000, 0.000000000000000000 ) ) ;
#79987 = LINE ( 'NONE', #44498, #78647 ) ;
#79988 = PLANE ( 'NONE',  #75532 ) ;
#79989 = DIRECTION ( 'NONE',  ( -0.7071067811865486830, -0.7071067811865464625, -0.000000000000000000 ) ) ;
#79990 = FACE_OUTER_BOUND ( 'NONE', #51076, .T. ) ;
#79991 = AXIS2_PLACEMENT_3D ( 'NONE', #130947, #10543, #77983 ) ;
#79992 = DIRECTION ( 'NONE',  ( -1.000000000000000000, -1.224606353822377258E-16, -0.000000000000000000 ) ) ;
#79993 = CARTESIAN_POINT ( 'NONE',  ( 57.07876352523144448, -7.482591942790325086E-16, 6.109999999999998543 ) ) ;
#79994 = VECTOR ( 'NONE', #77996, 1000.000000000000000 ) ;
#79995 = DIRECTION ( 'NONE',  ( 0.7071067811865487940, 0.7071067811865463515, 0.000000000000000000 ) ) ;
#79996 = LINE ( 'NONE', #49510, #6140 ) ;
#79998 = ORIENTED_EDGE ( 'NONE', *, *, #32114, .T. ) ;
#79997 = DIRECTION ( 'NONE',  ( 0.7071067811865487940, -0.7071067811865463515, 0.000000000000000000 ) ) ;
#79999 = EDGE_LOOP ( 'NONE', ( #67986, #7778, #137359, #36334 ) ) ;
#80000 = CARTESIAN_POINT ( 'NONE',  ( 23.99999999999983302, 4.384688058510586295, -7.090945410444628116 ) ) ;
#80001 = ORIENTED_EDGE ( 'NONE', *, *, #125759, .F. ) ;
#80002 = ADVANCED_FACE ( 'NONE', ( #59995 ), #57167, .T. ) ;
#80003 = AXIS2_PLACEMENT_3D ( 'NONE', #55112, #89852, #24602 ) ;
#80004 = CARTESIAN_POINT ( 'NONE',  ( 32.27133846272768380, 22.27000000000000668, -14.68128223927440956 ) ) ;
#80005 = ORIENTED_EDGE ( 'NONE', *, *, #49553, .T. ) ;
#80006 = DIRECTION ( 'NONE',  ( 0.000000000000000000, 1.000000000000000000, 0.000000000000000000 ) ) ;
#80007 = EDGE_CURVE ( 'NONE', #21679, #92143, #68744, .T. ) ;
#80008 = CYLINDRICAL_SURFACE ( 'NONE', #21084, 3.000000000000000000 ) ;
#80009 = FACE_BOUND ( 'NONE', #135794, .T. ) ;
#80010 = DIRECTION ( 'NONE',  ( 0.7071067811865486830, 0.7071067811865463515, 0.000000000000000000 ) ) ;
#80011 = EDGE_CURVE ( 'NONE', #88361, #100840, #68060, .T. ) ;
#80012 = EDGE_CURVE ( 'NONE', #141003, #26697, #78907, .T. ) ;
#80013 = LINE ( 'NONE', #227, #95241 ) ;
#80014 = LINE ( 'NONE', #10410, #59618 ) ;
#80016 = ORIENTED_EDGE ( 'NONE', *, *, #35043, .F. ) ;
#80015 = LINE ( 'NONE', #113296, #94432 ) ;
#80017 = VERTEX_POINT ( 'NONE', #35416 ) ;
#80018 = CARTESIAN_POINT ( 'NONE',  ( 0.000000000000000000, 0.000000000000000000, 5.000000000000000000 ) ) ;
#80019 = VECTOR ( 'NONE', #51408, 1000.000000000000000 ) ;
#80020 = ORIENTED_EDGE ( 'NONE', *, *, #86841, .F. ) ;
#80021 = EDGE_CURVE ( 'NONE', #31148, #96439, #34671, .T. ) ;
#80022 = EDGE_CURVE ( 'NONE', #82135, #8845, #124528, .T. ) ;
#80024 = ORIENTED_EDGE ( 'NONE', *, *, #65344, .T. ) ;
#80023 = AXIS2_PLACEMENT_3D ( 'NONE', #126115, #102933, #39839 ) ;
#80025 = CARTESIAN_POINT ( 'NONE',  ( 77.64126352523146579, 4.472830434245835818, 4.472830434245840259 ) ) ;
#80026 = VERTEX_POINT ( 'NONE', #25196 ) ;
#80027 = EDGE_CURVE ( 'NONE', #106377, #4302, #102060, .T. ) ;
#80028 = AXIS2_PLACEMENT_3D ( 'NONE', #137609, #128165, #28841 ) ;
#80029 = PLANE ( 'NONE',  #69554 ) ;
#80030 = EDGE_CURVE ( 'NONE', #94256, #10011, #36109, .T. ) ;
#80031 = VERTEX_POINT ( 'NONE', #90474 ) ;
#80033 = EDGE_CURVE ( 'NONE', #108713, #88501, #15708, .T. ) ;
#80032 = AXIS2_PLACEMENT_3D ( 'NONE', #29413, #136744, #37460 ) ;
#80034 = FACE_OUTER_BOUND ( 'NONE', #78846, .T. ) ;
#80035 = EDGE_CURVE ( 'NONE', #112402, #33663, #24491, .T. ) ;
#80036 = DIRECTION ( 'NONE',  ( -0.7071067811865486830, -0.7071067811865464625, 0.000000000000000000 ) ) ;
#80037 = CARTESIAN_POINT ( 'NONE',  ( -18.18398860626898994, 28.73617430169800002, 5.000000000000000000 ) ) ;
#80038 = DIRECTION ( 'NONE',  ( 0.6830127018922180770, -0.6830127018922204085, -0.2588190451025213501 ) ) ;
#80039 = CARTESIAN_POINT ( 'NONE',  ( 18.79289321881332242, -17.24070752338410983, 5.000000000000000000 ) ) ;
#80040 = EDGE_LOOP ( 'NONE', ( #133338, #61670, #62997, #79939, #134854, #104909, #83803, #98707, #57333, #18810, #65733, #79582, #11893, #6085, #142726 ) ) ;
#80041 = ORIENTED_EDGE ( 'NONE', *, *, #1876, .F. ) ;
#80042 = CARTESIAN_POINT ( 'NONE',  ( 24.99033360189226016, 3.759292476615681888, 4.478963035907999490 ) ) ;
#80043 = CARTESIAN_POINT ( 'NONE',  ( 45.48921356237309510, -27.52281430457087197, 5.000000000000000000 ) ) ;
#80044 = ORIENTED_EDGE ( 'NONE', *, *, #86927, .T. ) ;
#80045 = EDGE_CURVE ( 'NONE', #137395, #83728, #25931, .T. ) ;
#80046 = ORIENTED_EDGE ( 'NONE', *, *, #118769, .F. ) ;
#80047 = EDGE_LOOP ( 'NONE', ( #59657, #119621, #15735, #20005 ) ) ;
#80048 = APPLICATION_CONTEXT ( 'automotive_design' ) ;
#80049 = CARTESIAN_POINT ( 'NONE',  ( 29.16709685856476497, -3.055000000000000160, -5.291415217122921177 ) ) ;
#80050 = ORIENTED_EDGE ( 'NONE', *, *, #62965, .F. ) ;
#80051 = DIRECTION ( 'NONE',  ( -0.3543493200069162685, -0.000000000000000000, -0.9351131265310288487 ) ) ;
#80052 = ADVANCED_FACE ( 'NONE', ( #80338 ), #69453, .F. ) ;
#80053 = CARTESIAN_POINT ( 'NONE',  ( 45.18398860626900415, 28.73617430169818832, 5.000000000000000000 ) ) ;
#80054 = CARTESIAN_POINT ( 'NONE',  ( 32.12913961620377989, 5.278424836066147208, 3.047499999999990550 ) ) ;
#80055 = CARTESIAN_POINT ( 'NONE',  ( -25.65788372223791569, 22.22500000000000142, 1.488343219358003067 ) ) ;
#80056 = ORIENTED_EDGE ( 'NONE', *, *, #93425, .T. ) ;
#80057 = DIRECTION ( 'NONE',  ( -0.3543493200069162685, -0.000000000000000000, -0.9351131265310288487 ) ) ;
#80058 =( NAMED_UNIT ( * ) SI_UNIT ( $, .STERADIAN. ) SOLID_ANGLE_UNIT ( ) );
#80059 = LINE ( 'NONE', #122076, #133189 ) ;
#80061 = ORIENTED_EDGE ( 'NONE', *, *, #42204, .T. ) ;
#80060 = LINE ( 'NONE', #101042, #132870 ) ;
#80062 = ORIENTED_EDGE ( 'NONE', *, *, #35265, .T. ) ;
#80063 = FACE_OUTER_BOUND ( 'NONE', #16915, .T. ) ;
#80064 = CARTESIAN_POINT ( 'NONE',  ( 11.30840764549667554, 9.139736423841732040E-16, 0.000000000000000000 ) ) ;
#80065 = VERTEX_POINT ( 'NONE', #4102 ) ;
#80066 = FILL_AREA_STYLE ('',( #88784 ) ) ;
#80067 = EDGE_CURVE ( 'NONE', #111354, #37298, #48386, .T. ) ;
#80068 = CARTESIAN_POINT ( 'NONE',  ( -39.18398860626899705, 28.73617430169814568, 5.000000000000000000 ) ) ;
#80069 = EDGE_CURVE ( 'NONE', #22073, #39230, #111784, .T. ) ;
#80070 = FACE_OUTER_BOUND ( 'NONE', #29774, .T. ) ;
#80071 = CARTESIAN_POINT ( 'NONE',  ( 28.41666666666666075, -6.884901960086287076, -3.975000000000000977 ) ) ;
#80072 = CARTESIAN_POINT ( 'NONE',  ( -26.99999999999980460, 20.58746187583902909, 4.000000000000000000 ) ) ;
#80073 = ORIENTED_EDGE ( 'NONE', *, *, #103436, .T. ) ;
#80074 = CARTESIAN_POINT ( 'NONE',  ( 25.39999999999999858, -57.15000000000003411, 15.92499999999935589 ) ) ;
#80075 = DIRECTION ( 'NONE',  ( 0.6830127018922181881, 0.6830127018922202975, -0.2588190451025214056 ) ) ;
#80076 = EDGE_CURVE ( 'NONE', #23783, #127787, #18581, .T. ) ;
#80077 = CARTESIAN_POINT ( 'NONE',  ( 21.33747294953710849, 6.094999999999989981, -1.119633336120465690E-15 ) ) ;
#80078 = DIRECTION ( 'NONE',  ( -0.000000000000000000, 0.000000000000000000, 1.000000000000000000 ) ) ;
#80079 = CARTESIAN_POINT ( 'NONE',  ( -9.707106781186475075, 11.25929247661560773, 5.000000000000000000 ) ) ;
#80080 = VERTEX_POINT ( 'NONE', #71579 ) ;
#80081 = VERTEX_POINT ( 'NONE', #128111 ) ;
#80082 = LINE ( 'NONE', #45312, #118787 ) ;
#80083 = VECTOR ( 'NONE', #108605, 1000.000000000000227 ) ;
#80084 = CARTESIAN_POINT ( 'NONE',  ( -26.34505516254601076, 5.259292476615672562, 12.77922209995887393 ) ) ;
#80085 = LINE ( 'NONE', #124265, #60096 ) ;
#80086 = DIRECTION ( 'NONE',  ( -0.7071067811865486830, -0.7071067811865464625, 0.000000000000000000 ) ) ;
#80087 = CARTESIAN_POINT ( 'NONE',  ( 26.99999999999980815, -13.97847968911258043, -0.1324546996126166887 ) ) ;
#80088 = ORIENTED_EDGE ( 'NONE', *, *, #10443, .T. ) ;
#80089 = EDGE_CURVE ( 'NONE', #127258, #4075, #61453, .T. ) ;
#80090 = PLANE ( 'NONE',  #62726 ) ;
#80091 = DIRECTION ( 'NONE',  ( 0.7071067811865486830, -0.7071067811865464625, -0.000000000000000000 ) ) ;
#80092 = DIRECTION ( 'NONE',  ( 0.6830127018922181881, 0.6830127018922202975, -0.2588190451025214056 ) ) ;
#80093 = CARTESIAN_POINT ( 'NONE',  ( 54.01626352523143737, -4.472830434245839371, 4.472830434245839371 ) ) ;
#80094 =( BOUNDED_CURVE ( )  B_SPLINE_CURVE ( 3, ( #5259, #85681, #127798, #62539 ),
 .UNSPECIFIED., .F., .F. ) 
 B_SPLINE_CURVE_WITH_KNOTS ( ( 4, 4 ),
 ( 1.864375635226932282, 1.933014472006549189 ),
 .UNSPECIFIED. ) 
 CURVE ( )  GEOMETRIC_REPRESENTATION_ITEM ( )  RATIONAL_B_SPLINE_CURVE ( ( 1.000000000000000000, 0.9996074310407763175, 0.9996074310407763175, 1.000000000000000000 ) ) 
 REPRESENTATION_ITEM ( '' )  );
#80095 = DIRECTION ( 'NONE',  ( 0.6830127018922180770, -0.6830127018922204085, -0.2588190451025213501 ) ) ;
#80096 = CARTESIAN_POINT ( 'NONE',  ( -34.49999999999976552, 6.054329344830883031, 4.994342998332166772 ) ) ;
#80097 = CARTESIAN_POINT ( 'NONE',  ( -27.29974487139158512, -27.71228299555225405, 4.000000000000000000 ) ) ;
#80098 = EDGE_CURVE ( 'NONE', #65481, #62418, #16553, .T. ) ;
#80099 = ORIENTED_EDGE ( 'NONE', *, *, #109144, .F. ) ;
#80100 = CARTESIAN_POINT ( 'NONE',  ( 20.99065804761471199, 4.584330080086930965E-16, 0.000000000000000000 ) ) ;
#80101 = ORIENTED_EDGE ( 'NONE', *, *, #27711, .F. ) ;
#80102 = CARTESIAN_POINT ( 'NONE',  ( 11.25346039003969523, 2.055000000000001048, 2.516649172247811554E-16 ) ) ;
#80103 = DIRECTION ( 'NONE',  ( -0.7071067811865487940, 0.7071067811865463515, 0.000000000000000000 ) ) ;
#80104 = LINE ( 'NONE', #67065, #72123 ) ;
#80105 = DIRECTION ( 'NONE',  ( 0.6830127018922181881, 0.6830127018922202975, -0.2588190451025214056 ) ) ;
#80106 = EDGE_CURVE ( 'NONE', #42811, #98176, #104907, .T. ) ;
#80107 = DIRECTION ( 'NONE',  ( -0.7071067811865486830, -0.7071067811865464625, -0.000000000000000000 ) ) ;
#80108 = DIRECTION ( 'NONE',  ( 0.7071067811865487940, -0.7071067811865463515, 0.000000000000000000 ) ) ;
#80109 = VERTEX_POINT ( 'NONE', #51261 ) ;
#80110 = ORIENTED_EDGE ( 'NONE', *, *, #84467, .F. ) ;
#80111 = LINE ( 'NONE', #112011, #115740 ) ;
#80112 = DIRECTION ( 'NONE',  ( 0.000000000000000000, -1.000000000000000000, 0.000000000000000000 ) ) ;
#80113 = CARTESIAN_POINT ( 'NONE',  ( -17.99999999999986855, -15.03360074219758680, 5.000000000000000000 ) ) ;
#80114 = CIRCLE ( 'NONE', #17554, 2.055000000000000604 ) ;
#80115 = CARTESIAN_POINT ( 'NONE',  ( 71.10002705046289861, 5.819803920172570422, 5.819803920172574863 ) ) ;
#80116 = LINE ( 'NONE', #118214, #71805 ) ;
#80117 = ADVANCED_FACE ( 'NONE', ( #138259 ), #19331, .F. ) ;
#80118 = VECTOR ( 'NONE', #66219, 1000.000000000000000 ) ;
#80119 = LINE ( 'NONE', #110542, #62302 ) ;
#80120 = ORIENTED_EDGE ( 'NONE', *, *, #131407, .T. ) ;
#80121 = CARTESIAN_POINT ( 'NONE',  ( 71.43749999999998579, 5.819803920172573974, -5.819803920172572198 ) ) ;
#80122 = AXIS2_PLACEMENT_3D ( 'NONE', #103036, #88610, #22576 ) ;
#80123 = DIRECTION ( 'NONE',  ( 0.7071067811865487940, -0.7071067811865463515, 0.000000000000000000 ) ) ;
#80124 = AXIS2_PLACEMENT_3D ( 'NONE', #39279, #138585, #106627 ) ;
#80125 = CARTESIAN_POINT ( 'NONE',  ( -36.48921356237310221, -27.52281430457080802, 5.000000000000000000 ) ) ;
#80126 = LINE ( 'NONE', #2494, #8036 ) ;
#80127 = AXIS2_PLACEMENT_3D ( 'NONE', #61045, #118192, #117481 ) ;
#80128 = ORIENTED_EDGE ( 'NONE', *, *, #73138, .F. ) ;
#80129 = EDGE_CURVE ( 'NONE', #60169, #94753, #28796, .T. ) ;
#80130 = CARTESIAN_POINT ( 'NONE',  ( -12.98911971346042904, -22.02621442084247505, 4.990779571109221990 ) ) ;
#80131 = EDGE_CURVE ( 'NONE', #58696, #120651, #94019, .T. ) ;
#80132 = DIRECTION ( 'NONE',  ( 1.000000000000000000, 0.000000000000000000, 0.000000000000000000 ) ) ;
#80133 = CARTESIAN_POINT ( 'NONE',  ( 66.20876352523144703, -7.482591942790329030E-16, 6.110000000000001208 ) ) ;
#80134 = CARTESIAN_POINT ( 'NONE',  ( -15.49816348513947339, -17.24070752338410628, 8.407044977365259797 ) ) ;
#80135 = VERTEX_POINT ( 'NONE', #27331 ) ;
#80136 = ORIENTED_EDGE ( 'NONE', *, *, #119766, .T. ) ;
#80137 = LINE ( 'NONE', #124318, #89396 ) ;
#80138 = CARTESIAN_POINT ( 'NONE',  ( 21.18398860626899349, 28.73617430169802134, 5.000000000000000000 ) ) ;
#80139 = CARTESIAN_POINT ( 'NONE',  ( -13.10362284818588741, 2.655808543615126638, 5.000000000000000000 ) ) ;
#80140 = ADVANCED_FACE ( 'NONE', ( #105596 ), #118635, .F. ) ;
#80141 = DIRECTION ( 'NONE',  ( -0.3543493200069162685, -0.000000000000000000, -0.9351131265310288487 ) ) ;
#80143 = VERTEX_POINT ( 'NONE', #39682 ) ;
#80142 = CARTESIAN_POINT ( 'NONE',  ( 86.31249999999998579, 5.819803920172571310, 5.819803920172576639 ) ) ;
#80144 = LINE ( 'NONE', #89553, #34563 ) ;
#80145 = LINE ( 'NONE', #78687, #133292 ) ;
#80146 = DIRECTION ( 'NONE',  ( 0.3543493200069162685, -0.000000000000000000, -0.9351131265310288487 ) ) ;
#80147 = DIRECTION ( 'NONE',  ( 1.000000000000000000, 0.000000000000000000, 0.000000000000000000 ) ) ;
#80148 = ORIENTED_EDGE ( 'NONE', *, *, #47432, .T. ) ;
#80149 = ORIENTED_EDGE ( 'NONE', *, *, #138287, .F. ) ;
#80150 = CARTESIAN_POINT ( 'NONE',  ( 58.47959685856477563, 6.109999999999999432, 1.637169565754164280 ) ) ;
#80151 = ORIENTED_EDGE ( 'NONE', *, *, #79307, .T. ) ;
#80152 = CARTESIAN_POINT ( 'NONE',  ( -30.79289321881324071, 15.75929247661555443, 5.000000000000000000 ) ) ;
#80153 = DIRECTION ( 'NONE',  ( 0.7071067811865486830, -0.7071067811865464625, -0.000000000000000000 ) ) ;
#80154 = DIRECTION ( 'NONE',  ( 0.7071067811865487940, -0.7071067811865463515, 0.000000000000000000 ) ) ;
#80155 = DIRECTION ( 'NONE',  ( 0.7071067811865487940, 0.7071067811865463515, -0.000000000000000000 ) ) ;
#80156 = ORIENTED_EDGE ( 'NONE', *, *, #19301, .T. ) ;
#80157 = ORIENTED_EDGE ( 'NONE', *, *, #105148, .T. ) ;
#80158 = VECTOR ( 'NONE', #5538, 999.9999999999998863 ) ;
#80159 = DIRECTION ( 'NONE',  ( -1.000000000000000000, -1.224606353822377258E-16, -0.000000000000000000 ) ) ;
#80160 = CARTESIAN_POINT ( 'NONE',  ( -19.48942811940429465, -0.003197019174711220046, -31.00987262783852572 ) ) ;
#80161 = ORIENTED_EDGE ( 'NONE', *, *, #61691, .T. ) ;
#80162 = DIRECTION ( 'NONE',  ( 0.000000000000000000, -0.3543493200069152138, 0.9351131265310292928 ) ) ;
#80163 = ORIENTED_EDGE ( 'NONE', *, *, #99421, .T. ) ;
#80164 = EDGE_CURVE ( 'NONE', #63701, #11751, #117187, .T. ) ;
#80165 = LINE ( 'NONE', #121485, #59615 ) ;
#80166 = CARTESIAN_POINT ( 'NONE',  ( 20.66840764549667497, 0.000000000000000000, 2.500000000000001332 ) ) ;
#80167 = EDGE_LOOP ( 'NONE', ( #62037, #9174, #97950, #2944 ) ) ;
#80168 = FACE_BOUND ( 'NONE', #130407, .T. ) ;
#80169 = CARTESIAN_POINT ( 'NONE',  ( 25.17183060077630330, 21.75929247661549937, 4.000000000000000000 ) ) ;
#80170 = ADVANCED_FACE ( 'NONE', ( #83913 ), #16442, .T. ) ;
#80171 = CARTESIAN_POINT ( 'NONE',  ( 0.000000000000000000, 0.000000000000000000, 5.000000000000000000 ) ) ;
#80172 = CARTESIAN_POINT ( 'NONE',  ( 21.18398860626899349, 28.73617430169802134, 5.000000000000000000 ) ) ;
#80173 = DIRECTION ( 'NONE',  ( -0.7071067811865487940, 0.7071067811865463515, 0.000000000000000000 ) ) ;
#80174 = DIRECTION ( 'NONE',  ( 0.7071067811865487940, 0.7071067811865463515, -0.000000000000000000 ) ) ;
#80175 = DIRECTION ( 'NONE',  ( -1.224646799147353207E-16, -2.039446610170337541E-32, -1.000000000000000000 ) ) ;
#80177 = VERTEX_POINT ( 'NONE', #96150 ) ;
#80176 = COLOUR_RGB ( '', 0.66274510, 0.83137255, 0.94901961) ;
#80178 = EDGE_CURVE ( 'NONE', #43125, #46125, #127369, .T. ) ;
#80179 = VERTEX_POINT ( 'NONE', #104162 ) ;
#80180 = CARTESIAN_POINT ( 'NONE',  ( 103.3079301918980946, -6.109999999999998543, 1.637169565754158507 ) ) ;
#80181 = ORIENTED_EDGE ( 'NONE', *, *, #96800, .F. ) ;
#80182 = EDGE_CURVE ( 'NONE', #46696, #22146, #77036, .T. ) ;
#80183 = VECTOR ( 'NONE', #115750, 1000.000000000000227 ) ;
#80184 = LINE ( 'NONE', #137400, #85969 ) ;
#80185 = ORIENTED_EDGE ( 'NONE', *, *, #59143, .F. ) ;
#80186 = EDGE_CURVE ( 'NONE', #141894, #140092, #49131, .T. ) ;
#80187 = DIRECTION ( 'NONE',  ( 0.7071067811865487940, 0.7071067811865463515, 0.000000000000000000 ) ) ;
#80188 = EDGE_CURVE ( 'NONE', #6977, #35122, #93322, .T. ) ;
#80189 = DIRECTION ( 'NONE',  ( -0.7071067811865486830, -0.7071067811865464625, -0.000000000000000000 ) ) ;
#80190 = LINE ( 'NONE', #58469, #61112 ) ;
#80191 = VERTEX_POINT ( 'NONE', #106295 ) ;
#80192 = FACE_OUTER_BOUND ( 'NONE', #20974, .T. ) ;
#80193 = DIRECTION ( 'NONE',  ( 0.000000000000000000, 0.000000000000000000, 1.000000000000000000 ) ) ;
#80195 = EDGE_CURVE ( 'NONE', #10002, #114801, #40395, .T. ) ;
#80194 = CIRCLE ( 'NONE', #17634, 2.055000000000001048 ) ;
#80196 = SURFACE_STYLE_FILL_AREA ( #59167 ) ;
#80197 = CARTESIAN_POINT ( 'NONE',  ( -5.999999999999960032, 10.93112307739207623, 4.000000000000000000 ) ) ;
#80198 = CARTESIAN_POINT ( 'NONE',  ( -8.004924772211888140, -5.240707523384228850, 12.38332538355497903 ) ) ;
#80199 = ORIENTED_EDGE ( 'NONE', *, *, #45766, .F. ) ;
#80200 = DIRECTION ( 'NONE',  ( -0.000000000000000000, 0.3543493200069153248, 0.9351131265310292928 ) ) ;
#80201 = CARTESIAN_POINT ( 'NONE',  ( 19.93618820137057668, -3.269999999999996465, -36.39086428169088094 ) ) ;
#80202 = EDGE_CURVE ( 'NONE', #11599, #33380, #137556, .T. ) ;
#80203 = ORIENTED_EDGE ( 'NONE', *, *, #44696, .F. ) ;
#80205 = ORIENTED_EDGE ( 'NONE', *, *, #99435, .T. ) ;
#80204 = VECTOR ( 'NONE', #56459, 1000.000000000000000 ) ;
#80206 = ADVANCED_FACE ( 'NONE', ( #99738 ), #141845, .F. ) ;
#80207 = ORIENTED_EDGE ( 'NONE', *, *, #113326, .T. ) ;
#80208 = CARTESIAN_POINT ( 'NONE',  ( 56.29209685856477563, -5.291415217122921177, 3.054999999999999272 ) ) ;
#80209 = EDGE_LOOP ( 'NONE', ( #132484, #77359, #39643, #23804 ) ) ;
#80210 = ADVANCED_FACE ( 'NONE', ( #407 ), #10568, .F. ) ;
#80211 = VECTOR ( 'NONE', #48050, 1000.000000000000000 ) ;
#80212 = AXIS2_PLACEMENT_3D ( 'NONE', #11811, #16076, #36455 ) ;
#80213 =( GEOMETRIC_REPRESENTATION_CONTEXT ( 3 ) GLOBAL_UNCERTAINTY_ASSIGNED_CONTEXT ( ( #82246 ) ) GLOBAL_UNIT_ASSIGNED_CONTEXT ( ( #95802, #19668, #10902 ) ) REPRESENTATION_CONTEXT ( 'NONE', 'WORKASPACE' ) );
#80214 = CARTESIAN_POINT ( 'NONE',  ( 9.379139616203772789, -5.278424836066145431, -3.047499999999993658 ) ) ;
#80215 = CARTESIAN_POINT ( 'NONE',  ( 89.39626352523144703, 4.472830434245840259, -4.472830434245838482 ) ) ;
#80216 = CARTESIAN_POINT ( 'NONE',  ( 4.171830600776445408, -14.24070752338413470, 4.000000000000000000 ) ) ;
#80217 = ORIENTED_EDGE ( 'NONE', *, *, #74764, .F. ) ;
#80218 = DIRECTION ( 'NONE',  ( -0.7071067811865486830, -0.7071067811865464625, 0.000000000000000000 ) ) ;
#80219 = ORIENTED_EDGE ( 'NONE', *, *, #43514, .T. ) ;
#80220 = FILL_AREA_STYLE ('',( #59189 ) ) ;
#80221 = AXIS2_PLACEMENT_3D ( 'NONE', #141219, #76724, #133239 ) ;
#80222 = CARTESIAN_POINT ( 'NONE',  ( -33.33010218547244108, 17.25929247661554555, 19.83885114516079184 ) ) ;
#80223 = ORIENTED_EDGE ( 'NONE', *, *, #139126, .F. ) ;
#80224 = CARTESIAN_POINT ( 'NONE',  ( -7.499999999999944045, 13.46639925780212366, 5.000000000000000000 ) ) ;
#80225 = LINE ( 'NONE', #114919, #2025 ) ;
#80226 = CARTESIAN_POINT ( 'NONE',  ( 125.3287635252314516, 0.000000000000000000, -6.109999999999999432 ) ) ;
#80227 = VERTEX_POINT ( 'NONE', #64268 ) ;
#80228 = PLANE ( 'NONE',  #101267 ) ;
#80229 = ORIENTED_EDGE ( 'NONE', *, *, #69846, .T. ) ;
#80230 = ORIENTED_EDGE ( 'NONE', *, *, #55281, .T. ) ;
#80231 = VERTEX_POINT ( 'NONE', #99013 ) ;
#80232 = EDGE_CURVE ( 'NONE', #60276, #73694, #43945, .T. ) ;
#80233 = DIRECTION ( 'NONE',  ( -0.7071067811865487940, 0.7071067811865463515, 0.000000000000000000 ) ) ;
#80234 = CARTESIAN_POINT ( 'NONE',  ( -5.999999999999952927, 14.96639925780211478, 5.000000000000000000 ) ) ;
#80235 = DIRECTION ( 'NONE',  ( -0.6830127018922181881, 0.6830127018922202975, -0.2588190451025214056 ) ) ;
#80236 = DIRECTION ( 'NONE',  ( -1.000000000000000000, -1.224606353822377258E-16, -0.000000000000000000 ) ) ;
#80237 = ORIENTED_EDGE ( 'NONE', *, *, #43304, .F. ) ;
#80238 = EDGE_CURVE ( 'NONE', #82756, #74817, #97588, .T. ) ;
#80239 = CARTESIAN_POINT ( 'NONE',  ( 23.45790314143522437, 6.871911579029515771, 3.967499999999989146 ) ) ;
#80240 = CARTESIAN_POINT ( 'NONE',  ( -19.49999999999986855, -12.66682484999668112, -0.6294897503864391730 ) ) ;
#80241 = AXIS2_PLACEMENT_3D ( 'NONE', #136894, #72400, #113713 ) ;
#80242 = CARTESIAN_POINT ( 'NONE',  ( 0.000000000000000000, -57.14999999999999147, -34.92499999999972715 ) ) ;
#80243 =( BOUNDED_CURVE ( )  B_SPLINE_CURVE ( 2, ( #91744, #57019, #101193, #135970, #36646, #1831, #90318, #12744, #59851, #112097, #3967, #57722, #25051 ),
 .UNSPECIFIED., .F., .T. ) 
 B_SPLINE_CURVE_WITH_KNOTS ( ( 3, 2, 2, 2, 2, 2, 3 ),
 ( 0.5500000000000000444, 0.5527777777777778123, 0.5555555555555555802, 0.5583333333333333481, 0.5611111111111111160, 0.5638888888888888840, 0.5666666666666666519 ),
 .UNSPECIFIED. ) 
 CURVE ( )  GEOMETRIC_REPRESENTATION_ITEM ( )  RATIONAL_B_SPLINE_CURVE ( ( 1.000000000000000000, 0.9659258262890683122, 1.000000000000000000, 0.9659258262890683122, 1.000000000000000000, 0.9659258262890683122, 1.000000000000000000, 0.9659258262890683122, 1.000000000000000000, 0.9659258262890683122, 1.000000000000000000, 0.9659258262890683122, 1.000000000000000000 ) ) 
 REPRESENTATION_ITEM ( '' )  );
#80244 = FACE_OUTER_BOUND ( 'NONE', #34165, .T. ) ;
#80245 = VERTEX_POINT ( 'NONE', #66421 ) ;
#80246 = ORIENTED_EDGE ( 'NONE', *, *, #121943, .T. ) ;
#80247 = EDGE_CURVE ( 'NONE', #120012, #91787, #45401, .T. ) ;
#80248 = ORIENTED_EDGE ( 'NONE', *, *, #136312, .F. ) ;
#80249 = CARTESIAN_POINT ( 'NONE',  ( -12.70000000000000284, -34.64999999999999147, -40.00000000000000000 ) ) ;
#80250 = PLANE ( 'NONE',  #71911 ) ;
#80251 = VECTOR ( 'NONE', #40024, 999.9999999999998863 ) ;
#80252 = DIRECTION ( 'NONE',  ( -1.000000000000000000, -0.000000000000000000, -0.000000000000000000 ) ) ;
#80253 = CARTESIAN_POINT ( 'NONE',  ( -14.99451991528749595, 28.92564299267948513, 4.000000000000000000 ) ) ;
#80254 = CARTESIAN_POINT ( 'NONE',  ( 9.278254515685670611, 8.259292476615634371, 11.78515199841152850 ) ) ;
#80255 = FACE_OUTER_BOUND ( 'NONE', #37712, .T. ) ;
#80256 = DIRECTION ( 'NONE',  ( -1.000000000000000000, -1.224606353822377258E-16, -0.000000000000000000 ) ) ;
#80257 = ADVANCED_FACE ( 'NONE', ( #107746 ), #121486, .F. ) ;
#80258 = PLANE ( 'NONE',  #141284 ) ;
#80259 = CARTESIAN_POINT ( 'NONE',  ( 18.18398860626898994, 28.73617430169800002, 5.000000000000000000 ) ) ;
#80260 = CARTESIAN_POINT ( 'NONE',  ( 34.42499999999998295, 21.72500000000000142, 5.000000000000000000 ) ) ;
#80261 = VECTOR ( 'NONE', #142485, 999.9999999999998863 ) ;
#80262 = ORIENTED_EDGE ( 'NONE', *, *, #50050, .T. ) ;
#80263 = VERTEX_POINT ( 'NONE', #132420 ) ;
#80264 = DIRECTION ( 'NONE',  ( -0.7071067811865486830, -0.7071067811865464625, 0.000000000000000000 ) ) ;
#80266 = ORIENTED_EDGE ( 'NONE', *, *, #119211, .F. ) ;
#80265 = CARTESIAN_POINT ( 'NONE',  ( 12.48921356237309155, -27.52281430457064104, 5.000000000000000000 ) ) ;
#80267 = ADVANCED_FACE ( 'NONE', ( #98333 ), #65001, .F. ) ;
#80268 = CARTESIAN_POINT ( 'NONE',  ( -26.20710678118636139, 18.75929247661552068, 5.000000000000000000 ) ) ;
#80269 = EDGE_CURVE ( 'NONE', #126646, #59525, #88897, .T. ) ;
#80270 = VERTEX_POINT ( 'NONE', #119332 ) ;
#80271 = FACE_OUTER_BOUND ( 'NONE', #113861, .T. ) ;
#80272 = ORIENTED_EDGE ( 'NONE', *, *, #123807, .F. ) ;
#80273 = LINE ( 'NONE', #123773, #125385 ) ;
#80274 = ORIENTED_EDGE ( 'NONE', *, *, #68569, .F. ) ;
#80275 =( BOUNDED_CURVE ( )  B_SPLINE_CURVE ( 2, ( #43316, #20101, #141172, #76676, #41886, #86101, #31020, #8483, #119405, #18667, #87525, #64346, #131753 ),
 .UNSPECIFIED., .F., .F. ) 
 B_SPLINE_CURVE_WITH_KNOTS ( ( 3, 2, 2, 2, 2, 2, 3 ),
 ( 0.8333333333333334814, 0.8361111111111112493, 0.8388888888888890172, 0.8416666666666667851, 0.8444444444444445530, 0.8472222222222223209, 0.8500000000000000888 ),
 .UNSPECIFIED. ) 
 CURVE ( )  GEOMETRIC_REPRESENTATION_ITEM ( )  RATIONAL_B_SPLINE_CURVE ( ( 0.9999999999999986677, 0.9659258262890696445, 1.000000000000000000, 0.9659258262890683122, 1.000000000000000000, 0.9659258262890683122, 1.000000000000000000, 0.9659258262890683122, 1.000000000000000000, 0.9659258262890683122, 1.000000000000000000, 0.9659258262890669799, 1.000000000000001332 ) ) 
 REPRESENTATION_ITEM ( '' )  );
#80276 = CARTESIAN_POINT ( 'NONE',  ( 45.18398860626900415, 28.73617430169818832, 5.000000000000000000 ) ) ;
#80277 = AXIS2_PLACEMENT_3D ( 'NONE', #77856, #56859, #110448 ) ;
#80278 = CARTESIAN_POINT ( 'NONE',  ( 100.2666937171295842, -7.949999999999999289, 2.130196079827424427 ) ) ;
#80279 = CARTESIAN_POINT ( 'NONE',  ( 42.18398860626899705, 28.73617430169816700, 5.000000000000000000 ) ) ;
#80280 = CARTESIAN_POINT ( 'NONE',  ( 13.19018167574440348, -18.74070752338408852, 7.910009926591477836 ) ) ;
#80281 = VERTEX_POINT ( 'NONE', #21480 ) ;
#80282 = VECTOR ( 'NONE', #89580, 1000.000000000000000 ) ;
#80283 = DIRECTION ( 'NONE',  ( 0.6830127018922181881, 0.6830127018922202975, -0.2588190451025214056 ) ) ;
#80284 = DIRECTION ( 'NONE',  ( -0.7071067811865486830, -0.7071067811865464625, 0.000000000000000000 ) ) ;
#80285 = DIRECTION ( 'NONE',  ( -0.000000000000000000, 0.3543493200069153248, 0.9351131265310292928 ) ) ;
#80286 = CARTESIAN_POINT ( 'NONE',  ( 13.56250000000000000, 4.461849672132300881, 4.461849672132299105 ) ) ;
#80287 = CARTESIAN_POINT ( 'NONE',  ( 21.99956980810188867, -3.967499999999998028, -6.871911579029511330 ) ) ;
#80288 = LINE ( 'NONE', #25150, #10723 ) ;
#80289 = ORIENTED_EDGE ( 'NONE', *, *, #13381, .F. ) ;
#80290 = EDGE_CURVE ( 'NONE', #113241, #67529, #130968, .T. ) ;
#80291 = PLANE ( 'NONE',  #39824 ) ;
#80292 = ORIENTED_EDGE ( 'NONE', *, *, #109651, .T. ) ;
#80293 = EDGE_CURVE ( 'NONE', #49354, #51668, #9872, .T. ) ;
#80294 = AXIS2_PLACEMENT_3D ( 'NONE', #142575, #42564, #63605 ) ;
#80295 = CARTESIAN_POINT ( 'NONE',  ( 96.68793019189811844, 6.110000000000002984, -1.637169565754156730 ) ) ;
#80296 = DIRECTION ( 'NONE',  ( -0.7071067811865486830, -0.7071067811865464625, 0.000000000000000000 ) ) ;
#80297 = CARTESIAN_POINT ( 'NONE',  ( 8.999999999999944933, -7.447814304570754551, 5.000000000000000000 ) ) ;
#80298 = LINE ( 'NONE', #33926, #72431 ) ;
#80299 = CARTESIAN_POINT ( 'NONE',  ( -10.03340032343016652, 6.759292476615645917, 12.28218704918519855 ) ) ;
#80300 = VERTEX_POINT ( 'NONE', #130254 ) ;
#80301 = CARTESIAN_POINT ( 'NONE',  ( 53.99451991528749062, 28.92564299267975869, 4.000000000000000000 ) ) ;
#80302 = CARTESIAN_POINT ( 'NONE',  ( 8.999999999999937828, 20.96639925780204905, 5.000000000000000000 ) ) ;
#80303 = EDGE_CURVE ( 'NONE', #17021, #10403, #142554, .T. ) ;
#80304 = CONICAL_SURFACE ( 'NONE', #45544, 2.500000000000000888, 0.9599310885968822538 ) ;
#80305 = ORIENTED_EDGE ( 'NONE', *, *, #86515, .F. ) ;
#80306 = CARTESIAN_POINT ( 'NONE',  ( 48.48921356237309510, -27.52281430457089328, 5.000000000000000000 ) ) ;
#80307 = ADVANCED_FACE ( 'NONE', ( #86013 ), #95513, .T. ) ;
#80308 = DIRECTION ( 'NONE',  ( 0.000000000000000000, 0.000000000000000000, -1.000000000000000000 ) ) ;
#80310 = EDGE_LOOP ( 'NONE', ( #11076, #134157, #14289, #93867 ) ) ;
#80309 = CARTESIAN_POINT ( 'NONE',  ( -30.85181644961836867, 17.25929247661554200, 8.802941693769131604 ) ) ;
#80311 = LINE ( 'NONE', #98638, #108501 ) ;
#80312 = CARTESIAN_POINT ( 'NONE',  ( 102.8916937171295416, 2.130196079827421762, 7.950000000000000178 ) ) ;
#80313 = DIRECTION ( 'NONE',  ( -0.6830127018922181881, 0.6830127018922202975, -0.2588190451025214056 ) ) ;
#80314 = CARTESIAN_POINT ( 'NONE',  ( -50.99451991528749062, 28.92564299267973738, 4.000000000000000000 ) ) ;
#80315 = AXIS2_PLACEMENT_3D ( 'NONE', #94375, #50895, #96488 ) ;
#80316 = CARTESIAN_POINT ( 'NONE',  ( -3.183988606268992161, 28.73617430169789699, 5.000000000000000000 ) ) ;
#80317 = VECTOR ( 'NONE', #8069, 1000.000000000000000 ) ;
#80318 = ORIENTED_EDGE ( 'NONE', *, *, #50133, .F. ) ;
#80319 = VERTEX_POINT ( 'NONE', #96848 ) ;
#80320 = VERTEX_POINT ( 'NONE', #22160 ) ;
#80321 = VECTOR ( 'NONE', #112893, 1000.000000000000000 ) ;
#80322 = CARTESIAN_POINT ( 'NONE',  ( 80.79209685856477563, -5.291415217122921177, 3.054999999999999272 ) ) ;
#80323 = ORIENTED_EDGE ( 'NONE', *, *, #83126, .T. ) ;
#80324 = FACE_OUTER_BOUND ( 'NONE', #17372, .T. ) ;
#80325 = CARTESIAN_POINT ( 'NONE',  ( -2.816011393730999401, 28.73617430169785436, 5.000000000000000000 ) ) ;
#80327 = AXIS2_PLACEMENT_3D ( 'NONE', #99511, #115370, #14679 ) ;
#80326 = LINE ( 'NONE', #34661, #129018 ) ;
#80328 = DIRECTION ( 'NONE',  ( 0.7071067811865487940, 0.7071067811865463515, 0.000000000000000000 ) ) ;
#80329 = VERTEX_POINT ( 'NONE', #9110 ) ;
#80330 = ADVANCED_FACE ( 'NONE', ( #76598 ), #55541, .F. ) ;
#80331 = CARTESIAN_POINT ( 'NONE',  ( 14.09068777029287567, 6.496774105546209377, 4.000000000000000000 ) ) ;
#80332 = DIRECTION ( 'NONE',  ( 0.7071067811865487940, -0.7071067811865463515, 0.000000000000000000 ) ) ;
#80333 = CARTESIAN_POINT ( 'NONE',  ( 27.70701326429285061, -21.74070752338406365, 4.999753212805213565 ) ) ;
#80334 = CARTESIAN_POINT ( 'NONE',  ( 75.45376352523145158, -6.109999999999998543, -3.741295971395162543E-16 ) ) ;
#80335 = EDGE_LOOP ( 'NONE', ( #4976, #79658, #143049, #14186 ) ) ;
#80336 = FACE_OUTER_BOUND ( 'NONE', #118203, .T. ) ;
#80337 = CARTESIAN_POINT ( 'NONE',  ( -34.42500000000001137, -9.022814304570477617, 5.000000000000000000 ) ) ;
#80338 = FACE_OUTER_BOUND ( 'NONE', #29270, .T. ) ;
#80339 = VERTEX_POINT ( 'NONE', #23608 ) ;
#80340 = EDGE_LOOP ( 'NONE', ( #68973, #24151, #136699 ) ) ;
#80341 = DIRECTION ( 'NONE',  ( 0.6830127018922180770, -0.6830127018922204085, -0.2588190451025213501 ) ) ;
#80342 = DIRECTION ( 'NONE',  ( 0.3543493200069162685, -0.000000000000000000, -0.9351131265310288487 ) ) ;
#80343 = DIRECTION ( 'NONE',  ( 0.7071067811865487940, 0.7071067811865463515, -0.000000000000000000 ) ) ;
#80344 = VECTOR ( 'NONE', #18096, 1000.000000000000227 ) ;
#80345 = CARTESIAN_POINT ( 'NONE',  ( 57.48921356237308800, -27.52281430457095368, 5.000000000000000000 ) ) ;
#80346 = CARTESIAN_POINT ( 'NONE',  ( -30.32816939922332367, -3.740707523384244837, 4.000000000000000000 ) ) ;
#80347 = ADVANCED_FACE ( 'NONE', ( #100473 ), #34493, .T. ) ;
#80348 = VECTOR ( 'NONE', #81579, 1000.000000000000227 ) ;
#80349 = ORIENTED_EDGE ( 'NONE', *, *, #89352, .T. ) ;
#80350 = ORIENTED_EDGE ( 'NONE', *, *, #5057, .T. ) ;
#80351 = EDGE_CURVE ( 'NONE', #62423, #116876, #37355, .T. ) ;
#80352 = FACE_OUTER_BOUND ( 'NONE', #17694, .T. ) ;
#80353 = VERTEX_POINT ( 'NONE', #46852 ) ;
#80354 = ORIENTED_EDGE ( 'NONE', *, *, #8912, .F. ) ;
#80355 = CIRCLE ( 'NONE', #140540, 5.968999999999998529 ) ;
#80356 = EDGE_CURVE ( 'NONE', #20015, #61417, #135938, .T. ) ;
#80357 = EDGE_CURVE ( 'NONE', #94939, #93121, #35234, .T. ) ;
#80358 = LINE ( 'NONE', #25951, #105325 ) ;
#80359 = ORIENTED_EDGE ( 'NONE', *, *, #97317, .F. ) ;
#80360 = DIRECTION ( 'NONE',  ( 0.7071067811865486830, -0.7071067811865464625, -0.000000000000000000 ) ) ;
#80361 = CARTESIAN_POINT ( 'NONE',  ( 59.99451991528749772, 28.92564299267980132, 4.000000000000000000 ) ) ;
#80362 = AXIS2_PLACEMENT_3D ( 'NONE', #100228, #876, #69775 ) ;
#80363 = DIRECTION ( 'NONE',  ( 0.3543493200069162685, -0.000000000000000000, -0.9351131265310288487 ) ) ;
#80364 = CARTESIAN_POINT ( 'NONE',  ( 5.510786437626906675, -27.52281430457051314, 5.000000000000000000 ) ) ;
#80365 = ORIENTED_EDGE ( 'NONE', *, *, #83240, .T. ) ;
#80366 = LINE ( 'NONE', #123865, #27884 ) ;
#80367 = EDGE_CURVE ( 'NONE', #53073, #128957, #80869, .T. ) ;
#80369 = EDGE_LOOP ( 'NONE', ( #51823, #71229, #10442, #36615 ) ) ;
#80368 = VECTOR ( 'NONE', #50914, 1000.000000000000000 ) ;
#80370 = FACE_OUTER_BOUND ( 'NONE', #95029, .T. ) ;
#80371 = EDGE_LOOP ( 'NONE', ( #107777, #83595, #129372, #46969 ) ) ;
#80372 = ADVANCED_FACE ( 'NONE', ( #45400 ), #14867, .F. ) ;
#80373 = ORIENTED_EDGE ( 'NONE', *, *, #57092, .F. ) ;
#80374 = CARTESIAN_POINT ( 'NONE',  ( -39.29974487139159578, -27.71228299555233576, 4.000000000000000000 ) ) ;
#80375 = ORIENTED_EDGE ( 'NONE', *, *, #33517, .T. ) ;
#80376 = ORIENTED_EDGE ( 'NONE', *, *, #65723, .T. ) ;
#80377 = CARTESIAN_POINT ( 'NONE',  ( 19.49999999999986500, 15.05218569542901541, 5.000000000000000000 ) ) ;
#80378 = ORIENTED_EDGE ( 'NONE', *, *, #131895, .F. ) ;
#80379 = EDGE_CURVE ( 'NONE', #49858, #13267, #68572, .T. ) ;
#80380 = DIRECTION ( 'NONE',  ( -0.3543493200069162685, -0.000000000000000000, -0.9351131265310288487 ) ) ;
#80381 = DIRECTION ( 'NONE',  ( 0.7071067811865486830, -0.7071067811865464625, -0.000000000000000000 ) ) ;
#80382 = AXIS2_PLACEMENT_3D ( 'NONE', #84449, #114189, #17029 ) ;
#80383 = CARTESIAN_POINT ( 'NONE',  ( 120.8962635252314470, 4.472830434245840259, -4.472830434245838482 ) ) ;
#80384 = DIRECTION ( 'NONE',  ( 0.000000000000000000, -1.000000000000000000, 0.000000000000000000 ) ) ;
#80385 = CARTESIAN_POINT ( 'NONE',  ( 24.66331758004193375, 1.142935889642021863, 4.329525704382053419 ) ) ;
#80386 = CARTESIAN_POINT ( 'NONE',  ( -47.99451991528749062, 28.92564299267971251, 4.000000000000000000 ) ) ;
#80387 = ADVANCED_FACE ( 'NONE', ( #114183 ), #1806, .T. ) ;
#80388 = LINE ( 'NONE', #81091, #5327 ) ;
#80389 = LINE ( 'NONE', #126022, #43669 ) ;
#80390 = ORIENTED_EDGE ( 'NONE', *, *, #24189, .F. ) ;
#80391 = PLANE ( 'NONE',  #66616 ) ;
#80392 = ORIENTED_EDGE ( 'NONE', *, *, #24266, .F. ) ;
#80393 = ORIENTED_EDGE ( 'NONE', *, *, #48883, .F. ) ;
#80394 = EDGE_CURVE ( 'NONE', #1058, #131599, #67879, .T. ) ;
#80395 = DIRECTION ( 'NONE',  ( -0.000000000000000000, -0.3543493200069152693, 0.9351131265310292928 ) ) ;
#80396 = VERTEX_POINT ( 'NONE', #3269 ) ;
#80397 = CARTESIAN_POINT ( 'NONE',  ( -19.49999999999986500, 15.43112307739202826, 4.000000000000000000 ) ) ;
#80398 = CARTESIAN_POINT ( 'NONE',  ( 113.2916666666666714, 3.975000000000003642, -6.884901960086285300 ) ) ;
#80399 = LINE ( 'NONE', #4166, #136637 ) ;
#80400 = CARTESIAN_POINT ( 'NONE',  ( 24.87999999999999901, 2.055000000000001492, 0.000000000000000000 ) ) ;
#80401 = EDGE_CURVE ( 'NONE', #131572, #60798, #3944, .T. ) ;
#80402 = ORIENTED_EDGE ( 'NONE', *, *, #38960, .T. ) ;
#80403 = LINE ( 'NONE', #36861, #127395 ) ;
#80404 = ORIENTED_EDGE ( 'NONE', *, *, #111131, .T. ) ;
#80405 = VECTOR ( 'NONE', #22860, 999.9999999999998863 ) ;
#80407 = CARTESIAN_POINT ( 'NONE',  ( 5.510786437626906675, -27.52281430457051314, 5.000000000000000000 ) ) ;
#80406 = VECTOR ( 'NONE', #69472, 1000.000000000000000 ) ;
#80408 = ADVANCED_FACE ( 'NONE', ( #24326 ), #124354, .F. ) ;
#80409 = PRESENTATION_LAYER_ASSIGNMENT (  '', '', ( #133687 ) ) ;
#80410 = CARTESIAN_POINT ( 'NONE',  ( 31.56706980810188767, 2.126176841940952134, -7.934999999999993392 ) ) ;
#80411 = ORIENTED_EDGE ( 'NONE', *, *, #89215, .T. ) ;
#80412 = CARTESIAN_POINT ( 'NONE',  ( 9.279999999999999361, 9.521314400968980422E-16, 0.000000000000000000 ) ) ;
#80413 = DIRECTION ( 'NONE',  ( -0.7071067811865486830, -0.7071067811865464625, 0.000000000000000000 ) ) ;
#80414 = VERTEX_POINT ( 'NONE', #90283 ) ;
#80415 = EDGE_LOOP ( 'NONE', ( #13838, #32242, #69858, #3368 ) ) ;
#80416 = ORIENTED_EDGE ( 'NONE', *, *, #105471, .F. ) ;
#80417 = LINE ( 'NONE', #102871, #51876 ) ;
#80418 = PLANE ( 'NONE',  #118088 ) ;
#80419 = VECTOR ( 'NONE', #67667, 1000.000000000000227 ) ;
#80420 = LINE ( 'NONE', #68835, #28866 ) ;
#80421 = DIRECTION ( 'NONE',  ( -0.6830127018922180770, -0.6830127018922204085, -0.2588190451025213501 ) ) ;
#80422 = ORIENTED_EDGE ( 'NONE', *, *, #94440, .F. ) ;
#80423 = DIRECTION ( 'NONE',  ( 0.3543493200069162685, -0.000000000000000000, -0.9351131265310288487 ) ) ;
#80424 = DIRECTION ( 'NONE',  ( 0.000000000000000000, -1.000000000000000000, 0.000000000000000000 ) ) ;
#80425 = ADVANCED_FACE ( 'NONE', ( #12004 ), #113457, .F. ) ;
#80426 = CARTESIAN_POINT ( 'NONE',  ( -1.499999999999987566, -10.04351517176478659, -1.623559851933826570 ) ) ;
#80427 = DIRECTION ( 'NONE',  ( -0.000000000000000000, 0.000000000000000000, 1.000000000000000000 ) ) ;
#80428 = ORIENTED_EDGE ( 'NONE', *, *, #111131, .F. ) ;
#80429 = CARTESIAN_POINT ( 'NONE',  ( 10.49999999999993072, -7.912538124160676922, 4.000000000000000000 ) ) ;
#80430 = VERTEX_POINT ( 'NONE', #56292 ) ;
#80432 = EDGE_LOOP ( 'NONE', ( #72913, #132220, #5508, #96726 ) ) ;
#80431 = CARTESIAN_POINT ( 'NONE',  ( 56.52198303709688787, -46.44627868284322858, -35.89947574910193850 ) ) ;
#80433 = ORIENTED_EDGE ( 'NONE', *, *, #25782, .F. ) ;
#80434 = EDGE_CURVE ( 'NONE', #65772, #17436, #35949, .T. ) ;
#80435 = CARTESIAN_POINT ( 'NONE',  ( 7.499999999999954703, 19.46639925780207037, 5.000000000000000000 ) ) ;
#80437 = AXIS2_PLACEMENT_3D ( 'NONE', #43121, #77193, #86632 ) ;
#80436 = LINE ( 'NONE', #27434, #34447 ) ;
#80438 = ORIENTED_EDGE ( 'NONE', *, *, #94300, .T. ) ;
#80439 = LINE ( 'NONE', #23905, #11937 ) ;
#80440 = ORIENTED_EDGE ( 'NONE', *, *, #39785, .T. ) ;
#80441 = DIRECTION ( 'NONE',  ( 1.000000000000000000, 0.000000000000000000, 0.000000000000000000 ) ) ;
#80442 = DIRECTION ( 'NONE',  ( -0.7071067811865486830, -0.7071067811865464625, 0.000000000000000000 ) ) ;
#80443 = VECTOR ( 'NONE', #78273, 1000.000000000000000 ) ;
#80444 = DIRECTION ( 'NONE',  ( -0.7071067811865486830, -0.7071067811865464625, 0.000000000000000000 ) ) ;
#80445 = CARTESIAN_POINT ( 'NONE',  ( -8.816011393731004731, 28.73617430169781173, 5.000000000000000000 ) ) ;
#80446 = DIRECTION ( 'NONE',  ( 0.6830127018922180770, -0.6830127018922204085, -0.2588190451025213501 ) ) ;
#80448 = EDGE_CURVE ( 'NONE', #84277, #76846, #35236, .T. ) ;
#80447 = CARTESIAN_POINT ( 'NONE',  ( -42.18398860626899705, 28.73617430169816700, 5.000000000000000000 ) ) ;
#80449 = DIRECTION ( 'NONE',  ( -0.7071067811865486830, 0.7071067811865464625, 0.000000000000000000 ) ) ;
#80450 = CARTESIAN_POINT ( 'NONE',  ( 23.20666063542136115, 21.75929247661548871, 4.998822639870701856 ) ) ;
#80451 = CARTESIAN_POINT ( 'NONE',  ( 25.35373647476855297, -5.808823158059035485, -5.808823158059033709 ) ) ;
#80453 = VECTOR ( 'NONE', #125951, 1000.000000000000000 ) ;
#80452 = CARTESIAN_POINT ( 'NONE',  ( -0.2997448713915885632, -27.71228299555206220, 4.000000000000000000 ) ) ;
#80454 = FACE_OUTER_BOUND ( 'NONE', #27333, .T. ) ;
#80455 = CARTESIAN_POINT ( 'NONE',  ( -17.69668852761918032, -22.22500000000000142, 11.52845124498734464 ) ) ;
#80456 = PLANE ( 'NONE',  #68733 ) ;
#80457 = VERTEX_POINT ( 'NONE', #80166 ) ;
#80458 = VERTEX_POINT ( 'NONE', #12721 ) ;
#80459 = CARTESIAN_POINT ( 'NONE',  ( 89.95833333333332860, 3.974999999999997424, 6.884901960086288852 ) ) ;
#80460 = ORIENTED_EDGE ( 'NONE', *, *, #139424, .T. ) ;
#80461 = EDGE_LOOP ( 'NONE', ( #81708, #121631, #5172, #30462 ) ) ;
#80462 = ADVANCED_FACE ( 'NONE', ( #14149 ), #102621, .F. ) ;
#80463 = ORIENTED_EDGE ( 'NONE', *, *, #114572, .T. ) ;
#80464 = VECTOR ( 'NONE', #66028, 1000.000000000000000 ) ;
#80465 = DIRECTION ( 'NONE',  ( 0.6830127018922180770, -0.6830127018922204085, -0.2588190451025213501 ) ) ;
#80466 = DIRECTION ( 'NONE',  ( 0.7071067811865487940, -0.7071067811865463515, 0.000000000000000000 ) ) ;
#80467 = CARTESIAN_POINT ( 'NONE',  ( 14.67146220324653250, 9.486753480112833259, 0.5775628020821772513 ) ) ;
#80468 = ORIENTED_EDGE ( 'NONE', *, *, #140418, .T. ) ;
#80469 = DIRECTION ( 'NONE',  ( 1.000000000000000000, 0.000000000000000000, 0.000000000000000000 ) ) ;
#80470 = CARTESIAN_POINT ( 'NONE',  ( -35.99451991528749772, 28.92564299267963079, 4.000000000000000000 ) ) ;
#80471 = CARTESIAN_POINT ( 'NONE',  ( -30.48921356237309510, -27.52281430457076894, 5.000000000000000000 ) ) ;
#80472 = LINE ( 'NONE', #59445, #104425 ) ;
#80473 = EDGE_CURVE ( 'NONE', #142250, #123516, #49681, .T. ) ;
#80474 = CARTESIAN_POINT ( 'NONE',  ( 126.9329301918981088, 1.637169565754156508, 6.110000000000000320 ) ) ;
#80475 = EDGE_CURVE ( 'NONE', #26874, #81201, #26471, .T. ) ;
#80476 = DIRECTION ( 'NONE',  ( 0.7071067811865486830, -0.7071067811865464625, -0.000000000000000000 ) ) ;
#80477 = CARTESIAN_POINT ( 'NONE',  ( -23.99999999999983302, -5.527737879153217015, -7.983877177622316523 ) ) ;
#80478 = LINE ( 'NONE', #79072, #24397 ) ;
#80479 = CARTESIAN_POINT ( 'NONE',  ( 1.734723475976807094E-15, -3.033600742197708477, 5.000000000000000000 ) ) ;
#80480 = CARTESIAN_POINT ( 'NONE',  ( 34.47516574401890210, 9.028067341115718847, 4.998110765256834398 ) ) ;
#80481 = CARTESIAN_POINT ( 'NONE',  ( -20.29289321881331531, 17.25929247661554200, 5.000000000000000000 ) ) ;
#80482 = FILL_AREA_STYLE_COLOUR ( '', #137105 ) ;
#80483 = VERTEX_POINT ( 'NONE', #103993 ) ;
#80484 = VERTEX_POINT ( 'NONE', #138818 ) ;
#80485 = CARTESIAN_POINT ( 'NONE',  ( 107.0420968585647756, 5.291415217122923842, -3.054999999999996163 ) ) ;
#80486 = VECTOR ( 'NONE', #134190, 999.9999999999998863 ) ;
#80487 = VERTEX_POINT ( 'NONE', #93859 ) ;
#80488 = EDGE_CURVE ( 'NONE', #127894, #26964, #126476, .T. ) ;
#80489 = CARTESIAN_POINT ( 'NONE',  ( 99.00000000000000000, 0.000000000000000000, -7.950000000000000178 ) ) ;
#80490 = LINE ( 'NONE', #69623, #142681 ) ;
#80491 = ADVANCED_FACE ( 'NONE', ( #48953 ), #93153, .F. ) ;
#80492 = DIRECTION ( 'NONE',  ( -0.7071067811865486830, -0.7071067811865464625, -0.000000000000000000 ) ) ;
#80493 = CARTESIAN_POINT ( 'NONE',  ( 0.1600000000000026401, -9.717572351234235426E-16, -7.934999999999990727 ) ) ;
#80494 = CARTESIAN_POINT ( 'NONE',  ( 103.5995968585647802, -6.109999999999997655, -1.637169565754160283 ) ) ;
#80495 = ORIENTED_EDGE ( 'NONE', *, *, #137828, .T. ) ;
#80496 = ORIENTED_EDGE ( 'NONE', *, *, #67297, .F. ) ;
#80497 = CARTESIAN_POINT ( 'NONE',  ( 4.499999999999972466, 6.277155672890274651, -3.510561720658952556 ) ) ;
#80498 = PLANE ( 'NONE',  #98691 ) ;
#80499 = AXIS2_PLACEMENT_3D ( 'NONE', #120830, #62924, #20081 ) ;
#80500 = VERTEX_POINT ( 'NONE', #138088 ) ;
#80501 = ORIENTED_EDGE ( 'NONE', *, *, #44927, .T. ) ;
#80502 = ORIENTED_EDGE ( 'NONE', *, *, #45579, .F. ) ;
#80503 = DIRECTION ( 'NONE',  ( 1.000000000000000000, 0.000000000000000000, 0.000000000000000000 ) ) ;
#80504 = PLANE ( 'NONE',  #41534 ) ;
#80505 = VECTOR ( 'NONE', #93532, 1000.000000000000000 ) ;
#80506 = VECTOR ( 'NONE', #61136, 1000.000000000000000 ) ;
#80507 = VECTOR ( 'NONE', #15020, 1000.000000000000000 ) ;
#80508 = EDGE_CURVE ( 'NONE', #9588, #91284, #47166, .T. ) ;
#80509 = CARTESIAN_POINT ( 'NONE',  ( 27.62043019189810877, 3.055000000000001936, -5.291415217122916737 ) ) ;
#80510 = ORIENTED_EDGE ( 'NONE', *, *, #113742, .F. ) ;
#80511 = ORIENTED_EDGE ( 'NONE', *, *, #647, .F. ) ;
#80512 = EDGE_CURVE ( 'NONE', #70831, #21420, #38076, .T. ) ;
#80513 = DIRECTION ( 'NONE',  ( 0.000000000000000000, -1.000000000000000000, 0.000000000000000000 ) ) ;
#80514 = ORIENTED_EDGE ( 'NONE', *, *, #78858, .T. ) ;
#80515 = ORIENTED_EDGE ( 'NONE', *, *, #111717, .T. ) ;
#80516 = VECTOR ( 'NONE', #9100, 1000.000000000000000 ) ;
#80517 = EDGE_CURVE ( 'NONE', #77643, #16581, #137385, .T. ) ;
#80518 = ADVANCED_FACE ( 'NONE', ( #105438 ), #72160, .F. ) ;
#80519 = FACE_OUTER_BOUND ( 'NONE', #85421, .T. ) ;
#80520 = DIRECTION ( 'NONE',  ( -1.000000000000000000, -1.224606353822377258E-16, -0.000000000000000000 ) ) ;
#80521 = ORIENTED_EDGE ( 'NONE', *, *, #43023, .F. ) ;
#80522 = PLANE ( 'NONE',  #99272 ) ;
#80523 = DIRECTION ( 'NONE',  ( 0.7071067811865487940, 0.7071067811865463515, 0.000000000000000000 ) ) ;
#80524 = PLANE ( 'NONE',  #60000 ) ;
#80525 = ADVANCED_FACE ( 'NONE', ( #27170 ), #71412, .T. ) ;
#80526 = DIRECTION ( 'NONE',  ( -0.6830127018922180770, -0.6830127018922204085, -0.2588190451025213501 ) ) ;
#80527 = FACE_BOUND ( 'NONE', #105627, .T. ) ;
#80528 = EDGE_CURVE ( 'NONE', #98083, #103858, #54697, .T. ) ;
#80529 = ORIENTED_EDGE ( 'NONE', *, *, #29114, .T. ) ;
#80530 = CARTESIAN_POINT ( 'NONE',  ( 63.22502705046288440, 5.819803920172573974, -5.819803920172573086 ) ) ;
#80531 = CARTESIAN_POINT ( 'NONE',  ( 14.27159235450332098, 9.902892378096218942E-16, 0.000000000000000000 ) ) ;
#80532 = LINE ( 'NONE', #124727, #49225 ) ;
#80533 = EDGE_CURVE ( 'NONE', #108682, #46312, #127942, .T. ) ;
#80534 = ORIENTED_EDGE ( 'NONE', *, *, #3640, .F. ) ;
#80535 = FACE_OUTER_BOUND ( 'NONE', #48174, .T. ) ;
#80536 = ORIENTED_EDGE ( 'NONE', *, *, #913, .F. ) ;
#80537 = AXIS2_PLACEMENT_3D ( 'NONE', #66106, #35634, #32763 ) ;
#80538 = ORIENTED_EDGE ( 'NONE', *, *, #102336, .F. ) ;
#80539 = ORIENTED_EDGE ( 'NONE', *, *, #60175, .F. ) ;
#80540 = CARTESIAN_POINT ( 'NONE',  ( 37.68293019189810167, -1.637169565754158951, -6.109999999999998543 ) ) ;
#80541 = EDGE_CURVE ( 'NONE', #73668, #77753, #70488, .T. ) ;
#80542 =( GEOMETRIC_REPRESENTATION_CONTEXT ( 3 ) GLOBAL_UNCERTAINTY_ASSIGNED_CONTEXT ( ( #111624 ) ) GLOBAL_UNIT_ASSIGNED_CONTEXT ( ( #118874, #63109, #97847 ) ) REPRESENTATION_CONTEXT ( 'NONE', 'WORKASPACE' ) );
#80543 = ORIENTED_EDGE ( 'NONE', *, *, #125346, .T. ) ;
#80544 = EDGE_CURVE ( 'NONE', #121977, #3709, #101627, .T. ) ;
#80545 = CARTESIAN_POINT ( 'NONE',  ( -48.48921356237309510, -27.52281430457089328, 5.000000000000000000 ) ) ;
#80546 = DIRECTION ( 'NONE',  ( 0.000000000000000000, 0.000000000000000000, 1.000000000000000000 ) ) ;
#80547 = DIRECTION ( 'NONE',  ( -0.6830127018922181881, 0.6830127018922202975, -0.2588190451025214056 ) ) ;
#80548 = VERTEX_POINT ( 'NONE', #81338 ) ;
#80549 = CARTESIAN_POINT ( 'NONE',  ( 2.999999999999983569, 18.08204922493373346, 0.9627537363044802454 ) ) ;
#80550 = FILL_AREA_STYLE_COLOUR ( '', #112993 ) ;
#80551 = EDGE_CURVE ( 'NONE', #98765, #115565, #2278, .T. ) ;
#80552 = PLANE ( 'NONE',  #120938 ) ;
#80553 = LINE ( 'NONE', #71822, #69147 ) ;
#80554 = DIRECTION ( 'NONE',  ( -0.3543493200069162685, -0.000000000000000000, -0.9351131265310288487 ) ) ;
#80555 = PLANE ( 'NONE',  #80711 ) ;
#80556 = CARTESIAN_POINT ( 'NONE',  ( 2.000000000000000000, 2.375000000000000000, 0.000000000000000000 ) ) ;
#80557 = EDGE_LOOP ( 'NONE', ( #13294, #9635, #116115 ) ) ;
#80558 = ORIENTED_EDGE ( 'NONE', *, *, #73598, .T. ) ;
#80560 = ORIENTED_EDGE ( 'NONE', *, *, #89007, .F. ) ;
#80559 = ADVANCED_FACE ( 'NONE', ( #82066 ), #80615, .T. ) ;
#80561 = ORIENTED_EDGE ( 'NONE', *, *, #123921, .T. ) ;
#80562 = DIRECTION ( 'NONE',  ( -0.000000000000000000, -0.000000000000000000, 1.000000000000000000 ) ) ;
#80563 = VERTEX_POINT ( 'NONE', #113935 ) ;
#80564 = EDGE_LOOP ( 'NONE', ( #104530, #21714, #56848, #96391 ) ) ;
#80565 = CARTESIAN_POINT ( 'NONE',  ( 153.6500000000000057, 0.000000000000000000, 6.349999999999997868 ) ) ;
#80566 = CYLINDRICAL_SURFACE ( 'NONE', #134288, 0.5000000000000004441 ) ;
#80567 = ORIENTED_EDGE ( 'NONE', *, *, #68898, .F. ) ;
#80568 = EDGE_CURVE ( 'NONE', #2777, #79775, #135012, .T. ) ;
#80569 = FACE_OUTER_BOUND ( 'NONE', #135939, .T. ) ;
#80570 = ORIENTED_EDGE ( 'NONE', *, *, #41668, .F. ) ;
#80571 = FACE_OUTER_BOUND ( 'NONE', #34778, .T. ) ;
#80572 = EDGE_CURVE ( 'NONE', #70280, #76991, #14626, .T. ) ;
#80573 = CARTESIAN_POINT ( 'NONE',  ( 31.27540314143522693, -2.126176841940958351, -7.934999999999989839 ) ) ;
#80574 = CARTESIAN_POINT ( 'NONE',  ( 2.692069808101885897, -7.934999999999991616, -2.126176841940955242 ) ) ;
#80575 = ORIENTED_EDGE ( 'NONE', *, *, #77776, .T. ) ;
#80577 = CARTESIAN_POINT ( 'NONE',  ( 14.35681257248253040, -20.24070752338407431, 21.22881796311216362 ) ) ;
#80576 = CARTESIAN_POINT ( 'NONE',  ( 110.4537635252314516, -6.109999999999999432, -3.741295971395163529E-16 ) ) ;
#80578 = AXIS2_PLACEMENT_3D ( 'NONE', #75358, #64467, #44733 ) ;
#80579 = DIRECTION ( 'NONE',  ( -1.000000000000000000, -0.000000000000000000, -0.000000000000000000 ) ) ;
#80580 = DIRECTION ( 'NONE',  ( -0.7071067811865486830, -0.7071067811865464625, 0.000000000000000000 ) ) ;
#80581 = ORIENTED_EDGE ( 'NONE', *, *, #11572, .T. ) ;
#80582 = FACE_OUTER_BOUND ( 'NONE', #79517, .T. ) ;
#80583 = ORIENTED_EDGE ( 'NONE', *, *, #109016, .T. ) ;
#80584 = CARTESIAN_POINT ( 'NONE',  ( 10.52840764549667618, 9.139736423841732040E-16, 0.000000000000000000 ) ) ;
#80585 = FACE_OUTER_BOUND ( 'NONE', #122227, .T. ) ;
#80586 = SURFACE_SIDE_STYLE ('',( #137091 ) ) ;
#80588 = EDGE_CURVE ( 'NONE', #92161, #137268, #92165, .T. ) ;
#80587 = DIRECTION ( 'NONE',  ( -0.7071067811865486830, -0.7071067811865464625, -0.000000000000000000 ) ) ;
#80589 = CARTESIAN_POINT ( 'NONE',  ( 27.48921356237309155, -27.52281430457074762, 5.000000000000000000 ) ) ;
#80590 = CARTESIAN_POINT ( 'NONE',  ( 121.6041666666666714, 2.130196079827450628, 7.949999999999986855 ) ) ;
#80591 = ORIENTED_EDGE ( 'NONE', *, *, #89395, .T. ) ;
#80592 = VECTOR ( 'NONE', #66197, 1000.000000000000000 ) ;
#80593 = CARTESIAN_POINT ( 'NONE',  ( 18.00548008471250583, 28.92564299267925776, 4.000000000000000000 ) ) ;
#80594 = DIRECTION ( 'NONE',  ( 1.000000000000000000, 0.000000000000000000, 0.000000000000000000 ) ) ;
#80595 = EDGE_LOOP ( 'NONE', ( #131312, #76956, #126153, #87921, #115213 ) ) ;
#80596 = PLANE ( 'NONE',  #136924 ) ;
#80597 = LINE ( 'NONE', #30491, #5283 ) ;
#80598 = ORIENTED_EDGE ( 'NONE', *, *, #132217, .T. ) ;
#80599 = VECTOR ( 'NONE', #17550, 999.9999999999998863 ) ;
#80601 = ORIENTED_EDGE ( 'NONE', *, *, #125007, .F. ) ;
#80600 = DIRECTION ( 'NONE',  ( 0.7071067811865487940, -0.7071067811865463515, 0.000000000000000000 ) ) ;
#80602 = EDGE_LOOP ( 'NONE', ( #68014, #55739, #112835, #137946 ) ) ;
#80603 = LINE ( 'NONE', #11726, #91276 ) ;
#80604 = LINE ( 'NONE', #11008, #96805 ) ;
#80605 = VECTOR ( 'NONE', #74117, 1000.000000000000227 ) ;
#80606 = VERTEX_POINT ( 'NONE', #111804 ) ;
#80607 = VECTOR ( 'NONE', #69672, 1000.000000000000227 ) ;
#80608 = DIRECTION ( 'NONE',  ( 0.6830127018922180770, -0.6830127018922204085, -0.2588190451025213501 ) ) ;
#80609 = ORIENTED_EDGE ( 'NONE', *, *, #135953, .T. ) ;
#80610 = CARTESIAN_POINT ( 'NONE',  ( -72.18398860626899705, 28.73617430169837661, 5.000000000000000000 ) ) ;
#80611 = DIRECTION ( 'NONE',  ( -0.7071067811865486830, -0.7071067811865464625, 0.000000000000000000 ) ) ;
#80612 = EDGE_CURVE ( 'NONE', #45041, #60739, #12470, .T. ) ;
#80613 = CARTESIAN_POINT ( 'NONE',  ( 12.69999999999999574, -59.76999999999998892, -40.00000000000000000 ) ) ;
#80614 = CARTESIAN_POINT ( 'NONE',  ( -78.48921356237309510, -27.52281430457109934, 5.000000000000000000 ) ) ;
#80615 = PLANE ( 'NONE',  #84182 ) ;
#80616 = DIRECTION ( 'NONE',  ( -0.6830127018922180770, -0.6830127018922204085, -0.2588190451025213501 ) ) ;
#80617 = FACE_OUTER_BOUND ( 'NONE', #63662, .T. ) ;
#80618 = CARTESIAN_POINT ( 'NONE',  ( 0.000000000000000000, 0.000000000000000000, 5.000000000000000000 ) ) ;
#80619 = VERTEX_POINT ( 'NONE', #69027 ) ;
#80620 = ORIENTED_EDGE ( 'NONE', *, *, #62911, .F. ) ;
#80621 = ORIENTED_EDGE ( 'NONE', *, *, #32548, .F. ) ;
#80622 = CARTESIAN_POINT ( 'NONE',  ( 117.0833333333333286, 6.884901960086290629, -3.974999999999994316 ) ) ;
#80623 = ORIENTED_EDGE ( 'NONE', *, *, #6430, .T. ) ;
#80624 = ORIENTED_EDGE ( 'NONE', *, *, #94898, .F. ) ;
#80625 = ORIENTED_EDGE ( 'NONE', *, *, #71815, .T. ) ;
#80626 = FACE_OUTER_BOUND ( 'NONE', #93501, .T. ) ;
#80627 = DIRECTION ( 'NONE',  ( 0.000000000000000000, -1.000000000000000000, 0.000000000000000000 ) ) ;
#80628 = VERTEX_POINT ( 'NONE', #125547 ) ;
#80629 = CARTESIAN_POINT ( 'NONE',  ( -36.48921356237310221, -27.52281430457080802, 5.000000000000000000 ) ) ;
#80630 = VECTOR ( 'NONE', #8162, 1000.000000000000000 ) ;
#80631 = CARTESIAN_POINT ( 'NONE',  ( 25.49999999999982236, 18.43112307739199451, 4.000000000000000000 ) ) ;
#80632 = CARTESIAN_POINT ( 'NONE',  ( -34.92500000000001137, 20.81665438641021382, 4.500000000000000888 ) ) ;
#80633 = CARTESIAN_POINT ( 'NONE',  ( 114.0420968585647898, 5.291415217122923842, -3.054999999999996163 ) ) ;
#80634 = EDGE_CURVE ( 'NONE', #130061, #80908, #46598, .T. ) ;
#80635 = ORIENTED_EDGE ( 'NONE', *, *, #94860, .F. ) ;
#80636 = CARTESIAN_POINT ( 'NONE',  ( 25.01899999999999835, 3.174999999999997158, 5.000000000000000000 ) ) ;
#80637 = CARTESIAN_POINT ( 'NONE',  ( 106.3916937171295558, 2.130196079827421762, 7.950000000000000178 ) ) ;
#80638 = VECTOR ( 'NONE', #88399, 999.9999999999998863 ) ;
#80639 = CARTESIAN_POINT ( 'NONE',  ( 27.99999999999999645, -2.055000000000000160, 0.000000000000000000 ) ) ;
#80640 = DIRECTION ( 'NONE',  ( -0.3543493200069162685, -0.000000000000000000, -0.9351131265310288487 ) ) ;
#80641 = CARTESIAN_POINT ( 'NONE',  ( 14.53839644629420569, -9.740707523384173783, 17.74957260769614109 ) ) ;
#80642 = CARTESIAN_POINT ( 'NONE',  ( 33.29974487139158867, -27.71228299555229313, 4.000000000000000000 ) ) ;
#80643 = FACE_OUTER_BOUND ( 'NONE', #135132, .T. ) ;
#80644 = EDGE_CURVE ( 'NONE', #46174, #80908, #114635, .T. ) ;
#80646 = ADVANCED_FACE ( 'NONE', ( #34976 ), #45855, .T. ) ;
#80645 = CARTESIAN_POINT ( 'NONE',  ( 46.89169371712956291, 2.130196079827421762, 7.950000000000001066 ) ) ;
#80647 = DIRECTION ( 'NONE',  ( -0.000000000000000000, 0.3543493200069153248, 0.9351131265310292928 ) ) ;
#80648 = CARTESIAN_POINT ( 'NONE',  ( 36.18398860626899705, 28.73617430169812437, 5.000000000000000000 ) ) ;
#80649 = ORIENTED_EDGE ( 'NONE', *, *, #113862, .T. ) ;
#80650 = ORIENTED_EDGE ( 'NONE', *, *, #64943, .T. ) ;
#80651 = CARTESIAN_POINT ( 'NONE',  ( 39.35416666666665719, -2.130196079827425315, -7.950000000000001066 ) ) ;
#80652 = VERTEX_POINT ( 'NONE', #3702 ) ;
#80653 = ORIENTED_EDGE ( 'NONE', *, *, #24389, .F. ) ;
#80654 = ADVANCED_FACE ( 'NONE', ( #126249 ), #137126, .F. ) ;
#80655 = DIRECTION ( 'NONE',  ( -0.7071067811865487940, 0.7071067811865463515, 0.000000000000000000 ) ) ;
#80656 = DIRECTION ( 'NONE',  ( 0.7071067811865487940, 0.7071067811865463515, -0.000000000000000000 ) ) ;
#80657 = ORIENTED_EDGE ( 'NONE', *, *, #89799, .F. ) ;
#80658 = AXIS2_PLACEMENT_3D ( 'NONE', #92636, #124576, #25251 ) ;
#80659 = FACE_OUTER_BOUND ( 'NONE', #73794, .T. ) ;
#80661 = VECTOR ( 'NONE', #131590, 1000.000000000000000 ) ;
#80660 = DIRECTION ( 'NONE',  ( -0.000000000000000000, -0.3543493200069152693, 0.9351131265310292928 ) ) ;
#80662 = EDGE_CURVE ( 'NONE', #90647, #128697, #136395, .T. ) ;
#80663 = CARTESIAN_POINT ( 'NONE',  ( 26.25043019189810067, 3.055000000000002824, -5.291415217122919401 ) ) ;
#80664 = EDGE_LOOP ( 'NONE', ( #141282, #29631, #61596, #86415 ) ) ;
#80665 = LINE ( 'NONE', #38573, #57249 ) ;
#80666 = ORIENTED_EDGE ( 'NONE', *, *, #11759, .F. ) ;
#80667 = DIRECTION ( 'NONE',  ( -0.000000000000000000, 0.3543493200069153248, 0.9351131265310292928 ) ) ;
#80668 = EDGE_CURVE ( 'NONE', #47857, #672, #14606, .T. ) ;
#80669 = LINE ( 'NONE', #2336, #107885 ) ;
#80670 = SURFACE_STYLE_USAGE ( .BOTH. , #36436 ) ;
#80671 = CARTESIAN_POINT ( 'NONE',  ( 8.510786437626906675, -27.52281430457049183, 5.000000000000000000 ) ) ;
#80672 = ORIENTED_EDGE ( 'NONE', *, *, #47808, .T. ) ;
#80673 = ORIENTED_EDGE ( 'NONE', *, *, #54062, .T. ) ;
#80674 = DIRECTION ( 'NONE',  ( -0.6830127018922181881, 0.6830127018922202975, -0.2588190451025214056 ) ) ;
#80675 = LINE ( 'NONE', #124161, #143414 ) ;
#80676 = DIRECTION ( 'NONE',  ( -0.7071067811865487940, 0.7071067811865463515, -0.000000000000000000 ) ) ;
#80677 = ADVANCED_FACE ( 'NONE', ( #124102 ), #37831, .F. ) ;
#80678 = CARTESIAN_POINT ( 'NONE',  ( -34.49999999999975842, 10.46425560840038038, 4.994342998332163219 ) ) ;
#80680 = EDGE_CURVE ( 'NONE', #82809, #125587, #58181, .T. ) ;
#80679 = CARTESIAN_POINT ( 'NONE',  ( -17.99451991528748351, 28.92564299267950645, 4.000000000000000000 ) ) ;
#80681 = VECTOR ( 'NONE', #120422, 1000.000000000000000 ) ;
#80682 = CARTESIAN_POINT ( 'NONE',  ( 61.74543019189811588, -5.291415217122918513, -3.055000000000000160 ) ) ;
#80683 = CARTESIAN_POINT ( 'NONE',  ( 42.29974487139158157, -27.71228299555235708, 4.000000000000000000 ) ) ;
#80684 = ADVANCED_FACE ( 'NONE', ( #122996 ), #79544, .F. ) ;
#80685 = CARTESIAN_POINT ( 'NONE',  ( 29.29289321881325847, -12.74070752338415247, 5.000000000000000000 ) ) ;
#80686 = ORIENTED_EDGE ( 'NONE', *, *, #49089, .T. ) ;
#80687 = ORIENTED_EDGE ( 'NONE', *, *, #15657, .T. ) ;
#80688 = FACE_OUTER_BOUND ( 'NONE', #107253, .T. ) ;
#80689 = ORIENTED_EDGE ( 'NONE', *, *, #78750, .F. ) ;
#80690 = EDGE_CURVE ( 'NONE', #140203, #24994, #124416, .T. ) ;
#80691 = EDGE_CURVE ( 'NONE', #19406, #22039, #57764, .T. ) ;
#80692 = LINE ( 'NONE', #91560, #78960 ) ;
#80693 = PRODUCT_DEFINITION_CONTEXT ( 'detailed design', #38308, 'design' ) ;
#80694 = ORIENTED_EDGE ( 'NONE', *, *, #132041, .T. ) ;
#80695 = CARTESIAN_POINT ( 'NONE',  ( 34.75611968250419181, 7.705650698523971442, 4.955485411084875835 ) ) ;
#80696 = LINE ( 'NONE', #27005, #106389 ) ;
#80697 = AXIS2_PLACEMENT_3D ( 'NONE', #74473, #18609, #21506 ) ;
#80698 = CIRCLE ( 'NONE', #101473, 2.055000000000000604 ) ;
#80699 = EDGE_CURVE ( 'NONE', #7787, #10314, #113524, .T. ) ;
#80700 = DIRECTION ( 'NONE',  ( -3.115803279706882722E-16, 1.000000000000000000, 0.000000000000000000 ) ) ;
#80701 = VECTOR ( 'NONE', #13424, 1000.000000000000000 ) ;
#80702 = FACE_BOUND ( 'NONE', #86893, .T. ) ;
#80703 = ADVANCED_FACE ( 'NONE', ( #12073 ), #100537, .F. ) ;
#80704 = LINE ( 'NONE', #37915, #128981 ) ;
#80705 = VECTOR ( 'NONE', #109988, 1000.000000000000000 ) ;
#80706 = CARTESIAN_POINT ( 'NONE',  ( -9.792893218813388145, -5.240707523384232402, 5.000000000000000000 ) ) ;
#80707 = LINE ( 'NONE', #27724, #59543 ) ;
#80708 = FACE_OUTER_BOUND ( 'NONE', #23449, .T. ) ;
#80710 = ORIENTED_EDGE ( 'NONE', *, *, #78707, .F. ) ;
#80709 = DIRECTION ( 'NONE',  ( -1.000000000000000000, -0.000000000000000000, -0.000000000000000000 ) ) ;
#80711 = AXIS2_PLACEMENT_3D ( 'NONE', #2215, #101554, #70426 ) ;
#80712 = VECTOR ( 'NONE', #139465, 1000.000000000000000 ) ;
#80713 = LINE ( 'NONE', #25580, #35598 ) ;
#80714 = ITEM_DEFINED_TRANSFORMATION ( 'NONE', 'NONE', #35590,  #127880 ) ;
#80715 = ORIENTED_EDGE ( 'NONE', *, *, #107178, .T. ) ;
#80716 = ORIENTED_EDGE ( 'NONE', *, *, #133383, .T. ) ;
#80717 = CARTESIAN_POINT ( 'NONE',  ( 62.32876352523145158, 0.000000000000000000, -6.109999999999998543 ) ) ;
#80718 = EDGE_LOOP ( 'NONE', ( #66464, #129369, #62673, #86489 ) ) ;
#80719 = EDGE_CURVE ( 'NONE', #104365, #40167, #91103, .T. ) ;
#80720 = CARTESIAN_POINT ( 'NONE',  ( 60.18398860626900415, 28.73617430169829490, 5.000000000000000000 ) ) ;
#80721 = ORIENTED_EDGE ( 'NONE', *, *, #73489, .T. ) ;
#80722 = CARTESIAN_POINT ( 'NONE',  ( -42.18398860626899705, 28.73617430169816700, 5.000000000000000000 ) ) ;
#80723 = MECHANICAL_DESIGN_GEOMETRIC_PRESENTATION_REPRESENTATION (  '', ( #59915 ), #131631 ) ;
#80724 = EDGE_CURVE ( 'NONE', #25800, #39048, #1185, .T. ) ;
#80725 = LINE ( 'NONE', #69868, #77332 ) ;
#80726 = VECTOR ( 'NONE', #81154, 1000.000000000000114 ) ;
#80727 = LINE ( 'NONE', #69134, #31710 ) ;
#80728 = FACE_OUTER_BOUND ( 'NONE', #121082, .T. ) ;
#80729 = DIRECTION ( 'NONE',  ( -0.7071067811865486830, -0.7071067811865464625, 0.000000000000000000 ) ) ;
#80730 = LINE ( 'NONE', #58302, #116462 ) ;
#80731 = DIRECTION ( 'NONE',  ( -1.000000000000000000, -0.000000000000000000, -0.000000000000000000 ) ) ;
#80732 = ORIENTED_EDGE ( 'NONE', *, *, #125985, .F. ) ;
#80733 = AXIS2_PLACEMENT_3D ( 'NONE', #23162, #110881, #123953 ) ;
#80734 = ORIENTED_EDGE ( 'NONE', *, *, #42917, .T. ) ;
#80735 = CARTESIAN_POINT ( 'NONE',  ( 24.87999999999999901, 2.055000000000001492, 2.516649172247811554E-16 ) ) ;
#80736 = CARTESIAN_POINT ( 'NONE',  ( 20.28769006033958178, -21.73547319004781642, 4.999917730833664642 ) ) ;
#80737 = ORIENTED_EDGE ( 'NONE', *, *, #93864, .T. ) ;
#80738 = AXIS2_PLACEMENT_3D ( 'NONE', #509, #133217, #33894 ) ;
#80739 = ORIENTED_EDGE ( 'NONE', *, *, #72802, .T. ) ;
#80740 = AXIS2_PLACEMENT_3D ( 'NONE', #103675, #91419, #15240 ) ;
#80741 = ORIENTED_EDGE ( 'NONE', *, *, #111040, .F. ) ;
#80742 = CARTESIAN_POINT ( 'NONE',  ( -19.49999999999986500, 9.127013188829483425, 4.802533355213530086 ) ) ;
#80743 = VERTEX_POINT ( 'NONE', #24390 ) ;
#80744 = VECTOR ( 'NONE', #69950, 999.9999999999998863 ) ;
#80745 = DIRECTION ( 'NONE',  ( 1.000000000000000000, 0.000000000000000000, 0.000000000000000000 ) ) ;
#80746 = EDGE_CURVE ( 'NONE', #70432, #75407, #47617, .T. ) ;
#80747 = PLANE ( 'NONE',  #60944 ) ;
#80748 = CARTESIAN_POINT ( 'NONE',  ( 2.692069808101885897, -7.934999999999991616, -2.126176841940955242 ) ) ;
#80749 = DIRECTION ( 'NONE',  ( -0.000000000000000000, 0.3543493200069153248, 0.9351131265310292928 ) ) ;
#80750 = ORIENTED_EDGE ( 'NONE', *, *, #130934, .F. ) ;
#80751 = DIRECTION ( 'NONE',  ( 0.000000000000000000, -1.000000000000000000, 0.000000000000000000 ) ) ;
#80752 = DIRECTION ( 'NONE',  ( 0.6830127018922181881, 0.6830127018922202975, -0.2588190451025214056 ) ) ;
#80753 = DIRECTION ( 'NONE',  ( 0.7071067811865487940, 0.7071067811865463515, -0.000000000000000000 ) ) ;
#80754 = VECTOR ( 'NONE', #90191, 999.9999999999998863 ) ;
#80756 = ORIENTED_EDGE ( 'NONE', *, *, #83066, .F. ) ;
#80755 = DIRECTION ( 'NONE',  ( -0.7071067811865486830, -0.7071067811865464625, 0.000000000000000000 ) ) ;
#80757 = VERTEX_POINT ( 'NONE', #112821 ) ;
#80758 = DIRECTION ( 'NONE',  ( -0.7071067811865487940, 0.7071067811865463515, 0.000000000000000000 ) ) ;
#80759 = FACE_OUTER_BOUND ( 'NONE', #127257, .T. ) ;
#80760 = VECTOR ( 'NONE', #44437, 1000.000000000000000 ) ;
#80761 = DIRECTION ( 'NONE',  ( 0.7071067811865486830, -0.7071067811865464625, -0.000000000000000000 ) ) ;
#80762 = ORIENTED_EDGE ( 'NONE', *, *, #53585, .T. ) ;
#80763 = DIRECTION ( 'NONE',  ( -0.7071067811865487940, 0.7071067811865463515, -0.000000000000000000 ) ) ;
#80764 = LINE ( 'NONE', #1707, #122782 ) ;
#80765 = DIRECTION ( 'NONE',  ( -0.7071067811865486830, 0.7071067811865464625, 0.000000000000000000 ) ) ;
#80766 = ORIENTED_EDGE ( 'NONE', *, *, #116429, .T. ) ;
#80767 = CARTESIAN_POINT ( 'NONE',  ( 17.84878961325748037, 4.584330080086930965E-16, 0.000000000000000000 ) ) ;
#80768 = FACE_OUTER_BOUND ( 'NONE', #142081, .T. ) ;
#80769 = DIRECTION ( 'NONE',  ( 0.7071067811865487940, 0.7071067811865463515, 0.000000000000000000 ) ) ;
#80770 = CARTESIAN_POINT ( 'NONE',  ( 27.99999999999999645, -57.14999999999999147, -45.92499999999969873 ) ) ;
#80771 = LINE ( 'NONE', #24239, #25149 ) ;
#80772 = VERTEX_POINT ( 'NONE', #135323 ) ;
#80773 = VERTEX_POINT ( 'NONE', #80929 ) ;
#80774 = CARTESIAN_POINT ( 'NONE',  ( 14.51078643762690490, -27.52281430457045275, 5.000000000000000000 ) ) ;
#80775 = CARTESIAN_POINT ( 'NONE',  ( 120.0000000000000000, 0.000000000000000000, -7.950000000000000178 ) ) ;
#80776 = CARTESIAN_POINT ( 'NONE',  ( 4.791236474768552966, -9.717572351234235426E-16, -7.934999999999990727 ) ) ;
#80777 = CARTESIAN_POINT ( 'NONE',  ( 21.48921356237309155, -27.52281430457070499, 5.000000000000000000 ) ) ;
#80778 = FACE_OUTER_BOUND ( 'NONE', #73620, .T. ) ;
#80779 = DIRECTION ( 'NONE',  ( 0.7071067811865487940, 0.7071067811865463515, 0.000000000000000000 ) ) ;
#80780 = CARTESIAN_POINT ( 'NONE',  ( -21.48921356237309155, -27.52281430457070499, 5.000000000000000000 ) ) ;
#80781 = ORIENTED_EDGE ( 'NONE', *, *, #130775, .F. ) ;
#80782 = FACE_OUTER_BOUND ( 'NONE', #73404, .T. ) ;
#80783 = LINE ( 'NONE', #124982, #107156 ) ;
#80784 = FILL_AREA_STYLE_COLOUR ( '', #96842 ) ;
#80785 = CARTESIAN_POINT ( 'NONE',  ( 59.12043019189810877, 3.055000000000002380, -5.291415217122917625 ) ) ;
#80786 = FACE_OUTER_BOUND ( 'NONE', #433, .T. ) ;
#80787 = EDGE_CURVE ( 'NONE', #115169, #54350, #13478, .T. ) ;
#80788 = CARTESIAN_POINT ( 'NONE',  ( -28.49999999999979750, -15.29013452822857033, 0.3645803511609698733 ) ) ;
#80789 = ORIENTED_EDGE ( 'NONE', *, *, #139695, .T. ) ;
#80790 = DIRECTION ( 'NONE',  ( -0.7071067811865487940, 0.7071067811865463515, -0.000000000000000000 ) ) ;
#80791 = ADVANCED_FACE ( 'NONE', ( #102684 ), #69340, .F. ) ;
#80792 = EDGE_CURVE ( 'NONE', #57879, #23024, #101952, .T. ) ;
#80793 = EDGE_LOOP ( 'NONE', ( #45161, #102937, #24618, #112590 ) ) ;
#80794 = EDGE_CURVE ( 'NONE', #2255, #91343, #2616, .T. ) ;
#80795 = DIRECTION ( 'NONE',  ( 0.000000000000000000, 1.000000000000000000, 0.000000000000000000 ) ) ;
#80796 = AXIS2_PLACEMENT_3D ( 'NONE', #34347, #26151, #80546 ) ;
#80797 = VECTOR ( 'NONE', #26550, 1000.000000000000000 ) ;
#80798 = VECTOR ( 'NONE', #75960, 1000.000000000000227 ) ;
#80799 = LINE ( 'NONE', #90969, #57766 ) ;
#80800 = CARTESIAN_POINT ( 'NONE',  ( 1.966599676569761534, 6.759292476615653023, 12.28218704918522519 ) ) ;
#80802 = EDGE_CURVE ( 'NONE', #89781, #102633, #49746, .T. ) ;
#80801 = AXIS2_PLACEMENT_3D ( 'NONE', #44908, #97798, #99197 ) ;
#80803 = DIRECTION ( 'NONE',  ( 0.7071067811865486830, -0.7071067811865464625, -0.000000000000000000 ) ) ;
#80804 = PLANE ( 'NONE',  #108977 ) ;
#80805 = CARTESIAN_POINT ( 'NONE',  ( 128.7663314791381026, -49.19090614206155010, 40.79110616922538668 ) ) ;
#80806 = EDGE_CURVE ( 'NONE', #75784, #66948, #128140, .T. ) ;
#80807 = ADVANCED_FACE ( 'NONE', ( #106198 ), #27962, .T. ) ;
#80808 = EDGE_LOOP ( 'NONE', ( #87266, #105541, #32063, #126660 ) ) ;
#80809 = ORIENTED_EDGE ( 'NONE', *, *, #114206, .F. ) ;
#80810 = DIRECTION ( 'NONE',  ( 0.000000000000000000, 0.000000000000000000, 1.000000000000000000 ) ) ;
#80811 = CARTESIAN_POINT ( 'NONE',  ( -48.48921356237309510, -27.52281430457089328, 5.000000000000000000 ) ) ;
#80812 = UNCERTAINTY_MEASURE_WITH_UNIT (LENGTH_MEASURE( 1.000000000000000082E-05 ), #12780, 'distance_accuracy_value', 'NONE');
#80813 = VECTOR ( 'NONE', #60293, 999.9999999999998863 ) ;
#80814 = CARTESIAN_POINT ( 'NONE',  ( -10.49999999999992717, 9.052185695429074030, 5.000000000000000000 ) ) ;
#80815 = CARTESIAN_POINT ( 'NONE',  ( -84.18398860626899705, 28.73617430169846187, 5.000000000000000000 ) ) ;
#80816 = EDGE_CURVE ( 'NONE', #63172, #132990, #104933, .T. ) ;
#80818 = EDGE_CURVE ( 'NONE', #73610, #89253, #83059, .T. ) ;
#80817 = CARTESIAN_POINT ( 'NONE',  ( 73.87086038379622721, 6.884901960086289741, -3.974999999999993427 ) ) ;
#80819 = LINE ( 'NONE', #33754, #83090 ) ;
#80820 = VERTEX_POINT ( 'NONE', #139616 ) ;
#80821 = CARTESIAN_POINT ( 'NONE',  ( 64.29166666666665719, 3.975000000000003642, -6.884901960086285300 ) ) ;
#80822 = DIRECTION ( 'NONE',  ( 1.000000000000000000, 0.000000000000000000, 0.000000000000000000 ) ) ;
#80823 = ADVANCED_FACE ( 'NONE', ( #104060 ), #38141, .F. ) ;
#80824 = CARTESIAN_POINT ( 'NONE',  ( 22.49999999999984723, -7.912538124160680475, 4.000000000000000000 ) ) ;
#80825 = CARTESIAN_POINT ( 'NONE',  ( 8.999999999999944933, -0.8619312979531862373, -5.102805207349806693 ) ) ;
#80826 = VECTOR ( 'NONE', #33385, 1000.000000000000000 ) ;
#80827 = VERTEX_POINT ( 'NONE', #7613 ) ;
#80828 = DIRECTION ( 'NONE',  ( -0.7071067811865486830, -0.7071067811865464625, -0.000000000000000000 ) ) ;
#80829 = EDGE_CURVE ( 'NONE', #7006, #94037, #70781, .T. ) ;
#80830 = VECTOR ( 'NONE', #62811, 1000.000000000000000 ) ;
#80831 = CARTESIAN_POINT ( 'NONE',  ( 26.29289321881327623, -15.74070752338411694, 5.000000000000000000 ) ) ;
#80832 = CARTESIAN_POINT ( 'NONE',  ( 68.68793019189809002, 6.110000000000002984, -1.637169565754156730 ) ) ;
#80833 = DIRECTION ( 'NONE',  ( 0.6830127018922181881, 0.6830127018922202975, -0.2588190451025214056 ) ) ;
#80834 = ORIENTED_EDGE ( 'NONE', *, *, #98369, .F. ) ;
#80835 = ORIENTED_EDGE ( 'NONE', *, *, #17388, .T. ) ;
#80836 = STYLED_ITEM ( 'NONE', ( #44676 ), #51969 ) ;
#80837 = VECTOR ( 'NONE', #138023, 1000.000000000000227 ) ;
#80838 = CARTESIAN_POINT ( 'NONE',  ( -34.49999999999975842, -1.592773361805403853, -6.492772025301150052 ) ) ;
#80839 = PLANE ( 'NONE',  #92880 ) ;
#80840 = CIRCLE ( 'NONE', #92381, 5.968999999999998529 ) ;
#80841 = CARTESIAN_POINT ( 'NONE',  ( 44.02083333333332860, 7.949999999999998401, 2.130196079827431532 ) ) ;
#80842 = CARTESIAN_POINT ( 'NONE',  ( -12.49289321881344783, -60.26999999999998181, 25.00000000000000355 ) ) ;
#80844 = ORIENTED_EDGE ( 'NONE', *, *, #108893, .T. ) ;
#80843 = DIRECTION ( 'NONE',  ( -0.3543493200069162685, -0.000000000000000000, -0.9351131265310288487 ) ) ;
#80845 = CARTESIAN_POINT ( 'NONE',  ( 2.816011393730999401, 28.73617430169785436, 5.000000000000000000 ) ) ;
#80846 = DIRECTION ( 'NONE',  ( -1.000000000000000000, -0.000000000000000000, -0.000000000000000000 ) ) ;
#80847 = FACE_OUTER_BOUND ( 'NONE', #28664, .T. ) ;
#80848 = VECTOR ( 'NONE', #2674, 1000.000000000000000 ) ;
#80849 = EDGE_CURVE ( 'NONE', #16022, #74522, #105499, .T. ) ;
#80850 = LINE ( 'NONE', #35927, #140986 ) ;
#80851 = ORIENTED_EDGE ( 'NONE', *, *, #50346, .T. ) ;
#80852 = VERTEX_POINT ( 'NONE', #6875 ) ;
#80853 = SURFACE_STYLE_USAGE ( .BOTH. , #136626 ) ;
#80854 = CARTESIAN_POINT ( 'NONE',  ( -32.93988928955960205, -9.740707523384180888, 10.89222023123388539 ) ) ;
#80855 = ADVANCED_FACE ( 'NONE', ( #127260 ), #140294, .F. ) ;
#80856 = DIRECTION ( 'NONE',  ( 0.7071067811865486830, -0.7071067811865464625, -0.000000000000000000 ) ) ;
#80857 = LINE ( 'NONE', #125048, #133471 ) ;
#80858 = ORIENTED_EDGE ( 'NONE', *, *, #24705, .F. ) ;
#80859 = ORIENTED_EDGE ( 'NONE', *, *, #77719, .T. ) ;
#80860 = AXIS2_PLACEMENT_3D ( 'NONE', #76310, #31373, #87886 ) ;
#80861 = CARTESIAN_POINT ( 'NONE',  ( -8.999999999999937828, -10.06887692260771416, 4.000000000000000000 ) ) ;
#80862 = CARTESIAN_POINT ( 'NONE',  ( 6.707106781186507050, 5.259292476615661016, 5.000000000000000000 ) ) ;
#80863 = EDGE_CURVE ( 'NONE', #7505, #40271, #71473, .T. ) ;
#80864 = VERTEX_POINT ( 'NONE', #137449 ) ;
#80865 = CARTESIAN_POINT ( 'NONE',  ( 5.524873872149501430, 14.25929247661557397, 9.797011795316649341 ) ) ;
#80867 = EDGE_CURVE ( 'NONE', #102793, #43279, #105041, .T. ) ;
#80866 = ORIENTED_EDGE ( 'NONE', *, *, #13385, .F. ) ;
#80868 = CYLINDRICAL_SURFACE ( 'NONE', #38687, 0.5000000000000004441 ) ;
#80869 = LINE ( 'NONE', #70016, #139551 ) ;
#80870 = ORIENTED_EDGE ( 'NONE', *, *, #131378, .F. ) ;
#80871 = EDGE_CURVE ( 'NONE', #36504, #101734, #40298, .T. ) ;
#80872 = FACE_BOUND ( 'NONE', #24574, .T. ) ;
#80873 = LINE ( 'NONE', #66426, #29327 ) ;
#80874 = DIRECTION ( 'NONE',  ( 1.000000000000000000, 0.000000000000000000, 0.000000000000000000 ) ) ;
#80875 = DIRECTION ( 'NONE',  ( -1.000000000000000000, -0.000000000000000000, -0.000000000000000000 ) ) ;
#80876 = CARTESIAN_POINT ( 'NONE',  ( -30.29974487139158867, -27.71228299555227537, 4.000000000000000000 ) ) ;
#80877 = EDGE_CURVE ( 'NONE', #111536, #70500, #104805, .T. ) ;
#80878 = CARTESIAN_POINT ( 'NONE',  ( 94.86850992298123231, -32.76500000000005031, 11.45999999999952657 ) ) ;
#80879 = ORIENTED_EDGE ( 'NONE', *, *, #91771, .T. ) ;
#80880 = VERTEX_POINT ( 'NONE', #4716 ) ;
#80881 = CARTESIAN_POINT ( 'NONE',  ( 90.03709685856478018, -3.054999999999998828, -5.291415217122919401 ) ) ;
#80882 = ORIENTED_EDGE ( 'NONE', *, *, #64279, .T. ) ;
#80883 = EDGE_CURVE ( 'NONE', #41591, #38790, #62752, .T. ) ;
#80884 = FACE_OUTER_BOUND ( 'NONE', #39724, .T. ) ;
#80885 = FACE_OUTER_BOUND ( 'NONE', #96970, .T. ) ;
#80886 = CARTESIAN_POINT ( 'NONE',  ( 2.962472949537105826, -7.464222240803106570E-16, -6.094999999999989981 ) ) ;
#80887 = CARTESIAN_POINT ( 'NONE',  ( -32.01844734635648848, 18.75929247661553134, 20.33588619593450630 ) ) ;
#80888 = ORIENTED_EDGE ( 'NONE', *, *, #106887, .F. ) ;
#80889 = LINE ( 'NONE', #127214, #13591 ) ;
#80890 = DIRECTION ( 'NONE',  ( 0.7071067811865487940, 0.7071067811865463515, -0.000000000000000000 ) ) ;
#80891 = LINE ( 'NONE', #69304, #22999 ) ;
#80892 = VECTOR ( 'NONE', #83389, 1000.000000000000000 ) ;
#80893 = VECTOR ( 'NONE', #46766, 1000.000000000000000 ) ;
#80894 = CARTESIAN_POINT ( 'NONE',  ( -33.32816939922329880, -0.7407075233842822515, 4.000000000000000000 ) ) ;
#80895 = AXIS2_PLACEMENT_3D ( 'NONE', #100446, #21458, #109884 ) ;
#80896 = ORIENTED_EDGE ( 'NONE', *, *, #99339, .F. ) ;
#80897 = DIRECTION ( 'NONE',  ( 0.7071067811865487940, -0.7071067811865463515, 0.000000000000000000 ) ) ;
#80898 = DIRECTION ( 'NONE',  ( 0.7071067811865487940, 0.7071067811865463515, -0.000000000000000000 ) ) ;
#80899 = VECTOR ( 'NONE', #94052, 1000.000000000000000 ) ;
#80900 = ORIENTED_EDGE ( 'NONE', *, *, #52142, .T. ) ;
#80901 = ORIENTED_EDGE ( 'NONE', *, *, #3240, .T. ) ;
#80902 = VERTEX_POINT ( 'NONE', #38843 ) ;
#80903 = CARTESIAN_POINT ( 'NONE',  ( 43.89626352523143282, 4.472830434245840259, -4.472830434245838482 ) ) ;
#80904 = ORIENTED_EDGE ( 'NONE', *, *, #8812, .T. ) ;
#80905 = CIRCLE ( 'NONE', #64753, 2.500000000000000444 ) ;
#80906 = CARTESIAN_POINT ( 'NONE',  ( 9.087472949537108491, -6.094999999999989981, 3.732111120401553285E-16 ) ) ;
#80907 = CYLINDRICAL_SURFACE ( 'NONE', #118919, 0.5000000000000004441 ) ;
#80908 = VERTEX_POINT ( 'NONE', #82361 ) ;
#80909 = CARTESIAN_POINT ( 'NONE',  ( -2.207106781186527478, 9.759292476615625489, 5.000000000000000000 ) ) ;
#80910 = ORIENTED_EDGE ( 'NONE', *, *, #123216, .T. ) ;
#80911 = PRESENTATION_STYLE_ASSIGNMENT (( #71459 ) ) ;
#80912 =( GEOMETRIC_REPRESENTATION_CONTEXT ( 3 ) GLOBAL_UNCERTAINTY_ASSIGNED_CONTEXT ( ( #34787 ) ) GLOBAL_UNIT_ASSIGNED_CONTEXT ( ( #94824, #51366, #40498 ) ) REPRESENTATION_CONTEXT ( 'NONE', 'WORKASPACE' ) );
#80913 = AXIS2_PLACEMENT_3D ( 'NONE', #92313, #133711, #81495 ) ;
#80915 = VERTEX_POINT ( 'NONE', #6164 ) ;
#80914 = CARTESIAN_POINT ( 'NONE',  ( 29.99451991528749417, 28.92564299267958816, 4.000000000000000000 ) ) ;
#80916 = VERTEX_POINT ( 'NONE', #50441 ) ;
#80918 = EDGE_CURVE ( 'NONE', #32917, #36959, #115638, .T. ) ;
#80917 =( BOUNDED_CURVE ( )  B_SPLINE_CURVE ( 3, ( #132919, #78507, #133611, #98119 ),
 .UNSPECIFIED., .F., .F. ) 
 B_SPLINE_CURVE_WITH_KNOTS ( ( 4, 4 ),
 ( 1.208578181583236821, 1.359146454359402734 ),
 .UNSPECIFIED. ) 
 CURVE ( )  GEOMETRIC_REPRESENTATION_ITEM ( )  RATIONAL_B_SPLINE_CURVE ( ( 1.000000000000000000, 0.9981116584018963067, 0.9981116584018963067, 1.000000000000000000 ) ) 
 REPRESENTATION_ITEM ( '' )  );
#80919 = CARTESIAN_POINT ( 'NONE',  ( -1.499999999999982236, 12.05218569542904561, 5.000000000000000000 ) ) ;
#80920 = LINE ( 'NONE', #57755, #120105 ) ;
#80921 = CARTESIAN_POINT ( 'NONE',  ( -13.49999999999990585, -17.91344420646044000, 1.358650452708432654 ) ) ;
#80922 = ORIENTED_EDGE ( 'NONE', *, *, #15329, .T. ) ;
#80923 = AXIS2_PLACEMENT_3D ( 'NONE', #24817, #69060, #113240 ) ;
#80924 = EDGE_CURVE ( 'NONE', #71113, #82851, #5465, .T. ) ;
#80925 = CARTESIAN_POINT ( 'NONE',  ( -66.18398860626901126, 28.73617430169833753, 5.000000000000000000 ) ) ;
#80926 = VERTEX_POINT ( 'NONE', #28697 ) ;
#80927 = ORIENTED_EDGE ( 'NONE', *, *, #82792, .F. ) ;
#80928 = ORIENTED_EDGE ( 'NONE', *, *, #31562, .F. ) ;
#80929 = CARTESIAN_POINT ( 'NONE',  ( 5.292893218813423672, -6.740707523384216415, 5.000000000000000000 ) ) ;
#80930 = VECTOR ( 'NONE', #36444, 1000.000000000000114 ) ;
#80931 = AXIS2_PLACEMENT_3D ( 'NONE', #46616, #90044, #3038 ) ;
#80932 = DIRECTION ( 'NONE',  ( 0.3543493200069162685, -0.000000000000000000, -0.9351131265310288487 ) ) ;
#80933 = AXIS2_PLACEMENT_3D ( 'NONE', #73301, #84197, #18146 ) ;
#80934 = CARTESIAN_POINT ( 'NONE',  ( 30.48921356237309510, -27.52281430457076894, 5.000000000000000000 ) ) ;
#80935 = CARTESIAN_POINT ( 'NONE',  ( -42.48921356237308800, -27.52281430457085065, 5.000000000000000000 ) ) ;
#80936 = ADVANCED_FACE ( 'NONE', ( #109071 ), #119928, .F. ) ;
#80937 = DIRECTION ( 'NONE',  ( -0.6830127018922181881, 0.6830127018922202975, -0.2588190451025214056 ) ) ;
#80938 = ORIENTED_EDGE ( 'NONE', *, *, #140769, .T. ) ;
#80939 = AXIS2_PLACEMENT_3D ( 'NONE', #41039, #19286, #63544 ) ;
#80940 = FACE_OUTER_BOUND ( 'NONE', #128620, .T. ) ;
#80941 = CARTESIAN_POINT ( 'NONE',  ( 27.24956980810188867, 3.967499999999998916, 6.871911579029510442 ) ) ;
#80942 = CARTESIAN_POINT ( 'NONE',  ( -1.773258392821650098, -11.24070752338416135, 18.24660765846982358 ) ) ;
#80943 = DIRECTION ( 'NONE',  ( -0.000000000000000000, 0.3543493200069153248, 0.9351131265310292928 ) ) ;
#80944 = DIRECTION ( 'NONE',  ( 0.7071067811865486830, -0.7071067811865464625, -0.000000000000000000 ) ) ;
#80945 = ORIENTED_EDGE ( 'NONE', *, *, #29920, .F. ) ;
#80946 = VERTEX_POINT ( 'NONE', #66317 ) ;
#80947 = ORIENTED_EDGE ( 'NONE', *, *, #83540, .F. ) ;
#80948 = DIRECTION ( 'NONE',  ( 0.7071067811865486830, -0.7071067811865464625, -0.000000000000000000 ) ) ;
#80949 = CARTESIAN_POINT ( 'NONE',  ( 14.99451991528749595, 28.92564299267948513, 4.000000000000000000 ) ) ;
#80950 = VECTOR ( 'NONE', #91998, 1000.000000000000000 ) ;
#80951 = DIRECTION ( 'NONE',  ( -0.7071067811865487940, 0.7071067811865463515, -0.000000000000000000 ) ) ;
#80952 = FACE_OUTER_BOUND ( 'NONE', #108650, .T. ) ;
#80953 = CARTESIAN_POINT ( 'NONE',  ( 16.49999999999987921, -20.56887692260760758, 4.000000000000000000 ) ) ;
#80954 = CARTESIAN_POINT ( 'NONE',  ( 7.435109797308763646, 8.912112549869320333, -3.296747536672480550 ) ) ;
#80955 = DIRECTION ( 'NONE',  ( 0.7071067811865487940, -0.7071067811865463515, 0.000000000000000000 ) ) ;
#80956 = LINE ( 'NONE', #115667, #52960 ) ;
#80957 = CARTESIAN_POINT ( 'NONE',  ( 36.29974487139159578, -27.71228299555231445, 4.000000000000000000 ) ) ;
#80958 = CARTESIAN_POINT ( 'NONE',  ( -10.49999999999992184, 3.431123077392145948, 4.000000000000000000 ) ) ;
#80959 = CARTESIAN_POINT ( 'NONE',  ( 14.70025512860841133, -27.71228299555195917, 4.000000000000000000 ) ) ;
#80960 = FACE_OUTER_BOUND ( 'NONE', #86939, .T. ) ;
#80961 = ORIENTED_EDGE ( 'NONE', *, *, #78698, .T. ) ;
#80962 = EDGE_CURVE ( 'NONE', #31098, #129128, #140983, .T. ) ;
#80963 = VERTEX_POINT ( 'NONE', #9765 ) ;
#80964 = DIRECTION ( 'NONE',  ( 0.000000000000000000, -1.000000000000000000, 0.000000000000000000 ) ) ;
#80966 = ORIENTED_EDGE ( 'NONE', *, *, #80544, .F. ) ;
#80965 = CARTESIAN_POINT ( 'NONE',  ( 6.640000000000060965, 12.19802518668051583, 4.711086268963014412 ) ) ;
#80967 = DIRECTION ( 'NONE',  ( 0.000000000000000000, 0.000000000000000000, 1.000000000000000000 ) ) ;
#80968 = CARTESIAN_POINT ( 'NONE',  ( 12.45983838949732281, 18.75929247661552779, 8.305906642995514844 ) ) ;
#80969 = EDGE_CURVE ( 'NONE', #74762, #131532, #143142, .T. ) ;
#80970 = ORIENTED_EDGE ( 'NONE', *, *, #126098, .T. ) ;
#80971 = DIRECTION ( 'NONE',  ( -0.7071067811865486830, -0.7071067811865464625, 0.000000000000000000 ) ) ;
#80972 = VERTEX_POINT ( 'NONE', #52560 ) ;
#80973 = VERTEX_POINT ( 'NONE', #42438 ) ;
#80974 = CARTESIAN_POINT ( 'NONE',  ( -39.29974487139159578, -27.71228299555233576, 4.000000000000000000 ) ) ;
#80975 = EDGE_CURVE ( 'NONE', #119393, #108094, #63385, .T. ) ;
#80977 = EDGE_CURVE ( 'NONE', #47233, #30840, #85905, .T. ) ;
#80976 = CARTESIAN_POINT ( 'NONE',  ( 102.0166937171295558, 7.950000000000001066, -2.130196079827421318 ) ) ;
#80978 = DIRECTION ( 'NONE',  ( 0.7071067811865487940, -0.7071067811865463515, 0.000000000000000000 ) ) ;
#80980 = EDGE_CURVE ( 'NONE', #79052, #97544, #130145, .T. ) ;
#80979 = ORIENTED_EDGE ( 'NONE', *, *, #81230, .T. ) ;
#80981 = PLANE ( 'NONE',  #42358 ) ;
#80982 = CARTESIAN_POINT ( 'NONE',  ( 19.41972383043609440, 2.500000000000000444, 0.000000000000000000 ) ) ;
#80983 = EDGE_CURVE ( 'NONE', #32103, #76991, #96742, .T. ) ;
#80984 = DIRECTION ( 'NONE',  ( -0.7071067811865487940, 0.7071067811865463515, 0.000000000000000000 ) ) ;
#80985 = CARTESIAN_POINT ( 'NONE',  ( 25.81250000000000000, -4.461849672132299993, -4.461849672132299105 ) ) ;
#80986 = DIRECTION ( 'NONE',  ( -0.7071067811865486830, -0.7071067811865464625, -0.000000000000000000 ) ) ;
#80987 = PLANE ( 'NONE',  #111423 ) ;
#80989 = ADVANCED_FACE ( 'NONE', ( #98223 ), #107650, .T. ) ;
#80988 = LINE ( 'NONE', #91165, #117205 ) ;
#80990 = EDGE_LOOP ( 'NONE', ( #21538, #117850, #97936, #67444 ) ) ;
#80991 = PLANE ( 'NONE',  #106830 ) ;
#80993 = EDGE_LOOP ( 'NONE', ( #7061, #56035, #87934, #142439, #69338, #71900 ) ) ;
#80992 = EDGE_CURVE ( 'NONE', #83227, #130423, #97481, .T. ) ;
#80994 = CARTESIAN_POINT ( 'NONE',  ( 95.22959685856474721, -6.110000000000000320, -1.637169565754161393 ) ) ;
#80995 = DIRECTION ( 'NONE',  ( -0.000000000000000000, -0.3543493200069152693, 0.9351131265310292928 ) ) ;
#80996 = DIRECTION ( 'NONE',  ( -1.000000000000000000, -1.224606353822377258E-16, -0.000000000000000000 ) ) ;
#80997 = VECTOR ( 'NONE', #58269, 1000.000000000000000 ) ;
#80998 = LINE ( 'NONE', #127333, #77070 ) ;
#80999 = CARTESIAN_POINT ( 'NONE',  ( 31.49999999999978684, -9.462702396500981550, -9.474982329943586024 ) ) ;
#81000 = ORIENTED_EDGE ( 'NONE', *, *, #56820, .F. ) ;
#81001 = AXIS2_PLACEMENT_3D ( 'NONE', #76281, #98026, #128516 ) ;
#81002 = CONICAL_SURFACE ( 'NONE', #125060, 2.500000000000000888, 0.9599310885968822538 ) ;
#81003 = VECTOR ( 'NONE', #141547, 999.9999999999998863 ) ;
#81004 = LINE ( 'NONE', #36076, #109056 ) ;
#81005 = AXIS2_PLACEMENT_3D ( 'NONE', #81455, #2397, #35814 ) ;
#81006 = ADVANCED_FACE ( 'NONE', ( #30841 ), #44594, .F. ) ;
#81007 = DIRECTION ( 'NONE',  ( -1.000000000000000000, -1.155222954767600912E-14, 0.000000000000000000 ) ) ;
#81008 = ORIENTED_EDGE ( 'NONE', *, *, #86207, .F. ) ;
#81009 = ADVANCED_FACE ( 'NONE', ( #41691 ), #30088, .F. ) ;
#81010 = FACE_OUTER_BOUND ( 'NONE', #128023, .T. ) ;
#81012 = EDGE_LOOP ( 'NONE', ( #115760, #56174, #7946, #53659 ) ) ;
#81011 = DIRECTION ( 'NONE',  ( -0.000000000000000000, -0.3543493200069152693, 0.9351131265310292928 ) ) ;
#81013 = LINE ( 'NONE', #37511, #4269 ) ;
#81014 = LINE ( 'NONE', #125219, #8225 ) ;
#81015 = DIRECTION ( 'NONE',  ( -0.7071067811865486830, 0.7071067811865464625, 0.000000000000000000 ) ) ;
#81016 = VECTOR ( 'NONE', #128064, 1000.000000000000227 ) ;
#81017 = EDGE_CURVE ( 'NONE', #123046, #116750, #8310, .T. ) ;
#81018 = FACE_OUTER_BOUND ( 'NONE', #37493, .T. ) ;
#81019 = ORIENTED_EDGE ( 'NONE', *, *, #97157, .F. ) ;
#81020 = EDGE_LOOP ( 'NONE', ( #139945, #73349, #15230, #115299 ) ) ;
#81021 = ORIENTED_EDGE ( 'NONE', *, *, #63399, .F. ) ;
#81022 = CARTESIAN_POINT ( 'NONE',  ( 87.06293019189807580, 1.637169565754157174, 6.110000000000002984 ) ) ;
#81023 = CIRCLE ( 'NONE', #90202, 1.000000000000000888 ) ;
#81024 = ORIENTED_EDGE ( 'NONE', *, *, #83966, .F. ) ;
#81025 = CARTESIAN_POINT ( 'NONE',  ( -23.93182425469048979, -0.2601698552150356059, 4.222180570310114511 ) ) ;
#81026 = CIRCLE ( 'NONE', #11529, 2.500000000000000888 ) ;
#81027 = VECTOR ( 'NONE', #19698, 1000.000000000000000 ) ;
#81028 = LINE ( 'NONE', #94008, #138346 ) ;
#81029 = CARTESIAN_POINT ( 'NONE',  ( -33.88837638105221117, 9.759292476615614831, 17.35367589129220534 ) ) ;
#81030 = ORIENTED_EDGE ( 'NONE', *, *, #76961, .T. ) ;
#81031 = DIRECTION ( 'NONE',  ( 1.000000000000000000, 0.000000000000000000, 0.000000000000000000 ) ) ;
#81032 = PLANE ( 'NONE',  #109117 ) ;
#81033 = AXIS2_PLACEMENT_3D ( 'NONE', #2697, #69423, #25898 ) ;
#81034 = CARTESIAN_POINT ( 'NONE',  ( 75.74543019189810877, -5.291415217122918513, -3.055000000000000160 ) ) ;
#81035 = ORIENTED_EDGE ( 'NONE', *, *, #33590, .F. ) ;
#81036 = DIRECTION ( 'NONE',  ( 0.7071067811865487940, 0.7071067811865463515, -0.000000000000000000 ) ) ;
#81037 = EDGE_CURVE ( 'NONE', #79690, #124291, #121286, .T. ) ;
#81038 = LINE ( 'NONE', #132028, #131190 ) ;
#81039 = LINE ( 'NONE', #37535, #91004 ) ;
#81040 = AXIS2_PLACEMENT_3D ( 'NONE', #75839, #75146, #121459 ) ;
#81041 = AXIS2_PLACEMENT_3D ( 'NONE', #20328, #53719, #66031 ) ;
#81042 = VERTEX_POINT ( 'NONE', #88057 ) ;
#81043 = ORIENTED_EDGE ( 'NONE', *, *, #8329, .T. ) ;
#81044 = LINE ( 'NONE', #27334, #127965 ) ;
#81045 = AXIS2_PLACEMENT_3D ( 'NONE', #90716, #56691, #32769 ) ;
#81046 = LINE ( 'NONE', #33970, #103308 ) ;
#81047 = CARTESIAN_POINT ( 'NONE',  ( 23.54623647476855552, -7.934999999999990727, 4.858786175617117713E-16 ) ) ;
#81048 = CARTESIAN_POINT ( 'NONE',  ( -11.99999999999992006, -0.2811185226894441502, -5.995736974527487106 ) ) ;
#81049 = AXIS2_PLACEMENT_3D ( 'NONE', #10197, #123811, #121103 ) ;
#81050 = DIRECTION ( 'NONE',  ( 0.000000000000000000, 0.000000000000000000, -1.000000000000000000 ) ) ;
#81051 = EDGE_CURVE ( 'NONE', #94676, #57817, #10468, .T. ) ;
#81052 = DIRECTION ( 'NONE',  ( -0.3543493200069162685, -0.000000000000000000, -0.9351131265310288487 ) ) ;
#81053 = LINE ( 'NONE', #49143, #9488 ) ;
#81054 = AXIS2_PLACEMENT_3D ( 'NONE', #123517, #24172, #68426 ) ;
#81055 = ORIENTED_EDGE ( 'NONE', *, *, #36533, .T. ) ;
#81056 = ORIENTED_EDGE ( 'NONE', *, *, #92112, .T. ) ;
#81057 = LINE ( 'NONE', #101355, #103532 ) ;
#81058 = EDGE_CURVE ( 'NONE', #4187, #97296, #118528, .T. ) ;
#81059 = EDGE_LOOP ( 'NONE', ( #3299, #77762, #38606, #109249 ) ) ;
#81060 = AXIS2_PLACEMENT_3D ( 'NONE', #47336, #91506, #135717 ) ;
#81061 = PLANE ( 'NONE',  #35837 ) ;
#81062 = ORIENTED_EDGE ( 'NONE', *, *, #49297, .T. ) ;
#81063 = CARTESIAN_POINT ( 'NONE',  ( 2.999999999999985345, 5.966399257802200040, 5.000000000000000000 ) ) ;
#81064 = CARTESIAN_POINT ( 'NONE',  ( -53.99451991528749062, 28.92564299267975869, 4.000000000000000000 ) ) ;
#81065 = EDGE_CURVE ( 'NONE', #23940, #71937, #294, .T. ) ;
#81066 = CARTESIAN_POINT ( 'NONE',  ( 32.53839644629409378, -9.740707523384184441, 17.74957260769618728 ) ) ;
#81067 = CARTESIAN_POINT ( 'NONE',  ( -22.49999999999984723, -10.53360074219763121, 5.000000000000000000 ) ) ;
#81068 = VECTOR ( 'NONE', #140273, 1000.000000000000000 ) ;
#81069 = CARTESIAN_POINT ( 'NONE',  ( 19.49999999999986855, 19.39370406404968605, 1.459788787078156513 ) ) ;
#81070 = VERTEX_POINT ( 'NONE', #31537 ) ;
#81071 = FACE_OUTER_BOUND ( 'NONE', #73369, .T. ) ;
#81072 = LINE ( 'NONE', #94056, #44261 ) ;
#81073 = ORIENTED_EDGE ( 'NONE', *, *, #29370, .F. ) ;
#81075 = ADVANCED_FACE ( 'NONE', ( #19228 ), #63484, .F. ) ;
#81074 = DIRECTION ( 'NONE',  ( 0.7071067811865487940, -0.7071067811865463515, 0.000000000000000000 ) ) ;
#81076 = ORIENTED_EDGE ( 'NONE', *, *, #115252, .T. ) ;
#81077 = VERTEX_POINT ( 'NONE', #35126 ) ;
#81078 = LINE ( 'NONE', #80374, #131511 ) ;
#81079 = VERTEX_POINT ( 'NONE', #135159 ) ;
#81080 = ORIENTED_EDGE ( 'NONE', *, *, #17745, .F. ) ;
#81081 = CARTESIAN_POINT ( 'NONE',  ( -5.292893218813415679, -18.74070752338409562, 5.000000000000000000 ) ) ;
#81083 = ORIENTED_EDGE ( 'NONE', *, *, #68943, .F. ) ;
#81082 = AXIS2_PLACEMENT_3D ( 'NONE', #25126, #125174, #80967 ) ;
#81084 = CARTESIAN_POINT ( 'NONE',  ( 94.62500000000000000, -7.950000000000000178, -4.867971026610729436E-16 ) ) ;
#81085 = CARTESIAN_POINT ( 'NONE',  ( -2.576721541936451310, 11.25929247661560240, 17.85071094206585229 ) ) ;
#81086 = CARTESIAN_POINT ( 'NONE',  ( 115.7920968585647756, -5.291415217122921177, 3.054999999999999272 ) ) ;
#81087 = CARTESIAN_POINT ( 'NONE',  ( 36.18398860626899705, 28.73617430169812437, 5.000000000000000000 ) ) ;
#81088 = LINE ( 'NONE', #13646, #99121 ) ;
#81089 = LINE ( 'NONE', #80386, #2685 ) ;
#81090 = CARTESIAN_POINT ( 'NONE',  ( 15.48921356237309510, -27.52281430457066236, 5.000000000000000000 ) ) ;
#81091 = CARTESIAN_POINT ( 'NONE',  ( 16.75173015016484968, 2.055000000000001048, 2.516649172247811554E-16 ) ) ;
#81092 = EDGE_CURVE ( 'NONE', #89124, #127280, #56890, .T. ) ;
#81093 = DIRECTION ( 'NONE',  ( -0.6830127018922181881, 0.6830127018922202975, -0.2588190451025214056 ) ) ;
#81094 = LINE ( 'NONE', #127426, #106133 ) ;
#81096 = EDGE_LOOP ( 'NONE', ( #85543, #73587, #78709, #29823 ) ) ;
#81095 = VECTOR ( 'NONE', #50604, 1000.000000000000227 ) ;
#81097 = EDGE_CURVE ( 'NONE', #139613, #16650, #2437, .T. ) ;
#81098 = DIRECTION ( 'NONE',  ( -0.000000000000000000, -0.3543493200069152693, 0.9351131265310292928 ) ) ;
#81099 = CARTESIAN_POINT ( 'NONE',  ( 21.29974487139158512, -27.71228299555221142, 4.000000000000000000 ) ) ;
#81100 = ORIENTED_EDGE ( 'NONE', *, *, #116592, .F. ) ;
#81101 = ORIENTED_EDGE ( 'NONE', *, *, #897, .T. ) ;
#81102 = DIRECTION ( 'NONE',  ( 0.7071067811865486830, -0.7071067811865464625, -0.000000000000000000 ) ) ;
#81103 = VECTOR ( 'NONE', #98909, 1000.000000000000000 ) ;
#81104 = VERTEX_POINT ( 'NONE', #36525 ) ;
#81105 = VECTOR ( 'NONE', #94982, 1000.000000000000000 ) ;
#81106 = AXIS2_PLACEMENT_3D ( 'NONE', #94776, #30251, #61500 ) ;
#81107 = CARTESIAN_POINT ( 'NONE',  ( 27.18398860626900060, 28.73617430169806042, 5.000000000000000000 ) ) ;
#81108 = DIRECTION ( 'NONE',  ( 0.000000000000000000, -1.000000000000000000, 0.000000000000000000 ) ) ;
#81109 = LINE ( 'NONE', #12951, #59537 ) ;
#81110 = CARTESIAN_POINT ( 'NONE',  ( 23.53839644629415062, -9.740707523384177335, 17.74957260769616241 ) ) ;
#81111 = EDGE_CURVE ( 'NONE', #9966, #77074, #14803, .T. ) ;
#81112 = DIRECTION ( 'NONE',  ( -0.7071067811865487940, 0.7071067811865463515, 0.000000000000000000 ) ) ;
#81113 = VERTEX_POINT ( 'NONE', #1706 ) ;
#81114 = FACE_OUTER_BOUND ( 'NONE', #107505, .T. ) ;
#81116 = ORIENTED_EDGE ( 'NONE', *, *, #95198, .F. ) ;
#81115 = VECTOR ( 'NONE', #43538, 1000.000000000000000 ) ;
#81117 = DIRECTION ( 'NONE',  ( -0.7071067811865487940, 0.7071067811865463515, 0.000000000000000000 ) ) ;
#81118 = CARTESIAN_POINT ( 'NONE',  ( 26.31706980810189123, -2.126176841940956130, 7.934999999999991616 ) ) ;
#81119 = CARTESIAN_POINT ( 'NONE',  ( 0.3281693992235254487, 2.259292476615687661, 4.000000000000000000 ) ) ;
#81120 = CARTESIAN_POINT ( 'NONE',  ( 98.80836038379622721, 7.949999999999996625, 2.130196079827431088 ) ) ;
#81121 = ORIENTED_EDGE ( 'NONE', *, *, #55796, .F. ) ;
#81122 = VERTEX_POINT ( 'NONE', #112656 ) ;
#81123 = ORIENTED_EDGE ( 'NONE', *, *, #65488, .T. ) ;
#81125 = VECTOR ( 'NONE', #61542, 1000.000000000000227 ) ;
#81124 = CARTESIAN_POINT ( 'NONE',  ( -34.92382263987071411, 21.75929247661549226, 4.252424926123421933 ) ) ;
#81126 = LINE ( 'NONE', #5656, #134396 ) ;
#81127 = CARTESIAN_POINT ( 'NONE',  ( -7.499999999999944045, -13.53360074219760101, 5.000000000000000000 ) ) ;
#81128 = DIRECTION ( 'NONE',  ( -0.7071067811865487940, 0.7071067811865463515, -0.000000000000000000 ) ) ;
#81129 = EDGE_LOOP ( 'NONE', ( #96298, #85122, #76701, #133174 ) ) ;
#81130 = DIRECTION ( 'NONE',  ( 0.7071067811865486830, -0.7071067811865464625, -0.000000000000000000 ) ) ;
#81131 = CARTESIAN_POINT ( 'NONE',  ( 0.000000000000000000, -14.29000000000013593, 12.69999999999954632 ) ) ;
#81132 = VECTOR ( 'NONE', #103967, 1000.000000000000000 ) ;
#81133 = AXIS2_PLACEMENT_3D ( 'NONE', #58832, #102300, #37010 ) ;
#81134 = DIRECTION ( 'NONE',  ( 0.6830127018922180770, -0.6830127018922204085, -0.2588190451025213501 ) ) ;
#81135 = CARTESIAN_POINT ( 'NONE',  ( 27.32816939922334143, -18.74070752338409562, 4.000000000000000000 ) ) ;
#81136 = AXIS2_PLACEMENT_3D ( 'NONE', #56930, #103242, #122866 ) ;
#81137 = VERTEX_POINT ( 'NONE', #90179 ) ;
#81139 = AXIS2_PLACEMENT_3D ( 'NONE', #85048, #6723, #131422 ) ;
#81138 = DIRECTION ( 'NONE',  ( 0.000000000000000000, 0.000000000000000000, 1.000000000000000000 ) ) ;
#81140 = VERTEX_POINT ( 'NONE', #111206 ) ;
#81142 = ORIENTED_EDGE ( 'NONE', *, *, #4742, .F. ) ;
#81141 = DIRECTION ( 'NONE',  ( 0.7071067811865487940, -0.7071067811865463515, 0.000000000000000000 ) ) ;
#81143 = ORIENTED_EDGE ( 'NONE', *, *, #4833, .T. ) ;
#81144 = FACE_OUTER_BOUND ( 'NONE', #83012, .T. ) ;
#81145 = CARTESIAN_POINT ( 'NONE',  ( 105.1250000000000000, -7.950000000000000178, -4.867971026610729436E-16 ) ) ;
#81146 = VERTEX_POINT ( 'NONE', #90931 ) ;
#81147 = UNCERTAINTY_MEASURE_WITH_UNIT (LENGTH_MEASURE( 1.000000000000000082E-05 ), #13492, 'distance_accuracy_value', 'NONE');
#81148 = CARTESIAN_POINT ( 'NONE',  ( 27.70710678118635428, 11.25929247661560062, 5.000000000000000000 ) ) ;
#81149 = CARTESIAN_POINT ( 'NONE',  ( 17.99451991528748351, 28.92564299267950645, 4.000000000000000000 ) ) ;
#81151 = EDGE_CURVE ( 'NONE', #83013, #101443, #120957, .T. ) ;
#81150 = CARTESIAN_POINT ( 'NONE',  ( 29.95376352523145158, -6.109999999999999432, -3.741295971395163529E-16 ) ) ;
#81152 = CARTESIAN_POINT ( 'NONE',  ( -16.49999999999988276, -7.533600742197656963, 5.000000000000000000 ) ) ;
#81153 = VECTOR ( 'NONE', #85847, 1000.000000000000000 ) ;
#81154 = DIRECTION ( 'NONE',  ( 0.000000000000000000, 0.3543493200069153248, 0.9351131265310291818 ) ) ;
#81155 = EDGE_CURVE ( 'NONE', #123895, #9541, #12619, .T. ) ;
#81156 = DIRECTION ( 'NONE',  ( -1.000000000000000000, -1.224606353822377258E-16, -0.000000000000000000 ) ) ;
#81157 = CARTESIAN_POINT ( 'NONE',  ( 0.000000000000000000, 0.000000000000000000, 5.000000000000000000 ) ) ;
#81158 = ADVANCED_FACE ( 'NONE', ( #80070 ), #122088, .T. ) ;
#81159 = PLANE ( 'NONE',  #134025 ) ;
#81161 = VECTOR ( 'NONE', #129642, 1000.000000000000000 ) ;
#81160 = CARTESIAN_POINT ( 'NONE',  ( 31.62456980810188867, -6.871911579029512218, 3.967499999999996252 ) ) ;
#81162 = CARTESIAN_POINT ( 'NONE',  ( 1.291236474768552966, -9.717572351234235426E-16, -7.934999999999990727 ) ) ;
#81163 = DIRECTION ( 'NONE',  ( 1.000000000000000000, 0.000000000000000000, 0.000000000000000000 ) ) ;
#81164 = CARTESIAN_POINT ( 'NONE',  ( -36.48921356237310221, -27.52281430457080802, 5.000000000000000000 ) ) ;
#81166 = EDGE_CURVE ( 'NONE', #36536, #33570, #114082, .T. ) ;
#81165 = LINE ( 'NONE', #126092, #96296 ) ;
#81167 = ORIENTED_EDGE ( 'NONE', *, *, #44381, .F. ) ;
#81168 = EDGE_LOOP ( 'NONE', ( #138808, #134354, #88717, #32292 ) ) ;
#81169 = CARTESIAN_POINT ( 'NONE',  ( 93.31249999999997158, 5.819803920172571310, 5.819803920172575751 ) ) ;
#81170 = ORIENTED_EDGE ( 'NONE', *, *, #106090, .T. ) ;
#81171 = EDGE_LOOP ( 'NONE', ( #118613, #141248, #59727, #96978, #170 ) ) ;
#81172 = CARTESIAN_POINT ( 'NONE',  ( 18.70710678118642178, 17.25929247661554200, 5.000000000000000000 ) ) ;
#81173 = CARTESIAN_POINT ( 'NONE',  ( -5.510786437626906675, -27.52281430457051314, 5.000000000000000000 ) ) ;
#81174 = VECTOR ( 'NONE', #129039, 1000.000000000000000 ) ;
#81175 = DIRECTION ( 'NONE',  ( 0.000000000000000000, 0.000000000000000000, 1.000000000000000000 ) ) ;
#81176 = ORIENTED_EDGE ( 'NONE', *, *, #22497, .T. ) ;
#81177 = LINE ( 'NONE', #25336, #55579 ) ;
#81178 = CARTESIAN_POINT ( 'NONE',  ( 7.139999999999991687, -35.62922597241576739, -11.84864515520817640 ) ) ;
#81179 = EDGE_CURVE ( 'NONE', #42504, #123918, #133016, .T. ) ;
#81180 = DIRECTION ( 'NONE',  ( 0.6830127018922181881, 0.6830127018922202975, -0.2588190451025214056 ) ) ;
#81181 = CARTESIAN_POINT ( 'NONE',  ( 125.5994534179081796, -2.266258037075818077, -7.520521262005186003 ) ) ;
#81182 = EDGE_CURVE ( 'NONE', #138807, #17766, #67774, .T. ) ;
#81183 = PLANE ( 'NONE',  #7637 ) ;
#81184 = FACE_OUTER_BOUND ( 'NONE', #23380, .T. ) ;
#81185 = CARTESIAN_POINT ( 'NONE',  ( 25.39999999999999858, -14.29000000000013593, -12.70000000000045404 ) ) ;
#81186 = DIRECTION ( 'NONE',  ( 1.000000000000000000, 3.115803279706882722E-16, -0.000000000000000000 ) ) ;
#81187 = VECTOR ( 'NONE', #93644, 1000.000000000000000 ) ;
#81188 = DIRECTION ( 'NONE',  ( 0.3543493200069162685, -0.000000000000000000, -0.9351131265310288487 ) ) ;
#81189 = DIRECTION ( 'NONE',  ( 0.6830127018922181881, 0.6830127018922202975, -0.2588190451025214056 ) ) ;
#81190 = CIRCLE ( 'NONE', #62658, 28.00000000000002487 ) ;
#81191 = FACE_OUTER_BOUND ( 'NONE', #45141, .T. ) ;
#81192 = EDGE_CURVE ( 'NONE', #131602, #5802, #1017, .T. ) ;
#81193 = CARTESIAN_POINT ( 'NONE',  ( 0.000000000000000000, 0.000000000000000000, 5.000000000000000000 ) ) ;
#81194 = ORIENTED_EDGE ( 'NONE', *, *, #83500, .F. ) ;
#81195 = EDGE_LOOP ( 'NONE', ( #136616, #72, #58793, #76411 ) ) ;
#81196 = CARTESIAN_POINT ( 'NONE',  ( 109.9587635252314470, 0.000000000000000000, -6.110000000000001208 ) ) ;
#81197 = ORIENTED_EDGE ( 'NONE', *, *, #130159, .T. ) ;
#81198 = LINE ( 'NONE', #7136, #112718 ) ;
#81199 = EDGE_CURVE ( 'NONE', #119390, #73106, #122822, .T. ) ;
#81200 = DIRECTION ( 'NONE',  ( -0.7071067811865487940, 0.7071067811865463515, 0.000000000000000000 ) ) ;
#81201 = VERTEX_POINT ( 'NONE', #16157 ) ;
#81202 = AXIS2_PLACEMENT_3D ( 'NONE', #15067, #99388, #22539 ) ;
#81203 = LINE ( 'NONE', #37701, #102269 ) ;
#81204 = CARTESIAN_POINT ( 'NONE',  ( 5.510786437626906675, -27.52281430457051314, 5.000000000000000000 ) ) ;
#81205 = STYLED_ITEM ( 'NONE', ( #12210 ), #116870 ) ;
#81206 = AXIS2_PLACEMENT_3D ( 'NONE', #20548, #65550, #106854 ) ;
#81207 = CARTESIAN_POINT ( 'NONE',  ( 102.8704301918981230, -3.055000000000001492, 5.291415217122917625 ) ) ;
#81208 = ORIENTED_EDGE ( 'NONE', *, *, #86497, .F. ) ;
#81209 = VERTEX_POINT ( 'NONE', #82206 ) ;
#81211 = ADVANCED_FACE ( 'NONE', ( #94458 ), #105338, .F. ) ;
#81210 = CARTESIAN_POINT ( 'NONE',  ( 39.29974487139159578, -27.71228299555233576, 4.000000000000000000 ) ) ;
#81212 = AXIS2_PLACEMENT_3D ( 'NONE', #82725, #36364, #3682 ) ;
#81213 = AXIS2_PLACEMENT_3D ( 'NONE', #38180, #82396, #115677 ) ;
#81214 = CARTESIAN_POINT ( 'NONE',  ( 0.1839886062690032631, 28.73617430169787568, 5.000000000000000000 ) ) ;
#81215 = AXIS2_PLACEMENT_3D ( 'NONE', #36028, #27249, #136022 ) ;
#81216 = VECTOR ( 'NONE', #139341, 1000.000000000000114 ) ;
#81217 = LINE ( 'NONE', #39119, #54744 ) ;
#81218 = AXIS2_PLACEMENT_3D ( 'NONE', #72214, #52547, #140970 ) ;
#81219 = ORIENTED_EDGE ( 'NONE', *, *, #33671, .T. ) ;
#81220 = ORIENTED_EDGE ( 'NONE', *, *, #122546, .F. ) ;
#81221 = ORIENTED_EDGE ( 'NONE', *, *, #112792, .F. ) ;
#81222 = DIRECTION ( 'NONE',  ( 1.000000000000000000, 3.115803279706882722E-16, 0.000000000000000000 ) ) ;
#81223 = LINE ( 'NONE', #13766, #46138 ) ;
#81224 = CIRCLE ( 'NONE', #22, 2.055000000000000604 ) ;
#81225 = EDGE_CURVE ( 'NONE', #47109, #117707, #37241, .T. ) ;
#81226 = LINE ( 'NONE', #136287, #91651 ) ;
#81227 = ORIENTED_EDGE ( 'NONE', *, *, #23993, .T. ) ;
#81228 = ORIENTED_EDGE ( 'NONE', *, *, #138799, .T. ) ;
#81229 = DIRECTION ( 'NONE',  ( 1.000000000000000000, 0.000000000000000000, 0.000000000000000000 ) ) ;
#81231 = VERTEX_POINT ( 'NONE', #92309 ) ;
#81230 = EDGE_CURVE ( 'NONE', #37537, #57989, #50977, .T. ) ;
#81232 = ORIENTED_EDGE ( 'NONE', *, *, #55023, .T. ) ;
#81233 = AXIS2_PLACEMENT_3D ( 'NONE', #50471, #127296, #70122 ) ;
#81234 = CARTESIAN_POINT ( 'NONE',  ( 4.499999999999962697, 1.030536316426508670, -5.498701923753811727 ) ) ;
#81235 = AXIS2_PLACEMENT_3D ( 'NONE', #79981, #79277, #102433 ) ;
#81236 = AXIS2_PLACEMENT_3D ( 'NONE', #17676, #82272, #7519 ) ;
#81237 = CARTESIAN_POINT ( 'NONE',  ( 36.18398860626899705, 28.73617430169812437, 5.000000000000000000 ) ) ;
#81238 = VERTEX_POINT ( 'NONE', #137277 ) ;
#81239 = LINE ( 'NONE', #34877, #27465 ) ;
#81240 = ADVANCED_FACE ( 'NONE', ( #71311 ), #29206, .F. ) ;
#81241 = VECTOR ( 'NONE', #38550, 999.9999999999998863 ) ;
#81242 = FACE_OUTER_BOUND ( 'NONE', #87608, .T. ) ;
#81243 = VECTOR ( 'NONE', #129089, 1000.000000000000000 ) ;
#81244 = DIRECTION ( 'NONE',  ( -1.000000000000000000, -0.000000000000000000, 0.000000000000000000 ) ) ;
#81245 = CARTESIAN_POINT ( 'NONE',  ( 10.99806943317893726, -22.22500000000000142, 4.500000000000000888 ) ) ;
#81246 = FACE_BOUND ( 'NONE', #58836, .T. ) ;
#81247 = ORIENTED_EDGE ( 'NONE', *, *, #83419, .F. ) ;
#81248 = DIRECTION ( 'NONE',  ( 0.6830127018922180770, -0.6830127018922204085, -0.2588190451025213501 ) ) ;
#81250 = EDGE_CURVE ( 'NONE', #65792, #128178, #73449, .T. ) ;
#81249 = CARTESIAN_POINT ( 'NONE',  ( -5.999999999999963585, -16.06887692260763956, 4.000000000000000000 ) ) ;
#81251 = AXIS2_PLACEMENT_3D ( 'NONE', #90207, #46770, #81512 ) ;
#81252 = EDGE_LOOP ( 'NONE', ( #49601, #53980, #52752, #130881 ) ) ;
#81253 = LINE ( 'NONE', #59502, #57537 ) ;
#81254 = ORIENTED_EDGE ( 'NONE', *, *, #6792, .F. ) ;
#81255 = ORIENTED_EDGE ( 'NONE', *, *, #97767, .F. ) ;
#81256 = ORIENTED_EDGE ( 'NONE', *, *, #87459, .T. ) ;
#81257 = CARTESIAN_POINT ( 'NONE',  ( 37.53709685856478018, -3.054999999999998828, -5.291415217122919401 ) ) ;
#81258 = ORIENTED_EDGE ( 'NONE', *, *, #67133, .T. ) ;
#81259 = AXIS2_PLACEMENT_3D ( 'NONE', #48155, #61224, #105368 ) ;
#81260 = B_SPLINE_CURVE_WITH_KNOTS ( 'NONE', 3,
 ( #73275, #8658, #117442, #29726 ),
 .UNSPECIFIED., .F., .F.,
 ( 4, 4 ),
 ( 0.000000000000000000, 0.001115544020566869386 ),
 .UNSPECIFIED. ) ;
#81261 = CARTESIAN_POINT ( 'NONE',  ( 39.18398860626899705, 28.73617430169814568, 5.000000000000000000 ) ) ;
#81262 = SURFACE_SIDE_STYLE ('',( #37011 ) ) ;
#81263 = CARTESIAN_POINT ( 'NONE',  ( -7.499999999999940492, 1.087461875839228931, 4.000000000000000000 ) ) ;
#81264 = VERTEX_POINT ( 'NONE', #82901 ) ;
#81265 = DIRECTION ( 'NONE',  ( -1.000000000000000000, -0.000000000000000000, -0.000000000000000000 ) ) ;
#81267 = CARTESIAN_POINT ( 'NONE',  ( 25.39999999999999858, -30.18000000000009564, 15.92499999999935945 ) ) ;
#81266 = VECTOR ( 'NONE', #9255, 1000.000000000000227 ) ;
#81268 = DIRECTION ( 'NONE',  ( -0.7071067811865486830, 0.7071067811865464625, 0.000000000000000000 ) ) ;
#81269 = PLANE ( 'NONE',  #131957 ) ;
#81270 = ADVANCED_FACE ( 'NONE', ( #26373 ), #70627, .F. ) ;
#81271 = DIRECTION ( 'NONE',  ( 0.7071067811865486830, -0.7071067811865464625, -0.000000000000000000 ) ) ;
#81272 = CARTESIAN_POINT ( 'NONE',  ( 57.29974487139158157, -27.71228299555246011, 4.000000000000000000 ) ) ;
#81273 = ORIENTED_EDGE ( 'NONE', *, *, #52701, .T. ) ;
#81274 = ORIENTED_EDGE ( 'NONE', *, *, #115544, .T. ) ;
#81275 = ORIENTED_EDGE ( 'NONE', *, *, #121246, .T. ) ;
#81276 = AXIS2_PLACEMENT_3D ( 'NONE', #57772, #80236, #25092 ) ;
#81277 = EDGE_LOOP ( 'NONE', ( #40187, #15527, #39323, #139154 ) ) ;
#81278 = LINE ( 'NONE', #134957, #93443 ) ;
#81279 = ORIENTED_EDGE ( 'NONE', *, *, #69015, .F. ) ;
#81280 = VERTEX_POINT ( 'NONE', #136532 ) ;
#81281 = DIRECTION ( 'NONE',  ( 0.6830127018922181881, 0.6830127018922202975, -0.2588190451025214056 ) ) ;
#81282 = FACE_OUTER_BOUND ( 'NONE', #18646, .T. ) ;
#81283 = ADVANCED_FACE ( 'NONE', ( #62572 ), #72716, .T. ) ;
#81284 = EDGE_CURVE ( 'NONE', #103836, #126734, #104629, .T. ) ;
#81285 = CARTESIAN_POINT ( 'NONE',  ( -27.29974487139158512, -27.71228299555225405, 4.000000000000000000 ) ) ;
#81286 = ORIENTED_EDGE ( 'NONE', *, *, #31726, .F. ) ;
#81287 = CARTESIAN_POINT ( 'NONE',  ( 12.48921356237309155, -27.52281430457064104, 5.000000000000000000 ) ) ;
#81288 = VECTOR ( 'NONE', #132375, 1000.000000000000000 ) ;
#81289 = ORIENTED_EDGE ( 'NONE', *, *, #50610, .T. ) ;
#81290 = CARTESIAN_POINT ( 'NONE',  ( -15.70701326429294475, -21.74070752338406365, 4.999753212805219782 ) ) ;
#81291 = CARTESIAN_POINT ( 'NONE',  ( 42.48921356237308800, -27.52281430457085065, 5.000000000000000000 ) ) ;
#81292 = CARTESIAN_POINT ( 'NONE',  ( 3.567069808101885897, 2.126176841940952134, -7.934999999999993392 ) ) ;
#81293 = EDGE_LOOP ( 'NONE', ( #27423, #50771, #61709, #66115 ) ) ;
#81295 = DIRECTION ( 'NONE',  ( -0.3543493200069162685, -0.000000000000000000, -0.9351131265310288487 ) ) ;
#81294 = CARTESIAN_POINT ( 'NONE',  ( 97.91209685856478018, 5.291415217122922066, -3.054999999999995275 ) ) ;
#81296 = CARTESIAN_POINT ( 'NONE',  ( 17.39159235450332019, 9.902892378096218942E-16, 0.000000000000000000 ) ) ;
#81297 = ORIENTED_EDGE ( 'NONE', *, *, #109828, .T. ) ;
#81298 = ORIENTED_EDGE ( 'NONE', *, *, #12222, .F. ) ;
#81299 = DIRECTION ( 'NONE',  ( -0.7071067811865486830, -0.7071067811865464625, 0.000000000000000000 ) ) ;
#81300 = VERTEX_POINT ( 'NONE', #116226 ) ;
#81301 = DIRECTION ( 'NONE',  ( -0.7071067811865487940, 0.7071067811865463515, 0.000000000000000000 ) ) ;
#81302 = LINE ( 'NONE', #47285, #21918 ) ;
#81303 = VECTOR ( 'NONE', #6509, 1000.000000000000000 ) ;
#81304 = DIRECTION ( 'NONE',  ( -0.3543493200069162685, -0.000000000000000000, -0.9351131265310288487 ) ) ;
#81305 = ADVANCED_FACE ( 'NONE', ( #49578 ), #84345, .T. ) ;
#81306 = ORIENTED_EDGE ( 'NONE', *, *, #75026, .F. ) ;
#81307 = AXIS2_PLACEMENT_3D ( 'NONE', #23649, #100510, #57025 ) ;
#81308 = CARTESIAN_POINT ( 'NONE',  ( 45.48921356237309510, -27.52281430457087197, 5.000000000000000000 ) ) ;
#81309 = VECTOR ( 'NONE', #92595, 1000.000000000000000 ) ;
#81310 = LINE ( 'NONE', #71144, #37204 ) ;
#81311 = DIRECTION ( 'NONE',  ( 0.000000000000000000, -1.000000000000000000, 0.000000000000000000 ) ) ;
#81312 = ORIENTED_EDGE ( 'NONE', *, *, #84272, .T. ) ;
#81313 = DIRECTION ( 'NONE',  ( 1.000000000000000000, 0.000000000000000000, 0.000000000000000000 ) ) ;
#81314 = AXIS2_PLACEMENT_3D ( 'NONE', #18870, #52905, #63134 ) ;
#81315 = VECTOR ( 'NONE', #78650, 1000.000000000000000 ) ;
#81316 = VECTOR ( 'NONE', #7995, 999.9999999999998863 ) ;
#81317 = VECTOR ( 'NONE', #5730, 999.9999999999998863 ) ;
#81318 = LINE ( 'NONE', #115295, #63207 ) ;
#81320 = ORIENTED_EDGE ( 'NONE', *, *, #83233, .F. ) ;
#81319 = VECTOR ( 'NONE', #78425, 1000.000000000000000 ) ;
#81322 = ORIENTED_EDGE ( 'NONE', *, *, #43583, .F. ) ;
#81321 = LINE ( 'NONE', #35694, #62576 ) ;
#81323 = ORIENTED_EDGE ( 'NONE', *, *, #6430, .F. ) ;
#81324 = DIRECTION ( 'NONE',  ( -1.000000000000000000, -1.224606353822377258E-16, -0.000000000000000000 ) ) ;
#81325 = VECTOR ( 'NONE', #75995, 999.9999999999998863 ) ;
#81326 = ORIENTED_EDGE ( 'NONE', *, *, #116340, .T. ) ;
#81327 = DIRECTION ( 'NONE',  ( 0.7071067811865486830, -0.7071067811865464625, -0.000000000000000000 ) ) ;
#81328 = DIRECTION ( 'NONE',  ( -1.000000000000000000, -0.000000000000000000, -0.000000000000000000 ) ) ;
#81329 = EDGE_CURVE ( 'NONE', #36068, #60957, #127088, .T. ) ;
#81330 = PLANE ( 'NONE',  #11310 ) ;
#81331 = ORIENTED_EDGE ( 'NONE', *, *, #65099, .T. ) ;
#81332 = VECTOR ( 'NONE', #106149, 1000.000000000000000 ) ;
#81333 = CARTESIAN_POINT ( 'NONE',  ( 45.18398860626900415, 28.73617430169818832, 5.000000000000000000 ) ) ;
#81334 = EDGE_CURVE ( 'NONE', #130580, #22223, #16916, .T. ) ;
#81335 = CARTESIAN_POINT ( 'NONE',  ( -17.99451991528748351, 28.92564299267950645, 4.000000000000000000 ) ) ;
#81336 = DIRECTION ( 'NONE',  ( -0.7071067811865486830, -0.7071067811865464625, 0.000000000000000000 ) ) ;
#81337 = CARTESIAN_POINT ( 'NONE',  ( 12.18398860626900060, 28.73617430169795739, 5.000000000000000000 ) ) ;
#81338 = CARTESIAN_POINT ( 'NONE',  ( 15.32816939922340005, -21.74070752338407786, 4.000000000000000000 ) ) ;
#81339 = CARTESIAN_POINT ( 'NONE',  ( 125.9649422558287171, -6.613910356672960233, 3.556986441759899975 ) ) ;
#81340 = PLANE ( 'NONE',  #44193 ) ;
#81342 = EDGE_CURVE ( 'NONE', #120324, #3555, #138711, .T. ) ;
#81341 = CARTESIAN_POINT ( 'NONE',  ( 2.999999999999983569, 1.931123077392163712, 4.000000000000000000 ) ) ;
#81344 = ADVANCED_FACE ( 'NONE', ( #15440 ), #127838, .F. ) ;
#81343 = ORIENTED_EDGE ( 'NONE', *, *, #90288, .T. ) ;
#81345 = VERTEX_POINT ( 'NONE', #72779 ) ;
#81346 = VERTEX_POINT ( 'NONE', #61870 ) ;
#81347 = CARTESIAN_POINT ( 'NONE',  ( 121.3124999999999858, 5.819803920172571310, 5.819803920172575751 ) ) ;
#81348 = VECTOR ( 'NONE', #72500, 1000.000000000000000 ) ;
#81349 = ORIENTED_EDGE ( 'NONE', *, *, #141591, .T. ) ;
#81350 = VERTEX_POINT ( 'NONE', #139446 ) ;
#81351 = VECTOR ( 'NONE', #7020, 999.9999999999998863 ) ;
#81352 = ORIENTED_EDGE ( 'NONE', *, *, #81411, .T. ) ;
#81353 = DIRECTION ( 'NONE',  ( 0.7071067811865487940, -0.7071067811865463515, 0.000000000000000000 ) ) ;
#81354 = LINE ( 'NONE', #71908, #18459 ) ;
#81355 = AXIS2_PLACEMENT_3D ( 'NONE', #8525, #107163, #85401 ) ;
#81356 = ORIENTED_EDGE ( 'NONE', *, *, #78589, .F. ) ;
#81357 = DIRECTION ( 'NONE',  ( -0.7071067811865487940, 0.7071067811865463515, -0.000000000000000000 ) ) ;
#81358 = CARTESIAN_POINT ( 'NONE',  ( -30.79289321881324071, 0.7592924766157069794, 5.000000000000000000 ) ) ;
#81359 = ADVANCED_FACE ( 'NONE', ( #40131 ), #117613, .F. ) ;
#81360 = LINE ( 'NONE', #125566, #32645 ) ;
#81361 = CARTESIAN_POINT ( 'NONE',  ( 113.6045968585647614, 1.637169565754164946, -6.109999999999999432 ) ) ;
#81362 = CIRCLE ( 'NONE', #9587, 2.500000000000000888 ) ;
#81363 = ORIENTED_EDGE ( 'NONE', *, *, #44045, .F. ) ;
#81364 = EDGE_CURVE ( 'NONE', #80915, #12285, #68143, .T. ) ;
#81365 = FACE_OUTER_BOUND ( 'NONE', #28452, .T. ) ;
#81366 = DIRECTION ( 'NONE',  ( -0.7071067811865486830, -0.7071067811865464625, 0.000000000000000000 ) ) ;
#81367 = DIRECTION ( 'NONE',  ( 0.7071067811865486830, -0.7071067811865464625, -0.000000000000000000 ) ) ;
#81368 = CARTESIAN_POINT ( 'NONE',  ( 10.37159235450332062, 9.902892378096218942E-16, 0.000000000000000000 ) ) ;
#81369 = DIRECTION ( 'NONE',  ( -0.6830127018922180770, -0.6830127018922204085, -0.2588190451025213501 ) ) ;
#81370 = CARTESIAN_POINT ( 'NONE',  ( -45.48921356237309510, -27.52281430457087197, 5.000000000000000000 ) ) ;
#81371 = PLANE ( 'NONE',  #124547 ) ;
#81372 = CARTESIAN_POINT ( 'NONE',  ( 35.37086038379622011, 6.884901960086289741, -3.974999999999993427 ) ) ;
#81373 = CARTESIAN_POINT ( 'NONE',  ( -24.18398860626899705, 28.73617430169804265, 5.000000000000000000 ) ) ;
#81374 =( NAMED_UNIT ( * ) SI_UNIT ( $, .STERADIAN. ) SOLID_ANGLE_UNIT ( ) );
#81375 = VECTOR ( 'NONE', #40164, 1000.000000000000000 ) ;
#81376 = VERTEX_POINT ( 'NONE', #44965 ) ;
#81377 = ORIENTED_EDGE ( 'NONE', *, *, #133673, .F. ) ;
#81378 = CARTESIAN_POINT ( 'NONE',  ( 39.93750000000000711, 5.819803920172573974, -5.819803920172572198 ) ) ;
#81379 = EDGE_CURVE ( 'NONE', #42327, #13174, #134071, .T. ) ;
#81380 = VERTEX_POINT ( 'NONE', #89142 ) ;
#81381 = ORIENTED_EDGE ( 'NONE', *, *, #87283, .T. ) ;
#81382 = DIRECTION ( 'NONE',  ( -0.7071067811865487940, 0.7071067811865463515, -0.000000000000000000 ) ) ;
#81383 = AXIS2_PLACEMENT_3D ( 'NONE', #30557, #140717, #140040 ) ;
#81384 = LINE ( 'NONE', #33769, #135700 ) ;
#81385 = DIRECTION ( 'NONE',  ( -0.7071067811865487940, 0.7071067811865463515, -0.000000000000000000 ) ) ;
#81386 = ORIENTED_EDGE ( 'NONE', *, *, #52322, .F. ) ;
#81387 = EDGE_CURVE ( 'NONE', #19726, #16488, #1372, .T. ) ;
#81388 = VECTOR ( 'NONE', #95199, 999.9999999999998863 ) ;
#81389 = DIRECTION ( 'NONE',  ( -1.000000000000000000, -1.224606353822377258E-16, -0.000000000000000000 ) ) ;
#81390 = CARTESIAN_POINT ( 'NONE',  ( -20.67183060077632106, -21.74070752338406010, 4.000000000000000000 ) ) ;
#81391 = PLANE ( 'NONE',  #4817 ) ;
#81392 = CARTESIAN_POINT ( 'NONE',  ( 30.77126352523143638, 4.472830434245839371, 4.472830434245842035 ) ) ;
#81393 = VERTEX_POINT ( 'NONE', #99255 ) ;
#81394 = CARTESIAN_POINT ( 'NONE',  ( 13.49999999999990763, -17.56887692260763245, 4.000000000000000000 ) ) ;
#81395 = EDGE_LOOP ( 'NONE', ( #94910, #109518, #71565, #80073 ) ) ;
#81396 = EDGE_CURVE ( 'NONE', #139855, #31203, #122450, .T. ) ;
#81397 = VECTOR ( 'NONE', #141751, 1000.000000000000000 ) ;
#81398 = CARTESIAN_POINT ( 'NONE',  ( -32.99999999999976552, 20.96639925780205260, 5.000000000000000000 ) ) ;
#81399 = CARTESIAN_POINT ( 'NONE',  ( 21.29159235450332233, 2.500000000000001776, 0.000000000000000000 ) ) ;
#81401 =( BOUNDED_CURVE ( )  B_SPLINE_CURVE ( 3, ( #133786, #14124, #67106, #123649 ),
 .UNSPECIFIED., .F., .T. ) 
 B_SPLINE_CURVE_WITH_KNOTS ( ( 4, 4 ),
 ( 3.334020839929784152, 3.401188224464155141 ),
 .UNSPECIFIED. ) 
 CURVE ( )  GEOMETRIC_REPRESENTATION_ITEM ( )  RATIONAL_B_SPLINE_CURVE ( ( 1.000000000000000000, 0.9996240805387412998, 0.9996240805387412998, 1.000000000000000000 ) ) 
 REPRESENTATION_ITEM ( '' )  );
#81400 = FACE_OUTER_BOUND ( 'NONE', #132975, .T. ) ;
#81402 = CARTESIAN_POINT ( 'NONE',  ( -57.48921356237308800, -27.52281430457095368, 5.000000000000000000 ) ) ;
#81403 = ORIENTED_EDGE ( 'NONE', *, *, #118797, .T. ) ;
#81404 = ORIENTED_EDGE ( 'NONE', *, *, #91168, .T. ) ;
#81405 = LINE ( 'NONE', #70546, #42507 ) ;
#81406 = PLANE ( 'NONE',  #83305 ) ;
#81407 = CARTESIAN_POINT ( 'NONE',  ( 25.39999999999999858, 7.464222240803104598E-16, -6.094999999999989093 ) ) ;
#81408 = ADVANCED_FACE ( 'NONE', ( #674 ), #66674, .F. ) ;
#81409 = CARTESIAN_POINT ( 'NONE',  ( 183.3316408629058287, -52.14999999999999147, 41.64499999999997470 ) ) ;
#81410 = VECTOR ( 'NONE', #104696, 999.9999999999998863 ) ;
#81411 = EDGE_CURVE ( 'NONE', #72508, #135668, #17192, .T. ) ;
#81412 = CARTESIAN_POINT ( 'NONE',  ( 48.91209685856478018, 5.291415217122921177, -3.054999999999994831 ) ) ;
#81413 = LINE ( 'NONE', #69827, #92862 ) ;
#81414 = DIRECTION ( 'NONE',  ( -1.000000000000000000, -1.224606353822377258E-16, -0.000000000000000000 ) ) ;
#81415 = ORIENTED_EDGE ( 'NONE', *, *, #54641, .T. ) ;
#81416 = ORIENTED_EDGE ( 'NONE', *, *, #126909, .T. ) ;
#81417 = DIRECTION ( 'NONE',  ( -0.7071067811865486830, -0.7071067811865464625, 0.000000000000000000 ) ) ;
#81418 = VECTOR ( 'NONE', #123745, 1000.000000000000000 ) ;
#81419 = ORIENTED_EDGE ( 'NONE', *, *, #1089, .F. ) ;
#81420 = AXIS2_PLACEMENT_3D ( 'NONE', #29180, #50951, #116903 ) ;
#81421 = VECTOR ( 'NONE', #101168, 1000.000000000000000 ) ;
#81422 = DIRECTION ( 'NONE',  ( -1.000000000000000000, -0.000000000000000000, -0.000000000000000000 ) ) ;
#81423 = ORIENTED_EDGE ( 'NONE', *, *, #7319, .F. ) ;
#81424 = SURFACE_STYLE_FILL_AREA ( #3105 ) ;
#81425 = AXIS2_PLACEMENT_3D ( 'NONE', #79573, #123758, #51905 ) ;
#81427 = LINE ( 'NONE', #135098, #3816 ) ;
#81426 = AXIS2_PLACEMENT_3D ( 'NONE', #135716, #33572, #124118 ) ;
#81428 = VECTOR ( 'NONE', #112178, 1000.000000000000000 ) ;
#81429 = VECTOR ( 'NONE', #27325, 1000.000000000000114 ) ;
#81430 =( GEOMETRIC_REPRESENTATION_CONTEXT ( 3 ) GLOBAL_UNCERTAINTY_ASSIGNED_CONTEXT ( ( #131758 ) ) GLOBAL_UNIT_ASSIGNED_CONTEXT ( ( #50087, #126208, #5095 ) ) REPRESENTATION_CONTEXT ( 'NONE', 'WORKASPACE' ) );
#81431 = CARTESIAN_POINT ( 'NONE',  ( 18.48921356237309510, -27.52281430457068367, 5.000000000000000000 ) ) ;
#81432 = FACE_BOUND ( 'NONE', #35343, .T. ) ;
#81433 = LINE ( 'NONE', #59670, #52615 ) ;
#81434 = CARTESIAN_POINT ( 'NONE',  ( -11.20666063542143753, 21.75929247661549937, 4.998822639870708073 ) ) ;
#81435 = VECTOR ( 'NONE', #48923, 1000.000000000000000 ) ;
#81437 = VERTEX_POINT ( 'NONE', #33365 ) ;
#81436 = CARTESIAN_POINT ( 'NONE',  ( 3.758600742197928835, 21.72499999999999432, 5.000000000000000000 ) ) ;
#81438 = CARTESIAN_POINT ( 'NONE',  ( -26.99999999999981171, 7.588810512006185505, -3.013526669885166154 ) ) ;
#81439 = VERTEX_POINT ( 'NONE', #78268 ) ;
#81440 = ORIENTED_EDGE ( 'NONE', *, *, #79435, .F. ) ;
#81441 = CARTESIAN_POINT ( 'NONE',  ( 68.59959685856478018, -6.109999999999997655, -1.637169565754160283 ) ) ;
#81442 = VERTEX_POINT ( 'NONE', #118349 ) ;
#81443 = AXIS2_PLACEMENT_3D ( 'NONE', #55393, #141684, #42384 ) ;
#81444 = CARTESIAN_POINT ( 'NONE',  ( -31.25154412867556175, -11.24070752338416490, 10.39518518046016560 ) ) ;
#81445 = DIRECTION ( 'NONE',  ( 0.7071067811865486830, -0.7071067811865464625, -0.000000000000000000 ) ) ;
#81446 = VERTEX_POINT ( 'NONE', #40813 ) ;
#81447 = CARTESIAN_POINT ( 'NONE',  ( -6.707106781186501721, 5.259292476615663681, 5.000000000000000000 ) ) ;
#81448 = AXIS2_PLACEMENT_3D ( 'NONE', #62343, #127581, #60950 ) ;
#81449 = VECTOR ( 'NONE', #5398, 1000.000000000000000 ) ;
#81450 = CARTESIAN_POINT ( 'NONE',  ( 35.70833333333332860, -3.974999999999999201, -6.884901960086287964 ) ) ;
#81451 = LINE ( 'NONE', #82864, #124636 ) ;
#81452 = PLANE ( 'NONE',  #31954 ) ;
#81453 = VECTOR ( 'NONE', #109598, 1000.000000000000000 ) ;
#81454 = PLANE ( 'NONE',  #30795 ) ;
#81455 = CARTESIAN_POINT ( 'NONE',  ( 3.183988606268992161, 28.73617430169789699, 5.000000000000000000 ) ) ;
#81456 = ORIENTED_EDGE ( 'NONE', *, *, #34489, .F. ) ;
#81457 = EDGE_LOOP ( 'NONE', ( #136206, #69364, #62523, #35691 ) ) ;
#81458 = VECTOR ( 'NONE', #3736, 999.9999999999998863 ) ;
#81459 = LINE ( 'NONE', #114741, #3335 ) ;
#81460 = LINE ( 'NONE', #39370, #95240 ) ;
#81461 = ORIENTED_EDGE ( 'NONE', *, *, #118073, .F. ) ;
#81462 = VERTEX_POINT ( 'NONE', #51700 ) ;
#81463 = ORIENTED_EDGE ( 'NONE', *, *, #71392, .F. ) ;
#81464 = ADVANCED_FACE ( 'NONE', ( #43486 ), #85016, .F. ) ;
#81465 = ADVANCED_FACE ( 'NONE', ( #56557 ), #131933, .F. ) ;
#81466 = CARTESIAN_POINT ( 'NONE',  ( 16.49999999999988987, -14.70932175296475819, -11.46312253303840833 ) ) ;
#81467 = VERTEX_POINT ( 'NONE', #45657 ) ;
#81468 = CARTESIAN_POINT ( 'NONE',  ( -9.183988606268997046, 28.73617430169793607, 5.000000000000000000 ) ) ;
#81469 = VECTOR ( 'NONE', #105451, 999.9999999999998863 ) ;
#81470 = CARTESIAN_POINT ( 'NONE',  ( 21.18398860626899349, 28.73617430169802134, 5.000000000000000000 ) ) ;
#81471 = CARTESIAN_POINT ( 'NONE',  ( 5.317069808101885897, -2.126176841940956130, 7.934999999999991616 ) ) ;
#81472 = LINE ( 'NONE', #5276, #77366 ) ;
#81473 = VERTEX_POINT ( 'NONE', #107483 ) ;
#81474 = EDGE_CURVE ( 'NONE', #14862, #43234, #132675, .T. ) ;
#81475 = CARTESIAN_POINT ( 'NONE',  ( -45.18398860626900415, 28.73617430169818832, 5.000000000000000000 ) ) ;
#81476 = CARTESIAN_POINT ( 'NONE',  ( 118.9333603837970088, 2.130196079837088252, -7.949999999994423305 ) ) ;
#81477 = CARTESIAN_POINT ( 'NONE',  ( 18.29974487139159223, -27.71228299555219010, 4.000000000000000000 ) ) ;
#81479 = ORIENTED_EDGE ( 'NONE', *, *, #141537, .F. ) ;
#81478 = FACE_OUTER_BOUND ( 'NONE', #75866, .T. ) ;
#81481 = AXIS2_PLACEMENT_3D ( 'NONE', #56022, #100215, #45155 ) ;
#81480 = CARTESIAN_POINT ( 'NONE',  ( -9.005480084712511157, 28.92564299267931816, 4.000000000000000000 ) ) ;
#81482 = ORIENTED_EDGE ( 'NONE', *, *, #138401, .T. ) ;
#81483 = CARTESIAN_POINT ( 'NONE',  ( 34.92499999999998295, -21.72500000000000142, 5.000000000000000000 ) ) ;
#81484 = CARTESIAN_POINT ( 'NONE',  ( 2.602085213965210642E-15, -15.41253812416060143, 4.000000000000000000 ) ) ;
#81485 = CARTESIAN_POINT ( 'NONE',  ( 9.370933818357753964, -2.499999999999999112, 0.000000000000000000 ) ) ;
#81486 = EDGE_CURVE ( 'NONE', #90821, #51507, #56569, .T. ) ;
#81487 = ORIENTED_EDGE ( 'NONE', *, *, #67925, .T. ) ;
#81488 = CARTESIAN_POINT ( 'NONE',  ( 34.92499999999998295, -12.03857301832750970, 17.98374865626353625 ) ) ;
#81489 = DIRECTION ( 'NONE',  ( 0.000000000000000000, -1.000000000000000000, 0.000000000000000000 ) ) ;
#81490 = DIRECTION ( 'NONE',  ( 0.6830127018922181881, 0.6830127018922202975, -0.2588190451025214056 ) ) ;
#81491 = DIRECTION ( 'NONE',  ( 0.7071067811865486830, -0.7071067811865464625, -0.000000000000000000 ) ) ;
#81492 = VECTOR ( 'NONE', #106029, 1000.000000000000000 ) ;
#81493 = VERTEX_POINT ( 'NONE', #34759 ) ;
#81494 = EDGE_CURVE ( 'NONE', #6816, #107486, #140809, .T. ) ;
#81495 = DIRECTION ( 'NONE',  ( -0.7071067811865486830, -0.7071067811865464625, 0.000000000000000000 ) ) ;
#81496 = LINE ( 'NONE', #79374, #93319 ) ;
#81497 = CARTESIAN_POINT ( 'NONE',  ( 0.2100385686636480065, -0.3999999999999998002, -2.083955130345452211 ) ) ;
#81498 = CARTESIAN_POINT ( 'NONE',  ( 10.21321903303352840, 12.75929247661559351, 10.29404684609037623 ) ) ;
#81499 =( LENGTH_UNIT ( ) NAMED_UNIT ( * ) SI_UNIT ( .MILLI., .METRE. ) );
#81500 = ORIENTED_EDGE ( 'NONE', *, *, #110741, .T. ) ;
#81501 = ORIENTED_EDGE ( 'NONE', *, *, #95227, .T. ) ;
#81502 = ADVANCED_FACE ( 'NONE', ( #121733 ), #52385, .F. ) ;
#81503 = VECTOR ( 'NONE', #79770, 1000.000000000000000 ) ;
#81504 = FACE_OUTER_BOUND ( 'NONE', #38621, .T. ) ;
#81505 = CARTESIAN_POINT ( 'NONE',  ( 1.728736474768552522, 5.808823158059031044, -5.808823158059038150 ) ) ;
#81506 = DIRECTION ( 'NONE',  ( -0.3543493200069162685, -0.000000000000000000, -0.9351131265310288487 ) ) ;
#81507 = CARTESIAN_POINT ( 'NONE',  ( 14.16170612452611444, -6.740707523384212863, 16.75550250614870862 ) ) ;
#81508 = CARTESIAN_POINT ( 'NONE',  ( -34.92500000000001137, 21.72500000000000142, 5.000000000000000000 ) ) ;
#81509 = LINE ( 'NONE', #14790, #97722 ) ;
#81510 = ORIENTED_EDGE ( 'NONE', *, *, #137954, .F. ) ;
#81511 = ADVANCED_FACE ( 'NONE', ( #110144 ), #100505, .T. ) ;
#81512 = DIRECTION ( 'NONE',  ( 0.000000000000000000, 0.000000000000000000, 1.000000000000000000 ) ) ;
#81513 = DIRECTION ( 'NONE',  ( 0.7071067811865487940, 0.7071067811865463515, -0.000000000000000000 ) ) ;
#81514 = VECTOR ( 'NONE', #19737, 1000.000000000000227 ) ;
#81515 = PLANE ( 'NONE',  #1825 ) ;
#81516 = CARTESIAN_POINT ( 'NONE',  ( 49.05793019189810877, 6.110000000000001208, -1.637169565754156286 ) ) ;
#81517 = CARTESIAN_POINT ( 'NONE',  ( 184.0335292699550678, -51.38852430739337507, -37.54101415799217278 ) ) ;
#81518 = ADVANCED_FACE ( 'NONE', ( #121032 ), #55084, .T. ) ;
#81520 = EDGE_CURVE ( 'NONE', #47269, #90697, #80417, .T. ) ;
#81519 = AXIS2_PLACEMENT_3D ( 'NONE', #34191, #108853, #53818 ) ;
#81521 = AXIS2_PLACEMENT_3D ( 'NONE', #53789, #107425, #9509 ) ;
#81522 = VERTEX_POINT ( 'NONE', #59386 ) ;
#81523 = LINE ( 'NONE', #116259, #99750 ) ;
#81524 = VERTEX_POINT ( 'NONE', #103542 ) ;
#81525 = CARTESIAN_POINT ( 'NONE',  ( -63.48921356237309510, -27.52281430457099631, 5.000000000000000000 ) ) ;
#81526 = ORIENTED_EDGE ( 'NONE', *, *, #20737, .T. ) ;
#81527 = AXIS2_PLACEMENT_3D ( 'NONE', #13380, #113420, #35193 ) ;
#81528 = VECTOR ( 'NONE', #59941, 1000.000000000000000 ) ;
#81529 = CARTESIAN_POINT ( 'NONE',  ( -4.499999999999964473, -10.91253812416064761, 4.000000000000000000 ) ) ;
#81530 = EDGE_CURVE ( 'NONE', #103220, #131264, #115117, .T. ) ;
#81531 = CARTESIAN_POINT ( 'NONE',  ( -24.29974487139158867, -27.71228299555223273, 4.000000000000000000 ) ) ;
#81532 = DIRECTION ( 'NONE',  ( -0.7071067811865486830, -0.7071067811865464625, 0.000000000000000000 ) ) ;
#81533 = PLANE ( 'NONE',  #101939 ) ;
#81534 = EDGE_CURVE ( 'NONE', #140963, #139479, #113732, .T. ) ;
#81535 = FACE_OUTER_BOUND ( 'NONE', #142649, .T. ) ;
#81536 = CARTESIAN_POINT ( 'NONE',  ( 128.8216926156734132, -52.14999999996970814, 41.05175048930652082 ) ) ;
#81537 = VERTEX_POINT ( 'NONE', #114438 ) ;
#81538 = ADVANCED_FACE ( 'NONE', ( #126724 ), #124607, .F. ) ;
#81539 = PLANE ( 'NONE',  #120393 ) ;
#81540 = DIRECTION ( 'NONE',  ( -0.6830127018922181881, 0.6830127018922202975, -0.2588190451025214056 ) ) ;
#81541 = PLANE ( 'NONE',  #139995 ) ;
#81542 = CARTESIAN_POINT ( 'NONE',  ( 116.5000000000000000, 0.000000000000000000, -7.950000000000000178 ) ) ;
#81543 = CARTESIAN_POINT ( 'NONE',  ( 74.45419371712955581, 6.884901960086283523, 3.975000000000002753 ) ) ;
#81544 = CARTESIAN_POINT ( 'NONE',  ( 7.139999999999991687, -35.76999999999998892, -7.899272885403729738 ) ) ;
#81545 = EDGE_LOOP ( 'NONE', ( #32173, #99389, #12200, #98445 ) ) ;
#81546 = ORIENTED_EDGE ( 'NONE', *, *, #12582, .T. ) ;
#81547 = CARTESIAN_POINT ( 'NONE',  ( 65.60416666666665719, 2.130196079827422206, 7.950000000000001954 ) ) ;
#81548 = EDGE_CURVE ( 'NONE', #108392, #86264, #27412, .T. ) ;
#81549 = PLANE ( 'NONE',  #111774 ) ;
#81550 = DIRECTION ( 'NONE',  ( -0.6830127018922181881, 0.6830127018922202975, -0.2588190451025214056 ) ) ;
#81551 = CARTESIAN_POINT ( 'NONE',  ( 13.08316395874281568, 3.014287036135060660, 4.000000000000000000 ) ) ;
#81552 = ORIENTED_EDGE ( 'NONE', *, *, #72208, .F. ) ;
#81553 = EDGE_CURVE ( 'NONE', #112837, #61060, #58702, .T. ) ;
#81554 = VECTOR ( 'NONE', #47062, 1000.000000000000000 ) ;
#81555 = PLANE ( 'NONE',  #81527 ) ;
#81556 = CIRCLE ( 'NONE', #90528, 2.499999999999998668 ) ;
#81557 = DIRECTION ( 'NONE',  ( 0.7071067811865486830, -0.7071067811865464625, -0.000000000000000000 ) ) ;
#81558 = CARTESIAN_POINT ( 'NONE',  ( 59.93793019189809712, -6.110000000000001208, 1.637169565754158951 ) ) ;
#81559 = CARTESIAN_POINT ( 'NONE',  ( -24.48921356237309510, -27.52281430457072631, 5.000000000000000000 ) ) ;
#81560 = VERTEX_POINT ( 'NONE', #113004 ) ;
#81561 = VERTEX_POINT ( 'NONE', #4181 ) ;
#81562 = VECTOR ( 'NONE', #82415, 1000.000000000000000 ) ;
#81563 = DIRECTION ( 'NONE',  ( 0.7071067811865487940, 0.7071067811865463515, -0.000000000000000000 ) ) ;
#81564 = LINE ( 'NONE', #125768, #19742 ) ;
#81565 = CARTESIAN_POINT ( 'NONE',  ( -36.29974487139159578, -27.71228299555231445, 4.000000000000000000 ) ) ;
#81566 = CARTESIAN_POINT ( 'NONE',  ( 63.18398860626900415, 28.73617430169831621, 5.000000000000000000 ) ) ;
#81567 = DIRECTION ( 'NONE',  ( -0.7071067811865487940, 0.7071067811865463515, 0.000000000000000000 ) ) ;
#81569 = EDGE_LOOP ( 'NONE', ( #60042, #15842, #43617, #73949 ) ) ;
#81568 = CARTESIAN_POINT ( 'NONE',  ( 41.99451991528749062, 28.92564299267967343, 4.000000000000000000 ) ) ;
#81570 = LINE ( 'NONE', #60535, #11330 ) ;
#81571 = LINE ( 'NONE', #125775, #103332 ) ;
#81572 = DIRECTION ( 'NONE',  ( -1.000000000000000000, -0.000000000000000000, -0.000000000000000000 ) ) ;
#81573 = CARTESIAN_POINT ( 'NONE',  ( 7.139999999999993463, -34.64999999999999858, 17.49210858042622263 ) ) ;
#81574 = EDGE_CURVE ( 'NONE', #73921, #97839, #57247, .T. ) ;
#81575 = ORIENTED_EDGE ( 'NONE', *, *, #61691, .F. ) ;
#81576 = ADVANCED_FACE ( 'NONE', ( #101422 ), #112100, .T. ) ;
#81577 = ORIENTED_EDGE ( 'NONE', *, *, #25871, .F. ) ;
#81578 = CARTESIAN_POINT ( 'NONE',  ( 20.81601139373100295, 28.73617430169773002, 5.000000000000000000 ) ) ;
#81579 = DIRECTION ( 'NONE',  ( -0.3543493200069162685, -0.000000000000000000, -0.9351131265310288487 ) ) ;
#81580 = AXIS2_PLACEMENT_3D ( 'NONE', #88162, #22854, #108427 ) ;
#81581 = CARTESIAN_POINT ( 'NONE',  ( -18.18398860626898994, 28.73617430169800002, 5.000000000000000000 ) ) ;
#81582 = CARTESIAN_POINT ( 'NONE',  ( 15.32816939922342314, -12.74070752338415247, 4.000000000000000000 ) ) ;
#81583 = EDGE_LOOP ( 'NONE', ( #23311, #46287, #55636, #126854 ) ) ;
#81584 = ORIENTED_EDGE ( 'NONE', *, *, #167, .F. ) ;
#81585 = VECTOR ( 'NONE', #33395, 1000.000000000000000 ) ;
#81586 = FACE_OUTER_BOUND ( 'NONE', #15208, .T. ) ;
#81587 = CARTESIAN_POINT ( 'NONE',  ( 78.48921356237309510, -27.52281430457109934, 5.000000000000000000 ) ) ;
#81588 = ORIENTED_EDGE ( 'NONE', *, *, #104586, .F. ) ;
#81589 = VERTEX_POINT ( 'NONE', #2071 ) ;
#81590 = FACE_OUTER_BOUND ( 'NONE', #124480, .T. ) ;
#81591 = DIRECTION ( 'NONE',  ( -0.7071067811865487940, 0.7071067811865463515, -0.000000000000000000 ) ) ;
#81592 = VECTOR ( 'NONE', #15986, 1000.000000000000000 ) ;
#81593 = FACE_BOUND ( 'NONE', #108099, .T. ) ;
#81594 = DIRECTION ( 'NONE',  ( -0.7071067811865486830, -0.7071067811865464625, 0.000000000000000000 ) ) ;
#81595 = FACE_OUTER_BOUND ( 'NONE', #46681, .T. ) ;
#81596 = DIRECTION ( 'NONE',  ( -0.000000000000000000, 0.000000000000000000, 1.000000000000000000 ) ) ;
#81597 = VECTOR ( 'NONE', #11770, 1000.000000000000000 ) ;
#81598 = CARTESIAN_POINT ( 'NONE',  ( -23.20710678118638981, 15.75929247661555976, 5.000000000000000000 ) ) ;
#81599 = DIRECTION ( 'NONE',  ( -0.000000000000000000, 0.000000000000000000, 1.000000000000000000 ) ) ;
#81600 = APPLICATION_PROTOCOL_DEFINITION ( 'draft international standard', 'automotive_design', 1998, #45749 ) ;
#81601 = ORIENTED_EDGE ( 'NONE', *, *, #140222, .F. ) ;
#81602 = ORIENTED_EDGE ( 'NONE', *, *, #25966, .F. ) ;
#81603 = CARTESIAN_POINT ( 'NONE',  ( 97.47459685856478018, 1.637169565754164280, -6.109999999999996767 ) ) ;
#81604 = VERTEX_POINT ( 'NONE', #70283 ) ;
#81605 = CARTESIAN_POINT ( 'NONE',  ( -13.17183060077637613, -14.24070752338413648, 4.000000000000000000 ) ) ;
#81606 = EDGE_CURVE ( 'NONE', #1799, #72134, #10235, .T. ) ;
#81607 = CARTESIAN_POINT ( 'NONE',  ( 72.48921356237309510, -27.52281430457106026, 5.000000000000000000 ) ) ;
#81608 = VECTOR ( 'NONE', #52757, 1000.000000000000000 ) ;
#81609 = AXIS2_PLACEMENT_3D ( 'NONE', #73617, #19926, #81850 ) ;
#81610 = CIRCLE ( 'NONE', #56173, 3.999999999999996447 ) ;
#81611 = FACE_OUTER_BOUND ( 'NONE', #124766, .T. ) ;
#81612 = VECTOR ( 'NONE', #70622, 1000.000000000000227 ) ;
#81613 = MECHANICAL_DESIGN_GEOMETRIC_PRESENTATION_REPRESENTATION (  '', ( #137180 ), #12138 ) ;
#81614 = FACE_OUTER_BOUND ( 'NONE', #37096, .T. ) ;
#81615 = ORIENTED_EDGE ( 'NONE', *, *, #49271, .T. ) ;
#81616 = DIRECTION ( 'NONE',  ( -1.000000000000000000, -0.000000000000000000, -0.000000000000000000 ) ) ;
#81617 = CARTESIAN_POINT ( 'NONE',  ( 16.77149322861325231, 20.25929247661551713, 7.808871592221806601 ) ) ;
#81618 = CARTESIAN_POINT ( 'NONE',  ( 20.52487387214941350, 14.25929247661557042, 9.797011795316684868 ) ) ;
#81620 = LINE ( 'NONE', #48980, #93671 ) ;
#81619 = CARTESIAN_POINT ( 'NONE',  ( -15.67180000000000284, 3.174999999999997158, 1.444000000000000394 ) ) ;
#81621 = DIRECTION ( 'NONE',  ( 1.321231229586337907E-16, -0.9647414015272155474, 0.2631995976047525887 ) ) ;
#81622 = VECTOR ( 'NONE', #141622, 1000.000000000000000 ) ;
#81623 = AXIS2_PLACEMENT_3D ( 'NONE', #139495, #84388, #86517 ) ;
#81624 =( GEOMETRIC_REPRESENTATION_CONTEXT ( 3 ) GLOBAL_UNCERTAINTY_ASSIGNED_CONTEXT ( ( #75090 ) ) GLOBAL_UNIT_ASSIGNED_CONTEXT ( ( #64441, #108624, #130433 ) ) REPRESENTATION_CONTEXT ( 'NONE', 'WORKASPACE' ) );
#81625 = DIRECTION ( 'NONE',  ( 0.6830127018922181881, 0.6830127018922202975, -0.2588190451025214056 ) ) ;
#81626 = ORIENTED_EDGE ( 'NONE', *, *, #125066, .T. ) ;
#81627 = DIRECTION ( 'NONE',  ( 0.7071067811865487940, -0.7071067811865463515, 0.000000000000000000 ) ) ;
#81628 = CARTESIAN_POINT ( 'NONE',  ( 17.99451991528748351, 28.92564299267950645, 4.000000000000000000 ) ) ;
#81629 = EDGE_CURVE ( 'NONE', #142812, #25609, #13673, .T. ) ;
#81630 = ORIENTED_EDGE ( 'NONE', *, *, #117441, .F. ) ;
#81631 = ORIENTED_EDGE ( 'NONE', *, *, #115661, .T. ) ;
#81632 = ADVANCED_FACE ( 'NONE', ( #104252 ), #92671, .F. ) ;
#81633 = EDGE_CURVE ( 'NONE', #68934, #58171, #134804, .T. ) ;
#81634 = ORIENTED_EDGE ( 'NONE', *, *, #136201, .F. ) ;
#81635 = CARTESIAN_POINT ( 'NONE',  ( 44.91709685856476142, 3.054999999999998828, 5.291415217122922066 ) ) ;
#81636 = ORIENTED_EDGE ( 'NONE', *, *, #96015, .F. ) ;
#81637 = EDGE_CURVE ( 'NONE', #100092, #75407, #136192, .T. ) ;
#81638 = EDGE_CURVE ( 'NONE', #42005, #42538, #91973, .T. ) ;
#81639 = CARTESIAN_POINT ( 'NONE',  ( 11.56663961620376924, 1.633150327867695095, 6.094999999999988205 ) ) ;
#81640 = CARTESIAN_POINT ( 'NONE',  ( -14.47644487788491396, 4.930979942669944549, -31.94426976426194287 ) ) ;
#81641 = ORIENTED_EDGE ( 'NONE', *, *, #135880, .T. ) ;
#81642 = EDGE_CURVE ( 'NONE', #77572, #68590, #129604, .T. ) ;
#81643 = DIRECTION ( 'NONE',  ( 0.6830127018922180770, -0.6830127018922204085, -0.2588190451025213501 ) ) ;
#81644 = ORIENTED_EDGE ( 'NONE', *, *, #97203, .T. ) ;
#81645 = CARTESIAN_POINT ( 'NONE',  ( 34.42499999999998295, 22.22500000000000142, 4.165035510187007795 ) ) ;
#81646 = DIRECTION ( 'NONE',  ( -0.7071067811865486830, 0.7071067811865464625, 0.000000000000000000 ) ) ;
#81648 = ORIENTED_EDGE ( 'NONE', *, *, #142856, .T. ) ;
#81647 = LINE ( 'NONE', #13467, #26269 ) ;
#81649 = ORIENTED_EDGE ( 'NONE', *, *, #68274, .F. ) ;
#81650 = FACE_OUTER_BOUND ( 'NONE', #71717, .T. ) ;
#81651 = VECTOR ( 'NONE', #115597, 1000.000000000000000 ) ;
#81652 = DIRECTION ( 'NONE',  ( -0.7071067811865486830, -0.7071067811865464625, 0.000000000000000000 ) ) ;
#81653 = EDGE_CURVE ( 'NONE', #13056, #140226, #86648, .T. ) ;
#81654 = EDGE_LOOP ( 'NONE', ( #47969, #117152 ) ) ;
#81655 = FACE_OUTER_BOUND ( 'NONE', #53197, .T. ) ;
#81656 = ORIENTED_EDGE ( 'NONE', *, *, #66006, .F. ) ;
#81657 = EDGE_LOOP ( 'NONE', ( #45632, #110859, #138944, #42842 ) ) ;
#81658 = AXIS2_PLACEMENT_3D ( 'NONE', #88961, #109967, #133179 ) ;
#81659 = ORIENTED_EDGE ( 'NONE', *, *, #137980, .T. ) ;
#81660 = ORIENTED_EDGE ( 'NONE', *, *, #143335, .F. ) ;
#81661 = DIRECTION ( 'NONE',  ( 0.6830127018922181881, 0.6830127018922202975, -0.2588190451025214056 ) ) ;
#81662 = VECTOR ( 'NONE', #37321, 1000.000000000000000 ) ;
#81663 = VECTOR ( 'NONE', #52275, 1000.000000000000000 ) ;
#81664 = EDGE_CURVE ( 'NONE', #87975, #31572, #24130, .T. ) ;
#81665 = CARTESIAN_POINT ( 'NONE',  ( 24.48921356237309510, -27.52281430457072631, 5.000000000000000000 ) ) ;
#81666 = FACE_OUTER_BOUND ( 'NONE', #9495, .T. ) ;
#81667 = DIRECTION ( 'NONE',  ( -0.000000000000000000, -0.3543493200069152693, 0.9351131265310292928 ) ) ;
#81668 = CARTESIAN_POINT ( 'NONE',  ( 0.000000000000000000, 0.000000000000000000, 5.000000000000000000 ) ) ;
#81669 = ORIENTED_EDGE ( 'NONE', *, *, #96381, .T. ) ;
#81670 = EDGE_CURVE ( 'NONE', #117172, #42180, #128195, .T. ) ;
#81671 = DIRECTION ( 'NONE',  ( 0.7071067811865486830, -0.7071067811865464625, -0.000000000000000000 ) ) ;
#81672 = CARTESIAN_POINT ( 'NONE',  ( 24.04123647476855652, 0.000000000000000000, 7.934999999999990727 ) ) ;
#81673 = DIRECTION ( 'NONE',  ( -0.5735764363510499342, -0.8191520442889891340, 0.000000000000000000 ) ) ;
#81674 = LINE ( 'NONE', #6890, #80797 ) ;
#81675 = CARTESIAN_POINT ( 'NONE',  ( -18.18398860626898994, 28.73617430169800002, 5.000000000000000000 ) ) ;
#81676 = ORIENTED_EDGE ( 'NONE', *, *, #66782, .T. ) ;
#81677 = VERTEX_POINT ( 'NONE', #106378 ) ;
#81678 = AXIS2_PLACEMENT_3D ( 'NONE', #33626, #47387, #56824 ) ;
#81680 = ORIENTED_EDGE ( 'NONE', *, *, #98511, .F. ) ;
#81679 = ADVANCED_FACE ( 'NONE', ( #41891 ), #96227, .F. ) ;
#81681 = PLANE ( 'NONE',  #34888 ) ;
#81682 = DIRECTION ( 'NONE',  ( -0.7071067811865486830, -0.7071067811865464625, -0.000000000000000000 ) ) ;
#81683 = LINE ( 'NONE', #114274, #103211 ) ;
#81684 = AXIS2_PLACEMENT_3D ( 'NONE', #142511, #65698, #22810 ) ;
#81685 = CARTESIAN_POINT ( 'NONE',  ( -32.20710678118632586, 6.759292476615653023, 5.000000000000000000 ) ) ;
#81686 = FACE_OUTER_BOUND ( 'NONE', #112442, .T. ) ;
#81687 = CARTESIAN_POINT ( 'NONE',  ( 78.37043019189812298, -3.055000000000001936, 5.291415217122918513 ) ) ;
#81688 = CARTESIAN_POINT ( 'NONE',  ( 79.89583333333331439, -2.130196079827351596, 7.950000000000043698 ) ) ;
#81689 = EDGE_CURVE ( 'NONE', #119254, #23935, #138344, .T. ) ;
#81690 = DIRECTION ( 'NONE',  ( 0.000000000000000000, 0.000000000000000000, 1.000000000000000000 ) ) ;
#81691 = DIRECTION ( 'NONE',  ( -0.7071067811865487940, 0.7071067811865463515, 0.000000000000000000 ) ) ;
#81692 = DIRECTION ( 'NONE',  ( 0.7071067811865487940, 0.7071067811865463515, 0.000000000000000000 ) ) ;
#81693 = EDGE_CURVE ( 'NONE', #47322, #85488, #104986, .T. ) ;
#81694 = DIRECTION ( 'NONE',  ( 0.7071067811865486830, -0.7071067811865464625, -0.000000000000000000 ) ) ;
#81695 = ORIENTED_EDGE ( 'NONE', *, *, #9444, .F. ) ;
#81696 = VECTOR ( 'NONE', #38944, 999.9999999999998863 ) ;
#81697 = CARTESIAN_POINT ( 'NONE',  ( 17.01299345042646749, -0.9444868035190607802, -36.39086428169088094 ) ) ;
#81698 = ORIENTED_EDGE ( 'NONE', *, *, #129720, .T. ) ;
#81699 = EDGE_CURVE ( 'NONE', #70901, #41454, #61532, .T. ) ;
#81700 = CARTESIAN_POINT ( 'NONE',  ( -8.700255128608413102, -27.71228299555199825, 4.000000000000000000 ) ) ;
#81702 = VERTEX_POINT ( 'NONE', #40479 ) ;
#81701 = CARTESIAN_POINT ( 'NONE',  ( -14.59243874171183641, 22.22500000000000142, 12.70476753181831775 ) ) ;
#81703 = DIRECTION ( 'NONE',  ( -0.000000000000000000, 0.3543493200069153248, 0.9351131265310292928 ) ) ;
#81704 = DIRECTION ( 'NONE',  ( 0.5735764363510453823, -0.8191520442889923537, 1.003171929053525486E-16 ) ) ;
#81705 = VERTEX_POINT ( 'NONE', #49924 ) ;
#81706 = CARTESIAN_POINT ( 'NONE',  ( -33.79289321881321939, -17.24070752338409918, 5.000000000000000000 ) ) ;
#81708 = ORIENTED_EDGE ( 'NONE', *, *, #38996, .F. ) ;
#81707 = MECHANICAL_DESIGN_GEOMETRIC_PRESENTATION_REPRESENTATION (  '', ( #100206 ), #109511 ) ;
#81709 = CARTESIAN_POINT ( 'NONE',  ( 121.9958603837962272, -3.974999999999998312, -6.884901960086286188 ) ) ;
#81710 = ORIENTED_EDGE ( 'NONE', *, *, #92274, .T. ) ;
#81711 = DIRECTION ( 'NONE',  ( -1.000000000000000000, -1.224606353822377258E-16, -0.000000000000000000 ) ) ;
#81712 = CARTESIAN_POINT ( 'NONE',  ( 103.3291937171295700, -3.975000000000001865, 6.884901960086284411 ) ) ;
#81713 = PLANE ( 'NONE',  #69531 ) ;
#81714 = DIRECTION ( 'NONE',  ( -0.5735764363510507113, 0.8191520442889885789, 1.003171929053520926E-16 ) ) ;
#81715 = ORIENTED_EDGE ( 'NONE', *, *, #65780, .T. ) ;
#81716 = EDGE_CURVE ( 'NONE', #27773, #21069, #73109, .T. ) ;
#81717 = DIRECTION ( 'NONE',  ( 0.6830127018922181881, 0.6830127018922202975, -0.2588190451025214056 ) ) ;
#81718 = DIRECTION ( 'NONE',  ( 0.6830127018922181881, 0.6830127018922202975, -0.2588190451025214056 ) ) ;
#81719 = CARTESIAN_POINT ( 'NONE',  ( 15.05159235450332034, -2.500000000000000444, 3.061616997868384620E-16 ) ) ;
#81720 = CARTESIAN_POINT ( 'NONE',  ( 23.91666666666666785, 5.278424836066147208, 3.047499999999990550 ) ) ;
#81721 = PRESENTATION_STYLE_ASSIGNMENT (( #74943 ) ) ;
#81722 = VECTOR ( 'NONE', #111028, 1000.000000000000000 ) ;
#81723 = DIRECTION ( 'NONE',  ( 0.7071067811865486830, -0.7071067811865464625, -0.000000000000000000 ) ) ;
#81724 = ORIENTED_EDGE ( 'NONE', *, *, #119414, .F. ) ;
#81725 = EDGE_CURVE ( 'NONE', #68485, #29586, #18671, .T. ) ;
#81726 = VECTOR ( 'NONE', #57411, 999.9999999999998863 ) ;
#81727 = AXIS2_PLACEMENT_3D ( 'NONE', #62006, #129363, #93181 ) ;
#81728 = CARTESIAN_POINT ( 'NONE',  ( -0.4892135623730947680, -27.52281430457055578, 5.000000000000000000 ) ) ;
#81729 = VERTEX_POINT ( 'NONE', #83249 ) ;
#81730 = EDGE_CURVE ( 'NONE', #60519, #79079, #130334, .T. ) ;
#81731 = CARTESIAN_POINT ( 'NONE',  ( 86.18793019189811844, 6.110000000000002984, -1.637169565754156730 ) ) ;
#81732 = DIRECTION ( 'NONE',  ( -0.7071067811865486830, -0.7071067811865464625, 0.000000000000000000 ) ) ;
#81733 = VECTOR ( 'NONE', #104980, 999.9999999999998863 ) ;
#81735 = MECHANICAL_DESIGN_GEOMETRIC_PRESENTATION_REPRESENTATION (  '', ( #21481 ), #16821 ) ;
#81734 = CARTESIAN_POINT ( 'NONE',  ( -6.707106781186484845, -18.74070752338408852, 5.000000000000000000 ) ) ;
#81736 = AXIS2_PLACEMENT_3D ( 'NONE', #67138, #1815, #112075 ) ;
#81737 = FACE_OUTER_BOUND ( 'NONE', #2886, .T. ) ;
#81738 = ORIENTED_EDGE ( 'NONE', *, *, #91595, .F. ) ;
#81739 = CARTESIAN_POINT ( 'NONE',  ( 23.51078643762690490, -27.52281430457038880, 5.000000000000000000 ) ) ;
#81740 = DIRECTION ( 'NONE',  ( -0.7071067811865487940, -0.7071067811865463515, -0.000000000000000000 ) ) ;
#81741 = ORIENTED_EDGE ( 'NONE', *, *, #34820, .F. ) ;
#81742 = CARTESIAN_POINT ( 'NONE',  ( 0.000000000000000000, 0.000000000000000000, 5.000000000000000000 ) ) ;
#81743 = DIRECTION ( 'NONE',  ( 0.7071067811865487940, -0.7071067811865463515, 0.000000000000000000 ) ) ;
#81745 = VERTEX_POINT ( 'NONE', #7062 ) ;
#81744 = CARTESIAN_POINT ( 'NONE',  ( -34.49999999999976552, -1.535744391599501490, 4.994342998332164996 ) ) ;
#81746 = CARTESIAN_POINT ( 'NONE',  ( -6.183988606268994381, 28.73617430169791476, 5.000000000000000000 ) ) ;
#81747 = DIRECTION ( 'NONE',  ( -1.000000000000000000, -1.224606353822377258E-16, -0.000000000000000000 ) ) ;
#81748 = CARTESIAN_POINT ( 'NONE',  ( 1.889689338576429289, -5.719221863398560757, 2.436636208257458858 ) ) ;
#81749 = DIRECTION ( 'NONE',  ( -1.000000000000000000, -0.000000000000000000, -0.000000000000000000 ) ) ;
#81750 = EDGE_LOOP ( 'NONE', ( #122394, #43522, #117580, #123585 ) ) ;
#81751 = EDGE_CURVE ( 'NONE', #125982, #33206, #28156, .T. ) ;
#81752 = VERTEX_POINT ( 'NONE', #95532 ) ;
#81753 = ORIENTED_EDGE ( 'NONE', *, *, #137694, .T. ) ;
#81754 = CARTESIAN_POINT ( 'NONE',  ( 81.08376352523144703, -6.110000000000001208, -3.741295971395164515E-16 ) ) ;
#81755 = AXIS2_PLACEMENT_3D ( 'NONE', #85929, #42464, #117809 ) ;
#81756 = ORIENTED_EDGE ( 'NONE', *, *, #6442, .T. ) ;
#81757 = EDGE_CURVE ( 'NONE', #129447, #28284, #72415, .T. ) ;
#81758 = CARTESIAN_POINT ( 'NONE',  ( 33.18398860626899705, 28.73617430169810305, 5.000000000000000000 ) ) ;
#81759 = CARTESIAN_POINT ( 'NONE',  ( 6.299744871391586898, -27.71228299555210484, 4.000000000000000000 ) ) ;
#81760 = CARTESIAN_POINT ( 'NONE',  ( -24.34427593291135139, 5.931737808750704666, 4.000000000000000000 ) ) ;
#81761 = FACE_OUTER_BOUND ( 'NONE', #45557, .T. ) ;
#81762 = ORIENTED_EDGE ( 'NONE', *, *, #51388, .F. ) ;
#81763 = CARTESIAN_POINT ( 'NONE',  ( 15.72281430457048934, -21.72500000000000497, 5.000000000000000000 ) ) ;
#81764 = DIRECTION ( 'NONE',  ( -0.000000000000000000, 0.3543493200069153248, 0.9351131265310292928 ) ) ;
#81765 = VECTOR ( 'NONE', #5623, 1000.000000000000000 ) ;
#81766 = CARTESIAN_POINT ( 'NONE',  ( 72.82876352523145158, 0.000000000000000000, -6.109999999999998543 ) ) ;
#81767 = EDGE_CURVE ( 'NONE', #11132, #24858, #113498, .T. ) ;
#81768 = VERTEX_POINT ( 'NONE', #118714 ) ;
#81769 = VECTOR ( 'NONE', #61354, 1000.000000000000000 ) ;
#81770 = CARTESIAN_POINT ( 'NONE',  ( 15.79076468313838433, 8.175634574663693144, 5.000000000000000000 ) ) ;
#81771 = CARTESIAN_POINT ( 'NONE',  ( 54.29974487139159578, -27.71228299555243879, 4.000000000000000000 ) ) ;
#81772 = CARTESIAN_POINT ( 'NONE',  ( -3.330102185472624932, 17.25929247661554555, 19.83885114516072079 ) ) ;
#81773 = ORIENTED_EDGE ( 'NONE', *, *, #39223, .T. ) ;
#81774 = EDGE_LOOP ( 'NONE', ( #141954, #87747, #110336, #101008 ) ) ;
#81775 = LINE ( 'NONE', #91891, #28410 ) ;
#81776 = EDGE_CURVE ( 'NONE', #139533, #30840, #107823, .T. ) ;
#81777 = CYLINDRICAL_SURFACE ( 'NONE', #133458, 9.119999999999999218 ) ;
#81778 = DIRECTION ( 'NONE',  ( -0.6830127018922181881, 0.6830127018922202975, -0.2588190451025214056 ) ) ;
#81779 = CARTESIAN_POINT ( 'NONE',  ( 8.999999999999950262, 2.587461875839218273, 4.000000000000000000 ) ) ;
#81780 = CARTESIAN_POINT ( 'NONE',  ( 28.00000000000002487, -52.14999999999999147, -62.92499999999978400 ) ) ;
#81781 = CARTESIAN_POINT ( 'NONE',  ( -1.499999999999990896, 15.43112307739202471, 4.000000000000000000 ) ) ;
#81782 = AXIS2_PLACEMENT_3D ( 'NONE', #38341, #14446, #104277 ) ;
#81783 = DIRECTION ( 'NONE',  ( 0.3543493200069163240, -0.000000000000000000, 0.9351131265310288487 ) ) ;
#81784 = VERTEX_POINT ( 'NONE', #116584 ) ;
#81785 = ORIENTED_EDGE ( 'NONE', *, *, #132696, .F. ) ;
#81786 = DIRECTION ( 'NONE',  ( -0.7071067811865487940, 0.7071067811865463515, 0.000000000000000000 ) ) ;
#81787 = ORIENTED_EDGE ( 'NONE', *, *, #9186, .F. ) ;
#81788 = VECTOR ( 'NONE', #71429, 1000.000000000000000 ) ;
#81789 = AXIS2_PLACEMENT_3D ( 'NONE', #6396, #103602, #28217 ) ;
#81790 =( BOUNDED_CURVE ( )  B_SPLINE_CURVE ( 2, ( #47462, #3172, #27072, #82213, #90938, #2444, #80077, #91627, #46755, #135165, #104636, #5303, #124252 ),
 .UNSPECIFIED., .F., .F. ) 
 B_SPLINE_CURVE_WITH_KNOTS ( ( 3, 2, 2, 2, 2, 2, 3 ),
 ( 0.6500000000000001332, 0.6583333333333334370, 0.6666666666666667407, 0.6750000000000001554, 0.6833333333333334592, 0.6916666666666667629, 0.7000000000000000666 ),
 .UNSPECIFIED. ) 
 CURVE ( )  GEOMETRIC_REPRESENTATION_ITEM ( )  RATIONAL_B_SPLINE_CURVE ( ( 0.9999999999999995559, 0.9659258262890687563, 1.000000000000000000, 0.9659258262890683122, 1.000000000000000000, 0.9659258262890683122, 1.000000000000000000, 0.9659258262890683122, 1.000000000000000000, 0.9659258262890683122, 1.000000000000000000, 0.9659258262890678681, 1.000000000000000444 ) ) 
 REPRESENTATION_ITEM ( '' )  );
#81791 = LINE ( 'NONE', #83933, #12705 ) ;
#81792 = VERTEX_POINT ( 'NONE', #50618 ) ;
#81793 = FACE_OUTER_BOUND ( 'NONE', #76160, .T. ) ;
#81794 = DIRECTION ( 'NONE',  ( 0.7071067811865487940, 0.7071067811865463515, 0.000000000000000000 ) ) ;
#81795 = LINE ( 'NONE', #57903, #25297 ) ;
#81796 = VECTOR ( 'NONE', #90782, 1000.000000000000000 ) ;
#81797 = LINE ( 'NONE', #36136, #141660 ) ;
#81798 = ORIENTED_EDGE ( 'NONE', *, *, #91138, .T. ) ;
#81799 = EDGE_CURVE ( 'NONE', #132568, #99900, #28873, .T. ) ;
#81800 = DIRECTION ( 'NONE',  ( 0.6830127018922181881, 0.6830127018922202975, -0.2588190451025214056 ) ) ;
#81801 = DIRECTION ( 'NONE',  ( 0.000000000000000000, 0.000000000000000000, 1.000000000000000000 ) ) ;
#81802 = ORIENTED_EDGE ( 'NONE', *, *, #55586, .F. ) ;
#81803 = CARTESIAN_POINT ( 'NONE',  ( 23.99451991528749062, 28.92564299267954908, 4.000000000000000000 ) ) ;
#81804 = VERTEX_POINT ( 'NONE', #128879 ) ;
#81806 = ORIENTED_EDGE ( 'NONE', *, *, #125858, .F. ) ;
#81805 = EDGE_CURVE ( 'NONE', #76331, #116521, #29559, .T. ) ;
#81807 = ADVANCED_FACE ( 'NONE', ( #117968 ), #62948, .T. ) ;
#81808 = DIRECTION ( 'NONE',  ( -0.6830127018922180770, -0.6830127018922204085, -0.2588190451025213501 ) ) ;
#81809 = ORIENTED_EDGE ( 'NONE', *, *, #26144, .T. ) ;
#81810 = ORIENTED_EDGE ( 'NONE', *, *, #83350, .T. ) ;
#81811 = VECTOR ( 'NONE', #128615, 1000.000000000000000 ) ;
#81812 = CARTESIAN_POINT ( 'NONE',  ( 70.14626352523144703, -4.472830434245840259, 4.472830434245838482 ) ) ;
#81813 = VERTEX_POINT ( 'NONE', #66504 ) ;
#81814 = EDGE_CURVE ( 'NONE', #2927, #47322, #88977, .T. ) ;
#81815 = EDGE_CURVE ( 'NONE', #49412, #34663, #11030, .T. ) ;
#81816 = CARTESIAN_POINT ( 'NONE',  ( 95.50000000000000000, 0.000000000000000000, -7.950000000000000178 ) ) ;
#81818 = EDGE_CURVE ( 'NONE', #101163, #88773, #75940, .T. ) ;
#81817 = DIRECTION ( 'NONE',  ( 0.6830127018922180770, -0.6830127018922204085, -0.2588190451025213501 ) ) ;
#81819 = CARTESIAN_POINT ( 'NONE',  ( 112.8754301918981042, -5.291415217122920289, -3.055000000000001492 ) ) ;
#81820 = DIRECTION ( 'NONE',  ( -0.7071067811865487940, 0.7071067811865463515, -0.000000000000000000 ) ) ;
#81821 = ADVANCED_FACE ( 'NONE', ( #99827 ), #493, .F. ) ;
#81822 = LINE ( 'NONE', #112977, #136195 ) ;
#81823 = CARTESIAN_POINT ( 'NONE',  ( -34.92382263987071411, 21.75929247661549226, 4.252424926123421933 ) ) ;
#81824 = CARTESIAN_POINT ( 'NONE',  ( 6.183988606268994381, 28.73617430169791476, 5.000000000000000000 ) ) ;
#81825 = VECTOR ( 'NONE', #64533, 1000.000000000000000 ) ;
#81826 = ADVANCED_FACE ( 'NONE', ( #87530 ), #122270, .F. ) ;
#81827 = CYLINDRICAL_SURFACE ( 'NONE', #121039, 7.950000000000000178 ) ;
#81828 = VECTOR ( 'NONE', #137787, 1000.000000000000000 ) ;
#81829 = LINE ( 'NONE', #82509, #100021 ) ;
#81830 = CARTESIAN_POINT ( 'NONE',  ( 0.000000000000000000, 60.00000000000000000, 0.000000000000000000 ) ) ;
#81831 = ADVANCED_FACE ( 'NONE', ( #12091 ), #110669, .F. ) ;
#81832 = VERTEX_POINT ( 'NONE', #31721 ) ;
#81833 = CARTESIAN_POINT ( 'NONE',  ( -29.99999999999979039, -21.03360074219752462, 5.000000000000000000 ) ) ;
#81834 = DIRECTION ( 'NONE',  ( -0.3543493200069162685, -0.000000000000000000, -0.9351131265310288487 ) ) ;
#81835 = VERTEX_POINT ( 'NONE', #20105 ) ;
#81836 = EDGE_LOOP ( 'NONE', ( #140807, #85609, #30945, #57419 ) ) ;
#81837 = AXIS2_PLACEMENT_3D ( 'NONE', #101687, #47376, #79986 ) ;
#81838 = ORIENTED_EDGE ( 'NONE', *, *, #69380, .T. ) ;
#81839 = CARTESIAN_POINT ( 'NONE',  ( 25.39999999999999858, -2.599999999999900169, -1.445354724476153568E-14 ) ) ;
#81840 = ORIENTED_EDGE ( 'NONE', *, *, #134164, .F. ) ;
#81841 = CARTESIAN_POINT ( 'NONE',  ( 24.34427593291135139, 5.931737808750704666, 4.000000000000000000 ) ) ;
#81842 = CARTESIAN_POINT ( 'NONE',  ( -19.49999999999985434, 13.08746187583910725, 4.000000000000000000 ) ) ;
#81843 = EDGE_CURVE ( 'NONE', #73190, #22203, #132503, .T. ) ;
#81844 = FACE_OUTER_BOUND ( 'NONE', #124517, .T. ) ;
#81845 = FACE_OUTER_BOUND ( 'NONE', #137182, .T. ) ;
#81846 = EDGE_LOOP ( 'NONE', ( #105826, #83525, #4605, #13411, #132671, #29851 ) ) ;
#81847 = CARTESIAN_POINT ( 'NONE',  ( 27.79289321881326558, 3.759292476615680112, 5.000000000000000000 ) ) ;
#81848 = EDGE_LOOP ( 'NONE', ( #8980, #100139, #143072, #99939 ) ) ;
#81849 = ADVANCED_FACE ( 'NONE', ( #9197 ), #141936, .T. ) ;
#81850 = DIRECTION ( 'NONE',  ( 0.000000000000000000, -1.000000000000000000, 0.000000000000000000 ) ) ;
#81851 = CIRCLE ( 'NONE', #86388, 6.499999999999999112 ) ;
#81852 = CARTESIAN_POINT ( 'NONE',  ( 29.81706980810189478, -2.126176841940956130, 7.934999999999991616 ) ) ;
#81853 = PLANE ( 'NONE',  #82965 ) ;
#81854 = PLANE ( 'NONE',  #7249 ) ;
#81855 = ORIENTED_EDGE ( 'NONE', *, *, #138477, .F. ) ;
#81856 = ORIENTED_EDGE ( 'NONE', *, *, #89250, .F. ) ;
#81857 = ORIENTED_EDGE ( 'NONE', *, *, #62378, .F. ) ;
#81858 = CARTESIAN_POINT ( 'NONE',  ( -69.48921356237309510, -27.52281430457103895, 5.000000000000000000 ) ) ;
#81859 = DIRECTION ( 'NONE',  ( 0.7071067811865487940, 0.7071067811865463515, 0.000000000000000000 ) ) ;
#81860 = CARTESIAN_POINT ( 'NONE',  ( 0.000000000000000000, 0.000000000000000000, 5.000000000000000000 ) ) ;
#81861 = PRESENTATION_STYLE_ASSIGNMENT (( #103546 ) ) ;
#81862 = ORIENTED_EDGE ( 'NONE', *, *, #142868, .T. ) ;
#81863 = AXIS2_PLACEMENT_3D ( 'NONE', #18462, #51864, #126532 ) ;
#81864 = DIRECTION ( 'NONE',  ( -0.6830127018922180770, -0.6830127018922204085, -0.2588190451025213501 ) ) ;
#81865 = DIRECTION ( 'NONE',  ( -1.000000000000000000, -1.224606353822377258E-16, -0.000000000000000000 ) ) ;
#81866 = CARTESIAN_POINT ( 'NONE',  ( -21.98911971346036154, -22.02621442084248216, 4.990779571109221990 ) ) ;
#81867 = AXIS2_PLACEMENT_3D ( 'NONE', #126155, #26822, #58074 ) ;
#81868 = FACE_OUTER_BOUND ( 'NONE', #44077, .T. ) ;
#81869 = CARTESIAN_POINT ( 'NONE',  ( -34.92500000000001137, 21.72500000000000142, 5.000000000000000000 ) ) ;
#81870 = EDGE_CURVE ( 'NONE', #57148, #55993, #108822, .T. ) ;
#81871 = VERTEX_POINT ( 'NONE', #46201 ) ;
#81872 = CARTESIAN_POINT ( 'NONE',  ( 74.50000000000000000, 0.000000000000000000, -7.950000000000000178 ) ) ;
#81873 = CARTESIAN_POINT ( 'NONE',  ( 0.1839886062690032631, 28.73617430169787568, 5.000000000000000000 ) ) ;
#81874 = ORIENTED_EDGE ( 'NONE', *, *, #55110, .T. ) ;
#81875 = EDGE_CURVE ( 'NONE', #96656, #114250, #36027, .T. ) ;
#81876 = AXIS2_PLACEMENT_3D ( 'NONE', #98913, #22067, #87352 ) ;
#81877 = DIRECTION ( 'NONE',  ( -0.6830127018922180770, -0.6830127018922204085, -0.2588190451025213501 ) ) ;
#81878 = ORIENTED_EDGE ( 'NONE', *, *, #63254, .T. ) ;
#81879 = VERTEX_POINT ( 'NONE', #4735 ) ;
#81880 = CARTESIAN_POINT ( 'NONE',  ( -2.816011393730999401, 28.73617430169785436, 5.000000000000000000 ) ) ;
#81881 = LINE ( 'NONE', #49241, #95605 ) ;
#81882 = CARTESIAN_POINT ( 'NONE',  ( -15.48921356237309510, -27.52281430457066236, 5.000000000000000000 ) ) ;
#81883 = ORIENTED_EDGE ( 'NONE', *, *, #32017, .T. ) ;
#81884 = LINE ( 'NONE', #36898, #49021 ) ;
#81885 = ORIENTED_EDGE ( 'NONE', *, *, #92325, .T. ) ;
#81886 = EDGE_CURVE ( 'NONE', #36132, #13236, #85771, .T. ) ;
#81887 = VECTOR ( 'NONE', #101909, 999.9999999999998863 ) ;
#81888 = DIRECTION ( 'NONE',  ( -0.3543493200069162685, -0.000000000000000000, -0.9351131265310288487 ) ) ;
#81889 = FACE_OUTER_BOUND ( 'NONE', #36395, .T. ) ;
#81890 = CARTESIAN_POINT ( 'NONE',  ( 127.6833603837962414, -2.130196079827426203, 7.949999999999997513 ) ) ;
#81892 = CIRCLE ( 'NONE', #86422, 0.5000000000000013323 ) ;
#81891 = PLANE ( 'NONE',  #92453 ) ;
#81893 = CARTESIAN_POINT ( 'NONE',  ( 20.36747333860806819, -2.499999999999996447, 0.000000000000000000 ) ) ;
#81894 = ADVANCED_FACE ( 'NONE', ( #15623 ), #81681, .F. ) ;
#81895 = DIRECTION ( 'NONE',  ( -0.7071067811865486830, -0.7071067811865464625, -0.000000000000000000 ) ) ;
#81896 = CARTESIAN_POINT ( 'NONE',  ( 4.911592354503321545, 3.061616997868380183E-16, -2.500000000000001332 ) ) ;
#81897 = FACE_OUTER_BOUND ( 'NONE', #25578, .T. ) ;
#81898 = CARTESIAN_POINT ( 'NONE',  ( 26.08290314143522082, 3.967499999999992699, -6.871911579029513994 ) ) ;
#81899 = CARTESIAN_POINT ( 'NONE',  ( 7.707903141435219929, -6.871911579029513106, -3.967499999999993587 ) ) ;
#81900 = VECTOR ( 'NONE', #75301, 1000.000000000000000 ) ;
#81901 = CARTESIAN_POINT ( 'NONE',  ( -21.87889065874226091, 8.431076354171498366, 5.000000000000000000 ) ) ;
#81902 = DIRECTION ( 'NONE',  ( -1.000000000000000000, -1.224606353822377258E-16, -0.000000000000000000 ) ) ;
#81903 = DIRECTION ( 'NONE',  ( 1.000000000000000000, 0.000000000000000000, 0.000000000000000000 ) ) ;
#81904 = VERTEX_POINT ( 'NONE', #112152 ) ;
#81905 = ORIENTED_EDGE ( 'NONE', *, *, #66494, .F. ) ;
#81906 = CARTESIAN_POINT ( 'NONE',  ( 91.12500000000000000, -7.950000000000000178, -4.867971026610729436E-16 ) ) ;
#81907 = ORIENTED_EDGE ( 'NONE', *, *, #14377, .F. ) ;
#81908 = VERTEX_POINT ( 'NONE', #57072 ) ;
#81909 = EDGE_CURVE ( 'NONE', #17986, #69434, #90376, .T. ) ;
#81910 = CARTESIAN_POINT ( 'NONE',  ( -14.70025512860841133, -27.71228299555195917, 4.000000000000000000 ) ) ;
#81911 = CARTESIAN_POINT ( 'NONE',  ( 22.21247294953710494, 0.000000000000000000, 6.094999999999989981 ) ) ;
#81912 = VECTOR ( 'NONE', #78607, 1000.000000000000000 ) ;
#81913 = DIRECTION ( 'NONE',  ( -0.3543493200069162685, -0.000000000000000000, -0.9351131265310288487 ) ) ;
#81914 = EDGE_LOOP ( 'NONE', ( #133002, #53583, #38582, #48916 ) ) ;
#81915 = DIRECTION ( 'NONE',  ( 0.000000000000000000, 1.000000000000000000, 0.000000000000000000 ) ) ;
#81916 = FACE_OUTER_BOUND ( 'NONE', #34026, .T. ) ;
#81917 = CARTESIAN_POINT ( 'NONE',  ( 131.8806778009766276, -52.14999999999999147, -40.92499999999998295 ) ) ;
#81918 = CARTESIAN_POINT ( 'NONE',  ( 125.9070329220101030, 2.912925644401998859, -6.976214294840302088 ) ) ;
#81919 = ADVANCED_FACE ( 'NONE', ( #103372 ), #92500, .T. ) ;
#81920 = EDGE_CURVE ( 'NONE', #8586, #100840, #37442, .T. ) ;
#81922 = EDGE_CURVE ( 'NONE', #117423, #16702, #36702, .T. ) ;
#81921 = CARTESIAN_POINT ( 'NONE',  ( -33.18398860626899705, 28.73617430169810305, 5.000000000000000000 ) ) ;
#81923 = LINE ( 'NONE', #71737, #35799 ) ;
#81924 = PLANE ( 'NONE',  #132802 ) ;
#81925 = FACE_OUTER_BOUND ( 'NONE', #135318, .T. ) ;
#81926 = DIRECTION ( 'NONE',  ( -1.000000000000000000, -1.224606353822377258E-16, -0.000000000000000000 ) ) ;
#81927 = CARTESIAN_POINT ( 'NONE',  ( 10.37159235450332062, -2.500000000000000444, 3.061616997868384620E-16 ) ) ;
#81928 = LINE ( 'NONE', #39096, #8227 ) ;
#81929 = CARTESIAN_POINT ( 'NONE',  ( -26.99999999999980105, -16.44781430457065241, 5.000000000000000000 ) ) ;
#81930 = ADVANCED_FACE ( 'NONE', ( #70798 ), #115855, .T. ) ;
#81931 = ORIENTED_EDGE ( 'NONE', *, *, #77495, .F. ) ;
#81932 = ORIENTED_EDGE ( 'NONE', *, *, #111719, .F. ) ;
#81933 = CARTESIAN_POINT ( 'NONE',  ( 108.0629301918980900, 1.637169565754157174, 6.110000000000002984 ) ) ;
#81934 = AXIS2_PLACEMENT_3D ( 'NONE', #111549, #12226, #1338 ) ;
#81935 = ORIENTED_EDGE ( 'NONE', *, *, #85740, .T. ) ;
#81936 = FACE_OUTER_BOUND ( 'NONE', #113014, .T. ) ;
#81937 = SURFACE_SIDE_STYLE ('',( #24650 ) ) ;
#81938 = ORIENTED_EDGE ( 'NONE', *, *, #94394, .T. ) ;
#81939 = DIRECTION ( 'NONE',  ( -0.000000000000000000, 0.000000000000000000, 1.000000000000000000 ) ) ;
#81942 = EDGE_CURVE ( 'NONE', #136439, #141981, #130489, .T. ) ;
#81941 = AXIS2_PLACEMENT_3D ( 'NONE', #66612, #71606, #127391 ) ;
#81940 = PLANE ( 'NONE',  #7155 ) ;
#81943 = CARTESIAN_POINT ( 'NONE',  ( 105.6412635252314658, 4.472830434245836706, 4.472830434245840259 ) ) ;
#81944 = EDGE_CURVE ( 'NONE', #1174, #140583, #113542, .T. ) ;
#81945 = EDGE_LOOP ( 'NONE', ( #123177, #65727, #139657, #3266, #4265, #101341 ) ) ;
#81946 = ORIENTED_EDGE ( 'NONE', *, *, #34651, .T. ) ;
#81947 = DIRECTION ( 'NONE',  ( 0.7071067811865487940, 0.7071067811865463515, 0.000000000000000000 ) ) ;
#81948 = PLANE ( 'NONE',  #56473 ) ;
#81949 = DIRECTION ( 'NONE',  ( -0.6830127018922180770, -0.6830127018922204085, -0.2588190451025213501 ) ) ;
#81950 = ORIENTED_EDGE ( 'NONE', *, *, #104313, .F. ) ;
#81951 = ORIENTED_EDGE ( 'NONE', *, *, #123510, .T. ) ;
#81952 = VERTEX_POINT ( 'NONE', #59224 ) ;
#81953 = LINE ( 'NONE', #5016, #70041 ) ;
#81954 = EDGE_CURVE ( 'NONE', #110220, #124632, #72253, .T. ) ;
#81955 =( REPRESENTATION_RELATIONSHIP ('NONE','NONE', #69070, #54265 ) REPRESENTATION_RELATIONSHIP_WITH_TRANSFORMATION ( #124196 )SHAPE_REPRESENTATION_RELATIONSHIP( ) );
#81956 = AXIS2_PLACEMENT_3D ( 'NONE', #14719, #115414, #58995 ) ;
#81957 =( NAMED_UNIT ( * ) SI_UNIT ( $, .STERADIAN. ) SOLID_ANGLE_UNIT ( ) );
#81958 = LINE ( 'NONE', #137013, #22189 ) ;
#81959 = EDGE_LOOP ( 'NONE', ( #84094, #96437, #68828, #34121 ) ) ;
#81960 = ORIENTED_EDGE ( 'NONE', *, *, #57198, .T. ) ;
#81961 = LINE ( 'NONE', #90676, #50191 ) ;
#81962 = ORIENTED_EDGE ( 'NONE', *, *, #2146, .F. ) ;
#81963 = ORIENTED_EDGE ( 'NONE', *, *, #127275, .F. ) ;
#81964 = DIRECTION ( 'NONE',  ( -0.6830127018922180770, -0.6830127018922204085, -0.2588190451025213501 ) ) ;
#81965 = LINE ( 'NONE', #20206, #2633 ) ;
#81966 = VERTEX_POINT ( 'NONE', #127282 ) ;
#81967 = VECTOR ( 'NONE', #117450, 1000.000000000000000 ) ;
#81968 = CARTESIAN_POINT ( 'NONE',  ( 41.99451991528749062, 28.92564299267967343, 4.000000000000000000 ) ) ;
#81969 = LINE ( 'NONE', #50031, #108469 ) ;
#81970 = CARTESIAN_POINT ( 'NONE',  ( -39.48921356237310221, -27.52281430457082934, 5.000000000000000000 ) ) ;
#81971 = VECTOR ( 'NONE', #140823, 1000.000000000000000 ) ;
#81972 = CARTESIAN_POINT ( 'NONE',  ( 5.999999999999952927, -3.412538124160716002, 4.000000000000000000 ) ) ;
#81973 = FACE_BOUND ( 'NONE', #32553, .T. ) ;
#81975 = ORIENTED_EDGE ( 'NONE', *, *, #102796, .T. ) ;
#81974 = VECTOR ( 'NONE', #18114, 1000.000000000000000 ) ;
#81976 = CARTESIAN_POINT ( 'NONE',  ( 33.70710678118631165, -12.74070752338415247, 5.000000000000000000 ) ) ;
#81977 = CARTESIAN_POINT ( 'NONE',  ( -11.70025512860841133, -27.71228299555198049, 4.000000000000000000 ) ) ;
#81978 = DIRECTION ( 'NONE',  ( 0.000000000000000000, -1.000000000000000000, 0.000000000000000000 ) ) ;
#81979 = VERTEX_POINT ( 'NONE', #82379 ) ;
#81980 = CYLINDRICAL_SURFACE ( 'NONE', #32053, 3.378199999999994319 ) ;
#81981 = ORIENTED_EDGE ( 'NONE', *, *, #132387, .F. ) ;
#81982 = ORIENTED_EDGE ( 'NONE', *, *, #60749, .T. ) ;
#81983 =( BOUNDED_CURVE ( )  B_SPLINE_CURVE ( 3, ( #119427, #128894, #20121, #108537 ),
 .UNSPECIFIED., .F., .T. ) 
 B_SPLINE_CURVE_WITH_KNOTS ( ( 4, 4 ),
 ( 5.106027341939297415, 6.645403452391243526 ),
 .UNSPECIFIED. ) 
 CURVE ( )  GEOMETRIC_REPRESENTATION_ITEM ( )  RATIONAL_B_SPLINE_CURVE ( ( 1.000000000000000000, 0.8120851936182322817, 0.8120851936182322817, 1.000000000000000000 ) ) 
 REPRESENTATION_ITEM ( '' )  );
#81984 = ORIENTED_EDGE ( 'NONE', *, *, #110116, .F. ) ;
#81985 = CIRCLE ( 'NONE', #105122, 2.500000000000000444 ) ;
#81986 = ADVANCED_FACE ( 'NONE', ( #51896 ), #96076, .F. ) ;
#81987 = CARTESIAN_POINT ( 'NONE',  ( 36.66209685856478018, -5.291415217122919401, 3.054999999999997939 ) ) ;
#81989 = ORIENTED_EDGE ( 'NONE', *, *, #59524, .F. ) ;
#81988 = VECTOR ( 'NONE', #80395, 1000.000000000000000 ) ;
#81990 = DIRECTION ( 'NONE',  ( -0.3543493200069162685, -0.000000000000000000, -0.9351131265310288487 ) ) ;
#81991 = EDGE_CURVE ( 'NONE', #645, #79854, #30110, .T. ) ;
#81992 = FACE_OUTER_BOUND ( 'NONE', #60933, .T. ) ;
#81993 = CARTESIAN_POINT ( 'NONE',  ( -24.48921356237309510, -27.52281430457072631, 5.000000000000000000 ) ) ;
#81994 = EDGE_LOOP ( 'NONE', ( #55164, #47331, #74868, #33245 ) ) ;
#81995 = EDGE_CURVE ( 'NONE', #115605, #96412, #83082, .T. ) ;
#81996 = CARTESIAN_POINT ( 'NONE',  ( -17.20710678118641468, -14.24070752338413648, 5.000000000000000000 ) ) ;
#81997 = CARTESIAN_POINT ( 'NONE',  ( -8.671830600776413434, 2.259292476615694323, 4.000000000000000000 ) ) ;
#81998 = VECTOR ( 'NONE', #99851, 1000.000000000000000 ) ;
#81999 = EDGE_CURVE ( 'NONE', #68379, #56807, #138903, .T. ) ;
#82000 = FILL_AREA_STYLE_COLOUR ( '', #5225 ) ;
#82001 = CARTESIAN_POINT ( 'NONE',  ( 34.92499999999998295, 22.22500000000000142, 4.000000000000000000 ) ) ;
#82002 = DIRECTION ( 'NONE',  ( -0.7071067811865486830, -0.7071067811865464625, -0.000000000000000000 ) ) ;
#82003 = CARTESIAN_POINT ( 'NONE',  ( 21.48921356237309155, -27.52281430457070499, 5.000000000000000000 ) ) ;
#82004 = LINE ( 'NONE', #116728, #107232 ) ;
#82005 = ADVANCED_FACE ( 'NONE', ( #128721 ), #139638, .T. ) ;
#82006 = VERTEX_POINT ( 'NONE', #105521 ) ;
#82007 = ORIENTED_EDGE ( 'NONE', *, *, #58667, .T. ) ;
#82008 = ORIENTED_EDGE ( 'NONE', *, *, #135412, .F. ) ;
#82009 = ORIENTED_EDGE ( 'NONE', *, *, #9571, .F. ) ;
#82010 =( LENGTH_UNIT ( ) NAMED_UNIT ( * ) SI_UNIT ( .MILLI., .METRE. ) );
#82011 = ORIENTED_EDGE ( 'NONE', *, *, #70924, .T. ) ;
#82012 = VERTEX_POINT ( 'NONE', #140313 ) ;
#82013 = CARTESIAN_POINT ( 'NONE',  ( 8.111591955682463606, 4.202752102959690472E-16, 0.000000000000000000 ) ) ;
#82014 = EDGE_CURVE ( 'NONE', #100660, #101323, #41001, .T. ) ;
#82015 = EDGE_CURVE ( 'NONE', #132444, #93212, #17789, .T. ) ;
#82016 = DIRECTION ( 'NONE',  ( 0.3543493200069162685, -0.000000000000000000, -0.9351131265310288487 ) ) ;
#82017 = ORIENTED_EDGE ( 'NONE', *, *, #82678, .F. ) ;
#82018 = DIRECTION ( 'NONE',  ( -0.5735764363510503783, -0.8191520442889886899, 0.000000000000000000 ) ) ;
#82019 = ORIENTED_EDGE ( 'NONE', *, *, #18970, .F. ) ;
#82020 = ADVANCED_FACE ( 'NONE', ( #93943 ), #38861, .T. ) ;
#82021 = DIRECTION ( 'NONE',  ( 0.3543493200069162685, -0.000000000000000000, -0.9351131265310288487 ) ) ;
#82022 = DIRECTION ( 'NONE',  ( 0.7071067811865487940, 0.7071067811865463515, 0.000000000000000000 ) ) ;
#82023 = VECTOR ( 'NONE', #44200, 999.9999999999998863 ) ;
#82024 =( NAMED_UNIT ( * ) SI_UNIT ( $, .STERADIAN. ) SOLID_ANGLE_UNIT ( ) );
#82025 = ORIENTED_EDGE ( 'NONE', *, *, #6359, .F. ) ;
#82027 = LINE ( 'NONE', #126888, #133298 ) ;
#82026 = CARTESIAN_POINT ( 'NONE',  ( 97.62043019189812298, 3.055000000000002380, -5.291415217122917625 ) ) ;
#82028 = ORIENTED_EDGE ( 'NONE', *, *, #20605, .T. ) ;
#82029 = EDGE_LOOP ( 'NONE', ( #104778, #63702, #47616, #62566 ) ) ;
#82030 = FACE_OUTER_BOUND ( 'NONE', #52233, .T. ) ;
#82031 = ORIENTED_EDGE ( 'NONE', *, *, #52372, .T. ) ;
#82032 = LINE ( 'NONE', #82717, #39485 ) ;
#82033 =( LENGTH_UNIT ( ) NAMED_UNIT ( * ) SI_UNIT ( .MILLI., .METRE. ) );
#82034 = CARTESIAN_POINT ( 'NONE',  ( -72.18398860626899705, 28.73617430169837661, 5.000000000000000000 ) ) ;
#82035 = LINE ( 'NONE', #37056, #49329 ) ;
#82036 = CARTESIAN_POINT ( 'NONE',  ( 180.9625229943972329, -48.82538788374324668, -38.96958855984423309 ) ) ;
#82038 = EDGE_LOOP ( 'NONE', ( #71375, #137184, #137803, #116170 ) ) ;
#82037 = AXIS2_PLACEMENT_3D ( 'NONE', #71996, #84978, #6652 ) ;
#82039 = LINE ( 'NONE', #71865, #124653 ) ;
#82040 = DIRECTION ( 'NONE',  ( -0.7071067811865486830, -0.7071067811865464625, -0.000000000000000000 ) ) ;
#82041 = CARTESIAN_POINT ( 'NONE',  ( 12.69999999999999574, -60.06289321881344279, 24.72882142070205091 ) ) ;
#82042 = EDGE_CURVE ( 'NONE', #41011, #71142, #94644, .T. ) ;
#82043 = ORIENTED_EDGE ( 'NONE', *, *, #28965, .T. ) ;
#82044 = CARTESIAN_POINT ( 'NONE',  ( -32.67183060077623935, 11.25929247661560240, 4.000000000000000000 ) ) ;
#82045 = LINE ( 'NONE', #113918, #636 ) ;
#82046 = EDGE_LOOP ( 'NONE', ( #130767, #60333, #130233, #43987 ) ) ;
#82048 = ORIENTED_EDGE ( 'NONE', *, *, #51376, .T. ) ;
#82047 = DIRECTION ( 'NONE',  ( -0.7071067811865486830, 0.7071067811865464625, 0.000000000000000000 ) ) ;
#82049 = ORIENTED_EDGE ( 'NONE', *, *, #14990, .F. ) ;
#82050 = CARTESIAN_POINT ( 'NONE',  ( 34.49999999999975842, -11.94567065516892512, 4.994342998332160555 ) ) ;
#82051 = CARTESIAN_POINT ( 'NONE',  ( 0.06011071044020009635, -9.740707523384184441, 10.89222023123380900 ) ) ;
#82052 = VECTOR ( 'NONE', #63615, 999.9999999999998863 ) ;
#82053 = VERTEX_POINT ( 'NONE', #104822 ) ;
#82054 = LINE ( 'NONE', #126237, #39613 ) ;
#82055 = EDGE_CURVE ( 'NONE', #58993, #51758, #107671, .T. ) ;
#82056 = CARTESIAN_POINT ( 'NONE',  ( -31.49999999999977973, 21.05218569542895679, 5.000000000000000000 ) ) ;
#82057 = VECTOR ( 'NONE', #55662, 1000.000000000000000 ) ;
#82058 = DIRECTION ( 'NONE',  ( -0.000000000000000000, 0.3543493200069153248, 0.9351131265310292928 ) ) ;
#82059 = ORIENTED_EDGE ( 'NONE', *, *, #140904, .F. ) ;
#82060 = CARTESIAN_POINT ( 'NONE',  ( 8.865004262483717312, 3.759292476615678336, 15.36553568819724269 ) ) ;
#82062 = DIRECTION ( 'NONE',  ( -0.7071067811865486830, -0.7071067811865464625, 0.000000000000000000 ) ) ;
#82061 = VECTOR ( 'NONE', #53321, 1000.000000000000000 ) ;
#82063 = EDGE_CURVE ( 'NONE', #115378, #20512, #137468, .T. ) ;
#82064 = CARTESIAN_POINT ( 'NONE',  ( 3.250000000000000000, 4.999999999999998224, 8.040613248383180784E-16 ) ) ;
#82065 = LINE ( 'NONE', #60299, #56409 ) ;
#82066 = FACE_OUTER_BOUND ( 'NONE', #97097, .T. ) ;
#82067 = DIRECTION ( 'NONE',  ( 0.7071067811865486830, -0.7071067811865464625, -0.000000000000000000 ) ) ;
#82068 = DIRECTION ( 'NONE',  ( 0.5735764363510444941, 0.8191520442889929088, 0.000000000000000000 ) ) ;
#82069 = DIRECTION ( 'NONE',  ( -0.3543493200069162685, -0.000000000000000000, -0.9351131265310288487 ) ) ;
#82070 = ORIENTED_EDGE ( 'NONE', *, *, #74778, .T. ) ;
#82071 = ORIENTED_EDGE ( 'NONE', *, *, #15378, .F. ) ;
#82072 = ORIENTED_EDGE ( 'NONE', *, *, #43324, .T. ) ;
#82073 = CARTESIAN_POINT ( 'NONE',  ( 117.8125000000000000, 5.819803920172571310, 5.819803920172575751 ) ) ;
#82074 = VERTEX_POINT ( 'NONE', #8330 ) ;
#82075 = AXIS2_PLACEMENT_3D ( 'NONE', #88979, #34585, #33192 ) ;
#82076 = ORIENTED_EDGE ( 'NONE', *, *, #6492, .T. ) ;
#82077 = EDGE_CURVE ( 'NONE', #120532, #20063, #106221, .T. ) ;
#82078 = ORIENTED_EDGE ( 'NONE', *, *, #103114, .F. ) ;
#82079 = DIRECTION ( 'NONE',  ( -0.7071067811865486830, -0.7071067811865464625, -0.000000000000000000 ) ) ;
#82080 = CARTESIAN_POINT ( 'NONE',  ( -31.49999999999977973, -10.91253812416064584, 4.000000000000000000 ) ) ;
#82081 = ORIENTED_EDGE ( 'NONE', *, *, #108825, .F. ) ;
#82082 = LINE ( 'NONE', #105902, #32393 ) ;
#82083 = DIRECTION ( 'NONE',  ( 0.3543493200069162685, -0.000000000000000000, -0.9351131265310288487 ) ) ;
#82084 = VECTOR ( 'NONE', #48292, 1000.000000000000227 ) ;
#82085 = CARTESIAN_POINT ( 'NONE',  ( 20.67183060077632106, -3.740707523384244837, 4.000000000000000000 ) ) ;
#82086 = CARTESIAN_POINT ( 'NONE',  ( 109.5212635252314612, -4.472830434245839371, -4.472830434245840259 ) ) ;
#82087 = ADVANCED_FACE ( 'NONE', ( #6895 ), #52580, .F. ) ;
#82088 = VERTEX_POINT ( 'NONE', #84527 ) ;
#82089 = CARTESIAN_POINT ( 'NONE',  ( 0.000000000000000000, 0.000000000000000000, -6.349999999999999645 ) ) ;
#82090 = PLANE ( 'NONE',  #35375 ) ;
#82091 = LINE ( 'NONE', #59611, #116681 ) ;
#82092 = DIRECTION ( 'NONE',  ( -0.6830127018922181881, 0.6830127018922202975, -0.2588190451025214056 ) ) ;
#82093 = DIRECTION ( 'NONE',  ( -0.6830127018922180770, -0.6830127018922204085, -0.2588190451025213501 ) ) ;
#82094 = VECTOR ( 'NONE', #40633, 1000.000000000000000 ) ;
#82095 = CARTESIAN_POINT ( 'NONE',  ( 37.85002705046288440, -5.819803920172572198, -5.819803920172572198 ) ) ;
#82096 = FACE_OUTER_BOUND ( 'NONE', #17041, .T. ) ;
#82097 = CIRCLE ( 'NONE', #19540, 2.055000000000001048 ) ;
#82098 = FACE_OUTER_BOUND ( 'NONE', #47340, .T. ) ;
#82099 = ORIENTED_EDGE ( 'NONE', *, *, #26051, .T. ) ;
#82100 = VERTEX_POINT ( 'NONE', #19248 ) ;
#82101 = VECTOR ( 'NONE', #66678, 1000.000000000000000 ) ;
#82102 = CARTESIAN_POINT ( 'NONE',  ( 35.56249999999999289, -5.819803920172572198, -5.819803920172573086 ) ) ;
#82103 = ORIENTED_EDGE ( 'NONE', *, *, #109906, .T. ) ;
#82104 = ORIENTED_EDGE ( 'NONE', *, *, #21754, .F. ) ;
#82105 = CARTESIAN_POINT ( 'NONE',  ( 34.49999999999975131, 19.08746187583905751, 4.000000000000000000 ) ) ;
#82106 = CARTESIAN_POINT ( 'NONE',  ( -8.999999999999934275, -19.22509904557637128, 1.855685503482156662 ) ) ;
#82107 = EDGE_LOOP ( 'NONE', ( #41633, #60176, #35514, #25997 ) ) ;
#82108 = DIRECTION ( 'NONE',  ( 0.000000000000000000, 1.000000000000000000, 0.000000000000000000 ) ) ;
#82109 = CYLINDRICAL_SURFACE ( 'NONE', #97838, 3.999999999999996447 ) ;
#82110 = DIRECTION ( 'NONE',  ( 0.7071067811865487940, 0.7071067811865463515, 0.000000000000000000 ) ) ;
#82111 = VECTOR ( 'NONE', #127976, 1000.000000000000000 ) ;
#82112 = CARTESIAN_POINT ( 'NONE',  ( 25.08376352523143638, -6.110000000000001208, -3.741295971395164515E-16 ) ) ;
#82113 = ADVANCED_FACE ( 'NONE', ( #38161 ), #71495, .F. ) ;
#82114 = EDGE_LOOP ( 'NONE', ( #70578, #129236, #32081, #80205 ) ) ;
#82115 = EDGE_CURVE ( 'NONE', #141895, #5194, #125100, .T. ) ;
#82116 = CARTESIAN_POINT ( 'NONE',  ( 21.48921356237309155, -27.52281430457070499, 5.000000000000000000 ) ) ;
#82117 = ORIENTED_EDGE ( 'NONE', *, *, #114734, .T. ) ;
#82118 = LINE ( 'NONE', #73363, #141133 ) ;
#82119 = DIRECTION ( 'NONE',  ( -0.3543493200069162685, -0.000000000000000000, -0.9351131265310288487 ) ) ;
#82120 = DIRECTION ( 'NONE',  ( -1.000000000000000000, -0.000000000000000000, -0.000000000000000000 ) ) ;
#82121 = CARTESIAN_POINT ( 'NONE',  ( 62.54166666666666430, -3.975000000000002753, 6.884901960086286188 ) ) ;
#82123 = ADVANCED_FACE ( 'NONE', ( #31560 ), #33721, .F. ) ;
#82122 = ORIENTED_EDGE ( 'NONE', *, *, #18021, .T. ) ;
#82124 = ORIENTED_EDGE ( 'NONE', *, *, #95216, .F. ) ;
#82125 = CARTESIAN_POINT ( 'NONE',  ( 36.18398860626899705, 28.73617430169812437, 5.000000000000000000 ) ) ;
#82126 = EDGE_CURVE ( 'NONE', #101548, #29429, #132326, .T. ) ;
#82127 = CARTESIAN_POINT ( 'NONE',  ( -66.18398860626901126, 28.73617430169833753, 5.000000000000000000 ) ) ;
#82128 = CARTESIAN_POINT ( 'NONE',  ( 19.17183060077633172, -5.240707523384232402, 4.000000000000000000 ) ) ;
#82129 = CARTESIAN_POINT ( 'NONE',  ( 34.49999999999975131, 12.43112307739206024, 4.000000000000000000 ) ) ;
#82130 = CARTESIAN_POINT ( 'NONE',  ( 49.20376352523145158, 6.109999999999998543, 1.122388791418548911E-15 ) ) ;
#82131 = ORIENTED_EDGE ( 'NONE', *, *, #25530, .T. ) ;
#82132 = CARTESIAN_POINT ( 'NONE',  ( 30.18398860626900060, 28.73617430169808173, 5.000000000000000000 ) ) ;
#82133 = DIRECTION ( 'NONE',  ( 0.7071067811865487940, 0.7071067811865463515, -0.000000000000000000 ) ) ;
#82134 = ORIENTED_EDGE ( 'NONE', *, *, #84424, .T. ) ;
#82135 = VERTEX_POINT ( 'NONE', #98930 ) ;
#82136 = CARTESIAN_POINT ( 'NONE',  ( 60.48921356237309510, -27.52281430457097500, 5.000000000000000000 ) ) ;
#82137 = ORIENTED_EDGE ( 'NONE', *, *, #83151, .F. ) ;
#82138 = ADVANCED_FACE ( 'NONE', ( #33018 ), #109825, .T. ) ;
#82139 = CIRCLE ( 'NONE', #89058, 2.055000000000000604 ) ;
#82140 = CARTESIAN_POINT ( 'NONE',  ( 60.74586038379622721, 3.974999999999996980, 6.884901960086287964 ) ) ;
#82141 = ORIENTED_EDGE ( 'NONE', *, *, #37226, .T. ) ;
#82142 = DIRECTION ( 'NONE',  ( -0.7071067811865487940, 0.7071067811865463515, 0.000000000000000000 ) ) ;
#82143 =( NAMED_UNIT ( * ) SI_UNIT ( $, .STERADIAN. ) SOLID_ANGLE_UNIT ( ) );
#82144 = FACE_BOUND ( 'NONE', #65402, .T. ) ;
#82145 = DIRECTION ( 'NONE',  ( -0.3543493200069162685, -0.000000000000000000, -0.9351131265310288487 ) ) ;
#82146 = LINE ( 'NONE', #60388, #16693 ) ;
#82147 = DIRECTION ( 'NONE',  ( 0.7071067811865486830, -0.7071067811865464625, -0.000000000000000000 ) ) ;
#82148 = DIRECTION ( 'NONE',  ( 1.000000000000000000, 0.000000000000000000, 0.000000000000000000 ) ) ;
#82150 = VERTEX_POINT ( 'NONE', #22768 ) ;
#82149 = DIRECTION ( 'NONE',  ( 0.7071067811865486830, -0.7071067811865464625, -0.000000000000000000 ) ) ;
#82151 = VECTOR ( 'NONE', #70596, 1000.000000000000000 ) ;
#82152 = DIRECTION ( 'NONE',  ( 1.000000000000000000, 0.000000000000000000, 0.000000000000000000 ) ) ;
#82153 = ORIENTED_EDGE ( 'NONE', *, *, #78190, .F. ) ;
#82154 = VECTOR ( 'NONE', #7317, 1000.000000000000000 ) ;
#82156 = ORIENTED_EDGE ( 'NONE', *, *, #14636, .F. ) ;
#82155 = EDGE_CURVE ( 'NONE', #134004, #29420, #88082, .T. ) ;
#82157 = CARTESIAN_POINT ( 'NONE',  ( 63.20376352523145158, 6.109999999999998543, 1.122388791418548911E-15 ) ) ;
#82158 = ORIENTED_EDGE ( 'NONE', *, *, #39293, .F. ) ;
#82159 = DIRECTION ( 'NONE',  ( -0.000000000000000000, 0.3543493200069153248, 0.9351131265310292928 ) ) ;
#82160 = EDGE_CURVE ( 'NONE', #52188, #8725, #110509, .T. ) ;
#82161 = AXIS2_PLACEMENT_3D ( 'NONE', #101831, #2484, #35896 ) ;
#82162 = CARTESIAN_POINT ( 'NONE',  ( 8.206660635421465955, 21.75929247661549226, 4.998822639870702744 ) ) ;
#82163 = VERTEX_POINT ( 'NONE', #9787 ) ;
#82164 = SURFACE_SIDE_STYLE ('',( #47414 ) ) ;
#82165 = EDGE_CURVE ( 'NONE', #71270, #85690, #86664, .T. ) ;
#82166 = EDGE_CURVE ( 'NONE', #20488, #45231, #109096, .T. ) ;
#82167 = VECTOR ( 'NONE', #48306, 1000.000000000000000 ) ;
#82168 = CARTESIAN_POINT ( 'NONE',  ( 42.48921356237308800, -27.52281430457085065, 5.000000000000000000 ) ) ;
#82169 = CARTESIAN_POINT ( 'NONE',  ( 51.48921356237309510, -27.52281430457091460, 5.000000000000000000 ) ) ;
#82170 = DIRECTION ( 'NONE',  ( 1.000000000000000000, 0.000000000000000000, 0.000000000000000000 ) ) ;
#82171 = SURFACE_STYLE_USAGE ( .BOTH. , #95858 ) ;
#82172 = ORIENTED_EDGE ( 'NONE', *, *, #13248, .T. ) ;
#82173 = ORIENTED_EDGE ( 'NONE', *, *, #49774, .T. ) ;
#82174 = CARTESIAN_POINT ( 'NONE',  ( 24.29974487139158867, -27.71228299555223273, 4.000000000000000000 ) ) ;
#82175 = DIRECTION ( 'NONE',  ( 0.3543493200069162685, -0.000000000000000000, -0.9351131265310288487 ) ) ;
#82176 = EDGE_LOOP ( 'NONE', ( #20797, #54105, #50010, #48947 ) ) ;
#82177 = ORIENTED_EDGE ( 'NONE', *, *, #71991, .T. ) ;
#82178 = ORIENTED_EDGE ( 'NONE', *, *, #9737, .F. ) ;
#82179 = CARTESIAN_POINT ( 'NONE',  ( -19.05000000000000071, 3.174999999999997158, 4.000000000000000000 ) ) ;
#82180 = EDGE_CURVE ( 'NONE', #24024, #85105, #141009, .T. ) ;
#82181 = ADVANCED_FACE ( 'NONE', ( #11179 ), #124116, .T. ) ;
#82182 = DIRECTION ( 'NONE',  ( 0.3543493200069162685, -0.000000000000000000, -0.9351131265310288487 ) ) ;
#82183 = ORIENTED_EDGE ( 'NONE', *, *, #122434, .T. ) ;
#82184 = CARTESIAN_POINT ( 'NONE',  ( -2.218373117075048029, 21.74787736706806385, 4.999607392498049308 ) ) ;
#82185 = EDGE_CURVE ( 'NONE', #106062, #64397, #35149, .T. ) ;
#82186 = AXIS2_PLACEMENT_3D ( 'NONE', #93109, #63196, #103256 ) ;
#82187 = DIRECTION ( 'NONE',  ( 0.3543493200069162685, -0.000000000000000000, -0.9351131265310288487 ) ) ;
#82188 = VECTOR ( 'NONE', #79903, 1000.000000000000000 ) ;
#82189 = CARTESIAN_POINT ( 'NONE',  ( 10.56706980810188945, 2.126176841940952134, -7.934999999999993392 ) ) ;
#82190 = VECTOR ( 'NONE', #122989, 1000.000000000000227 ) ;
#82191 = PLANE ( 'NONE',  #123624 ) ;
#82192 = ORIENTED_EDGE ( 'NONE', *, *, #27489, .F. ) ;
#82193 = AXIS2_PLACEMENT_3D ( 'NONE', #10754, #55738, #141289 ) ;
#82194 = CARTESIAN_POINT ( 'NONE',  ( -5.700255128608413102, -27.71228299555201957, 4.000000000000000000 ) ) ;
#82195 = CARTESIAN_POINT ( 'NONE',  ( -29.99999999999979394, -19.22509904557638905, 1.855685503482108256 ) ) ;
#82196 = EDGE_CURVE ( 'NONE', #133600, #16078, #114109, .T. ) ;
#82198 = ORIENTED_EDGE ( 'NONE', *, *, #113757, .T. ) ;
#82197 = DIRECTION ( 'NONE',  ( 0.000000000000000000, -1.000000000000000000, 0.000000000000000000 ) ) ;
#82199 = DIRECTION ( 'NONE',  ( -0.000000000000000000, -0.3543493200069152693, 0.9351131265310292928 ) ) ;
#82200 = ORIENTED_EDGE ( 'NONE', *, *, #36112, .F. ) ;
#82201 = LINE ( 'NONE', #60445, #86628 ) ;
#82202 = CARTESIAN_POINT ( 'NONE',  ( 34.92499999999998295, 0.6624618758390189432, 4.000000000000000000 ) ) ;
#82203 = PLANE ( 'NONE',  #54030 ) ;
#82204 = ORIENTED_EDGE ( 'NONE', *, *, #14565, .F. ) ;
#82205 = DIRECTION ( 'NONE',  ( 1.000000000000000000, 0.000000000000000000, 0.000000000000000000 ) ) ;
#82206 = CARTESIAN_POINT ( 'NONE',  ( 13.49999999999990763, 18.05218569542898521, 5.000000000000000000 ) ) ;
#82207 = DIRECTION ( 'NONE',  ( 0.000000000000000000, -1.000000000000000000, 0.000000000000000000 ) ) ;
#82208 = FACE_OUTER_BOUND ( 'NONE', #142711, .T. ) ;
#82209 = EDGE_CURVE ( 'NONE', #75880, #23207, #69938, .T. ) ;
#82210 = VERTEX_POINT ( 'NONE', #23523 ) ;
#82211 = LINE ( 'NONE', #18305, #53145 ) ;
#82212 = CARTESIAN_POINT ( 'NONE',  ( -17.99999999999987566, 11.58746187583913390, 4.000000000000000000 ) ) ;
#82213 = CARTESIAN_POINT ( 'NONE',  ( 20.89997294953711204, 4.461849672132297329, -4.461849672132302658 ) ) ;
#82214 = CARTESIAN_POINT ( 'NONE',  ( -6.183988606268994381, 28.73617430169791476, 5.000000000000000000 ) ) ;
#82215 = LINE ( 'NONE', #116941, #120021 ) ;
#82216 = ORIENTED_EDGE ( 'NONE', *, *, #20091, .F. ) ;
#82217 = ADVANCED_FACE ( 'NONE', ( #12640 ), #47478, .F. ) ;
#82218 = VERTEX_POINT ( 'NONE', #100391 ) ;
#82219 = CARTESIAN_POINT ( 'NONE',  ( -2.292893218813443657, 8.259292476615634371, 5.000000000000000000 ) ) ;
#82220 = PLANE ( 'NONE',  #85333 ) ;
#82221 = EDGE_CURVE ( 'NONE', #108587, #104249, #34409, .T. ) ;
#82222 = CARTESIAN_POINT ( 'NONE',  ( 6.832903141435220817, -3.967499999999994476, 6.871911579029513106 ) ) ;
#82223 = DIRECTION ( 'NONE',  ( -0.3543493200069162685, -0.000000000000000000, -0.9351131265310288487 ) ) ;
#82224 = LINE ( 'NONE', #14788, #50770 ) ;
#82225 = CARTESIAN_POINT ( 'NONE',  ( -0.2392503087990174859, 22.22500000000000142, -8.143727179408113415 ) ) ;
#82226 = DIRECTION ( 'NONE',  ( 0.7071067811865487940, 0.7071067811865463515, 0.000000000000000000 ) ) ;
#82227 = ORIENTED_EDGE ( 'NONE', *, *, #11221, .T. ) ;
#82228 = DIRECTION ( 'NONE',  ( -0.7071067811865486830, -0.7071067811865464625, 0.000000000000000000 ) ) ;
#82229 = PLANE ( 'NONE',  #88670 ) ;
#82230 =( NAMED_UNIT ( * ) SI_UNIT ( $, .STERADIAN. ) SOLID_ANGLE_UNIT ( ) );
#82231 = CARTESIAN_POINT ( 'NONE',  ( 48.18293019189812298, -1.637169565754159173, -6.109999999999999432 ) ) ;
#82232 = PLANE ( 'NONE',  #71950 ) ;
#82233 = EDGE_LOOP ( 'NONE', ( #12980, #8975, #109183, #30082 ) ) ;
#82234 = PLANE ( 'NONE',  #62734 ) ;
#82235 = VERTEX_POINT ( 'NONE', #123596 ) ;
#82236 = ORIENTED_EDGE ( 'NONE', *, *, #111587, .T. ) ;
#82237 = FACE_OUTER_BOUND ( 'NONE', #101408, .T. ) ;
#82238 = DIRECTION ( 'NONE',  ( -0.7071067811865487940, 0.7071067811865463515, 0.000000000000000000 ) ) ;
#82239 = FACE_OUTER_BOUND ( 'NONE', #95938, .T. ) ;
#82240 = FACE_OUTER_BOUND ( 'NONE', #118937, .T. ) ;
#82241 = LINE ( 'NONE', #115507, #132098 ) ;
#82242 = DIRECTION ( 'NONE',  ( 0.7071067811865487940, 0.7071067811865463515, -0.000000000000000000 ) ) ;
#82243 = EDGE_LOOP ( 'NONE', ( #52333, #13177, #136313, #60428, #123603 ) ) ;
#82244 = CARTESIAN_POINT ( 'NONE',  ( 1.774971111182638506, 0.9254518332604928510, -6.256315204308075195 ) ) ;
#82245 = LINE ( 'NONE', #116273, #60745 ) ;
#82246 = UNCERTAINTY_MEASURE_WITH_UNIT (LENGTH_MEASURE( 1.000000000000000082E-05 ), #95802, 'distance_accuracy_value', 'NONE');
#82247 = CARTESIAN_POINT ( 'NONE',  ( -34.92500000000001137, -15.28150956279560191, 4.759050581649335143 ) ) ;
#82248 = DIRECTION ( 'NONE',  ( -0.000000000000000000, 0.000000000000000000, 1.000000000000000000 ) ) ;
#82249 = CARTESIAN_POINT ( 'NONE',  ( 117.5208333333333428, 7.949999999999998401, 2.130196079827431532 ) ) ;
#82250 = CARTESIAN_POINT ( 'NONE',  ( 69.49586038379622721, -3.974999999999998312, -6.884901960086286188 ) ) ;
#82251 = VECTOR ( 'NONE', #81011, 1000.000000000000000 ) ;
#82252 = FACE_OUTER_BOUND ( 'NONE', #2287, .T. ) ;
#82253 = ORIENTED_EDGE ( 'NONE', *, *, #43998, .T. ) ;
#82254 = VERTEX_POINT ( 'NONE', #102542 ) ;
#82255 = CARTESIAN_POINT ( 'NONE',  ( 60.93750000000000000, 5.819803920172573974, -5.819803920172572198 ) ) ;
#82256 = CARTESIAN_POINT ( 'NONE',  ( -0.5240013858544890768, 22.03583458319438648, 4.979811245910087614 ) ) ;
#82257 = VECTOR ( 'NONE', #102403, 999.9999999999998863 ) ;
#82258 = DIRECTION ( 'NONE',  ( 0.7071067811865487940, 0.7071067811865463515, 0.000000000000000000 ) ) ;
#82259 = DIRECTION ( 'NONE',  ( 0.000000000000000000, 1.000000000000000000, -0.000000000000000000 ) ) ;
#82260 = ORIENTED_EDGE ( 'NONE', *, *, #99785, .F. ) ;
#82261 = FACE_OUTER_BOUND ( 'NONE', #96068, .T. ) ;
#82262 = VECTOR ( 'NONE', #128220, 1000.000000000000000 ) ;
#82263 = CARTESIAN_POINT ( 'NONE',  ( -12.70000000000000817, -1.739288537755694446E-15, -0.5000000000000004441 ) ) ;
#82264 = CARTESIAN_POINT ( 'NONE',  ( 56.58376352523143993, -6.110000000000001208, -3.741295971395164515E-16 ) ) ;
#82265 = PLANE ( 'NONE',  #11211 ) ;
#82266 = ORIENTED_EDGE ( 'NONE', *, *, #81051, .T. ) ;
#82267 = VERTEX_POINT ( 'NONE', #68498 ) ;
#82268 = CARTESIAN_POINT ( 'NONE',  ( -35.95341186370433206, 14.25929247661557042, 18.84478104361335937 ) ) ;
#82269 = CARTESIAN_POINT ( 'NONE',  ( 0.000000000000000000, 0.000000000000000000, 5.000000000000000000 ) ) ;
#82270 = CARTESIAN_POINT ( 'NONE',  ( -4.499999999999964473, 0.05218569542916884352, 5.000000000000000000 ) ) ;
#82271 = ADVANCED_FACE ( 'NONE', ( #92330 ), #46023, .T. ) ;
#82272 = DIRECTION ( 'NONE',  ( -0.6830127018922181881, 0.6830127018922202975, -0.2588190451025214056 ) ) ;
#82274 = ORIENTED_EDGE ( 'NONE', *, *, #64686, .T. ) ;
#82273 = CARTESIAN_POINT ( 'NONE',  ( -34.49999999999975842, 16.18958161055400069, -11.56426086740819414 ) ) ;
#82275 = EDGE_CURVE ( 'NONE', #42602, #127303, #136557, .T. ) ;
#82276 = DIRECTION ( 'NONE',  ( -1.000000000000000000, -0.000000000000000000, -0.000000000000000000 ) ) ;
#82277 = PLANE ( 'NONE',  #47829 ) ;
#82278 = CARTESIAN_POINT ( 'NONE',  ( -48.48921356237309510, -27.52281430457089328, 5.000000000000000000 ) ) ;
#82279 = DIRECTION ( 'NONE',  ( -0.7071067811865487940, 0.7071067811865463515, -0.000000000000000000 ) ) ;
#82280 = VECTOR ( 'NONE', #135407, 1000.000000000000227 ) ;
#82281 = ORIENTED_EDGE ( 'NONE', *, *, #122794, .T. ) ;
#82282 = ORIENTED_EDGE ( 'NONE', *, *, #9012, .F. ) ;
#82284 = EDGE_CURVE ( 'NONE', #35225, #48229, #78632, .T. ) ;
#82283 = AXIS2_PLACEMENT_3D ( 'NONE', #39004, #115091, #82513 ) ;
#82285 = DIRECTION ( 'NONE',  ( -0.000000000000000000, -0.3543493200069152693, 0.9351131265310292928 ) ) ;
#82286 = CARTESIAN_POINT ( 'NONE',  ( -38.99451991528749062, 28.92564299267965211, 4.000000000000000000 ) ) ;
#82287 = PLANE ( 'NONE',  #135764 ) ;
#82288 = FILL_AREA_STYLE_COLOUR ( '', #1482 ) ;
#82289 = ORIENTED_EDGE ( 'NONE', *, *, #53124, .F. ) ;
#82290 = EDGE_LOOP ( 'NONE', ( #138277, #34857, #48189 ) ) ;
#82291 = FACE_OUTER_BOUND ( 'NONE', #65977, .T. ) ;
#82292 = FACE_OUTER_BOUND ( 'NONE', #57714, .T. ) ;
#82293 = ADVANCED_FACE ( 'NONE', ( #80782 ), #134543, .T. ) ;
#82294 = ORIENTED_EDGE ( 'NONE', *, *, #4713, .F. ) ;
#82295 = LINE ( 'NONE', #143076, #2754 ) ;
#82296 = ORIENTED_EDGE ( 'NONE', *, *, #599, .F. ) ;
#82297 = CARTESIAN_POINT ( 'NONE',  ( 66.29974487139159578, -27.71228299555252406, 4.000000000000000000 ) ) ;
#82298 = DIRECTION ( 'NONE',  ( -0.7071067811865486830, -0.7071067811865464625, 0.000000000000000000 ) ) ;
#82299 = EDGE_CURVE ( 'NONE', #106502, #32200, #90953, .T. ) ;
#82300 = FACE_BOUND ( 'NONE', #39165, .T. ) ;
#82301 = CARTESIAN_POINT ( 'NONE',  ( 17.85999999999999943, 9.521314400968980422E-16, 0.000000000000000000 ) ) ;
#82302 = CARTESIAN_POINT ( 'NONE',  ( -2.862559987030901976, 22.22500000000000142, -7.149657077860686272 ) ) ;
#82303 = DIRECTION ( 'NONE',  ( -0.7071067811865487940, 0.7071067811865463515, -0.000000000000000000 ) ) ;
#82304 = PLANE ( 'NONE',  #48194 ) ;
#82305 = FACE_OUTER_BOUND ( 'NONE', #8220, .T. ) ;
#82306 = SHAPE_DEFINITION_REPRESENTATION ( #108328, #88538 ) ;
#82307 = ORIENTED_EDGE ( 'NONE', *, *, #52191, .T. ) ;
#82308 = VERTEX_POINT ( 'NONE', #57614 ) ;
#82309 = CARTESIAN_POINT ( 'NONE',  ( 97.18293019189810877, -1.637169565754158951, -6.109999999999998543 ) ) ;
#82310 = EDGE_LOOP ( 'NONE', ( #37002, #37601, #23825, #119823 ) ) ;
#82311 = DIRECTION ( 'NONE',  ( 0.7071067811865487940, 0.7071067811865463515, 0.000000000000000000 ) ) ;
#82312 = ADVANCED_FACE ( 'NONE', ( #35874 ), #80090, .F. ) ;
#82313 = CARTESIAN_POINT ( 'NONE',  ( -26.99999999999980815, -6.412538124160691133, 4.000000000000000000 ) ) ;
#82314 = EDGE_CURVE ( 'NONE', #59374, #45046, #62594, .T. ) ;
#82315 = ADVANCED_FACE ( 'NONE', ( #17623 ), #95197, .F. ) ;
#82316 = DIRECTION ( 'NONE',  ( 0.7071067811865487940, 0.7071067811865463515, 0.000000000000000000 ) ) ;
#82317 = VERTEX_POINT ( 'NONE', #6016 ) ;
#82318 = LINE ( 'NONE', #126499, #18231 ) ;
#82319 = LINE ( 'NONE', #16295, #20004 ) ;
#82320 = PLANE ( 'NONE',  #131481 ) ;
#82322 = CARTESIAN_POINT ( 'NONE',  ( 42.48921356237308800, -27.52281430457085065, 5.000000000000000000 ) ) ;
#82321 = DIRECTION ( 'NONE',  ( 0.000000000000000000, -1.000000000000000000, 0.000000000000000000 ) ) ;
#82323 = LINE ( 'NONE', #126505, #88641 ) ;
#82324 = DIRECTION ( 'NONE',  ( -0.7071067811865486830, 0.7071067811865464625, 0.000000000000000000 ) ) ;
#82325 = CARTESIAN_POINT ( 'NONE',  ( -12.00548008471251293, 28.92564299267929684, 4.000000000000000000 ) ) ;
#82326 = ORIENTED_EDGE ( 'NONE', *, *, #113823, .T. ) ;
#82327 = ADVANCED_FACE ( 'NONE', ( #105359 ), #61215, .F. ) ;
#82328 = CARTESIAN_POINT ( 'NONE',  ( -41.99451991528749062, 28.92564299267967343, 4.000000000000000000 ) ) ;
#82329 = CARTESIAN_POINT ( 'NONE',  ( 1.629999999999999893, 4.202752102959690472E-16, -4.330509084666861676E-16 ) ) ;
#82330 = ORIENTED_EDGE ( 'NONE', *, *, #49297, .F. ) ;
#82331 = ORIENTED_EDGE ( 'NONE', *, *, #118444, .T. ) ;
#82332 = EDGE_CURVE ( 'NONE', #26466, #29361, #29934, .T. ) ;
#82334 = EDGE_LOOP ( 'NONE', ( #35073, #5007, #98222, #33896, #106342, #26887 ) ) ;
#82333 = EDGE_CURVE ( 'NONE', #43201, #20344, #117636, .T. ) ;
#82335 = CARTESIAN_POINT ( 'NONE',  ( 45.93793019189810423, -6.110000000000001208, 1.637169565754158951 ) ) ;
#82336 = VERTEX_POINT ( 'NONE', #15467 ) ;
#82337 = VECTOR ( 'NONE', #126449, 999.9999999999998863 ) ;
#82338 = ADVANCED_FACE ( 'NONE', ( #127109 ), #76604, .T. ) ;
#82339 = CARTESIAN_POINT ( 'NONE',  ( 15.94163961620377279, -6.094999999999989093, 1.633150327867691765 ) ) ;
#82340 =( BOUNDED_SURFACE ( )  B_SPLINE_SURFACE ( 1, 2, ( 
 ( #119804, #20495, #128573, #87213, #73491, #66188, #88657, #77774, #34997, #11762, #89350, #100235, #90048, #55311, #24103, #46620, #35732, #121953, #32856, #44453, #155, #111829, #56045, #90801, #135037, #54598, #79239, #123446, #57463, #87920, #21942, #122680, #11035, #23365, #111071, #13188, #132890, #33576, #886, #45174, #68357, #2302, #133582, #121254, #100932, #143017, #78484, #43705, #112529, #98778, #79949, #124121, #22624, #66891, #34262, #134298, #67637, #12491, #110360, #56772, #1589, #24799, #69048, #101645, #99484, #10343, #132163, #77079, #45873, #16030, #94341, #48711, #104499, #82771, #60322, #102395, #39271, #37852, #116087, #16783, #36404, #103089, #5160, #4407, #113228, #69782, #49456, #126960, #138577, #135719, #105219, #48015, #80633, #27650, #83493, #81361, #92185, #25506, #136412, #37107, #137873, #114652, #92917, #59607, #93645, #14649, #71919, #5876, #127707, #125567, #124833, #3724, #26246, #71192, #15323, #50143, #28391, #13904, #38547, #61065, #58204, #47339, #113956, #82086, #58926, #126266, #70510, #3042, #103766, #137149, #26942, #115340, #91508, #64577, #18922, #40005, #19639, #61746, #140693, #105907, #97160, #17491, #542, #11395, #62453, #84898, #40693, #8710, #129109, #74768, #84222, #96449, #118948, #55676, #99876, #20333, #73332, #42136, #31250, #44837, #29788, #110716, #6573, #89027, #74031, #129832, #107360, #41387, #63882, #118216, #108044, #95770, #51579, #133244, #50849, #29094, #72649, #116809, #140018, #63189, #139317, #52963, #8026, #52266, #141425, #95045, #128417, #117499, #85595, #86346, #30535, #130565, #18174, #75466, #119636, #106618, #7313, #1939, #113594, #59268, #70157, #78863, #13552, #36070, #90427, #68699, #103421, #124483, #46243, #134674, #91173, #80295, #14993, #112890, #25157, #3392, #69407, #22988, #4067, #102021, #36752, #80994, #100606, #23748, #14290, #57829, #33923, #133937, #58577, #47683, #48353, #56426, #25885, #112199, #1251, #91845, #92541, #35371, #12843, #89710, #57123, #101300, #102745, #79612, #2684, #123796, #136070, #123071, #125202, #114316, #78141, #24452, #45533, #68017, #46986, #135391, #122314, #67260, #111458, #12142, #34624, #62104, #40364, #70844, #4788, #105563, #137515, #6225, #93985, #139681, #115702, #126603, #38906, #83130, #51224, #128764, #127329, #104122, #83874, #125927, #61421, #26601, #17833, #81731, #62825, #73678, #27294, #5536, #104871, #73006, #49813, #138946, #49091, #17157, #39648, #117853, #18540, #84568, #38207, #106264, #95418, #107005, #138220, #29439, #114994, #7683, #28034, #50501, #72300, #94687, #128078, #116465, #28757, #16405, #60704, #51940, #15672, #93282, #136783, #37494, #117156, #6937, #59960, #82419, #71547, #19987, #140355, #42505, #22129, #141058, #131637, #33073, #142519, #76553, #41764, #8373, #88129, #66383, #118596, #19294, #85978, #110555, #11232, #109870, #75136, #130937, #9079, #54797, #52622, #64961, #77282, #63551, #9836, #53338, #30158, #65706, #120735, #97555, #31606, #107715, #96122, #32324, #43206, #10534, #21442, #87418, #86711, #141808, #64233, #96811, #41047, #119301, #98976, #143213, #108394, #130213, #30904, #75829, #119994, #20706, #43915, #109151, #54106, #132376, #98294, #121453, #74408, #85246, #129471, #33768, #113422, #46072, #2501, #55509, #112723, #114147, #69239, #101124, #1771, #57663, #88860, #100432, #101847, #80832, #36581, #34453, #35196, #46815, #133085, #90249, #22820, #112030, #56257, #91000, #14107, #12681, #1084, #77972, #135224, #11971, #80133, #35914, #135906, #45367, #24982, #134495, #102585, #124312, #58401, #25707, #89541, #3232, #79440, #47522, #23571, #67094, #91683, #125023, #123637, #133771, #122889, #24292, #111278, #69983, #68537, #99696, #122153, #78677, #371, #44664, #67842, #56953, #13384, #84404, #128600, #28586, #137348, #49647, #71372, #116998, #114833, #127155, #139512, #81558, #72118, #115534, #92372, #127906, #39467, #16225, #93825, #26435, #73516, #50332, #105402, #72845, #83699, #6060, #5364, #60516, #126440, #125762, #29274, #38040, #94519, #17667, #82264, #70685, #15509, #93117, #59790, #48914, #138776, #27851, #38737, #61939, #103958, #27134, #136605, #95242, #103261, #37312, #106089, #138052, #6764, #14831, #116288, #59106, #51046, #104697, #82960, #16986, #48186, #4602, #61256, #40197, #3911, #96636, #97361, #119828, #51767, #64060, #85087, #30733, #118416, #20516, #76367, #74962, #63379, #95957, #64777, #74221, #142347, #108957, #54621, #19117, #87237, #108225, #21264, #9649, #53923, #87945, #107547, #120536, #141624, #65521, #85795, #129290, #32138, #98116, #8890, #8208, #41575, #42324, #29982, #98805, #86537, #143040, #140194, #7508, #43726, #106824, #40881, #140875, #52447, #130027, #18365, #53158, #132185, #119135, #43033, #32885, #131461, #109697, #19819, #130766, #10365, #117677, #31433, #75655, #62640, #3072, #47363, #90830, #56073, #111854, #133609, #35754, #33597, #45896, #58231, #180, #134323, #34284, #11061, #46645, #101668, #78505, #12516, #88682, #135746, #112556, #24126, #135061, #2328, #68378, #67664, #122708, #45198, #44477, #91530, #100258, #13217, #79974, #914, #132917, #77797, #11787, #121980, #111095, #57489, #90072, #100956, #124144, #22649, #89376, #55332, #13930, #21966, #99508, #24830, #56796, #69075, #77105, #35024, #121281, #113251, #23389, #1613, #79266, #110387, #66915, #123468, #102425, #66211, #15348, #16053, #38570, #113986, #126290, #3751, #92945, #37137, #82805, #138607, #137181, #125598, #14676, #126986, #136438, #61091, #27675, #116837, #81392, #5898, #26969, #83520, #71944, #116114, #6596, #26272, #39294, #60346, #127734, #4431, #48039, #94363, #16816, #71219, #70536, #103792, #104529, #92212, #17513, #5192, #61769, #58957, #69809, #105934, #25536, #103112, #59636, #114680, #48743, #80663, #115368, #50876, #37878, #105248, #95072, #50170, #28417, #82112 ),
 ( #49484, #72679, #93672, #36430, #124858, #137896, #109531, #95795, #142184, #19663, #97948, #107383, #106650, #53747, #86371, #129857, #29814, #63215, #63902, #7338, #120360, #108065, #76198, #73357, #29117, #21086, #128446, #62472, #18952, #117524, #8052, #40033, #85617, #65350, #40719, #31274, #10203, #42159, #119658, #84925, #51603, #131286, #54468, #18200, #140042, #129137, #139342, #84246, #9469, #118241, #30559, #52287, #42877, #74052, #8734, #96474, #140718, #52990, #41411, #74797, #108778, #20355, #118972, #97183, #141451, #130595, #75486, #64603, #87071, #31972, #89909, #89218, #11606, #66751, #66057, #24654, #77642, #134152, #101500, #121810, #21809, #110219, #33440, #6, #132751, #34848, #111680, #122535, #23961, #10897, #22486, #32708, #35585, #43561, #76939, #13051, #133439, #45736, #98648, #12347, #13755, #112396, #743, #45039, #100801, #132013, #44301, #1451, #123991, #79813, #110924, #78338, #79088, #121111, #68911, #87781, #55163, #57324, #34127, #123292, #142874, #56634, #99342, #2154, #23204, #67489, #68219, #88513, #55893, #46462, #113086, #100091, #90658, #134889, #60166, #135586, #4263, #25364, #114514, #58784, #104337, #16625, #15190, #3591, #36266, #5003, #14499, #82618, #49303, #138426, #102948, #27493, #48561, #105071, #93491, #137725, #28237, #47881, #60909, #81943, #5731, #26101, #69628, #115917, #38399, #92759, #92045, #125415, #126127, #113813, #39111, #26802, #83335, #80494, #91375, #127542, #47194, #124691, #81207, #136272, #70360, #102245, #136997, #72498, #36958, #126809, #116661, #71758, #50000, #59466, #103624, #94182, #58048, #37703, #71046, #115195, #2899, #15876, #31103, #139874, #52120, #73879, #119489, #117349, #129669, #142013, #84074, #74610, #118049, #94888, #130416, #41974, #18758, #96302, #28948, #76017, #52809, #107895, #75322, #86185, #8563, #7882, #63032, #128964, #128271, #86904, #40549, #97007, #20179, #84754, #73187, #18022, #95619, #62303, #51426, #141259, #30367, #41234, #64422, #106462, #29634, #108602, #9281, #53560, #97766, #140547, #107208, #85441, #7145, #131120, #118798, #42704, #31804, #19490, #63737, #17345, #61606, #105756, #6415, #50700, #139153, #39853, #45572, #32525, #143410, #54300, #57163, #65169, #98481, #34668, #110750, #67301, #120193, #33961, #35411, #133967, #22312, #66584, #122352, #10039, #21644, #23031, #1972, #101336, #99163, #99911, #111498, #142706, #11438, #87607, #33275, #120939, #12178, #78904, #77477, #65896, #43397, #56465, #76763, #1287, #100641, #46286, #110052, #89745, #55713, #23788, #123113, #68054, #90470, #10729, #112232, #578, #12883, #88340, #131835, #134717, #20904, #44876, #54999, #44116, #89059, #132581, #109357, #133278, #121643, #78176, #112925, #18394, #68740, #2730, #102785, #13586, #3428, #123831, #25925, #7531, #124523, #115031, #62663, #125959, #59988, #25191, #135426, #73541, #51796, #102056, #47025, #69448, #95978, #140220, #95269, #58613, #114355, #136104, #40219, #36105, #48382, #106853, #91214, #136818, #36785, #57871, #51072, #104159, #81034, #15026, #80334, #79652, #15704, #113632, #14326, #47719, #91882, #6791, #92581, #103459, #139537, #125235, #70191, #59302, #24488, #4098, #37531, #84431, #81766, #26634, #70878, #128625, #29298, #117703, #86561, #130793, #43061, #74248, #85817, #87261, #66237, #21986, #19845, #20547, #131483, #118443, #31458, #8231, #97388, #41605, #32163, #143063, #141651, #130057, #19143, #76398, #75679, #98144, #21291, #110410, #119848, #120560, #10390, #65549, #30007, #11086, #108982, #43755, #87971, #107570, #30755, #109720, #64804, #40903, #140906, #54645, #98833, #55359, #63404, #32910, #119159, #52474, #132215, #99535, #8916, #64081, #96660, #108249, #53188, #77131, #42350, #9679, #53947, #121305, #74986, #85110, #129318, #142368, #67688, #22671, #34307, #133630, #101694, #1636, #80682, #36452, #44506, #24851, #69096, #47381, #77819, #11809, #112581, #937, #13240, #100980, #3095, #122736, #78532, #45917, #90101, #58253, #135766, #134347, #111121, #90853, #132941, #68401, #33620, #113277, #88707, #69826, #124882, #23413, #12540, #111876, #79993, #56817, #2352, #56096, #24146, #57510, #45223, #46664, #35046, #91549, #79288, #123492, #135085, #35774, #102442, #25559, #124171, #100286, #13952, #122004, #114005, #66940, #14694, #89399, #58974, #203, #92966, #115383, #71237, #39318, #16073, #105267, #114697, #127003, #5916, #84269, #128462, #50900, #103806, #72700, #61791, #29137, #60369, #139363, #37159, #73380, #104549, #16837, #137914, #27700, #94379, #5216, #50193, #126305, #82130, #40051, #81412, #59652, #117542, #95093, #26992, #49507, #26293, #138627, #93688, #38591, #83542, #18219, #103128, #4454, #82827, #127751, #71963, #116137, #3769, #28439, #61116, #116857, #17533, #105953, #48053, #6612, #92231, #136458, #125615, #70550, #15367, #48762, #137202, #37898, #129156, #52308, #9489, #97207, #62494, #18971, #97968, #31987, #87793, #84946, #54481, #140736, #29831, #76215, #132033, #30579, #41430, #118262, #85639, #129878, #87089, #63917, #141471, #8751, #142203, #107404, #120378, #98662, #32724, #74816, #74075, #96494, #118994, #20376, #108088, #142893, #43576, #106670, #131305, #21104, #109545, #140062, #63236, #8067, #42893, #65366, #76955, #19679, #121126, #53008, #42176, #10223, #7359, #86389, #130619, #31292, #75504, #119674, #51622, #64616, #108800, #53765, #95815, #40738, #35601, #58066, #47209, #89232, #44320, #55907, #11626, #123306, #23224, #102261, #2912, #66071, #46482, #90673, #68929, #99355, #33458, #134165, #22504, #34864, #122547, #24668, #759, #100108, #67505, #111693, #79827, #13768, #12365, #132768, #112408, #10916, #89922, #55181, #134904, #110233, #91390, #135596, #45059, #34145, #133456, #101515, #78355, #23973, #77656, #45754, #68234, #36279, #80509, #113102, #66767, #124003, #21828, #23, #56649, #88528, #121825 ) ),
 .UNSPECIFIED., .F., .F., .F. ) 
 B_SPLINE_SURFACE_WITH_KNOTS ( ( 2, 2 ),
 ( 3, 2, 2, 2, 2, 2, 2, 2, 2, 2, 2, 2, 2, 2, 2, 2, 2, 2, 2, 2, 2, 2, 2, 2, 2, 2, 2, 2, 2, 2, 2, 2, 2, 2, 2, 2, 2, 2, 2, 2, 2, 2, 2, 2, 2, 2, 2, 2, 2, 2, 2, 2, 2, 2, 2, 2, 2, 2, 2, 2, 2, 2, 2, 2, 2, 2, 2, 2, 2, 2, 2, 2, 2, 2, 2, 2, 2, 2, 2, 2, 2, 2, 2, 2, 2, 2, 2, 2, 2, 2, 2, 2, 2, 2, 2, 2, 2, 2, 2, 2, 2, 2, 2, 2, 2, 2, 2, 2, 2, 2, 2, 2, 2, 2, 2, 2, 2, 2, 2, 2, 2, 2, 2, 2, 2, 2, 2, 2, 2, 2, 2, 2, 2, 2, 2, 2, 2, 2, 2, 2, 2, 2, 2, 2, 2, 2, 2, 2, 2, 2, 2, 2, 2, 2, 2, 2, 2, 2, 2, 2, 2, 2, 2, 2, 2, 2, 2, 2, 2, 2, 2, 2, 2, 2, 2, 2, 2, 2, 2, 2, 2, 2, 2, 2, 2, 2, 2, 2, 2, 2, 2, 2, 2, 2, 2, 2, 2, 2, 2, 2, 2, 2, 2, 2, 2, 2, 2, 2, 2, 2, 2, 2, 2, 2, 2, 2, 2, 2, 2, 2, 2, 2, 2, 2, 2, 2, 2, 2, 2, 2, 2, 2, 2, 2, 2, 2, 2, 2, 2, 2, 2, 2, 2, 2, 2, 2, 2, 2, 2, 2, 2, 2, 2, 2, 2, 2, 2, 2, 2, 2, 2, 2, 2, 2, 2, 2, 2, 2, 2, 2, 2, 2, 2, 2, 2, 2, 2, 2, 2, 2, 2, 2, 2, 2, 2, 2, 2, 2, 2, 2, 2, 2, 2, 2, 2, 2, 2, 2, 2, 2, 2, 2, 2, 2, 2, 2, 2, 2, 2, 2, 2, 2, 2, 2, 2, 2, 2, 2, 2, 2, 2, 2, 2, 2, 2, 2, 2, 2, 2, 2, 2, 2, 2, 2, 2, 2, 2, 2, 2, 2, 2, 2, 2, 2, 2, 2, 2, 2, 2, 2, 2, 3 ),
 ( 0.000000000000000000, 1.000000000000000000 ),
 ( 0.000000000000000000, 0.002777777777777777884, 0.005555555555555555768, 0.008333333333333333218, 0.01111111111111111154, 0.01388888888888888812, 0.01666666666666666644, 0.01944444444444444475, 0.02222222222222222307, 0.02500000000000000139, 0.02777777777777777624, 0.03055555555555555455, 0.03333333333333333287, 0.03611111111111110772, 0.03888888888888888951, 0.04166666666666666435, 0.04444444444444444614, 0.04722222222222222099, 0.05000000000000000278, 0.05277777777777777762, 0.05555555555555555247, 0.05833333333333333426, 0.06111111111111110911, 0.06388888888888888395, 0.06666666666666666574, 0.06944444444444444753, 0.07222222222222221544, 0.07499999999999999722, 0.07777777777777777901, 0.08055555555555556080, 0.08333333333333332871, 0.08611111111111111049, 0.08888888888888889228, 0.09166666666666666019, 0.09444444444444444198, 0.09722222222222222376, 0.1000000000000000056, 0.1027777777777777735, 0.1055555555555555552, 0.1083333333333333370, 0.1111111111111111049, 0.1138888888888888867, 0.1166666666666666685, 0.1194444444444444503, 0.1222222222222222182, 0.1250000000000000000, 0.1277777777777777679, 0.1305555555555555636, 0.1333333333333333315, 0.1361111111111110994, 0.1388888888888888951, 0.1416666666666666630, 0.1444444444444444309, 0.1472222222222222265, 0.1499999999999999944, 0.1527777777777777901, 0.1555555555555555580, 0.1583333333333333259, 0.1611111111111111216, 0.1638888888888888895, 0.1666666666666666574, 0.1694444444444444531, 0.1722222222222222210, 0.1749999999999999889, 0.1777777777777777846, 0.1805555555555555525, 0.1833333333333333204, 0.1861111111111111160, 0.1888888888888888840, 0.1916666666666666796, 0.1944444444444444475, 0.1972222222222222154, 0.2000000000000000111, 0.2027777777777777790, 0.2055555555555555469, 0.2083333333333333426, 0.2111111111111111105, 0.2138888888888888784, 0.2166666666666666741, 0.2194444444444444420, 0.2222222222222222099, 0.2250000000000000056, 0.2277777777777777735, 0.2305555555555555691, 0.2333333333333333370, 0.2361111111111111049, 0.2388888888888889006, 0.2416666666666666685, 0.2444444444444444364, 0.2472222222222222321, 0.2500000000000000000, 0.2527777777777777679, 0.2555555555555555358, 0.2583333333333333592, 0.2611111111111111271, 0.2638888888888888951, 0.2666666666666666630, 0.2694444444444444309, 0.2722222222222221988, 0.2750000000000000222, 0.2777777777777777901, 0.2805555555555555580, 0.2833333333333333259, 0.2861111111111110938, 0.2888888888888888618, 0.2916666666666666852, 0.2944444444444444531, 0.2972222222222222210, 0.2999999999999999889, 0.3027777777777777568, 0.3055555555555555802, 0.3083333333333333481, 0.3111111111111111160, 0.3138888888888888840, 0.3166666666666666519, 0.3194444444444444198, 0.3222222222222222432, 0.3250000000000000111, 0.3277777777777777790, 0.3305555555555555469, 0.3333333333333333148, 0.3361111111111111382, 0.3388888888888889062, 0.3416666666666666741, 0.3444444444444444420, 0.3472222222222222099, 0.3499999999999999778, 0.3527777777777778012, 0.3555555555555555691, 0.3583333333333333370, 0.3611111111111111049, 0.3638888888888888729, 0.3666666666666666408, 0.3694444444444444642, 0.3722222222222222321, 0.3750000000000000000, 0.3777777777777777679, 0.3805555555555555358, 0.3833333333333333592, 0.3861111111111111271, 0.3888888888888888951, 0.3916666666666666630, 0.3944444444444444309, 0.3972222222222221988, 0.4000000000000000222, 0.4027777777777777901, 0.4055555555555555580, 0.4083333333333333259, 0.4111111111111110938, 0.4138888888888888618, 0.4166666666666666852, 0.4194444444444444531, 0.4222222222222222210, 0.4249999999999999889, 0.4277777777777777568, 0.4305555555555555802, 0.4333333333333333481, 0.4361111111111111160, 0.4388888888888888840, 0.4416666666666666519, 0.4444444444444444198, 0.4472222222222222432, 0.4500000000000000111, 0.4527777777777777790, 0.4555555555555555469, 0.4583333333333333148, 0.4611111111111111382, 0.4638888888888889062, 0.4666666666666666741, 0.4694444444444444420, 0.4722222222222222099, 0.4749999999999999778, 0.4777777777777778012, 0.4805555555555555691, 0.4833333333333333370, 0.4861111111111111049, 0.4888888888888888729, 0.4916666666666666408, 0.4944444444444444642, 0.4972222222222222321, 0.5000000000000000000, 0.5027777777777777679, 0.5055555555555555358, 0.5083333333333333037, 0.5111111111111110716, 0.5138888888888888395, 0.5166666666666667185, 0.5194444444444444864, 0.5222222222222222543, 0.5250000000000000222, 0.5277777777777777901, 0.5305555555555555580, 0.5333333333333333259, 0.5361111111111110938, 0.5388888888888888618, 0.5416666666666666297, 0.5444444444444443976, 0.5472222222222222765, 0.5500000000000000444, 0.5527777777777778123, 0.5555555555555555802, 0.5583333333333333481, 0.5611111111111111160, 0.5638888888888888840, 0.5666666666666666519, 0.5694444444444444198, 0.5722222222222221877, 0.5749999999999999556, 0.5777777777777777235, 0.5805555555555556024, 0.5833333333333333703, 0.5861111111111111382, 0.5888888888888889062, 0.5916666666666666741, 0.5944444444444444420, 0.5972222222222222099, 0.5999999999999999778, 0.6027777777777777457, 0.6055555555555555136, 0.6083333333333332815, 0.6111111111111111605, 0.6138888888888889284, 0.6166666666666666963, 0.6194444444444444642, 0.6222222222222222321, 0.6250000000000000000, 0.6277777777777777679, 0.6305555555555555358, 0.6333333333333333037, 0.6361111111111110716, 0.6388888888888888395, 0.6416666666666667185, 0.6444444444444444864, 0.6472222222222222543, 0.6500000000000000222, 0.6527777777777777901, 0.6555555555555555580, 0.6583333333333333259, 0.6611111111111110938, 0.6638888888888888618, 0.6666666666666666297, 0.6694444444444443976, 0.6722222222222222765, 0.6750000000000000444, 0.6777777777777778123, 0.6805555555555555802, 0.6833333333333333481, 0.6861111111111111160, 0.6888888888888888840, 0.6916666666666666519, 0.6944444444444444198, 0.6972222222222221877, 0.6999999999999999556, 0.7027777777777777235, 0.7055555555555556024, 0.7083333333333333703, 0.7111111111111111382, 0.7138888888888889062, 0.7166666666666666741, 0.7194444444444444420, 0.7222222222222222099, 0.7249999999999999778, 0.7277777777777777457, 0.7305555555555555136, 0.7333333333333332815, 0.7361111111111111605, 0.7388888888888889284, 0.7416666666666666963, 0.7444444444444444642, 0.7472222222222222321, 0.7500000000000000000, 0.7527777777777777679, 0.7555555555555555358, 0.7583333333333333037, 0.7611111111111110716, 0.7638888888888888395, 0.7666666666666667185, 0.7694444444444444864, 0.7722222222222222543, 0.7750000000000000222, 0.7777777777777777901, 0.7805555555555555580, 0.7833333333333333259, 0.7861111111111110938, 0.7888888888888888618, 0.7916666666666666297, 0.7944444444444443976, 0.7972222222222222765, 0.8000000000000000444, 0.8027777777777778123, 0.8055555555555555802, 0.8083333333333333481, 0.8111111111111111160, 0.8138888888888888840, 0.8166666666666666519, 0.8194444444444444198, 0.8222222222222221877, 0.8249999999999999556, 0.8277777777777777235, 0.8305555555555556024, 0.8333333333333333703, 0.8361111111111111382, 0.8388888888888889062, 0.8416666666666666741, 0.8444444444444444420, 0.8472222222222222099, 0.8499999999999999778, 0.8527777777777777457, 0.8555555555555555136, 0.8583333333333332815, 0.8611111111111111605, 0.8638888888888889284, 0.8666666666666666963, 0.8694444444444444642, 0.8722222222222222321, 0.8750000000000000000, 0.8777777777777777679, 0.8805555555555555358, 0.8833333333333333037, 0.8861111111111110716, 0.8888888888888888395, 0.8916666666666667185, 0.8944444444444444864, 0.8972222222222222543, 0.9000000000000000222, 0.9027777777777777901, 0.9055555555555555580, 0.9083333333333333259, 0.9111111111111110938, 0.9138888888888888618, 0.9166666666666666297, 0.9194444444444443976, 0.9222222222222222765, 0.9250000000000000444, 0.9277777777777778123, 0.9305555555555555802, 0.9333333333333333481, 0.9361111111111111160, 0.9388888888888888840, 0.9416666666666666519, 0.9444444444444444198, 0.9472222222222221877, 0.9499999999999999556, 0.9527777777777777235, 0.9555555555555556024, 0.9583333333333333703, 0.9611111111111111382, 0.9638888888888889062, 0.9666666666666666741, 0.9694444444444444420, 0.9722222222222222099, 0.9749999999999999778 ),
 .UNSPECIFIED. ) 
 GEOMETRIC_REPRESENTATION_ITEM ( )  RATIONAL_B_SPLINE_SURFACE ( (
 ( 1.000000000000000000, 0.9659258262890683122, 1.000000000000000000, 0.9659258262890683122, 1.000000000000000000, 0.9659258262890683122, 1.000000000000000000, 0.9659258262890683122, 1.000000000000000000, 0.9659258262890683122, 1.000000000000000000, 0.9659258262890683122, 1.000000000000000000, 0.9659258262890683122, 1.000000000000000000, 0.9659258262890683122, 1.000000000000000000, 0.9659258262890683122, 1.000000000000000000, 0.9659258262890683122, 1.000000000000000000, 0.9659258262890683122, 1.000000000000000000, 0.9659258262890683122, 1.000000000000000000, 0.9659258262890683122, 1.000000000000000000, 0.9659258262890683122, 1.000000000000000000, 0.9659258262890683122, 1.000000000000000000, 0.9659258262890683122, 1.000000000000000000, 0.9659258262890683122, 1.000000000000000000, 0.9659258262890683122, 1.000000000000000000, 0.9659258262890683122, 1.000000000000000000, 0.9659258262890683122, 1.000000000000000000, 0.9659258262890683122, 1.000000000000000000, 0.9659258262890683122, 1.000000000000000000, 0.9659258262890683122, 1.000000000000000000, 0.9659258262890683122, 1.000000000000000000, 0.9659258262890683122, 1.000000000000000000, 0.9659258262890683122, 1.000000000000000000, 0.9659258262890683122, 1.000000000000000000, 0.9659258262890683122, 1.000000000000000000, 0.9659258262890683122, 1.000000000000000000, 0.9659258262890683122, 1.000000000000000000, 0.9659258262890683122, 1.000000000000000000, 0.9659258262890683122, 1.000000000000000000, 0.9659258262890683122, 1.000000000000000000, 0.9659258262890683122, 1.000000000000000000, 0.9659258262890683122, 1.000000000000000000, 0.9659258262890683122, 1.000000000000000000, 0.9659258262890683122, 1.000000000000000000, 0.9659258262890683122, 1.000000000000000000, 0.9659258262890683122, 1.000000000000000000, 0.9659258262890683122, 1.000000000000000000, 0.9659258262890683122, 1.000000000000000000, 0.9659258262890683122, 1.000000000000000000, 0.9659258262890683122, 1.000000000000000000, 0.9659258262890683122, 1.000000000000000000, 0.9659258262890683122, 1.000000000000000000, 0.9659258262890683122, 1.000000000000000000, 0.9659258262890683122, 1.000000000000000000, 0.9659258262890683122, 1.000000000000000000, 0.9659258262890683122, 1.000000000000000000, 0.9659258262890683122, 1.000000000000000000, 0.9659258262890683122, 1.000000000000000000, 0.9659258262890683122, 1.000000000000000000, 0.9659258262890683122, 1.000000000000000000, 0.9659258262890683122, 1.000000000000000000, 0.9659258262890683122, 1.000000000000000000, 0.9659258262890683122, 1.000000000000000000, 0.9659258262890683122, 1.000000000000000000, 0.9659258262890683122, 1.000000000000000000, 0.9659258262890683122, 1.000000000000000000, 0.9659258262890683122, 1.000000000000000000, 0.9659258262890683122, 1.000000000000000000, 0.9659258262890683122, 1.000000000000000000, 0.9659258262890683122, 1.000000000000000000, 0.9659258262890683122, 1.000000000000000000, 0.9659258262890683122, 1.000000000000000000, 0.9659258262890683122, 1.000000000000000000, 0.9659258262890683122, 1.000000000000000000, 0.9659258262890683122, 1.000000000000000000, 0.9659258262890683122, 1.000000000000000000, 0.9659258262890683122, 1.000000000000000000, 0.9659258262890683122, 1.000000000000000000, 0.9659258262890683122, 1.000000000000000000, 0.9659258262890683122, 1.000000000000000000, 0.9659258262890683122, 1.000000000000000000, 0.9659258262890683122, 1.000000000000000000, 0.9659258262890683122, 1.000000000000000000, 0.9659258262890683122, 1.000000000000000000, 0.9659258262890683122, 1.000000000000000000, 0.9659258262890683122, 1.000000000000000000, 0.9659258262890683122, 1.000000000000000000, 0.9659258262890683122, 1.000000000000000000, 0.9659258262890683122, 1.000000000000000000, 0.9659258262890683122, 1.000000000000000000, 0.9659258262890683122, 1.000000000000000000, 0.9659258262890683122, 1.000000000000000000, 0.9659258262890683122, 1.000000000000000000, 0.9659258262890683122, 1.000000000000000000, 0.9659258262890683122, 1.000000000000000000, 0.9659258262890683122, 1.000000000000000000, 0.9659258262890683122, 1.000000000000000000, 0.9659258262890683122, 1.000000000000000000, 0.9659258262890683122, 1.000000000000000000, 0.9659258262890683122, 1.000000000000000000, 0.9659258262890683122, 1.000000000000000000, 0.9659258262890683122, 1.000000000000000000, 0.9659258262890683122, 1.000000000000000000, 0.9659258262890683122, 1.000000000000000000, 0.9659258262890683122, 1.000000000000000000, 0.9659258262890683122, 1.000000000000000000, 0.9659258262890683122, 1.000000000000000000, 0.9659258262890683122, 1.000000000000000000, 0.9659258262890683122, 1.000000000000000000, 0.9659258262890683122, 1.000000000000000000, 0.9659258262890683122, 1.000000000000000000, 0.9659258262890683122, 1.000000000000000000, 0.9659258262890683122, 1.000000000000000000, 0.9659258262890683122, 1.000000000000000000, 0.9659258262890683122, 1.000000000000000000, 0.9659258262890683122, 1.000000000000000000, 0.9659258262890683122, 1.000000000000000000, 0.9659258262890683122, 1.000000000000000000, 0.9659258262890683122, 1.000000000000000000, 0.9659258262890683122, 1.000000000000000000, 0.9659258262890683122, 1.000000000000000000, 0.9659258262890683122, 1.000000000000000000, 0.9659258262890683122, 1.000000000000000000, 0.9659258262890683122, 1.000000000000000000, 0.9659258262890683122, 1.000000000000000000, 0.9659258262890683122, 1.000000000000000000, 0.9659258262890683122, 1.000000000000000000, 0.9659258262890683122, 1.000000000000000000, 0.9659258262890683122, 1.000000000000000000, 0.9659258262890683122, 1.000000000000000000, 0.9659258262890683122, 1.000000000000000000, 0.9659258262890683122, 1.000000000000000000, 0.9659258262890683122, 1.000000000000000000, 0.9659258262890683122, 1.000000000000000000, 0.9659258262890683122, 1.000000000000000000, 0.9659258262890683122, 1.000000000000000000, 0.9659258262890683122, 1.000000000000000000, 0.9659258262890683122, 1.000000000000000000, 0.9659258262890683122, 1.000000000000000000, 0.9659258262890683122, 1.000000000000000000, 0.9659258262890683122, 1.000000000000000000, 0.9659258262890683122, 1.000000000000000000, 0.9659258262890683122, 1.000000000000000000, 0.9659258262890683122, 1.000000000000000000, 0.9659258262890683122, 1.000000000000000000, 0.9659258262890683122, 1.000000000000000000, 0.9659258262890683122, 1.000000000000000000, 0.9659258262890683122, 1.000000000000000000, 0.9659258262890683122, 1.000000000000000000, 0.9659258262890683122, 1.000000000000000000, 0.9659258262890683122, 1.000000000000000000, 0.9659258262890683122, 1.000000000000000000, 0.9659258262890683122, 1.000000000000000000, 0.9659258262890683122, 1.000000000000000000, 0.9659258262890683122, 1.000000000000000000, 0.9659258262890683122, 1.000000000000000000, 0.9659258262890683122, 1.000000000000000000, 0.9659258262890683122, 1.000000000000000000, 0.9659258262890683122, 1.000000000000000000, 0.9659258262890683122, 1.000000000000000000, 0.9659258262890683122, 1.000000000000000000, 0.9659258262890683122, 1.000000000000000000, 0.9659258262890683122, 1.000000000000000000, 0.9659258262890683122, 1.000000000000000000, 0.9659258262890683122, 1.000000000000000000, 0.9659258262890683122, 1.000000000000000000, 0.9659258262890683122, 1.000000000000000000, 0.9659258262890683122, 1.000000000000000000, 0.9659258262890683122, 1.000000000000000000, 0.9659258262890683122, 1.000000000000000000, 0.9659258262890683122, 1.000000000000000000, 0.9659258262890683122, 1.000000000000000000, 0.9659258262890683122, 1.000000000000000000, 0.9659258262890683122, 1.000000000000000000, 0.9659258262890683122, 1.000000000000000000, 0.9659258262890683122, 1.000000000000000000, 0.9659258262890683122, 1.000000000000000000, 0.9659258262890683122, 1.000000000000000000, 0.9659258262890683122, 1.000000000000000000, 0.9659258262890683122, 1.000000000000000000, 0.9659258262890683122, 1.000000000000000000, 0.9659258262890683122, 1.000000000000000000, 0.9659258262890683122, 1.000000000000000000, 0.9659258262890683122, 1.000000000000000000, 0.9659258262890683122, 1.000000000000000000, 0.9659258262890683122, 1.000000000000000000, 0.9659258262890683122, 1.000000000000000000, 0.9659258262890683122, 1.000000000000000000, 0.9659258262890683122, 1.000000000000000000, 0.9659258262890683122, 1.000000000000000000, 0.9659258262890683122, 1.000000000000000000, 0.9659258262890683122, 1.000000000000000000, 0.9659258262890683122, 1.000000000000000000, 0.9659258262890683122, 1.000000000000000000, 0.9659258262890683122, 1.000000000000000000, 0.9659258262890683122, 1.000000000000000000, 0.9659258262890683122, 1.000000000000000000, 0.9659258262890683122, 1.000000000000000000, 0.9659258262890683122, 1.000000000000000000, 0.9659258262890683122, 1.000000000000000000, 0.9659258262890683122, 1.000000000000000000, 0.9659258262890683122, 1.000000000000000000, 0.9659258262890683122, 1.000000000000000000, 0.9659258262890683122, 1.000000000000000000, 0.9659258262890683122, 1.000000000000000000, 0.9659258262890683122, 1.000000000000000000, 0.9659258262890683122, 1.000000000000000000, 0.9659258262890683122, 1.000000000000000000, 0.9659258262890683122, 1.000000000000000000, 0.9659258262890683122, 1.000000000000000000, 0.9659258262890683122, 1.000000000000000000, 0.9659258262890683122, 1.000000000000000000, 0.9659258262890683122, 1.000000000000000000, 0.9659258262890683122, 1.000000000000000000, 0.9659258262890683122, 1.000000000000000000, 0.9659258262890683122, 1.000000000000000000, 0.9659258262890683122, 1.000000000000000000, 0.9659258262890683122, 1.000000000000000000, 0.9659258262890683122, 1.000000000000000000, 0.9659258262890683122, 1.000000000000000000, 0.9659258262890683122, 1.000000000000000000, 0.9659258262890683122, 1.000000000000000000, 0.9659258262890683122, 1.000000000000000000, 0.9659258262890683122, 1.000000000000000000, 0.9659258262890683122, 1.000000000000000000, 0.9659258262890683122, 1.000000000000000000, 0.9659258262890683122, 1.000000000000000000, 0.9659258262890683122, 1.000000000000000000, 0.9659258262890683122, 1.000000000000000000, 0.9659258262890683122, 1.000000000000000000, 0.9659258262890683122, 1.000000000000000000, 0.9659258262890683122, 1.000000000000000000, 0.9659258262890683122, 1.000000000000000000, 0.9659258262890683122, 1.000000000000000000, 0.9659258262890683122, 1.000000000000000000, 0.9659258262890683122, 1.000000000000000000, 0.9659258262890683122, 1.000000000000000000, 0.9659258262890683122, 1.000000000000000000, 0.9659258262890683122, 1.000000000000000000, 0.9659258262890683122, 1.000000000000000000, 0.9659258262890683122, 1.000000000000000000, 0.9659258262890683122, 1.000000000000000000, 0.9659258262890683122, 1.000000000000000000, 0.9659258262890683122, 1.000000000000000000, 0.9659258262890683122, 1.000000000000000000, 0.9659258262890683122, 1.000000000000000000, 0.9659258262890683122, 1.000000000000000000, 0.9659258262890683122, 1.000000000000000000, 0.9659258262890683122, 1.000000000000000000, 0.9659258262890683122, 1.000000000000000000, 0.9659258262890683122, 1.000000000000000000, 0.9659258262890683122, 1.000000000000000000, 0.9659258262890683122, 1.000000000000000000, 0.9659258262890683122, 1.000000000000000000, 0.9659258262890683122, 1.000000000000000000, 0.9659258262890683122, 1.000000000000000000, 0.9659258262890683122, 1.000000000000000000, 0.9659258262890683122, 1.000000000000000000, 0.9659258262890683122, 1.000000000000000000, 0.9659258262890683122, 1.000000000000000000, 0.9659258262890683122, 1.000000000000000000, 0.9659258262890683122, 1.000000000000000000, 0.9659258262890683122, 1.000000000000000000, 0.9659258262890683122, 1.000000000000000000, 0.9659258262890683122, 1.000000000000000000, 0.9659258262890683122, 1.000000000000000000, 0.9659258262890683122, 1.000000000000000000, 0.9659258262890683122, 1.000000000000000000, 0.9659258262890683122, 1.000000000000000000, 0.9659258262890683122, 1.000000000000000000, 0.9659258262890683122, 1.000000000000000000, 0.9659258262890683122, 1.000000000000000000, 0.9659258262890683122, 1.000000000000000000, 0.9659258262890683122, 1.000000000000000000, 0.9659258262890683122, 1.000000000000000000, 0.9659258262890683122, 1.000000000000000000, 0.9659258262890683122, 1.000000000000000000, 0.9659258262890683122, 1.000000000000000000, 0.9659258262890683122, 1.000000000000000000, 0.9659258262890683122, 1.000000000000000000, 0.9659258262890683122, 1.000000000000000000, 0.9659258262890683122, 1.000000000000000000, 0.9659258262890683122, 1.000000000000000000, 0.9659258262890683122, 1.000000000000000000, 0.9659258262890683122, 1.000000000000000000, 0.9659258262890683122, 1.000000000000000000, 0.9659258262890683122, 1.000000000000000000, 0.9659258262890683122, 1.000000000000000000, 0.9659258262890683122, 1.000000000000000000, 0.9659258262890683122, 1.000000000000000000, 0.9659258262890683122, 1.000000000000000000, 0.9659258262890683122, 1.000000000000000000, 0.9659258262890683122, 1.000000000000000000, 0.9659258262890683122, 1.000000000000000000, 0.9659258262890683122, 1.000000000000000000, 0.9659258262890683122, 1.000000000000000000, 0.9659258262890683122, 1.000000000000000000, 0.9659258262890683122, 1.000000000000000000, 0.9659258262890683122, 1.000000000000000000, 0.9659258262890683122, 1.000000000000000000, 0.9659258262890683122, 1.000000000000000000, 0.9659258262890683122, 1.000000000000000000, 0.9659258262890683122, 1.000000000000000000, 0.9659258262890683122, 1.000000000000000000, 0.9659258262890683122, 1.000000000000000000, 0.9659258262890683122, 1.000000000000000000, 0.9659258262890683122, 1.000000000000000000, 0.9659258262890683122, 1.000000000000000000, 0.9659258262890683122, 1.000000000000000000, 0.9659258262890683122, 1.000000000000000000, 0.9659258262890683122, 1.000000000000000000, 0.9659258262890683122, 1.000000000000000000, 0.9659258262890683122, 1.000000000000000000, 0.9659258262890683122, 1.000000000000000000, 0.9659258262890683122, 1.000000000000000000, 0.9659258262890683122, 1.000000000000000000, 0.9659258262890683122, 1.000000000000000000, 0.9659258262890683122, 1.000000000000000000, 0.9659258262890683122, 1.000000000000000000, 0.9659258262890683122, 1.000000000000000000, 0.9659258262890683122, 1.000000000000000000, 0.9659258262890683122, 1.000000000000000000, 0.9659258262890683122, 1.000000000000000000, 0.9659258262890683122, 1.000000000000000000, 0.9659258262890683122, 1.000000000000000000, 0.9659258262890683122, 1.000000000000000000, 0.9659258262890683122, 1.000000000000000000, 0.9659258262890683122, 1.000000000000000000, 0.9659258262890683122, 1.000000000000000000, 0.9659258262890683122, 1.000000000000000000, 0.9659258262890683122, 1.000000000000000000, 0.9659258262890683122, 1.000000000000000000, 0.9659258262890683122, 1.000000000000000000, 0.9659258262890683122, 1.000000000000000000, 0.9659258262890683122, 1.000000000000000000, 0.9659258262890683122, 1.000000000000000000, 0.9659258262890683122, 1.000000000000000000, 0.9659258262890683122, 1.000000000000000000, 0.9659258262890683122, 1.000000000000000000, 0.9659258262890683122, 1.000000000000000000, 0.9659258262890683122, 1.000000000000000000, 0.9659258262890683122, 1.000000000000000000, 0.9659258262890683122, 1.000000000000000000, 0.9659258262890683122, 1.000000000000000000, 0.9659258262890683122, 1.000000000000000000, 0.9659258262890683122, 1.000000000000000000, 0.9659258262890683122, 1.000000000000000000, 0.9659258262890683122, 1.000000000000000000, 0.9659258262890683122, 1.000000000000000000, 0.9659258262890683122, 1.000000000000000000, 0.9659258262890683122, 1.000000000000000000, 0.9659258262890683122, 1.000000000000000000, 0.9659258262890683122, 1.000000000000000000, 0.9659258262890683122, 1.000000000000000000, 0.9659258262890683122, 1.000000000000000000, 0.9659258262890683122, 1.000000000000000000, 0.9659258262890683122, 1.000000000000000000, 0.9659258262890683122, 1.000000000000000000),
 ( 1.000000000000000000, 0.9659258262890683122, 1.000000000000000000, 0.9659258262890683122, 1.000000000000000000, 0.9659258262890683122, 1.000000000000000000, 0.9659258262890683122, 1.000000000000000000, 0.9659258262890683122, 1.000000000000000000, 0.9659258262890683122, 1.000000000000000000, 0.9659258262890683122, 1.000000000000000000, 0.9659258262890683122, 1.000000000000000000, 0.9659258262890683122, 1.000000000000000000, 0.9659258262890683122, 1.000000000000000000, 0.9659258262890683122, 1.000000000000000000, 0.9659258262890683122, 1.000000000000000000, 0.9659258262890683122, 1.000000000000000000, 0.9659258262890683122, 1.000000000000000000, 0.9659258262890683122, 1.000000000000000000, 0.9659258262890683122, 1.000000000000000000, 0.9659258262890683122, 1.000000000000000000, 0.9659258262890683122, 1.000000000000000000, 0.9659258262890683122, 1.000000000000000000, 0.9659258262890683122, 1.000000000000000000, 0.9659258262890683122, 1.000000000000000000, 0.9659258262890683122, 1.000000000000000000, 0.9659258262890683122, 1.000000000000000000, 0.9659258262890683122, 1.000000000000000000, 0.9659258262890683122, 1.000000000000000000, 0.9659258262890683122, 1.000000000000000000, 0.9659258262890683122, 1.000000000000000000, 0.9659258262890683122, 1.000000000000000000, 0.9659258262890683122, 1.000000000000000000, 0.9659258262890683122, 1.000000000000000000, 0.9659258262890683122, 1.000000000000000000, 0.9659258262890683122, 1.000000000000000000, 0.9659258262890683122, 1.000000000000000000, 0.9659258262890683122, 1.000000000000000000, 0.9659258262890683122, 1.000000000000000000, 0.9659258262890683122, 1.000000000000000000, 0.9659258262890683122, 1.000000000000000000, 0.9659258262890683122, 1.000000000000000000, 0.9659258262890683122, 1.000000000000000000, 0.9659258262890683122, 1.000000000000000000, 0.9659258262890683122, 1.000000000000000000, 0.9659258262890683122, 1.000000000000000000, 0.9659258262890683122, 1.000000000000000000, 0.9659258262890683122, 1.000000000000000000, 0.9659258262890683122, 1.000000000000000000, 0.9659258262890683122, 1.000000000000000000, 0.9659258262890683122, 1.000000000000000000, 0.9659258262890683122, 1.000000000000000000, 0.9659258262890683122, 1.000000000000000000, 0.9659258262890683122, 1.000000000000000000, 0.9659258262890683122, 1.000000000000000000, 0.9659258262890683122, 1.000000000000000000, 0.9659258262890683122, 1.000000000000000000, 0.9659258262890683122, 1.000000000000000000, 0.9659258262890683122, 1.000000000000000000, 0.9659258262890683122, 1.000000000000000000, 0.9659258262890683122, 1.000000000000000000, 0.9659258262890683122, 1.000000000000000000, 0.9659258262890683122, 1.000000000000000000, 0.9659258262890683122, 1.000000000000000000, 0.9659258262890683122, 1.000000000000000000, 0.9659258262890683122, 1.000000000000000000, 0.9659258262890683122, 1.000000000000000000, 0.9659258262890683122, 1.000000000000000000, 0.9659258262890683122, 1.000000000000000000, 0.9659258262890683122, 1.000000000000000000, 0.9659258262890683122, 1.000000000000000000, 0.9659258262890683122, 1.000000000000000000, 0.9659258262890683122, 1.000000000000000000, 0.9659258262890683122, 1.000000000000000000, 0.9659258262890683122, 1.000000000000000000, 0.9659258262890683122, 1.000000000000000000, 0.9659258262890683122, 1.000000000000000000, 0.9659258262890683122, 1.000000000000000000, 0.9659258262890683122, 1.000000000000000000, 0.9659258262890683122, 1.000000000000000000, 0.9659258262890683122, 1.000000000000000000, 0.9659258262890683122, 1.000000000000000000, 0.9659258262890683122, 1.000000000000000000, 0.9659258262890683122, 1.000000000000000000, 0.9659258262890683122, 1.000000000000000000, 0.9659258262890683122, 1.000000000000000000, 0.9659258262890683122, 1.000000000000000000, 0.9659258262890683122, 1.000000000000000000, 0.9659258262890683122, 1.000000000000000000, 0.9659258262890683122, 1.000000000000000000, 0.9659258262890683122, 1.000000000000000000, 0.9659258262890683122, 1.000000000000000000, 0.9659258262890683122, 1.000000000000000000, 0.9659258262890683122, 1.000000000000000000, 0.9659258262890683122, 1.000000000000000000, 0.9659258262890683122, 1.000000000000000000, 0.9659258262890683122, 1.000000000000000000, 0.9659258262890683122, 1.000000000000000000, 0.9659258262890683122, 1.000000000000000000, 0.9659258262890683122, 1.000000000000000000, 0.9659258262890683122, 1.000000000000000000, 0.9659258262890683122, 1.000000000000000000, 0.9659258262890683122, 1.000000000000000000, 0.9659258262890683122, 1.000000000000000000, 0.9659258262890683122, 1.000000000000000000, 0.9659258262890683122, 1.000000000000000000, 0.9659258262890683122, 1.000000000000000000, 0.9659258262890683122, 1.000000000000000000, 0.9659258262890683122, 1.000000000000000000, 0.9659258262890683122, 1.000000000000000000, 0.9659258262890683122, 1.000000000000000000, 0.9659258262890683122, 1.000000000000000000, 0.9659258262890683122, 1.000000000000000000, 0.9659258262890683122, 1.000000000000000000, 0.9659258262890683122, 1.000000000000000000, 0.9659258262890683122, 1.000000000000000000, 0.9659258262890683122, 1.000000000000000000, 0.9659258262890683122, 1.000000000000000000, 0.9659258262890683122, 1.000000000000000000, 0.9659258262890683122, 1.000000000000000000, 0.9659258262890683122, 1.000000000000000000, 0.9659258262890683122, 1.000000000000000000, 0.9659258262890683122, 1.000000000000000000, 0.9659258262890683122, 1.000000000000000000, 0.9659258262890683122, 1.000000000000000000, 0.9659258262890683122, 1.000000000000000000, 0.9659258262890683122, 1.000000000000000000, 0.9659258262890683122, 1.000000000000000000, 0.9659258262890683122, 1.000000000000000000, 0.9659258262890683122, 1.000000000000000000, 0.9659258262890683122, 1.000000000000000000, 0.9659258262890683122, 1.000000000000000000, 0.9659258262890683122, 1.000000000000000000, 0.9659258262890683122, 1.000000000000000000, 0.9659258262890683122, 1.000000000000000000, 0.9659258262890683122, 1.000000000000000000, 0.9659258262890683122, 1.000000000000000000, 0.9659258262890683122, 1.000000000000000000, 0.9659258262890683122, 1.000000000000000000, 0.9659258262890683122, 1.000000000000000000, 0.9659258262890683122, 1.000000000000000000, 0.9659258262890683122, 1.000000000000000000, 0.9659258262890683122, 1.000000000000000000, 0.9659258262890683122, 1.000000000000000000, 0.9659258262890683122, 1.000000000000000000, 0.9659258262890683122, 1.000000000000000000, 0.9659258262890683122, 1.000000000000000000, 0.9659258262890683122, 1.000000000000000000, 0.9659258262890683122, 1.000000000000000000, 0.9659258262890683122, 1.000000000000000000, 0.9659258262890683122, 1.000000000000000000, 0.9659258262890683122, 1.000000000000000000, 0.9659258262890683122, 1.000000000000000000, 0.9659258262890683122, 1.000000000000000000, 0.9659258262890683122, 1.000000000000000000, 0.9659258262890683122, 1.000000000000000000, 0.9659258262890683122, 1.000000000000000000, 0.9659258262890683122, 1.000000000000000000, 0.9659258262890683122, 1.000000000000000000, 0.9659258262890683122, 1.000000000000000000, 0.9659258262890683122, 1.000000000000000000, 0.9659258262890683122, 1.000000000000000000, 0.9659258262890683122, 1.000000000000000000, 0.9659258262890683122, 1.000000000000000000, 0.9659258262890683122, 1.000000000000000000, 0.9659258262890683122, 1.000000000000000000, 0.9659258262890683122, 1.000000000000000000, 0.9659258262890683122, 1.000000000000000000, 0.9659258262890683122, 1.000000000000000000, 0.9659258262890683122, 1.000000000000000000, 0.9659258262890683122, 1.000000000000000000, 0.9659258262890683122, 1.000000000000000000, 0.9659258262890683122, 1.000000000000000000, 0.9659258262890683122, 1.000000000000000000, 0.9659258262890683122, 1.000000000000000000, 0.9659258262890683122, 1.000000000000000000, 0.9659258262890683122, 1.000000000000000000, 0.9659258262890683122, 1.000000000000000000, 0.9659258262890683122, 1.000000000000000000, 0.9659258262890683122, 1.000000000000000000, 0.9659258262890683122, 1.000000000000000000, 0.9659258262890683122, 1.000000000000000000, 0.9659258262890683122, 1.000000000000000000, 0.9659258262890683122, 1.000000000000000000, 0.9659258262890683122, 1.000000000000000000, 0.9659258262890683122, 1.000000000000000000, 0.9659258262890683122, 1.000000000000000000, 0.9659258262890683122, 1.000000000000000000, 0.9659258262890683122, 1.000000000000000000, 0.9659258262890683122, 1.000000000000000000, 0.9659258262890683122, 1.000000000000000000, 0.9659258262890683122, 1.000000000000000000, 0.9659258262890683122, 1.000000000000000000, 0.9659258262890683122, 1.000000000000000000, 0.9659258262890683122, 1.000000000000000000, 0.9659258262890683122, 1.000000000000000000, 0.9659258262890683122, 1.000000000000000000, 0.9659258262890683122, 1.000000000000000000, 0.9659258262890683122, 1.000000000000000000, 0.9659258262890683122, 1.000000000000000000, 0.9659258262890683122, 1.000000000000000000, 0.9659258262890683122, 1.000000000000000000, 0.9659258262890683122, 1.000000000000000000, 0.9659258262890683122, 1.000000000000000000, 0.9659258262890683122, 1.000000000000000000, 0.9659258262890683122, 1.000000000000000000, 0.9659258262890683122, 1.000000000000000000, 0.9659258262890683122, 1.000000000000000000, 0.9659258262890683122, 1.000000000000000000, 0.9659258262890683122, 1.000000000000000000, 0.9659258262890683122, 1.000000000000000000, 0.9659258262890683122, 1.000000000000000000, 0.9659258262890683122, 1.000000000000000000, 0.9659258262890683122, 1.000000000000000000, 0.9659258262890683122, 1.000000000000000000, 0.9659258262890683122, 1.000000000000000000, 0.9659258262890683122, 1.000000000000000000, 0.9659258262890683122, 1.000000000000000000, 0.9659258262890683122, 1.000000000000000000, 0.9659258262890683122, 1.000000000000000000, 0.9659258262890683122, 1.000000000000000000, 0.9659258262890683122, 1.000000000000000000, 0.9659258262890683122, 1.000000000000000000, 0.9659258262890683122, 1.000000000000000000, 0.9659258262890683122, 1.000000000000000000, 0.9659258262890683122, 1.000000000000000000, 0.9659258262890683122, 1.000000000000000000, 0.9659258262890683122, 1.000000000000000000, 0.9659258262890683122, 1.000000000000000000, 0.9659258262890683122, 1.000000000000000000, 0.9659258262890683122, 1.000000000000000000, 0.9659258262890683122, 1.000000000000000000, 0.9659258262890683122, 1.000000000000000000, 0.9659258262890683122, 1.000000000000000000, 0.9659258262890683122, 1.000000000000000000, 0.9659258262890683122, 1.000000000000000000, 0.9659258262890683122, 1.000000000000000000, 0.9659258262890683122, 1.000000000000000000, 0.9659258262890683122, 1.000000000000000000, 0.9659258262890683122, 1.000000000000000000, 0.9659258262890683122, 1.000000000000000000, 0.9659258262890683122, 1.000000000000000000, 0.9659258262890683122, 1.000000000000000000, 0.9659258262890683122, 1.000000000000000000, 0.9659258262890683122, 1.000000000000000000, 0.9659258262890683122, 1.000000000000000000, 0.9659258262890683122, 1.000000000000000000, 0.9659258262890683122, 1.000000000000000000, 0.9659258262890683122, 1.000000000000000000, 0.9659258262890683122, 1.000000000000000000, 0.9659258262890683122, 1.000000000000000000, 0.9659258262890683122, 1.000000000000000000, 0.9659258262890683122, 1.000000000000000000, 0.9659258262890683122, 1.000000000000000000, 0.9659258262890683122, 1.000000000000000000, 0.9659258262890683122, 1.000000000000000000, 0.9659258262890683122, 1.000000000000000000, 0.9659258262890683122, 1.000000000000000000, 0.9659258262890683122, 1.000000000000000000, 0.9659258262890683122, 1.000000000000000000, 0.9659258262890683122, 1.000000000000000000, 0.9659258262890683122, 1.000000000000000000, 0.9659258262890683122, 1.000000000000000000, 0.9659258262890683122, 1.000000000000000000, 0.9659258262890683122, 1.000000000000000000, 0.9659258262890683122, 1.000000000000000000, 0.9659258262890683122, 1.000000000000000000, 0.9659258262890683122, 1.000000000000000000, 0.9659258262890683122, 1.000000000000000000, 0.9659258262890683122, 1.000000000000000000, 0.9659258262890683122, 1.000000000000000000, 0.9659258262890683122, 1.000000000000000000, 0.9659258262890683122, 1.000000000000000000, 0.9659258262890683122, 1.000000000000000000, 0.9659258262890683122, 1.000000000000000000, 0.9659258262890683122, 1.000000000000000000, 0.9659258262890683122, 1.000000000000000000, 0.9659258262890683122, 1.000000000000000000, 0.9659258262890683122, 1.000000000000000000, 0.9659258262890683122, 1.000000000000000000, 0.9659258262890683122, 1.000000000000000000, 0.9659258262890683122, 1.000000000000000000, 0.9659258262890683122, 1.000000000000000000, 0.9659258262890683122, 1.000000000000000000, 0.9659258262890683122, 1.000000000000000000, 0.9659258262890683122, 1.000000000000000000, 0.9659258262890683122, 1.000000000000000000, 0.9659258262890683122, 1.000000000000000000, 0.9659258262890683122, 1.000000000000000000, 0.9659258262890683122, 1.000000000000000000, 0.9659258262890683122, 1.000000000000000000, 0.9659258262890683122, 1.000000000000000000, 0.9659258262890683122, 1.000000000000000000, 0.9659258262890683122, 1.000000000000000000, 0.9659258262890683122, 1.000000000000000000, 0.9659258262890683122, 1.000000000000000000, 0.9659258262890683122, 1.000000000000000000, 0.9659258262890683122, 1.000000000000000000, 0.9659258262890683122, 1.000000000000000000, 0.9659258262890683122, 1.000000000000000000, 0.9659258262890683122, 1.000000000000000000, 0.9659258262890683122, 1.000000000000000000, 0.9659258262890683122, 1.000000000000000000, 0.9659258262890683122, 1.000000000000000000, 0.9659258262890683122, 1.000000000000000000, 0.9659258262890683122, 1.000000000000000000, 0.9659258262890683122, 1.000000000000000000, 0.9659258262890683122, 1.000000000000000000, 0.9659258262890683122, 1.000000000000000000, 0.9659258262890683122, 1.000000000000000000, 0.9659258262890683122, 1.000000000000000000, 0.9659258262890683122, 1.000000000000000000, 0.9659258262890683122, 1.000000000000000000, 0.9659258262890683122, 1.000000000000000000, 0.9659258262890683122, 1.000000000000000000, 0.9659258262890683122, 1.000000000000000000, 0.9659258262890683122, 1.000000000000000000, 0.9659258262890683122, 1.000000000000000000, 0.9659258262890683122, 1.000000000000000000, 0.9659258262890683122, 1.000000000000000000, 0.9659258262890683122, 1.000000000000000000, 0.9659258262890683122, 1.000000000000000000, 0.9659258262890683122, 1.000000000000000000, 0.9659258262890683122, 1.000000000000000000, 0.9659258262890683122, 1.000000000000000000, 0.9659258262890683122, 1.000000000000000000, 0.9659258262890683122, 1.000000000000000000, 0.9659258262890683122, 1.000000000000000000, 0.9659258262890683122, 1.000000000000000000, 0.9659258262890683122, 1.000000000000000000, 0.9659258262890683122, 1.000000000000000000, 0.9659258262890683122, 1.000000000000000000, 0.9659258262890683122, 1.000000000000000000, 0.9659258262890683122, 1.000000000000000000, 0.9659258262890683122, 1.000000000000000000, 0.9659258262890683122, 1.000000000000000000, 0.9659258262890683122, 1.000000000000000000, 0.9659258262890683122, 1.000000000000000000, 0.9659258262890683122, 1.000000000000000000, 0.9659258262890683122, 1.000000000000000000, 0.9659258262890683122, 1.000000000000000000, 0.9659258262890683122, 1.000000000000000000, 0.9659258262890683122, 1.000000000000000000, 0.9659258262890683122, 1.000000000000000000, 0.9659258262890683122, 1.000000000000000000, 0.9659258262890683122, 1.000000000000000000, 0.9659258262890683122, 1.000000000000000000, 0.9659258262890683122, 1.000000000000000000, 0.9659258262890683122, 1.000000000000000000, 0.9659258262890683122, 1.000000000000000000, 0.9659258262890683122, 1.000000000000000000, 0.9659258262890683122, 1.000000000000000000, 0.9659258262890683122, 1.000000000000000000, 0.9659258262890683122, 1.000000000000000000, 0.9659258262890683122, 1.000000000000000000) ) ) 
 REPRESENTATION_ITEM ( '' )  SURFACE ( )  );
#82341 = CARTESIAN_POINT ( 'NONE',  ( -13.57767111518905523, 9.030084587337581681, -27.47540428435809901 ) ) ;
#82342 = EDGE_CURVE ( 'NONE', #18045, #108455, #140158, .T. ) ;
#82343 = ORIENTED_EDGE ( 'NONE', *, *, #75523, .T. ) ;
#82344 = CIRCLE ( 'NONE', #105395, 6.499999999999999112 ) ;
#82345 = LINE ( 'NONE', #2599, #105737 ) ;
#82346 = EDGE_LOOP ( 'NONE', ( #143041, #36769, #84022, #62907, #104107, #56762, #96475, #19105, #105174 ) ) ;
#82347 = FACE_OUTER_BOUND ( 'NONE', #17368, .T. ) ;
#82348 = CYLINDRICAL_SURFACE ( 'NONE', #63652, 4.375000000000001776 ) ;
#82349 = EDGE_CURVE ( 'NONE', #52857, #15815, #27090, .T. ) ;
#82351 = ORIENTED_EDGE ( 'NONE', *, *, #113199, .F. ) ;
#82350 = LINE ( 'NONE', #62742, #33235 ) ;
#82352 = ORIENTED_EDGE ( 'NONE', *, *, #79326, .F. ) ;
#82353 = CARTESIAN_POINT ( 'NONE',  ( 6.640000000000043201, -9.638965590364918103E-15, -40.00000000000000000 ) ) ;
#82354 = ORIENTED_EDGE ( 'NONE', *, *, #75822, .T. ) ;
#82355 = LINE ( 'NONE', #138875, #27265 ) ;
#82356 = ORIENTED_EDGE ( 'NONE', *, *, #91976, .T. ) ;
#82357 = VECTOR ( 'NONE', #12120, 1000.000000000000000 ) ;
#82358 = ORIENTED_EDGE ( 'NONE', *, *, #139893, .T. ) ;
#82359 = VERTEX_POINT ( 'NONE', #72075 ) ;
#82360 = ORIENTED_EDGE ( 'NONE', *, *, #15863, .T. ) ;
#82361 = CARTESIAN_POINT ( 'NONE',  ( 10.49999999999993960, 22.08746187583901843, 4.000000000000000000 ) ) ;
#82362 = CARTESIAN_POINT ( 'NONE',  ( -2.510786437626908008, -27.52281430457053446, 5.000000000000000000 ) ) ;
#82363 = CARTESIAN_POINT ( 'NONE',  ( 63.48921356237309510, -27.52281430457099631, 5.000000000000000000 ) ) ;
#82364 = LINE ( 'NONE', #117094, #127079 ) ;
#82365 = DIRECTION ( 'NONE',  ( 0.7071067811865486830, -0.7071067811865464625, -0.000000000000000000 ) ) ;
#82366 = ORIENTED_EDGE ( 'NONE', *, *, #139243, .F. ) ;
#82367 = FACE_OUTER_BOUND ( 'NONE', #15489, .T. ) ;
#82368 = VECTOR ( 'NONE', #35210, 1000.000000000000227 ) ;
#82369 = EDGE_CURVE ( 'NONE', #39996, #69883, #50293, .T. ) ;
#82370 = ADVANCED_FACE ( 'NONE', ( #106051 ), #61894, .F. ) ;
#82371 = CARTESIAN_POINT ( 'NONE',  ( 21.27040314143522437, -7.934999999999989839, 2.126176841940957907 ) ) ;
#82372 = CARTESIAN_POINT ( 'NONE',  ( 9.682526172861077640, 4.202752102959690472E-16, 0.000000000000000000 ) ) ;
#82373 = FACE_OUTER_BOUND ( 'NONE', #19969, .T. ) ;
#82374 = AXIS2_PLACEMENT_3D ( 'NONE', #26186, #24040, #58866 ) ;
#82375 = CARTESIAN_POINT ( 'NONE',  ( -8.999999999999941380, -0.8619312979532035568, -5.102805207349846661 ) ) ;
#82376 = ORIENTED_EDGE ( 'NONE', *, *, #50279, .T. ) ;
#82377 = ORIENTED_EDGE ( 'NONE', *, *, #126321, .F. ) ;
#82378 = ORIENTED_EDGE ( 'NONE', *, *, #33248, .T. ) ;
#82379 = CARTESIAN_POINT ( 'NONE',  ( -19.82816939922339827, 12.75929247661558286, 4.000000000000000000 ) ) ;
#82380 = LINE ( 'NONE', #59912, #7043 ) ;
#82381 = UNCERTAINTY_MEASURE_WITH_UNIT (LENGTH_MEASURE( 1.000000000000000082E-05 ), #24133, 'distance_accuracy_value', 'NONE');
#82382 = DIRECTION ( 'NONE',  ( -0.7071067811865486830, 0.7071067811865464625, 0.000000000000000000 ) ) ;
#82383 = VECTOR ( 'NONE', #33037, 1000.000000000000000 ) ;
#82384 = CARTESIAN_POINT ( 'NONE',  ( 13.96000000000000085, 9.521314400968980422E-16, 0.000000000000000000 ) ) ;
#82385 = EDGE_CURVE ( 'NONE', #59942, #32191, #137303, .T. ) ;
#82386 = LINE ( 'NONE', #79566, #59845 ) ;
#82387 = CARTESIAN_POINT ( 'NONE',  ( 71.07876352523146579, -7.482591942790327058E-16, 6.109999999999999432 ) ) ;
#82388 = CARTESIAN_POINT ( 'NONE',  ( -69.18398860626899705, 28.73617430169835529, 5.000000000000000000 ) ) ;
#82389 = DIRECTION ( 'NONE',  ( -0.3543493200069162685, -0.000000000000000000, -0.9351131265310288487 ) ) ;
#82390 = LINE ( 'NONE', #126568, #104565 ) ;
#82391 = LINE ( 'NONE', #59924, #88157 ) ;
#82392 = ORIENTED_EDGE ( 'NONE', *, *, #50804, .T. ) ;
#82393 = CARTESIAN_POINT ( 'NONE',  ( 19.93294383519271662, -3.241747265911685716, -35.72051902601952378 ) ) ;
#82394 = ORIENTED_EDGE ( 'NONE', *, *, #123462, .T. ) ;
#82395 = CARTESIAN_POINT ( 'NONE',  ( -33.29974487139158867, -27.71228299555229313, 4.000000000000000000 ) ) ;
#82397 = ORIENTED_EDGE ( 'NONE', *, *, #122335, .F. ) ;
#82396 = DIRECTION ( 'NONE',  ( -0.6830127018922181881, 0.6830127018922202975, -0.2588190451025214056 ) ) ;
#82398 = DIRECTION ( 'NONE',  ( 0.000000000000000000, 1.000000000000000000, 0.000000000000000000 ) ) ;
#82399 = LINE ( 'NONE', #40339, #128230 ) ;
#82400 = ORIENTED_EDGE ( 'NONE', *, *, #112375, .T. ) ;
#82401 = LINE ( 'NONE', #132156, #57750 ) ;
#82402 = ORIENTED_EDGE ( 'NONE', *, *, #103841, .F. ) ;
#82403 = DIRECTION ( 'NONE',  ( 0.000000000000000000, -1.000000000000000000, 0.000000000000000000 ) ) ;
#82404 = VERTEX_POINT ( 'NONE', #85042 ) ;
#82405 = DIRECTION ( 'NONE',  ( -0.6830127018922181881, 0.6830127018922202975, -0.2588190451025214056 ) ) ;
#82406 = CARTESIAN_POINT ( 'NONE',  ( 91.07919371712955581, 3.975000000000002753, -6.884901960086283523 ) ) ;
#82407 = DIRECTION ( 'NONE',  ( -0.000000000000000000, 0.000000000000000000, 1.000000000000000000 ) ) ;
#82408 = CARTESIAN_POINT ( 'NONE',  ( -21.18398860626899349, 28.73617430169802134, 5.000000000000000000 ) ) ;
#82409 = ORIENTED_EDGE ( 'NONE', *, *, #103610, .F. ) ;
#82410 = DIRECTION ( 'NONE',  ( -0.7071067811865486830, 0.7071067811865464625, 0.000000000000000000 ) ) ;
#82411 = ADVANCED_FACE ( 'NONE', ( #116248 ), #127862, .F. ) ;
#82412 = DIRECTION ( 'NONE',  ( -0.000000000000000000, 0.3543493200069153248, 0.9351131265310292928 ) ) ;
#82413 = CARTESIAN_POINT ( 'NONE',  ( 18.95833333333333570, -3.047499999999997211, -5.278424836066143655 ) ) ;
#82414 = CYLINDRICAL_SURFACE ( 'NONE', #116238, 1.000000000000000888 ) ;
#82415 = DIRECTION ( 'NONE',  ( -0.7071067811865486830, -0.7071067811865464625, 0.000000000000000000 ) ) ;
#82416 = EDGE_LOOP ( 'NONE', ( #84348, #123997, #61880, #119895 ) ) ;
#82417 = CARTESIAN_POINT ( 'NONE',  ( -15.72281430457048934, -21.72500000000000497, 5.000000000000000000 ) ) ;
#82418 = ORIENTED_EDGE ( 'NONE', *, *, #43528, .F. ) ;
#82419 = CARTESIAN_POINT ( 'NONE',  ( 80.35459685856474721, -1.637169565754161615, 6.110000000000000320 ) ) ;
#82420 = DIRECTION ( 'NONE',  ( 0.7071067811865487940, -0.7071067811865463515, 0.000000000000000000 ) ) ;
#82421 = CARTESIAN_POINT ( 'NONE',  ( 21.29974487139158512, -27.71228299555221142, 4.000000000000000000 ) ) ;
#82422 = PLANE ( 'NONE',  #3865 ) ;
#82423 = ORIENTED_EDGE ( 'NONE', *, *, #117436, .T. ) ;
#82424 = CARTESIAN_POINT ( 'NONE',  ( 30.29974487139158867, -27.71228299555227537, 4.000000000000000000 ) ) ;
#82425 = ADVANCED_FACE ( 'NONE', ( #39421 ), #51002, .F. ) ;
#82426 = DIRECTION ( 'NONE',  ( 0.7071067811865487940, 0.7071067811865463515, 0.000000000000000000 ) ) ;
#82427 = CARTESIAN_POINT ( 'NONE',  ( 118.3500270504628986, -5.819803920172573086, -5.819803920172573086 ) ) ;
#82428 = EDGE_CURVE ( 'NONE', #82613, #85586, #6718, .T. ) ;
#82429 = CARTESIAN_POINT ( 'NONE',  ( 5.755190629914537226, 4.202752102959690472E-16, 0.000000000000000000 ) ) ;
#82431 = ORIENTED_EDGE ( 'NONE', *, *, #73598, .F. ) ;
#82430 = DIRECTION ( 'NONE',  ( -1.000000000000000000, -1.224606353822377258E-16, -0.000000000000000000 ) ) ;
#82432 = CARTESIAN_POINT ( 'NONE',  ( 13.85416666666666963, 1.633150327867675555, 6.094999999999998863 ) ) ;
#82433 = CARTESIAN_POINT ( 'NONE',  ( 16.61159235450331906, 9.902892378096218942E-16, 0.000000000000000000 ) ) ;
#82434 = FACE_OUTER_BOUND ( 'NONE', #106485, .T. ) ;
#82435 = DIRECTION ( 'NONE',  ( -0.6830127018922181881, 0.6830127018922202975, -0.2588190451025214056 ) ) ;
#82436 = ADVANCED_FACE ( 'NONE', ( #84368 ), #73472, .T. ) ;
#82438 = ORIENTED_EDGE ( 'NONE', *, *, #132007, .T. ) ;
#82437 = ADVANCED_FACE ( 'NONE', ( #128557 ), #86490, .F. ) ;
#82439 = AXIS2_PLACEMENT_3D ( 'NONE', #84758, #106466, #63038 ) ;
#82440 = VERTEX_POINT ( 'NONE', #121230 ) ;
#82441 = ORIENTED_EDGE ( 'NONE', *, *, #28788, .F. ) ;
#82442 = CARTESIAN_POINT ( 'NONE',  ( 79.62543019189810423, 5.291415217122919401, 3.055000000000002824 ) ) ;
#82443 = ORIENTED_EDGE ( 'NONE', *, *, #4280, .F. ) ;
#82444 = VECTOR ( 'NONE', #66236, 1000.000000000000000 ) ;
#82445 = ADVANCED_FACE ( 'NONE', ( #64723 ), #108186, .F. ) ;
#82446 = DIRECTION ( 'NONE',  ( -0.000000000000000000, 0.3543493200069153248, 0.9351131265310292928 ) ) ;
#82447 = PLANE ( 'NONE',  #15505 ) ;
#82448 = CARTESIAN_POINT ( 'NONE',  ( -60.29974487139158867, -27.71228299555248142, 4.000000000000000000 ) ) ;
#82449 = LINE ( 'NONE', #41072, #131412 ) ;
#82450 = ORIENTED_EDGE ( 'NONE', *, *, #130588, .T. ) ;
#82451 = LINE ( 'NONE', #73704, #83867 ) ;
#82452 = LINE ( 'NONE', #139708, #141632 ) ;
#82453 = EDGE_CURVE ( 'NONE', #95640, #141807, #11016, .T. ) ;
#82454 = ORIENTED_EDGE ( 'NONE', *, *, #91636, .F. ) ;
#82455 = VECTOR ( 'NONE', #82242, 1000.000000000000000 ) ;
#82456 = LINE ( 'NONE', #62134, #72155 ) ;
#82457 = FACE_OUTER_BOUND ( 'NONE', #133335, .T. ) ;
#82458 = DIRECTION ( 'NONE',  ( 1.000000000000000000, 0.000000000000000000, 0.000000000000000000 ) ) ;
#82459 = EDGE_CURVE ( 'NONE', #81462, #34037, #39548, .T. ) ;
#82460 = EDGE_LOOP ( 'NONE', ( #67692, #119903, #103389, #93607 ) ) ;
#82461 = ORIENTED_EDGE ( 'NONE', *, *, #54220, .F. ) ;
#82462 = CARTESIAN_POINT ( 'NONE',  ( 24.72281430457042717, -21.72500000000000142, 5.000000000000000000 ) ) ;
#82463 = CARTESIAN_POINT ( 'NONE',  ( 15.48921356237309510, -27.52281430457066236, 5.000000000000000000 ) ) ;
#82464 = DIRECTION ( 'NONE',  ( -0.000000000000000000, -0.3543493200069152693, 0.9351131265310292928 ) ) ;
#82465 = LINE ( 'NONE', #27338, #49023 ) ;
#82466 = EDGE_CURVE ( 'NONE', #48968, #58791, #83642, .T. ) ;
#82467 = VECTOR ( 'NONE', #114004, 1000.000000000000000 ) ;
#82468 = CARTESIAN_POINT ( 'NONE',  ( 12.03892749862900402, 4.202752102959690472E-16, 0.000000000000000000 ) ) ;
#82469 = LINE ( 'NONE', #72346, #72069 ) ;
#82470 = ORIENTED_EDGE ( 'NONE', *, *, #82155, .T. ) ;
#82471 = AXIS2_PLACEMENT_3D ( 'NONE', #26108, #6421, #49311 ) ;
#82472 = ORIENTED_EDGE ( 'NONE', *, *, #123840, .F. ) ;
#82473 = ORIENTED_EDGE ( 'NONE', *, *, #88055, .F. ) ;
#82474 = VECTOR ( 'NONE', #60329, 1000.000000000000000 ) ;
#82475 = EDGE_LOOP ( 'NONE', ( #42450, #48569, #113855, #95369 ) ) ;
#82476 = ADVANCED_FACE ( 'NONE', ( #42989 ), #87189, .F. ) ;
#82477 = VECTOR ( 'NONE', #121070, 1000.000000000000227 ) ;
#82478 = CARTESIAN_POINT ( 'NONE',  ( 151.4000000000000057, -16.48000000000005016, 33.92499999999998295 ) ) ;
#82479 = ADVANCED_FACE ( 'NONE', ( #76322 ), #109648, .T. ) ;
#82480 = ORIENTED_EDGE ( 'NONE', *, *, #80849, .T. ) ;
#82481 =( NAMED_UNIT ( * ) SI_UNIT ( $, .STERADIAN. ) SOLID_ANGLE_UNIT ( ) );
#82482 = LINE ( 'NONE', #48413, #49538 ) ;
#82483 = EDGE_CURVE ( 'NONE', #22968, #54633, #131, .T. ) ;
#82484 = CARTESIAN_POINT ( 'NONE',  ( -10.82816939922345512, 0.7592924766157138627, 4.000000000000000000 ) ) ;
#82485 = CARTESIAN_POINT ( 'NONE',  ( 27.00000000000001066, -4.901040733167808305, -4.492499863940687455 ) ) ;
#82486 = EDGE_LOOP ( 'NONE', ( #87146, #7633, #66094, #122991, #128867 ) ) ;
#82487 = ADVANCED_FACE ( 'NONE', ( #99460 ), #132865, .F. ) ;
#82488 = FACE_OUTER_BOUND ( 'NONE', #104145, .T. ) ;
#82489 = CARTESIAN_POINT ( 'NONE',  ( 25.39999999999999858, 0.000000000000000000, 0.000000000000000000 ) ) ;
#82490 = ORIENTED_EDGE ( 'NONE', *, *, #96849, .T. ) ;
#82491 = CARTESIAN_POINT ( 'NONE',  ( -27.18398860626900060, 28.73617430169806042, 5.000000000000000000 ) ) ;
#82492 = VERTEX_POINT ( 'NONE', #32832 ) ;
#82493 = ORIENTED_EDGE ( 'NONE', *, *, #88710, .F. ) ;
#82494 = CARTESIAN_POINT ( 'NONE',  ( 23.29289321881329755, -3.740707523384243505, 5.000000000000000000 ) ) ;
#82495 = EDGE_LOOP ( 'NONE', ( #119478, #36675, #136624, #35457 ) ) ;
#82496 = VERTEX_POINT ( 'NONE', #77055 ) ;
#82497 = CARTESIAN_POINT ( 'NONE',  ( 71.31293019189810423, -1.637169565754159617, -6.110000000000001208 ) ) ;
#82498 = EDGE_LOOP ( 'NONE', ( #131767, #115038, #92622, #138685, #84775 ) ) ;
#82499 = CARTESIAN_POINT ( 'NONE',  ( 94.91666666666665719, -6.884901960086287076, -3.975000000000000977 ) ) ;
#82500 = LINE ( 'NONE', #7764, #114430 ) ;
#82501 = CARTESIAN_POINT ( 'NONE',  ( 112.5837635252314470, -6.110000000000001208, -3.741295971395164515E-16 ) ) ;
#82502 = DIRECTION ( 'NONE',  ( -0.7071067811865486830, -0.7071067811865464625, -0.000000000000000000 ) ) ;
#82503 = EDGE_CURVE ( 'NONE', #23195, #32169, #33555, .T. ) ;
#82504 = DIRECTION ( 'NONE',  ( 1.000000000000000000, 0.000000000000000000, 0.000000000000000000 ) ) ;
#82505 = LINE ( 'NONE', #22548, #62581 ) ;
#82506 = AXIS2_PLACEMENT_3D ( 'NONE', #47359, #14669, #77284 ) ;
#82507 = EDGE_CURVE ( 'NONE', #114653, #38444, #96591, .T. ) ;
#82508 = CARTESIAN_POINT ( 'NONE',  ( 34.42499999999998295, -21.72500000000000142, 5.000000000000000000 ) ) ;
#82509 = CARTESIAN_POINT ( 'NONE',  ( -74.99451991528749772, 28.92564299267990435, 4.000000000000000000 ) ) ;
#82510 = CARTESIAN_POINT ( 'NONE',  ( 19.82816939922339472, -8.240707523384191546, 4.000000000000000000 ) ) ;
#82511 = VERTEX_POINT ( 'NONE', #3019 ) ;
#82512 = PLANE ( 'NONE',  #61976 ) ;
#82513 = DIRECTION ( 'NONE',  ( 0.000000000000000000, 0.000000000000000000, -1.000000000000000000 ) ) ;
#82514 = ORIENTED_EDGE ( 'NONE', *, *, #78589, .T. ) ;
#82515 = VERTEX_POINT ( 'NONE', #47311 ) ;
#82516 = VECTOR ( 'NONE', #46037, 1000.000000000000227 ) ;
#82517 = DIRECTION ( 'NONE',  ( 0.000000000000000000, 0.000000000000000000, 1.000000000000000000 ) ) ;
#82518 = EDGE_LOOP ( 'NONE', ( #96729, #99568, #53286, #137792 ) ) ;
#82519 = DIRECTION ( 'NONE',  ( 0.7071067811865487940, 0.7071067811865463515, 0.000000000000000000 ) ) ;
#82520 = CARTESIAN_POINT ( 'NONE',  ( -32.67183060077623935, -9.740707523384180888, 4.000000000000000000 ) ) ;
#82521 = PLANE ( 'NONE',  #94917 ) ;
#82522 = CARTESIAN_POINT ( 'NONE',  ( 34.92500000000001847, -6.269999999999991580, -37.00000000000000000 ) ) ;
#82523 = ORIENTED_EDGE ( 'NONE', *, *, #41510, .T. ) ;
#82524 = DIRECTION ( 'NONE',  ( 0.7071067811865487940, -0.7071067811865463515, -0.000000000000000000 ) ) ;
#82525 = ORIENTED_EDGE ( 'NONE', *, *, #42449, .F. ) ;
#82526 = LINE ( 'NONE', #126716, #21358 ) ;
#82527 = MECHANICAL_DESIGN_GEOMETRIC_PRESENTATION_REPRESENTATION (  '', ( #89451 ), #117171 ) ;
#82528 = EDGE_CURVE ( 'NONE', #1213, #97544, #46255, .T. ) ;
#82529 = CARTESIAN_POINT ( 'NONE',  ( 24.27540314143521982, -2.126176841940958351, -7.934999999999989839 ) ) ;
#82530 = CARTESIAN_POINT ( 'NONE',  ( 34.92499999999997584, -15.28150956279557526, 4.759050581649322709 ) ) ;
#82531 = CARTESIAN_POINT ( 'NONE',  ( -2.292893218813438772, -6.740707523384212863, 5.000000000000000000 ) ) ;
#82532 = MECHANICAL_DESIGN_GEOMETRIC_PRESENTATION_REPRESENTATION (  '', ( #33909 ), #6110 ) ;
#82533 = CARTESIAN_POINT ( 'NONE',  ( 26.99451991528749417, 28.92564299267956685, 4.000000000000000000 ) ) ;
#82534 = ORIENTED_EDGE ( 'NONE', *, *, #89505, .T. ) ;
#82535 = ORIENTED_EDGE ( 'NONE', *, *, #31902, .F. ) ;
#82536 = ORIENTED_EDGE ( 'NONE', *, *, #142207, .F. ) ;
#82537 = DIRECTION ( 'NONE',  ( -0.000000000000000000, -0.000000000000000000, -1.000000000000000000 ) ) ;
#82538 = DIRECTION ( 'NONE',  ( 0.7071067811865487940, 0.7071067811865463515, -0.000000000000000000 ) ) ;
#82539 = PLANE ( 'NONE',  #10318 ) ;
#82540 = DIRECTION ( 'NONE',  ( -0.7071067811865486830, -0.7071067811865464625, 0.000000000000000000 ) ) ;
#82541 = DIRECTION ( 'NONE',  ( -0.7071067811865487940, 0.7071067811865463515, -0.000000000000000000 ) ) ;
#82542 = LINE ( 'NONE', #5661, #138371 ) ;
#82543 = FACE_OUTER_BOUND ( 'NONE', #52718, .T. ) ;
#82544 = VECTOR ( 'NONE', #61470, 1000.000000000000000 ) ;
#82545 = CARTESIAN_POINT ( 'NONE',  ( 21.18398860626899349, 28.73617430169802134, 5.000000000000000000 ) ) ;
#82546 = DIRECTION ( 'NONE',  ( -0.7071067811865486830, -0.7071067811865464625, 0.000000000000000000 ) ) ;
#82547 = ORIENTED_EDGE ( 'NONE', *, *, #11625, .T. ) ;
#82548 = CARTESIAN_POINT ( 'NONE',  ( 73.18749999999997158, -5.819803920172573974, 5.819803920172573086 ) ) ;
#82549 = DIRECTION ( 'NONE',  ( 0.6830127018922180770, -0.6830127018922204085, -0.2588190451025213501 ) ) ;
#82550 = ORIENTED_EDGE ( 'NONE', *, *, #91892, .T. ) ;
#82551 = CARTESIAN_POINT ( 'NONE',  ( -5.200031220168336077, 8.259292476615634371, 16.85664084051842337 ) ) ;
#82553 = VERTEX_POINT ( 'NONE', #13875 ) ;
#82552 = CARTESIAN_POINT ( 'NONE',  ( 57.34909574878783189, -49.32595796886460704, -36.54674188582485783 ) ) ;
#82554 = TOROIDAL_SURFACE ( 'NONE', #101059, 9.000000000000001776, 3.000000000000000000 ) ;
#82555 = EDGE_LOOP ( 'NONE', ( #10171, #11966, #38858, #129899, #48918 ) ) ;
#82556 = LINE ( 'NONE', #17966, #44580 ) ;
#82557 = CARTESIAN_POINT ( 'NONE',  ( -23.99999999999981881, 20.58746187583902909, 4.000000000000000000 ) ) ;
#82558 = LINE ( 'NONE', #126747, #127043 ) ;
#82559 = ORIENTED_EDGE ( 'NONE', *, *, #41042, .F. ) ;
#82560 = CARTESIAN_POINT ( 'NONE',  ( 0.000000000000000000, 0.000000000000000000, 5.000000000000000000 ) ) ;
#82561 = ORIENTED_EDGE ( 'NONE', *, *, #53020, .F. ) ;
#82562 = AXIS2_PLACEMENT_3D ( 'NONE', #84262, #127748, #50188 ) ;
#82563 = AXIS2_PLACEMENT_3D ( 'NONE', #67690, #12543, #120563 ) ;
#82564 = DIRECTION ( 'NONE',  ( -1.000000000000000000, -1.224606353822377258E-16, -0.000000000000000000 ) ) ;
#82565 = CARTESIAN_POINT ( 'NONE',  ( 107.7500000000000000, -9.735942053221458872E-16, 7.950000000000000178 ) ) ;
#82566 = CARTESIAN_POINT ( 'NONE',  ( 122.7250270504628844, 5.819803920172573086, -5.819803920172572198 ) ) ;
#82567 = DIRECTION ( 'NONE',  ( 0.6830127018922180770, -0.6830127018922204085, -0.2588190451025213501 ) ) ;
#82568 = LINE ( 'NONE', #126760, #108714 ) ;
#82569 = DIRECTION ( 'NONE',  ( -0.000000000000000000, 0.000000000000000000, 1.000000000000000000 ) ) ;
#82570 = CARTESIAN_POINT ( 'NONE',  ( 6.229065384000522343, 2.500000000000001776, 3.061616997868385113E-16 ) ) ;
#82571 = CARTESIAN_POINT ( 'NONE',  ( 13.49999999999991118, -7.912538124160675146, 4.000000000000000000 ) ) ;
#82572 = CARTESIAN_POINT ( 'NONE',  ( 33.52040314143522437, 7.934999999999989839, -2.126176841940961904 ) ) ;
#82573 = CARTESIAN_POINT ( 'NONE',  ( 8.874569808101886892, 6.871911579029510442, -3.967499999999998916 ) ) ;
#82574 = DIRECTION ( 'NONE',  ( -0.000000000000000000, -0.3543493200069152693, 0.9351131265310292928 ) ) ;
#82575 = LINE ( 'NONE', #58740, #127701 ) ;
#82576 = LINE ( 'NONE', #22273, #128817 ) ;
#82577 = ORIENTED_EDGE ( 'NONE', *, *, #16898, .F. ) ;
#82578 = ORIENTED_EDGE ( 'NONE', *, *, #41255, .F. ) ;
#82579 = CARTESIAN_POINT ( 'NONE',  ( 84.85416666666668561, -2.130196079827425315, -7.950000000000001066 ) ) ;
#82581 = ORIENTED_EDGE ( 'NONE', *, *, #89872, .T. ) ;
#82580 = DIRECTION ( 'NONE',  ( -0.000000000000000000, 0.000000000000000000, 1.000000000000000000 ) ) ;
#82582 = ORIENTED_EDGE ( 'NONE', *, *, #65776, .F. ) ;
#82583 = EDGE_CURVE ( 'NONE', #79492, #55124, #67610, .T. ) ;
#82584 = CARTESIAN_POINT ( 'NONE',  ( -34.17183060077623225, 18.75929247661552779, 4.000000000000000000 ) ) ;
#82585 = LINE ( 'NONE', #27461, #126624 ) ;
#82586 = ORIENTED_EDGE ( 'NONE', *, *, #35406, .T. ) ;
#82587 = LINE ( 'NONE', #115891, #97221 ) ;
#82588 = CARTESIAN_POINT ( 'NONE',  ( -26.29289321881326913, 5.259292476615661016, 5.000000000000000000 ) ) ;
#82589 = DIRECTION ( 'NONE',  ( -0.7071067811865487940, 0.7071067811865463515, 0.000000000000000000 ) ) ;
#82590 = CARTESIAN_POINT ( 'NONE',  ( 126.8620668341126674, 3.744568938377744960, 5.426115537218553442 ) ) ;
#82591 = EDGE_CURVE ( 'NONE', #76029, #50763, #3699, .T. ) ;
#82592 = EDGE_CURVE ( 'NONE', #143132, #7428, #69024, .T. ) ;
#82593 = CARTESIAN_POINT ( 'NONE',  ( 16.19018167574437683, -18.74070752338409562, 7.910009926591468954 ) ) ;
#82594 = PLANE ( 'NONE',  #38151 ) ;
#82595 = CARTESIAN_POINT ( 'NONE',  ( -39.18398860626899705, 28.73617430169814568, 5.000000000000000000 ) ) ;
#82596 = LINE ( 'NONE', #4245, #112382 ) ;
#82597 = DIRECTION ( 'NONE',  ( -0.6830127018922181881, 0.6830127018922202975, -0.2588190451025214056 ) ) ;
#82598 = DIRECTION ( 'NONE',  ( -0.6830127018922181881, 0.6830127018922202975, -0.2588190451025214056 ) ) ;
#82599 = DIRECTION ( 'NONE',  ( -0.7071067811865487940, 0.7071067811865463515, 0.000000000000000000 ) ) ;
#82600 = FACE_OUTER_BOUND ( 'NONE', #63530, .T. ) ;
#82601 = EDGE_CURVE ( 'NONE', #99505, #4103, #91483, .T. ) ;
#82602 = EDGE_CURVE ( 'NONE', #110390, #16024, #47993, .T. ) ;
#82603 = ORIENTED_EDGE ( 'NONE', *, *, #65379, .T. ) ;
#82604 = EDGE_LOOP ( 'NONE', ( #116906, #32920, #46558, #42073 ) ) ;
#82605 = CARTESIAN_POINT ( 'NONE',  ( 112.2920968585647756, -5.291415217122921177, 3.054999999999999272 ) ) ;
#82606 = AXIS2_PLACEMENT_3D ( 'NONE', #126035, #14404, #102853 ) ;
#82607 = VERTEX_POINT ( 'NONE', #45154 ) ;
#82608 = EDGE_CURVE ( 'NONE', #56006, #141462, #113930, .T. ) ;
#82609 = DIRECTION ( 'NONE',  ( 0.6830127018922181881, 0.6830127018922202975, -0.2588190451025214056 ) ) ;
#82610 = AXIS2_PLACEMENT_3D ( 'NONE', #27669, #106641, #50164 ) ;
#82611 = ADVANCED_FACE ( 'NONE', ( #79212 ), #22604, .T. ) ;
#82612 = DIRECTION ( 'NONE',  ( 0.000000000000000000, -0.000000000000000000, 1.000000000000000000 ) ) ;
#82613 = VERTEX_POINT ( 'NONE', #2274 ) ;
#82614 = DIRECTION ( 'NONE',  ( 0.6830127018922180770, -0.6830127018922204085, -0.2588190451025213501 ) ) ;
#82616 =( BOUNDED_CURVE ( )  B_SPLINE_CURVE ( 2, ( #55967, #100166, #815, #111752, #56698, #100861, #61504, #6306, #126021, #116557, #28126, #83222, #126697 ),
 .UNSPECIFIED., .F., .F. ) 
 B_SPLINE_CURVE_WITH_KNOTS ( ( 3, 2, 2, 2, 2, 2, 3 ),
 ( 0.8833333333333333037, 0.8861111111111110716, 0.8888888888888888395, 0.8916666666666667185, 0.8944444444444444864, 0.8972222222222222543, 0.9000000000000000222 ),
 .UNSPECIFIED. ) 
 CURVE ( )  GEOMETRIC_REPRESENTATION_ITEM ( )  RATIONAL_B_SPLINE_CURVE ( ( 1.000000000000000000, 0.9659258262890683122, 1.000000000000000000, 0.9659258262890683122, 1.000000000000000000, 0.9659258262890683122, 1.000000000000000000, 0.9659258262890683122, 1.000000000000000000, 0.9659258262890683122, 1.000000000000000000, 0.9659258262890683122, 1.000000000000000000 ) ) 
 REPRESENTATION_ITEM ( '' )  );
#82615 = DIRECTION ( 'NONE',  ( -0.6830127018922181881, 0.6830127018922202975, -0.2588190451025214056 ) ) ;
#82617 = EDGE_CURVE ( 'NONE', #34870, #96749, #81362, .T. ) ;
#82618 = CARTESIAN_POINT ( 'NONE',  ( 107.3912635252314516, -4.472830434245839371, -4.472830434245839371 ) ) ;
#82619 = VERTEX_POINT ( 'NONE', #122656 ) ;
#82620 = DIRECTION ( 'NONE',  ( -0.000000000000000000, 0.000000000000000000, 1.000000000000000000 ) ) ;
#82621 = ORIENTED_EDGE ( 'NONE', *, *, #128641, .F. ) ;
#82622 = FACE_OUTER_BOUND ( 'NONE', #41689, .T. ) ;
#82623 = VECTOR ( 'NONE', #121945, 1000.000000000000000 ) ;
#82624 = DIRECTION ( 'NONE',  ( -0.000000000000000000, 0.3543493200069153248, 0.9351131265310292928 ) ) ;
#82625 = DIRECTION ( 'NONE',  ( 0.7071067811865487940, 0.7071067811865463515, -0.000000000000000000 ) ) ;
#82626 = EDGE_CURVE ( 'NONE', #71467, #77426, #25479, .T. ) ;
#82627 = ORIENTED_EDGE ( 'NONE', *, *, #63844, .F. ) ;
#82628 = ORIENTED_EDGE ( 'NONE', *, *, #65767, .T. ) ;
#82629 = VECTOR ( 'NONE', #77667, 1000.000000000000000 ) ;
#82630 = VERTEX_POINT ( 'NONE', #111800 ) ;
#82631 = DIRECTION ( 'NONE',  ( -1.000000000000000000, -0.000000000000000000, -0.000000000000000000 ) ) ;
#82632 = DIRECTION ( 'NONE',  ( 0.000000000000000000, -1.000000000000000000, 0.000000000000000000 ) ) ;
#82633 = CARTESIAN_POINT ( 'NONE',  ( 7.504569808101886785, 6.871911579029510442, -3.967499999999998916 ) ) ;
#82634 = ADVANCED_FACE ( 'NONE', ( #23337 ), #862, .F. ) ;
#82635 = CARTESIAN_POINT ( 'NONE',  ( 29.99999999999979750, -18.03360074219754949, 5.000000000000000000 ) ) ;
#82636 = VECTOR ( 'NONE', #79146, 1000.000000000000000 ) ;
#82637 =( NAMED_UNIT ( * ) SI_UNIT ( $, .STERADIAN. ) SOLID_ANGLE_UNIT ( ) );
#82638 = CARTESIAN_POINT ( 'NONE',  ( -65.99451991528749772, 28.92564299267984396, 4.000000000000000000 ) ) ;
#82639 = ORIENTED_EDGE ( 'NONE', *, *, #135622, .F. ) ;
#82640 = AXIS2_PLACEMENT_3D ( 'NONE', #125065, #12725, #34497 ) ;
#82641 = ORIENTED_EDGE ( 'NONE', *, *, #89408, .F. ) ;
#82642 = FACE_OUTER_BOUND ( 'NONE', #128152, .T. ) ;
#82643 = EDGE_LOOP ( 'NONE', ( #11693, #57203, #53126 ) ) ;
#82644 = ORIENTED_EDGE ( 'NONE', *, *, #142827, .T. ) ;
#82645 = EDGE_CURVE ( 'NONE', #69514, #135832, #45851, .T. ) ;
#82646 = DIRECTION ( 'NONE',  ( -0.7071067811865486830, -0.7071067811865464625, -0.000000000000000000 ) ) ;
#82647 = ADVANCED_FACE ( 'NONE', ( #77754 ), #57439, .F. ) ;
#82648 = LINE ( 'NONE', #116689, #5108 ) ;
#82649 = CARTESIAN_POINT ( 'NONE',  ( 21.71715331601274102, -2.164967620583693630, 5.000000000000000000 ) ) ;
#82650 = ORIENTED_EDGE ( 'NONE', *, *, #120816, .F. ) ;
#82651 = CARTESIAN_POINT ( 'NONE',  ( 5.541666666666666963, 3.047499999999993214, -5.278424836066146320 ) ) ;
#82652 = EDGE_CURVE ( 'NONE', #26845, #11127, #34242, .T. ) ;
#82653 = CARTESIAN_POINT ( 'NONE',  ( 12.18398860626900060, 28.73617430169795739, 5.000000000000000000 ) ) ;
#82654 = LINE ( 'NONE', #105104, #138644 ) ;
#82655 = EDGE_CURVE ( 'NONE', #91841, #26097, #34972, .T. ) ;
#82656 = LINE ( 'NONE', #39887, #58294 ) ;
#82657 = VERTEX_POINT ( 'NONE', #90778 ) ;
#82658 = EDGE_CURVE ( 'NONE', #44279, #23445, #135007, .T. ) ;
#82659 = CARTESIAN_POINT ( 'NONE',  ( -66.18398860626901126, 28.73617430169833753, 5.000000000000000000 ) ) ;
#82661 = FACE_BOUND ( 'NONE', #113941, .T. ) ;
#82660 = AXIS2_PLACEMENT_3D ( 'NONE', #29653, #41994, #50719 ) ;
#82662 = ORIENTED_EDGE ( 'NONE', *, *, #23589, .F. ) ;
#82663 = PLANE ( 'NONE',  #143061 ) ;
#82664 = LINE ( 'NONE', #50743, #29546 ) ;
#82665 = LINE ( 'NONE', #5774, #139478 ) ;
#82666 = ORIENTED_EDGE ( 'NONE', *, *, #126023, .F. ) ;
#82667 = DIRECTION ( 'NONE',  ( 0.7071067811865487940, -0.7071067811865463515, 0.000000000000000000 ) ) ;
#82668 = ORIENTED_EDGE ( 'NONE', *, *, #54228, .T. ) ;
#82669 = VERTEX_POINT ( 'NONE', #84198 ) ;
#82670 = VECTOR ( 'NONE', #130807, 1000.000000000000000 ) ;
#82671 = VERTEX_POINT ( 'NONE', #105193 ) ;
#82672 = VECTOR ( 'NONE', #88531, 1000.000000000000227 ) ;
#82673 = AXIS2_PLACEMENT_3D ( 'NONE', #36074, #102026, #78868 ) ;
#82674 = CARTESIAN_POINT ( 'NONE',  ( 40.16209685856478018, -5.291415217122919401, 3.054999999999997939 ) ) ;
#82675 = ORIENTED_EDGE ( 'NONE', *, *, #57015, .T. ) ;
#82676 = CARTESIAN_POINT ( 'NONE',  ( 151.4000000000000057, -17.48000000000005016, 33.92499999999998295 ) ) ;
#82677 = DIRECTION ( 'NONE',  ( -0.000000000000000000, 1.000000000000000000, -0.000000000000000000 ) ) ;
#82678 = EDGE_CURVE ( 'NONE', #47759, #9906, #72624, .T. ) ;
#82679 = AXIS2_PLACEMENT_3D ( 'NONE', #130397, #85425, #98463 ) ;
#82680 = DIRECTION ( 'NONE',  ( 0.7071067811865487940, 0.7071067811865463515, 0.000000000000000000 ) ) ;
#82681 = AXIS2_PLACEMENT_3D ( 'NONE', #37140, #37882, #79269 ) ;
#82682 = CARTESIAN_POINT ( 'NONE',  ( -30.48921356237309510, -27.52281430457076894, 5.000000000000000000 ) ) ;
#82683 = PLANE ( 'NONE',  #80740 ) ;
#82684 = LINE ( 'NONE', #3636, #48637 ) ;
#82686 = ADVANCED_FACE ( 'NONE', ( #95012 ), #51550, .T. ) ;
#82685 = CARTESIAN_POINT ( 'NONE',  ( 3.489213562373097322, -27.52281430457057709, 5.000000000000000000 ) ) ;
#82687 = LINE ( 'NONE', #39175, #132750 ) ;
#82688 = ORIENTED_EDGE ( 'NONE', *, *, #106172, .T. ) ;
#82689 = ORIENTED_EDGE ( 'NONE', *, *, #130980, .F. ) ;
#82690 = EDGE_LOOP ( 'NONE', ( #78312, #117451, #119282, #24308 ) ) ;
#82691 = ORIENTED_EDGE ( 'NONE', *, *, #47642, .T. ) ;
#82692 =( NAMED_UNIT ( * ) SI_UNIT ( $, .STERADIAN. ) SOLID_ANGLE_UNIT ( ) );
#82693 = ORIENTED_EDGE ( 'NONE', *, *, #57389, .T. ) ;
#82694 = ORIENTED_EDGE ( 'NONE', *, *, #79535, .F. ) ;
#82695 = DIRECTION ( 'NONE',  ( 1.000000000000000000, -0.000000000000000000, -0.000000000000000000 ) ) ;
#82696 = DIRECTION ( 'NONE',  ( 0.000000000000000000, -1.000000000000000000, 0.000000000000000000 ) ) ;
#82697 = ADVANCED_FACE ( 'NONE', ( #116784 ), #48685, .F. ) ;
#82698 = DIRECTION ( 'NONE',  ( -0.000000000000000000, 0.3543493200069153248, 0.9351131265310292928 ) ) ;
#82699 = VERTEX_POINT ( 'NONE', #73303 ) ;
#82700 = AXIS2_PLACEMENT_3D ( 'NONE', #124403, #71457, #104786 ) ;
#82701 = DIRECTION ( 'NONE',  ( 0.000000000000000000, -1.000000000000000000, 0.000000000000000000 ) ) ;
#82702 = ORIENTED_EDGE ( 'NONE', *, *, #66430, .F. ) ;
#82703 = DIRECTION ( 'NONE',  ( -1.084202172485504434E-16, 1.000000000000000000, -0.000000000000000000 ) ) ;
#82704 = PLANE ( 'NONE',  #51955 ) ;
#82705 = AXIS2_PLACEMENT_3D ( 'NONE', #69169, #123569, #113348 ) ;
#82706 = CARTESIAN_POINT ( 'NONE',  ( 3.129569808101886341, -3.967499999999998028, -6.871911579029511330 ) ) ;
#82707 = ORIENTED_EDGE ( 'NONE', *, *, #20789, .F. ) ;
#82709 = PLANE ( 'NONE',  #142509 ) ;
#82708 = CARTESIAN_POINT ( 'NONE',  ( 101.7037635252314374, 6.109999999999999432, 1.122388791418549108E-15 ) ) ;
#82710 = CARTESIAN_POINT ( 'NONE',  ( 0.000000000000000000, -30.18000000000009564, 15.92499999999935945 ) ) ;
#82711 = LINE ( 'NONE', #5815, #122983 ) ;
#82712 = ORIENTED_EDGE ( 'NONE', *, *, #24998, .F. ) ;
#82713 = ORIENTED_EDGE ( 'NONE', *, *, #77730, .T. ) ;
#82714 = CARTESIAN_POINT ( 'NONE',  ( 3.278254515685707027, 8.259292476615637923, 11.78515199841151073 ) ) ;
#82715 = EDGE_LOOP ( 'NONE', ( #83982, #97213, #23906, #70231 ) ) ;
#82716 = CARTESIAN_POINT ( 'NONE',  ( -21.49816348513943609, -17.24070752338411339, 8.407044977365272231 ) ) ;
#82717 = CARTESIAN_POINT ( 'NONE',  ( 0.4232784580635307048, 11.25929247661560240, 17.85071094206584519 ) ) ;
#82718 = FACE_OUTER_BOUND ( 'NONE', #132245, .T. ) ;
#82719 = LINE ( 'NONE', #126899, #97944 ) ;
#82720 = CARTESIAN_POINT ( 'NONE',  ( 181.0893910107582201, -48.47007572038016576, -38.12657027910816510 ) ) ;
#82722 = EDGE_CURVE ( 'NONE', #118694, #108262, #37826, .T. ) ;
#82721 = ORIENTED_EDGE ( 'NONE', *, *, #16717, .F. ) ;
#82723 = DIRECTION ( 'NONE',  ( -0.6830127018922180770, -0.6830127018922204085, -0.2588190451025213501 ) ) ;
#82724 = ADVANCED_FACE ( 'NONE', ( #117473 ), #127682, .T. ) ;
#82725 = CARTESIAN_POINT ( 'NONE',  ( 48.48921356237309510, -27.52281430457089328, 5.000000000000000000 ) ) ;
#82726 = DIRECTION ( 'NONE',  ( -0.000000000000000000, -0.3543493200069152693, 0.9351131265310292928 ) ) ;
#82727 = CONICAL_SURFACE ( 'NONE', #87065, 2.055000000000001048, 0.9599310885968758145 ) ;
#82728 = ORIENTED_EDGE ( 'NONE', *, *, #72900, .F. ) ;
#82729 = PLANE ( 'NONE',  #111464 ) ;
#82730 = FACE_OUTER_BOUND ( 'NONE', #36393, .T. ) ;
#82731 = ORIENTED_EDGE ( 'NONE', *, *, #126643, .T. ) ;
#82733 = EDGE_LOOP ( 'NONE', ( #81500, #75261, #68780, #12985 ) ) ;
#82732 = FACE_OUTER_BOUND ( 'NONE', #54201, .T. ) ;
#82734 = EDGE_CURVE ( 'NONE', #95876, #137275, #128392, .T. ) ;
#82735 = ORIENTED_EDGE ( 'NONE', *, *, #7792, .F. ) ;
#82736 = CARTESIAN_POINT ( 'NONE',  ( -5.226068967585342229, 13.12700265372691000, -24.83981276247084224 ) ) ;
#82737 = CYLINDRICAL_SURFACE ( 'NONE', #78538, 28.00000000000002487 ) ;
#82738 = ORIENTED_EDGE ( 'NONE', *, *, #102975, .T. ) ;
#82739 = DIRECTION ( 'NONE',  ( 2.781805975412905274E-17, -0.3543493200069152138, 0.9351131265310292928 ) ) ;
#82740 = LINE ( 'NONE', #61717, #142382 ) ;
#82741 = CARTESIAN_POINT ( 'NONE',  ( -34.47516574401893052, 18.02806734111563358, 4.998110765256835286 ) ) ;
#82742 = VECTOR ( 'NONE', #140752, 999.9999999999998863 ) ;
#82743 =( GEOMETRIC_REPRESENTATION_CONTEXT ( 3 ) GLOBAL_UNCERTAINTY_ASSIGNED_CONTEXT ( ( #124271 ) ) GLOBAL_UNIT_ASSIGNED_CONTEXT ( ( #105053, #50676, #6398 ) ) REPRESENTATION_CONTEXT ( 'NONE', 'WORKASPACE' ) );
#82744 = ORIENTED_EDGE ( 'NONE', *, *, #75394, .F. ) ;
#82745 = PLANE ( 'NONE',  #143416 ) ;
#82746 = CARTESIAN_POINT ( 'NONE',  ( -33.70701326429281153, -21.74070752338405299, 4.999753212805220670 ) ) ;
#82747 = LINE ( 'NONE', #12649, #74256 ) ;
#82748 = LINE ( 'NONE', #113932, #53625 ) ;
#82749 = SURFACE_STYLE_USAGE ( .BOTH. , #136394 ) ;
#82750 = LINE ( 'NONE', #127686, #25786 ) ;
#82751 = LINE ( 'NONE', #137128, #140923 ) ;
#82752 = CARTESIAN_POINT ( 'NONE',  ( 27.78752705046289151, 0.000000000000000000, -7.949999999999998401 ) ) ;
#82753 = DIRECTION ( 'NONE',  ( -0.7071067811865486830, 0.7071067811865464625, 0.000000000000000000 ) ) ;
#82754 = ORIENTED_EDGE ( 'NONE', *, *, #34397, .T. ) ;
#82755 = EDGE_LOOP ( 'NONE', ( #33296, #101605, #58265, #19176 ) ) ;
#82756 = VERTEX_POINT ( 'NONE', #105881 ) ;
#82757 = CARTESIAN_POINT ( 'NONE',  ( 118.9791666666666430, -7.950000000000001066, 2.130196079827424427 ) ) ;
#82758 = VECTOR ( 'NONE', #25691, 1000.000000000000000 ) ;
#82760 = EDGE_CURVE ( 'NONE', #3592, #128295, #16758, .T. ) ;
#82759 = EDGE_LOOP ( 'NONE', ( #137096, #131224, #10514, #49550 ) ) ;
#82761 = ORIENTED_EDGE ( 'NONE', *, *, #77644, .T. ) ;
#82762 = VERTEX_POINT ( 'NONE', #50827 ) ;
#82763 = CARTESIAN_POINT ( 'NONE',  ( -24.18398860626899705, 28.73617430169804265, 5.000000000000000000 ) ) ;
#82764 = CARTESIAN_POINT ( 'NONE',  ( 29.20710678118634718, -17.24070752338410628, 5.000000000000000000 ) ) ;
#82765 = ORIENTED_EDGE ( 'NONE', *, *, #89204, .T. ) ;
#82766 = LINE ( 'NONE', #29090, #76374 ) ;
#82767 = CARTESIAN_POINT ( 'NONE',  ( -34.92500000000001137, 21.66246187583877258, 4.000000000000000000 ) ) ;
#82768 = AXIS2_PLACEMENT_3D ( 'NONE', #50543, #94732, #138995 ) ;
#82769 = DIRECTION ( 'NONE',  ( 0.7071067811865487940, 0.7071067811865463515, 0.000000000000000000 ) ) ;
#82770 = DIRECTION ( 'NONE',  ( 0.6830127018922180770, -0.6830127018922204085, -0.2588190451025213501 ) ) ;
#82771 = CARTESIAN_POINT ( 'NONE',  ( 116.8129301918981184, -1.637169565754159617, -6.110000000000001208 ) ) ;
#82772 = VERTEX_POINT ( 'NONE', #26920 ) ;
#82773 = ADVANCED_FACE ( 'NONE', ( #114632 ), #27625, .F. ) ;
#82774 = DIRECTION ( 'NONE',  ( 0.000000000000000000, -1.000000000000000000, 0.000000000000000000 ) ) ;
#82775 = DIRECTION ( 'NONE',  ( -0.6830127018922180770, -0.6830127018922204085, -0.2588190451025214056 ) ) ;
#82776 = DIRECTION ( 'NONE',  ( -0.000000000000000000, 0.3543493200069153248, 0.9351131265310292928 ) ) ;
#82777 = CARTESIAN_POINT ( 'NONE',  ( 82.76669371712954160, -7.949999999999998401, 2.130196079827423983 ) ) ;
#82778 = DIRECTION ( 'NONE',  ( -0.000000000000000000, 0.3543493200069153248, 0.9351131265310292928 ) ) ;
#82779 = AXIS2_PLACEMENT_3D ( 'NONE', #101372, #46328, #102821 ) ;
#82780 = DIRECTION ( 'NONE',  ( -0.7071067811865487940, 0.7071067811865463515, -0.000000000000000000 ) ) ;
#82781 = PLANE ( 'NONE',  #19943 ) ;
#82782 = VECTOR ( 'NONE', #105779, 1000.000000000000227 ) ;
#82783 = CARTESIAN_POINT ( 'NONE',  ( 35.07919371712955581, 3.975000000000002753, -6.884901960086283523 ) ) ;
#82784 = LINE ( 'NONE', #71205, #99950 ) ;
#82785 = EDGE_CURVE ( 'NONE', #51759, #4075, #95746, .T. ) ;
#82787 = EDGE_CURVE ( 'NONE', #4323, #24129, #116063, .T. ) ;
#82786 = VECTOR ( 'NONE', #16050, 1000.000000000000000 ) ;
#82788 = CARTESIAN_POINT ( 'NONE',  ( -42.29974487139158157, -27.71228299555235708, 4.000000000000000000 ) ) ;
#82789 = ORIENTED_EDGE ( 'NONE', *, *, #56208, .T. ) ;
#82790 = ORIENTED_EDGE ( 'NONE', *, *, #111232, .T. ) ;
#82791 = CARTESIAN_POINT ( 'NONE',  ( 37.45833333333332860, 3.974999999999997424, 6.884901960086288852 ) ) ;
#82792 = EDGE_CURVE ( 'NONE', #118671, #32290, #26221, .T. ) ;
#82793 = ORIENTED_EDGE ( 'NONE', *, *, #11221, .F. ) ;
#82794 = LINE ( 'NONE', #116103, #104170 ) ;
#82795 = EDGE_CURVE ( 'NONE', #91137, #51968, #59581, .T. ) ;
#82796 = LINE ( 'NONE', #4425, #71041 ) ;
#82797 = VECTOR ( 'NONE', #70871, 1000.000000000000000 ) ;
#82798 = ORIENTED_EDGE ( 'NONE', *, *, #80293, .F. ) ;
#82799 = EDGE_CURVE ( 'NONE', #80231, #57697, #105465, .T. ) ;
#82800 = CARTESIAN_POINT ( 'NONE',  ( -18.18398860626898994, 28.73617430169800002, 5.000000000000000000 ) ) ;
#82801 = DIRECTION ( 'NONE',  ( 0.7071067811865487940, 0.7071067811865463515, 0.000000000000000000 ) ) ;
#82802 = CARTESIAN_POINT ( 'NONE',  ( 18.18398860626898994, 28.73617430169800002, 5.000000000000000000 ) ) ;
#82803 = LINE ( 'NONE', #95068, #41874 ) ;
#82804 = EDGE_CURVE ( 'NONE', #107216, #109623, #62429, .T. ) ;
#82805 = CARTESIAN_POINT ( 'NONE',  ( 32.22959685856477563, -6.110000000000000320, -1.637169565754161393 ) ) ;
#82807 = EDGE_CURVE ( 'NONE', #8819, #115197, #94315, .T. ) ;
#82806 = ORIENTED_EDGE ( 'NONE', *, *, #25662, .F. ) ;
#82808 = LINE ( 'NONE', #17515, #15471 ) ;
#82809 = VERTEX_POINT ( 'NONE', #61721 ) ;
#82810 = CARTESIAN_POINT ( 'NONE',  ( -7.001930566820925961, -22.22500000000000142, 4.500000000000000888 ) ) ;
#82811 = SURFACE_SIDE_STYLE ('',( #93678 ) ) ;
#82812 = LINE ( 'NONE', #126993, #123128 ) ;
#82813 = EDGE_CURVE ( 'NONE', #39592, #64109, #102144, .T. ) ;
#82814 = CYLINDRICAL_SURFACE ( 'NONE', #132147, 2.500000000000000444 ) ;
#82815 = ORIENTED_EDGE ( 'NONE', *, *, #56875, .T. ) ;
#82816 = CARTESIAN_POINT ( 'NONE',  ( 59.64626352523142572, -4.472830434245840259, 4.472830434245839371 ) ) ;
#82817 = EDGE_CURVE ( 'NONE', #66568, #44417, #55545, .T. ) ;
#82818 = VERTEX_POINT ( 'NONE', #52243 ) ;
#82819 = CARTESIAN_POINT ( 'NONE',  ( 0.2997448713915885632, -27.71228299555206220, 4.000000000000000000 ) ) ;
#82820 = CARTESIAN_POINT ( 'NONE',  ( 9.370933818357753964, 3.821174125832445049E-16, 0.000000000000000000 ) ) ;
#82821 = CARTESIAN_POINT ( 'NONE',  ( 17.99999999999987210, -4.068876922607775448, 4.000000000000000000 ) ) ;
#82822 = AXIS2_PLACEMENT_3D ( 'NONE', #76468, #55419, #20618 ) ;
#82823 = CARTESIAN_POINT ( 'NONE',  ( 5.068407645496677105, -3.851859888774471706E-31, 2.500000000000001332 ) ) ;
#82825 = EDGE_CURVE ( 'NONE', #54370, #93386, #63157, .T. ) ;
#82824 =( BOUNDED_CURVE ( )  B_SPLINE_CURVE ( 3, ( #62966, #42644, #17963, #8503 ),
 .UNSPECIFIED., .F., .T. ) 
 B_SPLINE_CURVE_WITH_KNOTS ( ( 4, 4 ),
 ( 1.964434688349490754, 3.503810798801452187 ),
 .UNSPECIFIED. ) 
 CURVE ( )  GEOMETRIC_REPRESENTATION_ITEM ( )  RATIONAL_B_SPLINE_CURVE ( ( 1.000000000000000000, 0.8120851936182287290, 0.8120851936182287290, 1.000000000000000000 ) ) 
 REPRESENTATION_ITEM ( '' )  );
#82826 = VECTOR ( 'NONE', #63669, 1000.000000000000000 ) ;
#82827 = CARTESIAN_POINT ( 'NONE',  ( 46.87043019189811588, -3.055000000000001492, 5.291415217122917625 ) ) ;
#82828 = ORIENTED_EDGE ( 'NONE', *, *, #95195, .T. ) ;
#82829 = CARTESIAN_POINT ( 'NONE',  ( 4.499999999999967137, 12.05218569542904561, 5.000000000000000000 ) ) ;
#82830 = CARTESIAN_POINT ( 'NONE',  ( 5.207106781186507050, -5.240707523384232402, 5.000000000000000000 ) ) ;
#82831 = ORIENTED_EDGE ( 'NONE', *, *, #44329, .F. ) ;
#82832 = ORIENTED_EDGE ( 'NONE', *, *, #40297, .T. ) ;
#82833 = CARTESIAN_POINT ( 'NONE',  ( -5.207106781186507050, 3.759292476615680112, 5.000000000000000000 ) ) ;
#82834 = EDGE_LOOP ( 'NONE', ( #109571, #35968, #130317, #34620, #62788, #78537, #134265, #87895, #32663, #63763, #82326, #15247, #139, #13205, #90693, #58256, #95102, #19891, #109378, #30135, #27452, #89613, #62019, #63602, #67837, #30547, #139561, #118393, #69479, #93721, #126599, #104502, #139016, #28919, #60687, #143037, #85352, #28740, #133511, #139732, #16489, #30560, #142456, #43385 ) ) ;
#82835 = DIRECTION ( 'NONE',  ( -0.7071067811865487940, 0.7071067811865463515, -0.000000000000000000 ) ) ;
#82836 = VERTEX_POINT ( 'NONE', #84873 ) ;
#82837 = DIRECTION ( 'NONE',  ( -0.7071067811865486830, -0.7071067811865464625, 0.000000000000000000 ) ) ;
#82838 = EDGE_CURVE ( 'NONE', #57316, #135321, #6355, .T. ) ;
#82839 = DIRECTION ( 'NONE',  ( 0.000000000000000000, 0.000000000000000000, 1.000000000000000000 ) ) ;
#82840 = DIRECTION ( 'NONE',  ( 1.000000000000000000, 3.115803279706882722E-16, 0.000000000000000000 ) ) ;
#82841 = FACE_BOUND ( 'NONE', #208, .T. ) ;
#82842 = DIRECTION ( 'NONE',  ( 0.8571673007021118895, 1.049727191138618079E-16, -0.5150380749100549327 ) ) ;
#82843 = LINE ( 'NONE', #37177, #140536 ) ;
#82844 = ORIENTED_EDGE ( 'NONE', *, *, #93518, .F. ) ;
#82845 = CARTESIAN_POINT ( 'NONE',  ( -13.43359823057990354, 1.153863645259229909, 4.000000000000000000 ) ) ;
#82847 = VERTEX_POINT ( 'NONE', #97897 ) ;
#82846 = CARTESIAN_POINT ( 'NONE',  ( -10.49999999999992539, 6.277155672890260441, -3.510561720658917473 ) ) ;
#82848 = VERTEX_POINT ( 'NONE', #86319 ) ;
#82849 = FACE_OUTER_BOUND ( 'NONE', #44393, .T. ) ;
#82850 = EDGE_CURVE ( 'NONE', #98330, #63466, #142136, .T. ) ;
#82851 = VERTEX_POINT ( 'NONE', #119610 ) ;
#82852 = EDGE_LOOP ( 'NONE', ( #51170, #107602, #131463, #37472 ) ) ;
#82853 = CARTESIAN_POINT ( 'NONE',  ( 69.91209685856478018, 5.291415217122921177, -3.054999999999994831 ) ) ;
#82854 = ORIENTED_EDGE ( 'NONE', *, *, #80238, .T. ) ;
#82855 = COLOUR_RGB ( '', 0.72549020, 0.75294118, 0.79215686) ;
#82856 = CARTESIAN_POINT ( 'NONE',  ( 26.40000000000000568, -17.48000000000005016, -12.70000000000043272 ) ) ;
#82857 = CARTESIAN_POINT ( 'NONE',  ( -60.18398860626900415, 28.73617430169829490, 5.000000000000000000 ) ) ;
#82858 = EDGE_CURVE ( 'NONE', #14349, #142647, #44166, .T. ) ;
#82859 = VERTEX_POINT ( 'NONE', #131234 ) ;
#82860 =( NAMED_UNIT ( * ) SI_UNIT ( $, .STERADIAN. ) SOLID_ANGLE_UNIT ( ) );
#82861 = VECTOR ( 'NONE', #24810, 999.9999999999998863 ) ;
#82862 = CARTESIAN_POINT ( 'NONE',  ( 27.32816939922334143, -6.740707523384214639, 4.000000000000000000 ) ) ;
#82863 = ADVANCED_FACE ( 'NONE', ( #31925 ), #21028, .F. ) ;
#82864 = CARTESIAN_POINT ( 'NONE',  ( 57.29974487139158157, -27.71228299555246011, 4.000000000000000000 ) ) ;
#82865 = PLANE ( 'NONE',  #119873 ) ;
#82866 = CARTESIAN_POINT ( 'NONE',  ( 16.91666666666666785, 5.278424836066147208, 3.047499999999990550 ) ) ;
#82867 = LINE ( 'NONE', #84986, #99481 ) ;
#82868 = ORIENTED_EDGE ( 'NONE', *, *, #13415, .T. ) ;
#82869 = ORIENTED_EDGE ( 'NONE', *, *, #72832, .F. ) ;
#82870 = CARTESIAN_POINT ( 'NONE',  ( 14.11732500641695509, -0.1862019290248694003, 4.000000000000000000 ) ) ;
#82872 = PLANE ( 'NONE',  #7253 ) ;
#82871 = AXIS2_PLACEMENT_3D ( 'NONE', #128008, #38837, #104798 ) ;
#82873 = VERTEX_POINT ( 'NONE', #66010 ) ;
#82874 = ORIENTED_EDGE ( 'NONE', *, *, #59307, .T. ) ;
#82876 = ORIENTED_EDGE ( 'NONE', *, *, #139482, .F. ) ;
#82875 = VECTOR ( 'NONE', #10411, 1000.000000000000000 ) ;
#82877 = LINE ( 'NONE', #72754, #130072 ) ;
#82878 = EDGE_CURVE ( 'NONE', #104684, #99346, #110174, .T. ) ;
#82879 = CARTESIAN_POINT ( 'NONE',  ( 12.86840764549667604, -3.851859888774471706E-31, 2.500000000000001332 ) ) ;
#82880 = ORIENTED_EDGE ( 'NONE', *, *, #119086, .F. ) ;
#82881 = CARTESIAN_POINT ( 'NONE',  ( -2.229957205422064437, 21.73644205237997440, 5.000000000000000888 ) ) ;
#82882 = CIRCLE ( 'NONE', #73663, 2.500000000000000888 ) ;
#82883 =( GEOMETRIC_REPRESENTATION_CONTEXT ( 3 ) GLOBAL_UNCERTAINTY_ASSIGNED_CONTEXT ( ( #104081 ) ) GLOBAL_UNIT_ASSIGNED_CONTEXT ( ( #83564, #137934, #38615 ) ) REPRESENTATION_CONTEXT ( 'NONE', 'WORKASPACE' ) );
#82884 = DIRECTION ( 'NONE',  ( 0.000000000000000000, 0.000000000000000000, 1.000000000000000000 ) ) ;
#82885 = CARTESIAN_POINT ( 'NONE',  ( 11.15040314143521982, 7.934999999999989839, -2.126176841940961904 ) ) ;
#82886 = DIRECTION ( 'NONE',  ( -0.7071067811865486830, -0.7071067811865464625, -0.000000000000000000 ) ) ;
#82887 = EDGE_LOOP ( 'NONE', ( #66381, #107761, #27293, #43178, #1124, #84500 ) ) ;
#82888 = DIRECTION ( 'NONE',  ( -0.000000000000000000, 0.000000000000000000, 1.000000000000000000 ) ) ;
#82889 = FACE_OUTER_BOUND ( 'NONE', #136708, .T. ) ;
#82890 = DIRECTION ( 'NONE',  ( -0.000000000000000000, 0.000000000000000000, 1.000000000000000000 ) ) ;
#82892 = ORIENTED_EDGE ( 'NONE', *, *, #129200, .F. ) ;
#82891 = CARTESIAN_POINT ( 'NONE',  ( -29.99999999999978328, 14.96639925780210767, 5.000000000000000000 ) ) ;
#82893 = CARTESIAN_POINT ( 'NONE',  ( 10.69163961620377279, 6.094999999999988205, -1.633150327867694651 ) ) ;
#82894 = VERTEX_POINT ( 'NONE', #33394 ) ;
#82895 = DIRECTION ( 'NONE',  ( 0.7071067811865487940, 0.7071067811865463515, 0.000000000000000000 ) ) ;
#82896 = LINE ( 'NONE', #37233, #81612 ) ;
#82897 = ADVANCED_FACE ( 'NONE', ( #57997 ), #46414, .F. ) ;
#82898 = FACE_OUTER_BOUND ( 'NONE', #101640, .T. ) ;
#82899 = EDGE_LOOP ( 'NONE', ( #58090, #117865, #71994, #65961 ) ) ;
#82900 = ADVANCED_FACE ( 'NONE', ( #102191 ), #35534, .F. ) ;
#82901 = CARTESIAN_POINT ( 'NONE',  ( 30.70710678118632231, -15.74070752338412760, 5.000000000000000000 ) ) ;
#82902 = FACE_BOUND ( 'NONE', #98263, .T. ) ;
#82903 = CYLINDRICAL_SURFACE ( 'NONE', #51358, 0.5000000000000004441 ) ;
#82904 = ORIENTED_EDGE ( 'NONE', *, *, #127289, .T. ) ;
#82905 = CARTESIAN_POINT ( 'NONE',  ( 10.17183060077640633, -2.240707523384257716, 4.000000000000000000 ) ) ;
#82906 = LINE ( 'NONE', #60458, #121041 ) ;
#82908 = AXIS2_PLACEMENT_3D ( 'NONE', #77018, #32795, #132830 ) ;
#82907 = CARTESIAN_POINT ( 'NONE',  ( 0.1630955763144141257, -0.3999999999999998002, -2.152173649344992334 ) ) ;
#82909 = FACE_OUTER_BOUND ( 'NONE', #104624, .T. ) ;
#82910 = DIRECTION ( 'NONE',  ( -1.000000000000000000, -0.000000000000000000, -0.000000000000000000 ) ) ;
#82911 = EDGE_LOOP ( 'NONE', ( #58167, #90267, #117218, #24356 ) ) ;
#82912 = EDGE_CURVE ( 'NONE', #119060, #63022, #13705, .T. ) ;
#82913 = EDGE_LOOP ( 'NONE', ( #121239, #128381, #87631, #133153 ) ) ;
#82914 = CIRCLE ( 'NONE', #36537, 2.055000000000001048 ) ;
#82915 = CARTESIAN_POINT ( 'NONE',  ( 17.99999999999987566, -4.447814304570784749, 5.000000000000000000 ) ) ;
#82916 = PLANE ( 'NONE',  #140912 ) ;
#82917 = PRODUCT_DEFINITION ( 'UNKNOWN', '', #109627, #80693 ) ;
#82918 = CARTESIAN_POINT ( 'NONE',  ( 3.770403141435219041, -7.934999999999989839, 2.126176841940957907 ) ) ;
#82919 = DIRECTION ( 'NONE',  ( -0.7071067811865486830, -0.7071067811865464625, 0.000000000000000000 ) ) ;
#82920 = DIRECTION ( 'NONE',  ( 0.000000000000000000, 0.000000000000000000, 1.000000000000000000 ) ) ;
#82921 = DIRECTION ( 'NONE',  ( -0.000000000000000000, 0.3543493200069153248, 0.9351131265310292928 ) ) ;
#82922 = LINE ( 'NONE', #37998, #53770 ) ;
#82923 = ORIENTED_EDGE ( 'NONE', *, *, #36788, .F. ) ;
#82924 = DIRECTION ( 'NONE',  ( 0.6830127018922180770, -0.6830127018922204085, -0.2588190451025213501 ) ) ;
#82925 = CARTESIAN_POINT ( 'NONE',  ( -8.999999999999937828, -1.068876922607800761, 4.000000000000000000 ) ) ;
#82926 = CARTESIAN_POINT ( 'NONE',  ( -16.49999999999988276, -10.91253812416064228, 4.000000000000000000 ) ) ;
#82927 = CARTESIAN_POINT ( 'NONE',  ( 50.22459685856477307, -1.637169565754161171, 6.109999999999998543 ) ) ;
#82928 = ADVANCED_FACE ( 'NONE', ( #11559 ), #143535, .F. ) ;
#82929 = DIRECTION ( 'NONE',  ( 0.000000000000000000, 0.000000000000000000, 1.000000000000000000 ) ) ;
#82930 = ORIENTED_EDGE ( 'NONE', *, *, #97143, .T. ) ;
#82931 = ORIENTED_EDGE ( 'NONE', *, *, #130768, .T. ) ;
#82932 = ORIENTED_EDGE ( 'NONE', *, *, #9532, .T. ) ;
#82933 = CARTESIAN_POINT ( 'NONE',  ( -28.49999999999980105, -5.947814304570768762, 5.000000000000000000 ) ) ;
#82934 = CARTESIAN_POINT ( 'NONE',  ( -5.999999999999950262, -4.447814304570779420, 5.000000000000000000 ) ) ;
#82935 = FACE_OUTER_BOUND ( 'NONE', #68608, .T. ) ;
#82936 = DIRECTION ( 'NONE',  ( -1.000000000000000000, 0.000000000000000000, 0.000000000000000000 ) ) ;
#82937 = DIRECTION ( 'NONE',  ( -0.7071067811865486830, -0.7071067811865464625, 0.000000000000000000 ) ) ;
#82938 = ORIENTED_EDGE ( 'NONE', *, *, #101936, .T. ) ;
#82939 = CARTESIAN_POINT ( 'NONE',  ( 1.693225894565048240, 0.2328265696750401181, -6.401774105435452000 ) ) ;
#82940 = LINE ( 'NONE', #127135, #14439 ) ;
#82941 = DIRECTION ( 'NONE',  ( -0.6830127018922181881, 0.6830127018922202975, -0.2588190451025214056 ) ) ;
#82942 = DIRECTION ( 'NONE',  ( -0.6830127018922180770, -0.6830127018922204085, -0.2588190451025213501 ) ) ;
#82943 = CARTESIAN_POINT ( 'NONE',  ( 103.7666937171295416, -7.949999999999998401, 2.130196079827423983 ) ) ;
#82944 = CARTESIAN_POINT ( 'NONE',  ( 68.32919371712955581, -3.975000000000001865, 6.884901960086284411 ) ) ;
#82945 = ADVANCED_FACE ( 'NONE', ( #23914 ), #121763, .T. ) ;
#82946 = CARTESIAN_POINT ( 'NONE',  ( 45.48921356237309510, -27.52281430457087197, 5.000000000000000000 ) ) ;
#82947 = EDGE_LOOP ( 'NONE', ( #135714, #87037, #132928, #47899 ) ) ;
#82948 = VERTEX_POINT ( 'NONE', #22441 ) ;
#82949 = VECTOR ( 'NONE', #40093, 1000.000000000000000 ) ;
#82950 = CARTESIAN_POINT ( 'NONE',  ( 65.16666666666667140, 6.884901960086285300, 3.975000000000003642 ) ) ;
#82951 = DIRECTION ( 'NONE',  ( -0.7071067811865486830, -0.7071067811865464625, -0.000000000000000000 ) ) ;
#82952 = ADVANCED_FACE ( 'NONE', ( #123948 ), #79766, .F. ) ;
#82953 = CARTESIAN_POINT ( 'NONE',  ( -15.48921356237309510, -27.52281430457066236, 5.000000000000000000 ) ) ;
#82954 = EDGE_CURVE ( 'NONE', #66142, #123918, #14454, .T. ) ;
#82955 = EDGE_LOOP ( 'NONE', ( #131078, #83357, #101984, #49533 ) ) ;
#82956 = EDGE_CURVE ( 'NONE', #28313, #36187, #122479, .T. ) ;
#82957 = CARTESIAN_POINT ( 'NONE',  ( 33.37499999999998579, 7.950000000000000178, 1.460391307983218535E-15 ) ) ;
#82958 = VECTOR ( 'NONE', #18122, 1000.000000000000000 ) ;
#82959 = LINE ( 'NONE', #72117, #111477 ) ;
#82960 = CARTESIAN_POINT ( 'NONE',  ( 53.08376352523143282, -6.110000000000001208, -3.741295971395164515E-16 ) ) ;
#82961 = CARTESIAN_POINT ( 'NONE',  ( 21.48921356237309155, -27.52281430457070499, 5.000000000000000000 ) ) ;
#82962 = EDGE_LOOP ( 'NONE', ( #116767, #130062, #134218, #102588 ) ) ;
#82963 = ORIENTED_EDGE ( 'NONE', *, *, #63030, .F. ) ;
#82964 = DIRECTION ( 'NONE',  ( 0.7071067811865487940, -0.7071067811865463515, 0.000000000000000000 ) ) ;
#82965 = AXIS2_PLACEMENT_3D ( 'NONE', #57960, #126048, #67395 ) ;
#82966 = LINE ( 'NONE', #19126, #15258 ) ;
#82967 = CARTESIAN_POINT ( 'NONE',  ( 48.18398860626899705, 28.73617430169820608, 5.000000000000000000 ) ) ;
#82968 = AXIS2_PLACEMENT_3D ( 'NONE', #80172, #46860, #103301 ) ;
#82969 = EDGE_CURVE ( 'NONE', #86438, #25446, #66700, .T. ) ;
#82970 = CARTESIAN_POINT ( 'NONE',  ( -42.18398860626899705, 28.73617430169816700, 5.000000000000000000 ) ) ;
#82971 = EDGE_CURVE ( 'NONE', #54208, #5533, #88463, .T. ) ;
#82972 = DIRECTION ( 'NONE',  ( 0.7071067811865487940, 0.7071067811865463515, -0.000000000000000000 ) ) ;
#82974 = EDGE_LOOP ( 'NONE', ( #94325, #34756, #11026, #45103 ) ) ;
#82973 = CARTESIAN_POINT ( 'NONE',  ( 36.29974487139159578, -27.71228299555231445, 4.000000000000000000 ) ) ;
#82975 = DIRECTION ( 'NONE',  ( -0.000000000000000000, 0.3543493200069153248, 0.9351131265310292928 ) ) ;
#82976 = DIRECTION ( 'NONE',  ( 0.6830127018922181881, 0.6830127018922202975, -0.2588190451025214056 ) ) ;
#82977 = CARTESIAN_POINT ( 'NONE',  ( 24.18398860626899705, 28.73617430169804265, 5.000000000000000000 ) ) ;
#82978 = VECTOR ( 'NONE', #98538, 999.9999999999998863 ) ;
#82979 = PLANE ( 'NONE',  #96981 ) ;
#82980 = VECTOR ( 'NONE', #87651, 1000.000000000000000 ) ;
#82981 = ADVANCED_FACE ( 'NONE', ( #110873 ), #135536, .F. ) ;
#82982 = EDGE_LOOP ( 'NONE', ( #106860, #136668, #52277, #47595 ) ) ;
#82983 = ORIENTED_EDGE ( 'NONE', *, *, #131432, .T. ) ;
#82984 = DIRECTION ( 'NONE',  ( -0.000000000000000000, -0.000000000000000000, 1.000000000000000000 ) ) ;
#82985 = DIRECTION ( 'NONE',  ( -1.000000000000000000, -1.224606353822377258E-16, -0.000000000000000000 ) ) ;
#82986 = CARTESIAN_POINT ( 'NONE',  ( 124.0375270504628986, -9.735942053221456900E-16, 7.949999999999998401 ) ) ;
#82987 = CARTESIAN_POINT ( 'NONE',  ( -34.92500000000001137, 1.701930566820992308, 4.500000000000000888 ) ) ;
#82988 = EDGE_LOOP ( 'NONE', ( #93130, #4801, #16827, #48816 ) ) ;
#82990 = ADVANCED_FACE ( 'NONE', ( #25312 ), #44994, .F. ) ;
#82989 = VERTEX_POINT ( 'NONE', #697 ) ;
#82991 = VECTOR ( 'NONE', #107496, 1000.000000000000000 ) ;
#82992 = CARTESIAN_POINT ( 'NONE',  ( -27.18398860626900060, 28.73617430169806042, 5.000000000000000000 ) ) ;
#82993 = DIRECTION ( 'NONE',  ( 0.000000000000000000, 0.000000000000000000, 1.000000000000000000 ) ) ;
#82994 = VERTEX_POINT ( 'NONE', #124638 ) ;
#82995 = ORIENTED_EDGE ( 'NONE', *, *, #43942, .F. ) ;
#82996 = VECTOR ( 'NONE', #102900, 1000.000000000000000 ) ;
#82997 = CARTESIAN_POINT ( 'NONE',  ( -45.18398860626900415, 28.73617430169818832, 5.000000000000000000 ) ) ;
#82998 = ORIENTED_EDGE ( 'NONE', *, *, #109477, .F. ) ;
#82999 = CARTESIAN_POINT ( 'NONE',  ( 61.18336038379621300, -2.130196079827426203, 7.949999999999996625 ) ) ;
#83000 = EDGE_CURVE ( 'NONE', #8977, #77966, #115601, .T. ) ;
#83001 = CARTESIAN_POINT ( 'NONE',  ( -0.2997448713915885632, -27.71228299555206220, 4.000000000000000000 ) ) ;
#83002 = AXIS2_PLACEMENT_3D ( 'NONE', #8689, #63863, #52938 ) ;
#83003 = VECTOR ( 'NONE', #83648, 1000.000000000000000 ) ;
#83004 = STYLED_ITEM ( 'NONE', ( #105132 ), #106917 ) ;
#83005 = FACE_BOUND ( 'NONE', #112331, .T. ) ;
#83006 = SURFACE_STYLE_FILL_AREA ( #38782 ) ;
#83008 = VERTEX_POINT ( 'NONE', #89168 ) ;
#83007 = DIRECTION ( 'NONE',  ( -0.7071067811865486830, -0.7071067811865464625, 0.000000000000000000 ) ) ;
#83009 = SURFACE_SIDE_STYLE ('',( #69285 ) ) ;
#83011 = ADVANCED_FACE ( 'NONE', ( #13002 ), #101452, .F. ) ;
#83010 = PRODUCT_CONTEXT ( 'NONE', #65216, 'mechanical' ) ;
#83012 = EDGE_LOOP ( 'NONE', ( #13501, #15926, #50227, #131979, #66991 ) ) ;
#83013 = VERTEX_POINT ( 'NONE', #96789 ) ;
#83014 = CARTESIAN_POINT ( 'NONE',  ( 93.97459685856478018, 1.637169565754164280, -6.109999999999996767 ) ) ;
#83015 = VERTEX_POINT ( 'NONE', #30137 ) ;
#83016 = CARTESIAN_POINT ( 'NONE',  ( 11.62000000000000099, 9.521314400968980422E-16, 0.000000000000000000 ) ) ;
#83017 = CARTESIAN_POINT ( 'NONE',  ( 13.49999999999991118, 9.052185695429077583, 5.000000000000000000 ) ) ;
#83018 =( BOUNDED_CURVE ( )  B_SPLINE_CURVE ( 3, ( #7555, #40928, #51815, #130080 ),
 .UNSPECIFIED., .F., .F. ) 
 B_SPLINE_CURVE_WITH_KNOTS ( ( 4, 4 ),
 ( 5.920967161967928050, 7.341195215986656031 ),
 .UNSPECIFIED. ) 
 CURVE ( )  GEOMETRIC_REPRESENTATION_ITEM ( )  RATIONAL_B_SPLINE_CURVE ( ( 1.000000000000000000, 0.8388583629366577199, 0.8388583629366577199, 1.000000000000000000 ) ) 
 REPRESENTATION_ITEM ( '' )  );
#83019 = DIRECTION ( 'NONE',  ( -0.000000000000000000, 0.000000000000000000, 1.000000000000000000 ) ) ;
#83020 =( GEOMETRIC_REPRESENTATION_CONTEXT ( 3 ) GLOBAL_UNCERTAINTY_ASSIGNED_CONTEXT ( ( #134831 ) ) GLOBAL_UNIT_ASSIGNED_CONTEXT ( ( #21217, #10326, #76325 ) ) REPRESENTATION_CONTEXT ( 'NONE', 'WORKASPACE' ) );
#83021 = DIRECTION ( 'NONE',  ( 0.3543493200069163240, 0.000000000000000000, -0.9351131265310288487 ) ) ;
#83022 = ORIENTED_EDGE ( 'NONE', *, *, #76492, .F. ) ;
#83023 = DIRECTION ( 'NONE',  ( 0.000000000000000000, -1.000000000000000000, -0.000000000000000000 ) ) ;
#83024 = CARTESIAN_POINT ( 'NONE',  ( -10.49999999999993250, 10.08746187583914633, 4.000000000000000000 ) ) ;
#83025 = ADVANCED_FACE ( 'NONE', ( #36906 ), #28012, .F. ) ;
#83026 = DIRECTION ( 'NONE',  ( 1.000000000000000000, 0.000000000000000000, 0.000000000000000000 ) ) ;
#83028 = FACE_OUTER_BOUND ( 'NONE', #110751, .T. ) ;
#83027 = DIRECTION ( 'NONE',  ( -0.000000000000000000, -0.3543493200069152693, 0.9351131265310292928 ) ) ;
#83029 = DIRECTION ( 'NONE',  ( 0.7071067811865487940, -0.7071067811865463515, 0.000000000000000000 ) ) ;
#83030 = LINE ( 'NONE', #49711, #76996 ) ;
#83031 = ORIENTED_EDGE ( 'NONE', *, *, #72131, .T. ) ;
#83032 = CARTESIAN_POINT ( 'NONE',  ( 39.48921356237310221, -27.52281430457082934, 5.000000000000000000 ) ) ;
#83033 = LINE ( 'NONE', #113492, #120571 ) ;
#83034 = ORIENTED_EDGE ( 'NONE', *, *, #78185, .T. ) ;
#83035 = ORIENTED_EDGE ( 'NONE', *, *, #88012, .F. ) ;
#83036 = EDGE_CURVE ( 'NONE', #96152, #49642, #138926, .T. ) ;
#83037 = ORIENTED_EDGE ( 'NONE', *, *, #108637, .T. ) ;
#83038 = CARTESIAN_POINT ( 'NONE',  ( 44.77126352523143282, 4.472830434245838482, 4.472830434245842035 ) ) ;
#83039 = ORIENTED_EDGE ( 'NONE', *, *, #89496, .T. ) ;
#83040 = CARTESIAN_POINT ( 'NONE',  ( 17.69163961620376924, 6.094999999999988205, -1.633150327867694651 ) ) ;
#83041 = CARTESIAN_POINT ( 'NONE',  ( -10.22679612720078346, 11.22999999113994996, -26.15788125827728905 ) ) ;
#83042 = ORIENTED_EDGE ( 'NONE', *, *, #135008, .F. ) ;
#83043 = DIRECTION ( 'NONE',  ( -0.7071067811865486830, -0.7071067811865464625, 0.000000000000000000 ) ) ;
#83044 = ORIENTED_EDGE ( 'NONE', *, *, #24785, .T. ) ;
#83045 = CARTESIAN_POINT ( 'NONE',  ( 72.48921356237309510, -27.52281430457106026, 5.000000000000000000 ) ) ;
#83046 = CARTESIAN_POINT ( 'NONE',  ( -23.51078643762690490, -27.52281430457038880, 5.000000000000000000 ) ) ;
#83048 = VERTEX_POINT ( 'NONE', #116449 ) ;
#83047 = CARTESIAN_POINT ( 'NONE',  ( -51.18398860626899705, 28.73617430169823095, 5.000000000000000000 ) ) ;
#83049 = ORIENTED_EDGE ( 'NONE', *, *, #6436, .T. ) ;
#83050 = LINE ( 'NONE', #25801, #111702 ) ;
#83051 = CARTESIAN_POINT ( 'NONE',  ( 31.49999999999977973, -13.53360074219760101, 5.000000000000000000 ) ) ;
#83052 = ORIENTED_EDGE ( 'NONE', *, *, #62945, .T. ) ;
#83053 = CARTESIAN_POINT ( 'NONE',  ( 10.49999999999992895, 15.43112307739203182, 4.000000000000000000 ) ) ;
#83054 = ORIENTED_EDGE ( 'NONE', *, *, #142994, .T. ) ;
#83056 = ORIENTED_EDGE ( 'NONE', *, *, #68561, .T. ) ;
#83055 = EDGE_CURVE ( 'NONE', #124292, #142286, #117138, .T. ) ;
#83057 = ORIENTED_EDGE ( 'NONE', *, *, #16642, .F. ) ;
#83058 = VERTEX_POINT ( 'NONE', #17817 ) ;
#83059 = LINE ( 'NONE', #51875, #42476 ) ;
#83060 = COLOUR_RGB ( '', 0.31764706, 0.68627451, 0.89019608) ;
#83061 = VECTOR ( 'NONE', #107818, 1000.000000000000227 ) ;
#83062 = CIRCLE ( 'NONE', #50665, 2.500000000000000888 ) ;
#83063 = DIRECTION ( 'NONE',  ( 1.000000000000000000, 0.000000000000000000, 0.000000000000000000 ) ) ;
#83064 = AXIS2_PLACEMENT_3D ( 'NONE', #4291, #85476, #28273 ) ;
#83066 = EDGE_CURVE ( 'NONE', #130315, #65177, #83107, .T. ) ;
#83065 = LINE ( 'NONE', #6879, #10014 ) ;
#83067 = CARTESIAN_POINT ( 'NONE',  ( 3.005480084712505828, 28.92564299267936079, 4.000000000000000000 ) ) ;
#83068 = ORIENTED_EDGE ( 'NONE', *, *, #129034, .F. ) ;
#83069 = EDGE_CURVE ( 'NONE', #84409, #4761, #73661, .T. ) ;
#83070 = DIRECTION ( 'NONE',  ( 0.6830127018922181881, 0.6830127018922202975, -0.2588190451025214056 ) ) ;
#83071 = ORIENTED_EDGE ( 'NONE', *, *, #93032, .T. ) ;
#83072 = COLOUR_RGB ( '', 0.09019608, 0.27058824, 0.51372549) ;
#83073 = CONICAL_SURFACE ( 'NONE', #73752, 2.055000000000000604, 0.9599310885968764806 ) ;
#83074 = CARTESIAN_POINT ( 'NONE',  ( 26.45376352523144803, -6.109999999999998543, -3.741295971395162543E-16 ) ) ;
#83075 = CARTESIAN_POINT ( 'NONE',  ( 28.70790314143522437, -6.871911579029513106, -3.967499999999993587 ) ) ;
#83076 = CARTESIAN_POINT ( 'NONE',  ( 20.99999999999985434, -7.068876922607736368, 4.000000000000000000 ) ) ;
#83077 = LINE ( 'NONE', #72954, #6629 ) ;
#83078 = CARTESIAN_POINT ( 'NONE',  ( 53.99451991528749062, 28.92564299267975869, 4.000000000000000000 ) ) ;
#83079 = VERTEX_POINT ( 'NONE', #141039 ) ;
#83080 = ORIENTED_EDGE ( 'NONE', *, *, #42734, .F. ) ;
#83081 = ORIENTED_EDGE ( 'NONE', *, *, #13560, .F. ) ;
#83082 = LINE ( 'NONE', #7634, #134336 ) ;
#83083 = CARTESIAN_POINT ( 'NONE',  ( 94.43336038379622721, 2.130196079827431532, -7.949999999999996625 ) ) ;
#83084 = DIRECTION ( 'NONE',  ( 0.3543493200069162685, -0.000000000000000000, -0.9351131265310288487 ) ) ;
#83085 = PLANE ( 'NONE',  #133083 ) ;
#83086 = CARTESIAN_POINT ( 'NONE',  ( 3.340980275924462894, -49.02095135882305499, -39.67421197283063350 ) ) ;
#83087 = CARTESIAN_POINT ( 'NONE',  ( 78.51626352523145158, -4.472830434245839371, 4.472830434245839371 ) ) ;
#83088 = EDGE_CURVE ( 'NONE', #44162, #129671, #29422, .T. ) ;
#83089 = CARTESIAN_POINT ( 'NONE',  ( 80.04166666666665719, -3.975000000000002753, 6.884901960086286188 ) ) ;
#83091 = LINE ( 'NONE', #4746, #117828 ) ;
#83090 = VECTOR ( 'NONE', #34441, 1000.000000000000000 ) ;
#83092 = CARTESIAN_POINT ( 'NONE',  ( 66.18398860626901126, 28.73617430169833753, 5.000000000000000000 ) ) ;
#83093 = LINE ( 'NONE', #8341, #104331 ) ;
#83094 = PLANE ( 'NONE',  #134 ) ;
#83095 = ORIENTED_EDGE ( 'NONE', *, *, #125081, .T. ) ;
#83096 = VECTOR ( 'NONE', #92166, 1000.000000000000000 ) ;
#83097 = DIRECTION ( 'NONE',  ( -0.7071067811865486830, -0.7071067811865464625, 0.000000000000000000 ) ) ;
#83098 = ORIENTED_EDGE ( 'NONE', *, *, #94110, .T. ) ;
#83099 = VECTOR ( 'NONE', #107017, 1000.000000000000000 ) ;
#83100 = DIRECTION ( 'NONE',  ( -0.3543493200069162685, -0.000000000000000000, -0.9351131265310288487 ) ) ;
#83102 = VERTEX_POINT ( 'NONE', #102901 ) ;
#83101 = CARTESIAN_POINT ( 'NONE',  ( 25.56687199751241835, -21.74070752338406365, 6.915939825044013389 ) ) ;
#83103 = CARTESIAN_POINT ( 'NONE',  ( 22.36246187583885359, 22.22500000000000853, 4.000000000000000000 ) ) ;
#83104 = CARTESIAN_POINT ( 'NONE',  ( -18.79333936457834753, 21.75929247661549937, 4.998822639870701856 ) ) ;
#83105 = VERTEX_POINT ( 'NONE', #61400 ) ;
#83106 = ORIENTED_EDGE ( 'NONE', *, *, #119198, .F. ) ;
#83107 = LINE ( 'NONE', #6919, #116088 ) ;
#83108 = CARTESIAN_POINT ( 'NONE',  ( 0.000000000000000000, 0.000000000000000000, 5.000000000000000000 ) ) ;
#83109 = ORIENTED_EDGE ( 'NONE', *, *, #71408, .T. ) ;
#83110 = AXIS2_PLACEMENT_3D ( 'NONE', #52934, #55843, #8686 ) ;
#83111 = AXIS2_PLACEMENT_3D ( 'NONE', #42031, #31854, #108654 ) ;
#83112 = CARTESIAN_POINT ( 'NONE',  ( -12.70000000000000462, -22.26999999999999247, -39.50000000000000000 ) ) ;
#83113 = CARTESIAN_POINT ( 'NONE',  ( 95.74586038379622721, 3.974999999999996980, 6.884901960086287964 ) ) ;
#83114 = CARTESIAN_POINT ( 'NONE',  ( 71.58333333333332860, 6.884901960086290629, -3.974999999999994316 ) ) ;
#83115 = EDGE_CURVE ( 'NONE', #63249, #92319, #3540, .T. ) ;
#83116 = DIRECTION ( 'NONE',  ( 0.000000000000000000, 0.000000000000000000, -1.000000000000000000 ) ) ;
#83117 = ORIENTED_EDGE ( 'NONE', *, *, #38407, .T. ) ;
#83118 = CARTESIAN_POINT ( 'NONE',  ( -13.49999999999989342, -17.94781430457065241, 5.000000000000000000 ) ) ;
#83119 = EDGE_CURVE ( 'NONE', #71833, #80864, #117836, .T. ) ;
#83120 = CARTESIAN_POINT ( 'NONE',  ( -44.99451991528749772, 28.92564299267969474, 4.000000000000000000 ) ) ;
#83121 = CARTESIAN_POINT ( 'NONE',  ( 22.16666666666666785, -5.278424836066145431, -3.047499999999993658 ) ) ;
#83122 = LINE ( 'NONE', #127322, #127851 ) ;
#83123 = AXIS2_PLACEMENT_3D ( 'NONE', #96059, #9011, #53270 ) ;
#83124 = CARTESIAN_POINT ( 'NONE',  ( -8.994519915287490619, 28.92564299267944250, 4.000000000000000000 ) ) ;
#83125 = ORIENTED_EDGE ( 'NONE', *, *, #83036, .F. ) ;
#83126 = EDGE_CURVE ( 'NONE', #66379, #80080, #118577, .T. ) ;
#83127 = ADVANCED_FACE ( 'NONE', ( #28741 ), #51920, .F. ) ;
#83128 = CARTESIAN_POINT ( 'NONE',  ( 46.16252705046289151, 7.949999999999998401, 1.460391307983218338E-15 ) ) ;
#83129 = ORIENTED_EDGE ( 'NONE', *, *, #69548, .T. ) ;
#83130 = CARTESIAN_POINT ( 'NONE',  ( 87.64626352523141861, -4.472830434245840259, 4.472830434245839371 ) ) ;
#83131 = PLANE ( 'NONE',  #105557 ) ;
#83132 = DIRECTION ( 'NONE',  ( 0.3543493200069162685, -0.000000000000000000, -0.9351131265310288487 ) ) ;
#83133 = DIRECTION ( 'NONE',  ( 0.6830127018922180770, -0.6830127018922204085, -0.2588190451025213501 ) ) ;
#83134 = ORIENTED_EDGE ( 'NONE', *, *, #52806, .T. ) ;
#83135 = LINE ( 'NONE', #71553, #48868 ) ;
#83136 = DIRECTION ( 'NONE',  ( 0.000000000000000000, 1.000000000000000000, 0.000000000000000000 ) ) ;
#83137 = ADVANCED_FACE ( 'NONE', ( #105545 ), #50483, .T. ) ;
#83138 = LINE ( 'NONE', #7693, #62507 ) ;
#83139 = EDGE_CURVE ( 'NONE', #18398, #59514, #133752, .T. ) ;
#83140 = PLANE ( 'NONE',  #28581 ) ;
#83142 = VERTEX_POINT ( 'NONE', #98272 ) ;
#83141 = LINE ( 'NONE', #40374, #140090 ) ;
#83143 = FACE_OUTER_BOUND ( 'NONE', #136703, .T. ) ;
#83144 = CARTESIAN_POINT ( 'NONE',  ( -34.49999999999976552, 3.054329344830908344, 4.994342998332172101 ) ) ;
#83145 = DIRECTION ( 'NONE',  ( 0.3543493200069162685, -0.000000000000000000, -0.9351131265310288487 ) ) ;
#83146 = CARTESIAN_POINT ( 'NONE',  ( 7.045157733366620434, -21.74070752338405654, 21.72585301388586032 ) ) ;
#83147 = ORIENTED_EDGE ( 'NONE', *, *, #35686, .T. ) ;
#83148 = ORIENTED_EDGE ( 'NONE', *, *, #115474, .T. ) ;
#83149 = CARTESIAN_POINT ( 'NONE',  ( 72.91709685856477563, 3.054999999999998828, 5.291415217122922066 ) ) ;
#83150 = ORIENTED_EDGE ( 'NONE', *, *, #50552, .T. ) ;
#83151 = EDGE_CURVE ( 'NONE', #139559, #125103, #42488, .T. ) ;
#83152 = CARTESIAN_POINT ( 'NONE',  ( -34.92500000000001137, 22.22500000000000142, 4.000000000000000000 ) ) ;
#83153 = DIRECTION ( 'NONE',  ( 0.7071067811865487940, 0.7071067811865463515, 0.000000000000000000 ) ) ;
#83154 = DIRECTION ( 'NONE',  ( -0.7071067811865486830, -0.7071067811865464625, 0.000000000000000000 ) ) ;
#83155 = ORIENTED_EDGE ( 'NONE', *, *, #88359, .F. ) ;
#83156 = ADVANCED_FACE ( 'NONE', ( #88836 ), #21422, .F. ) ;
#83157 = LINE ( 'NONE', #7711, #102371 ) ;
#83158 = CARTESIAN_POINT ( 'NONE',  ( 39.29974487139159578, -27.71228299555233576, 4.000000000000000000 ) ) ;
#83159 = ORIENTED_EDGE ( 'NONE', *, *, #127583, .F. ) ;
#83160 = AXIS2_PLACEMENT_3D ( 'NONE', #75416, #64525, #96406 ) ;
#83161 = LINE ( 'NONE', #132417, #113812 ) ;
#83162 = CARTESIAN_POINT ( 'NONE',  ( -11.51078643762690490, -27.52281430457047406, 5.000000000000000000 ) ) ;
#83163 = EDGE_CURVE ( 'NONE', #86472, #106936, #87399, .T. ) ;
#83164 = DIRECTION ( 'NONE',  ( 0.7071067811865486830, -0.7071067811865464625, -0.000000000000000000 ) ) ;
#83165 = VECTOR ( 'NONE', #66449, 1000.000000000000000 ) ;
#83166 = VECTOR ( 'NONE', #112430, 1000.000000000000114 ) ;
#83167 = VECTOR ( 'NONE', #22838, 1000.000000000000000 ) ;
#83168 = ORIENTED_EDGE ( 'NONE', *, *, #101230, .T. ) ;
#83169 = ORIENTED_EDGE ( 'NONE', *, *, #91118, .F. ) ;
#83170 = AXIS2_PLACEMENT_3D ( 'NONE', #59333, #2762, #101365 ) ;
#83171 = DIRECTION ( 'NONE',  ( 0.6830127018922181881, 0.6830127018922202975, -0.2588190451025214056 ) ) ;
#83172 = DIRECTION ( 'NONE',  ( 0.7071067811865487940, 0.7071067811865463515, 0.000000000000000000 ) ) ;
#83173 = EDGE_CURVE ( 'NONE', #92014, #118128, #16195, .T. ) ;
#83174 = CARTESIAN_POINT ( 'NONE',  ( 25.40000000000000213, -6.313548140616198623, -3.022842017553198257 ) ) ;
#83175 = SURFACE_STYLE_USAGE ( .BOTH. , #62871 ) ;
#83176 = EDGE_CURVE ( 'NONE', #122031, #77426, #97536, .T. ) ;
#83177 = CARTESIAN_POINT ( 'NONE',  ( 52.72502705046289151, 5.819803920172573974, -5.819803920172573086 ) ) ;
#83178 = CARTESIAN_POINT ( 'NONE',  ( -28.49999999999980460, -19.91253812416055169, 4.000000000000000000 ) ) ;
#83180 = EDGE_CURVE ( 'NONE', #11459, #136204, #9056, .T. ) ;
#83179 =( NAMED_UNIT ( * ) SI_UNIT ( $, .STERADIAN. ) SOLID_ANGLE_UNIT ( ) );
#83181 = EDGE_LOOP ( 'NONE', ( #77192, #77340, #88213, #136593 ) ) ;
#83182 = ORIENTED_EDGE ( 'NONE', *, *, #86020, .T. ) ;
#83183 = ORIENTED_EDGE ( 'NONE', *, *, #128655, .T. ) ;
#83184 = VERTEX_POINT ( 'NONE', #67072 ) ;
#83185 = VECTOR ( 'NONE', #125905, 1000.000000000000000 ) ;
#83186 = VECTOR ( 'NONE', #20511, 999.9999999999998863 ) ;
#83187 = LINE ( 'NONE', #115763, #75620 ) ;
#83188 = FILL_AREA_STYLE ('',( #93345 ) ) ;
#83189 = ORIENTED_EDGE ( 'NONE', *, *, #128395, .T. ) ;
#83190 = FACE_OUTER_BOUND ( 'NONE', #70014, .T. ) ;
#83191 = CARTESIAN_POINT ( 'NONE',  ( 10.46799328145038821, 4.202752102959690472E-16, 0.000000000000000000 ) ) ;
#83192 = CARTESIAN_POINT ( 'NONE',  ( 6.706123077391905163, 22.22500000000000142, 4.000000000000000000 ) ) ;
#83193 = VECTOR ( 'NONE', #30574, 1000.000000000000227 ) ;
#83194 = PLANE ( 'NONE',  #5106 ) ;
#83195 = ORIENTED_EDGE ( 'NONE', *, *, #112910, .T. ) ;
#83196 = VECTOR ( 'NONE', #140332, 1000.000000000000227 ) ;
#83197 = DIRECTION ( 'NONE',  ( -0.000000000000000000, 0.000000000000000000, 1.000000000000000000 ) ) ;
#83198 = PLANE ( 'NONE',  #34945 ) ;
#83199 = CONICAL_SURFACE ( 'NONE', #108610, 2.500000000000000444, 0.9599310885968830309 ) ;
#83200 = ORIENTED_EDGE ( 'NONE', *, *, #7511, .F. ) ;
#83201 = DIRECTION ( 'NONE',  ( -0.000000000000000000, -0.3543493200069152693, 0.9351131265310292928 ) ) ;
#83202 = ORIENTED_EDGE ( 'NONE', *, *, #124220, .T. ) ;
#83203 = ORIENTED_EDGE ( 'NONE', *, *, #112858, .F. ) ;
#83205 = AXIS2_PLACEMENT_3D ( 'NONE', #42880, #99345, #132755 ) ;
#83204 = CARTESIAN_POINT ( 'NONE',  ( 12.73330628287043886, -6.094999999999989981, -1.633150327867689322 ) ) ;
#83206 = ORIENTED_EDGE ( 'NONE', *, *, #89021, .T. ) ;
#83207 = ORIENTED_EDGE ( 'NONE', *, *, #41600, .F. ) ;
#83209 = VECTOR ( 'NONE', #77437, 1000.000000000000000 ) ;
#83208 = CARTESIAN_POINT ( 'NONE',  ( 75.83376352523144703, 6.110000000000001208, 1.122388791418549305E-15 ) ) ;
#83210 = ORIENTED_EDGE ( 'NONE', *, *, #79896, .F. ) ;
#83211 = AXIS2_PLACEMENT_3D ( 'NONE', #22077, #64184, #43150 ) ;
#83212 = DIRECTION ( 'NONE',  ( 0.000000000000000000, 1.000000000000000000, 0.000000000000000000 ) ) ;
#83213 = CARTESIAN_POINT ( 'NONE',  ( -78.18398860626899705, 28.73617430169841924, 5.000000000000000000 ) ) ;
#83214 = CARTESIAN_POINT ( 'NONE',  ( 105.1462635252314470, -4.472830434245840259, 4.472830434245838482 ) ) ;
#83215 = DIRECTION ( 'NONE',  ( -0.6830127018922181881, 0.6830127018922202975, -0.2588190451025214056 ) ) ;
#83216 = EDGE_CURVE ( 'NONE', #8256, #23712, #97219, .T. ) ;
#83217 = DIRECTION ( 'NONE',  ( 0.3543493200069163240, 0.000000000000000000, 0.9351131265310288487 ) ) ;
#83218 = CARTESIAN_POINT ( 'NONE',  ( 25.39999999999999858, -7.600000000000061817, 34.92499999999998295 ) ) ;
#83219 = VECTOR ( 'NONE', #119075, 1000.000000000000000 ) ;
#83220 = CARTESIAN_POINT ( 'NONE',  ( 25.49999999999982236, 7.466399257802184053, 5.000000000000000000 ) ) ;
#83221 = CARTESIAN_POINT ( 'NONE',  ( -8.999999999999934275, 10.55218569542906337, 5.000000000000000000 ) ) ;
#83222 = CARTESIAN_POINT ( 'NONE',  ( 34.93336038379622011, 2.130196079827431532, -7.949999999999996625 ) ) ;
#83223 = CARTESIAN_POINT ( 'NONE',  ( 34.42499999999998295, 4.541399257802000378, 5.000000000000000000 ) ) ;
#83224 = VERTEX_POINT ( 'NONE', #10515 ) ;
#83225 = FILL_AREA_STYLE ('',( #138318 ) ) ;
#83226 = DIRECTION ( 'NONE',  ( -0.7071067811865486830, -0.7071067811865464625, -0.000000000000000000 ) ) ;
#83227 = VERTEX_POINT ( 'NONE', #54776 ) ;
#83228 = VERTEX_POINT ( 'NONE', #98955 ) ;
#83229 = CARTESIAN_POINT ( 'NONE',  ( 114.9958603837962272, -3.974999999999998312, -6.884901960086286188 ) ) ;
#83230 = ORIENTED_EDGE ( 'NONE', *, *, #84150, .F. ) ;
#83231 = LINE ( 'NONE', #40460, #63133 ) ;
#83232 = CARTESIAN_POINT ( 'NONE',  ( 114.7500000000000000, -9.735942053221458872E-16, 7.950000000000000178 ) ) ;
#83233 = EDGE_CURVE ( 'NONE', #10331, #102158, #86691, .T. ) ;
#83234 = FACE_OUTER_BOUND ( 'NONE', #63371, .T. ) ;
#83235 = CARTESIAN_POINT ( 'NONE',  ( -36.69326993309576324, -3.740707523384241728, 12.88036043432876454 ) ) ;
#83236 = ORIENTED_EDGE ( 'NONE', *, *, #120413, .F. ) ;
#83237 = EDGE_CURVE ( 'NONE', #102725, #20835, #131614, .T. ) ;
#83238 = VERTEX_POINT ( 'NONE', #56235 ) ;
#83239 = EDGE_CURVE ( 'NONE', #128485, #9178, #43184, .T. ) ;
#83240 = EDGE_CURVE ( 'NONE', #23165, #87414, #111255, .T. ) ;
#83241 = CARTESIAN_POINT ( 'NONE',  ( -0.1670968585647806814, -3.967499999999994476, 6.871911579029513106 ) ) ;
#83242 = CARTESIAN_POINT ( 'NONE',  ( 24.70710678118637560, -12.74070752338415602, 5.000000000000000000 ) ) ;
#83243 = PLANE ( 'NONE',  #89878 ) ;
#83244 = EDGE_CURVE ( 'NONE', #41073, #65687, #20871, .T. ) ;
#83245 = DIRECTION ( 'NONE',  ( -0.7071067811865486830, -0.7071067811865464625, 0.000000000000000000 ) ) ;
#83246 = VERTEX_POINT ( 'NONE', #33048 ) ;
#83247 = ORIENTED_EDGE ( 'NONE', *, *, #94851, .F. ) ;
#83248 = ORIENTED_EDGE ( 'NONE', *, *, #75480, .F. ) ;
#83249 = CARTESIAN_POINT ( 'NONE',  ( 13.49999999999991829, 13.08746187583911080, 4.000000000000000000 ) ) ;
#83250 = CARTESIAN_POINT ( 'NONE',  ( 21.24169458425174284, 0.7592924766157173044, 14.37146558664978002 ) ) ;
#83251 = PLANE ( 'NONE',  #14977 ) ;
#83252 = LINE ( 'NONE', #113736, #40362 ) ;
#83253 = DIRECTION ( 'NONE',  ( -0.000000000000000000, 0.000000000000000000, 1.000000000000000000 ) ) ;
#83254 = LINE ( 'NONE', #39776, #117430 ) ;
#83255 = EDGE_CURVE ( 'NONE', #53085, #4806, #77262, .T. ) ;
#83256 = DIRECTION ( 'NONE',  ( -1.000000000000000000, -1.224606353822377258E-16, -0.000000000000000000 ) ) ;
#83257 = DIRECTION ( 'NONE',  ( 0.7071067811865487940, -0.7071067811865463515, 0.000000000000000000 ) ) ;
#83258 = CARTESIAN_POINT ( 'NONE',  ( 3.469446951953614189E-15, -4.447814304570782973, 5.000000000000000000 ) ) ;
#83259 = ORIENTED_EDGE ( 'NONE', *, *, #82954, .F. ) ;
#83260 = CARTESIAN_POINT ( 'NONE',  ( 181.1499999999998067, -49.85820393249939286, 34.92500000000001847 ) ) ;
#83262 = EDGE_CURVE ( 'NONE', #28630, #99304, #55489, .T. ) ;
#83261 = CIRCLE ( 'NONE', #53123, 1.898649999999994842 ) ;
#83263 = VECTOR ( 'NONE', #83342, 1000.000000000000000 ) ;
#83264 = CARTESIAN_POINT ( 'NONE',  ( 3.489213562373097322, -27.52281430457057709, 5.000000000000000000 ) ) ;
#83265 = ORIENTED_EDGE ( 'NONE', *, *, #141672, .T. ) ;
#83266 = CIRCLE ( 'NONE', #143476, 1.249999999999971578 ) ;
#83267 = FACE_OUTER_BOUND ( 'NONE', #59976, .T. ) ;
#83269 = EDGE_LOOP ( 'NONE', ( #36700, #117932, #23634 ) ) ;
#83268 = CARTESIAN_POINT ( 'NONE',  ( 56.65265948608890767, -50.37061236291224020, -37.32649486623387247 ) ) ;
#83270 = CARTESIAN_POINT ( 'NONE',  ( -12.20000000000000462, -22.26999999999999247, -40.00000000000000000 ) ) ;
#83271 = CARTESIAN_POINT ( 'NONE',  ( -8.671830600776406328, -6.740707523384212863, 4.000000000000000000 ) ) ;
#83272 = ADVANCED_FACE ( 'NONE', ( #349 ), #44645, .F. ) ;
#83273 = VERTEX_POINT ( 'NONE', #45346 ) ;
#83274 = ADVANCED_FACE ( 'NONE', ( #1059 ), #26418, .F. ) ;
#83275 = AXIS2_PLACEMENT_3D ( 'NONE', #45516, #78127, #90410 ) ;
#83276 = VERTEX_POINT ( 'NONE', #57639 ) ;
#83277 = CARTESIAN_POINT ( 'NONE',  ( 16.76840764549667639, -2.499999999999996003, 0.000000000000000000 ) ) ;
#83278 = CARTESIAN_POINT ( 'NONE',  ( 117.6208603837962272, -6.884901960086286188, 3.974999999999997424 ) ) ;
#83279 = CARTESIAN_POINT ( 'NONE',  ( 42.18398860626899705, 28.73617430169816700, 5.000000000000000000 ) ) ;
#83280 = AXIS2_PLACEMENT_3D ( 'NONE', #108886, #109628, #118353 ) ;
#83281 = LINE ( 'NONE', #16568, #76049 ) ;
#83282 = CARTESIAN_POINT ( 'NONE',  ( -28.49999999999980460, -7.533600742197660516, 5.000000000000000000 ) ) ;
#83284 = EDGE_CURVE ( 'NONE', #3074, #113572, #13364, .T. ) ;
#83283 = DIRECTION ( 'NONE',  ( -0.000000000000000000, -0.3543493200069152693, 0.9351131265310292928 ) ) ;
#83285 = DIRECTION ( 'NONE',  ( -0.7071067811865486830, -0.7071067811865464625, 0.000000000000000000 ) ) ;
#83286 = CARTESIAN_POINT ( 'NONE',  ( 32.64540314143522437, -2.126176841940958351, -7.934999999999989839 ) ) ;
#83288 = AXIS2_PLACEMENT_3D ( 'NONE', #108748, #31943, #140686 ) ;
#83287 = CARTESIAN_POINT ( 'NONE',  ( 11.49956980810188689, -3.967499999999998028, -6.871911579029511330 ) ) ;
#83289 = CARTESIAN_POINT ( 'NONE',  ( 72.18398860626899705, 28.73617430169837661, 5.000000000000000000 ) ) ;
#83290 = TOROIDAL_SURFACE ( 'NONE', #20764, 3.113037248396092416, 1.500000000000000000 ) ;
#83291 = DIRECTION ( 'NONE',  ( -0.3543493200069162685, -0.000000000000000000, -0.9351131265310288487 ) ) ;
#83292 = PLANE ( 'NONE',  #13107 ) ;
#83293 = ORIENTED_EDGE ( 'NONE', *, *, #125676, .F. ) ;
#83295 = ORIENTED_EDGE ( 'NONE', *, *, #46206, .T. ) ;
#83294 = EDGE_CURVE ( 'NONE', #122295, #1343, #138955, .T. ) ;
#83296 = EDGE_CURVE ( 'NONE', #398, #108741, #80111, .T. ) ;
#83297 = CARTESIAN_POINT ( 'NONE',  ( 79.02083333333332860, 7.949999999999999289, 2.130196079827431532 ) ) ;
#83298 = VECTOR ( 'NONE', #134687, 1000.000000000000000 ) ;
#83299 = DIRECTION ( 'NONE',  ( -0.000000000000000000, 0.000000000000000000, 1.000000000000000000 ) ) ;
#83300 = ORIENTED_EDGE ( 'NONE', *, *, #51867, .T. ) ;
#83301 = CARTESIAN_POINT ( 'NONE',  ( 11.27718569542934191, -21.72500000000000853, 5.000000000000000000 ) ) ;
#83302 = CARTESIAN_POINT ( 'NONE',  ( 44.99451991528749772, 28.92564299267969474, 4.000000000000000000 ) ) ;
#83303 = CARTESIAN_POINT ( 'NONE',  ( 30.26669371712955936, -7.949999999999998401, 2.130196079827423983 ) ) ;
#83304 = ORIENTED_EDGE ( 'NONE', *, *, #85527, .T. ) ;
#83305 = AXIS2_PLACEMENT_3D ( 'NONE', #92226, #125612, #83536 ) ;
#83306 = PLANE ( 'NONE',  #85653 ) ;
#83308 = EDGE_CURVE ( 'NONE', #133790, #25758, #12662, .T. ) ;
#83307 = AXIS2_PLACEMENT_3D ( 'NONE', #83487, #127703, #50845 ) ;
#83309 = CARTESIAN_POINT ( 'NONE',  ( -34.47516574401891631, 3.028067341115791233, 4.998110765256836174 ) ) ;
#83310 = VECTOR ( 'NONE', #14276, 1000.000000000000000 ) ;
#83311 = CARTESIAN_POINT ( 'NONE',  ( 10.15640092694706453, 3.821174125832445049E-16, 0.000000000000000000 ) ) ;
#83312 = DIRECTION ( 'NONE',  ( 0.7071067811865486830, -0.7071067811865464625, -0.000000000000000000 ) ) ;
#83313 = ADVANCED_FACE ( 'NONE', ( #3889 ), #125740, .F. ) ;
#83314 = AXIS2_PLACEMENT_3D ( 'NONE', #20830, #31030, #52744 ) ;
#83315 = CARTESIAN_POINT ( 'NONE',  ( -12.69999999999998153, 0.000000000000000000, 2.500000000000000444 ) ) ;
#83316 = CARTESIAN_POINT ( 'NONE',  ( 72.29974487139158157, -27.71228299555256669, 4.000000000000000000 ) ) ;
#83317 = VECTOR ( 'NONE', #16218, 1000.000000000000000 ) ;
#83318 = CARTESIAN_POINT ( 'NONE',  ( -33.29974487139158867, -27.71228299555229313, 4.000000000000000000 ) ) ;
#83319 = LINE ( 'NONE', #62286, #26212 ) ;
#83320 = CARTESIAN_POINT ( 'NONE',  ( 20.20519093902540320, -2.500000000000000000, 3.061616997868383634E-16 ) ) ;
#83321 = LINE ( 'NONE', #15860, #42952 ) ;
#83322 = LINE ( 'NONE', #128258, #139518 ) ;
#83323 = ORIENTED_EDGE ( 'NONE', *, *, #84374, .F. ) ;
#83324 = EDGE_LOOP ( 'NONE', ( #133845, #72250, #122643, #120103 ) ) ;
#83325 = CARTESIAN_POINT ( 'NONE',  ( 100.4795968585647614, 6.109999999999999432, 1.637169565754164280 ) ) ;
#83326 = ORIENTED_EDGE ( 'NONE', *, *, #36894, .T. ) ;
#83327 = EDGE_CURVE ( 'NONE', #75885, #123393, #1752, .T. ) ;
#83328 = SURFACE_SIDE_STYLE ('',( #51418 ) ) ;
#83329 = AXIS2_PLACEMENT_3D ( 'NONE', #23909, #68171, #134836 ) ;
#83330 = CARTESIAN_POINT ( 'NONE',  ( -54.48921356237310221, -27.52281430457093236, 5.000000000000000000 ) ) ;
#83331 = ORIENTED_EDGE ( 'NONE', *, *, #104100, .T. ) ;
#83332 = EDGE_CURVE ( 'NONE', #77939, #36177, #138981, .T. ) ;
#83333 = CARTESIAN_POINT ( 'NONE',  ( -63.18398860626900415, 28.73617430169831621, 5.000000000000000000 ) ) ;
#83334 = CARTESIAN_POINT ( 'NONE',  ( 13.08316395874281568, 3.014287036135060660, 4.000000000000000000 ) ) ;
#83335 = CARTESIAN_POINT ( 'NONE',  ( 103.7454301918981230, -5.291415217122918513, -3.055000000000000160 ) ) ;
#83336 = ORIENTED_EDGE ( 'NONE', *, *, #73139, .F. ) ;
#83337 = CARTESIAN_POINT ( 'NONE',  ( -8.994519915287490619, 28.92564299267944250, 4.000000000000000000 ) ) ;
#83338 = VERTEX_POINT ( 'NONE', #135886 ) ;
#83339 = CARTESIAN_POINT ( 'NONE',  ( 1.828169399223523284, 6.759292476615653023, 4.000000000000000000 ) ) ;
#83340 = AXIS2_PLACEMENT_3D ( 'NONE', #12596, #90909, #101031 ) ;
#83341 = LINE ( 'NONE', #72505, #10718 ) ;
#83342 = DIRECTION ( 'NONE',  ( 0.7071067811865486830, -0.7071067811865464625, -0.000000000000000000 ) ) ;
#83343 = ORIENTED_EDGE ( 'NONE', *, *, #89372, .F. ) ;
#83344 = EDGE_LOOP ( 'NONE', ( #20623, #66671, #80416, #12617 ) ) ;
#83345 = ORIENTED_EDGE ( 'NONE', *, *, #41306, .T. ) ;
#83346 = CARTESIAN_POINT ( 'NONE',  ( -31.49999999999977973, 21.43112307739196964, 4.000000000000000000 ) ) ;
#83347 = FACE_OUTER_BOUND ( 'NONE', #113878, .T. ) ;
#83348 = CARTESIAN_POINT ( 'NONE',  ( 11.15040314143522160, 7.934999999999988951, -2.126176841940961904 ) ) ;
#83349 = FACE_OUTER_BOUND ( 'NONE', #122854, .T. ) ;
#83350 = EDGE_CURVE ( 'NONE', #111254, #64560, #14814, .T. ) ;
#83351 = EDGE_CURVE ( 'NONE', #137064, #29922, #35175, .T. ) ;
#83352 = DIRECTION ( 'NONE',  ( -0.7071067811865487940, 0.7071067811865463515, -0.000000000000000000 ) ) ;
#83353 = VERTEX_POINT ( 'NONE', #135206 ) ;
#83354 = ORIENTED_EDGE ( 'NONE', *, *, #124799, .T. ) ;
#83355 = FACE_OUTER_BOUND ( 'NONE', #56685, .T. ) ;
#83356 = EDGE_LOOP ( 'NONE', ( #11545, #47593, #58913, #44810, #137301 ) ) ;
#83357 = ORIENTED_EDGE ( 'NONE', *, *, #30291, .F. ) ;
#83358 = B_SPLINE_CURVE_WITH_KNOTS ( 'NONE', 3,
 ( #122742, #45924, #90859, #100987 ),
 .UNSPECIFIED., .F., .F.,
 ( 4, 4 ),
 ( 0.003609336753060590330, 0.003809496093231038664 ),
 .UNSPECIFIED. ) ;
#83359 = CARTESIAN_POINT ( 'NONE',  ( 115.1204301918981230, 3.055000000000001936, -5.291415217122916737 ) ) ;
#83360 = VECTOR ( 'NONE', #72945, 1000.000000000000000 ) ;
#83361 = LINE ( 'NONE', #114541, #74398 ) ;
#83362 = FACE_OUTER_BOUND ( 'NONE', #97969, .T. ) ;
#83363 = EDGE_LOOP ( 'NONE', ( #50278, #99956, #91950, #124329 ) ) ;
#83364 = CARTESIAN_POINT ( 'NONE',  ( -13.49999999999990763, -1.592773361805379428, -6.492772025301195349 ) ) ;
#83365 = DIRECTION ( 'NONE',  ( -0.3543493200069162685, -0.000000000000000000, -0.9351131265310288487 ) ) ;
#83366 = CARTESIAN_POINT ( 'NONE',  ( 0.000000000000000000, 0.000000000000000000, 5.000000000000000000 ) ) ;
#83367 = CIRCLE ( 'NONE', #81001, 2.500000000000000888 ) ;
#83368 = VECTOR ( 'NONE', #60102, 1000.000000000000000 ) ;
#83369 = AXIS2_PLACEMENT_3D ( 'NONE', #57248, #78999, #89829 ) ;
#83370 = CARTESIAN_POINT ( 'NONE',  ( 14.08373646989360317, 2.500000000000003109, 3.061616997868386592E-16 ) ) ;
#83371 = VERTEX_POINT ( 'NONE', #4584 ) ;
#83372 = AXIS2_PLACEMENT_3D ( 'NONE', #53053, #42221, #130660 ) ;
#83373 = DIRECTION ( 'NONE',  ( 0.7071067811865487940, 0.7071067811865463515, 0.000000000000000000 ) ) ;
#83374 = FACE_BOUND ( 'NONE', #53218, .T. ) ;
#83375 = EDGE_LOOP ( 'NONE', ( #6841, #11004, #143225, #23866, #81403, #69884 ) ) ;
#83376 = DIRECTION ( 'NONE',  ( -0.6830127018922180770, -0.6830127018922204085, -0.2588190451025213501 ) ) ;
#83377 = CARTESIAN_POINT ( 'NONE',  ( 25.49999999999983302, 22.08746187583901843, 4.000000000000000000 ) ) ;
#83378 = FILL_AREA_STYLE_COLOUR ( '', #538 ) ;
#83379 = ORIENTED_EDGE ( 'NONE', *, *, #125346, .F. ) ;
#83380 = DIRECTION ( 'NONE',  ( 0.3543493200069163240, 0.000000000000000000, -0.9351131265310288487 ) ) ;
#83381 = ORIENTED_EDGE ( 'NONE', *, *, #102895, .T. ) ;
#83382 = ORIENTED_EDGE ( 'NONE', *, *, #19049, .F. ) ;
#83383 = VECTOR ( 'NONE', #87405, 1000.000000000000227 ) ;
#83384 = ORIENTED_EDGE ( 'NONE', *, *, #94830, .T. ) ;
#83385 = CARTESIAN_POINT ( 'NONE',  ( 26.89126352523144092, -4.472830434245838482, -4.472830434245838482 ) ) ;
#83386 = EDGE_LOOP ( 'NONE', ( #49269, #45461, #118131, #61842 ) ) ;
#83387 = LINE ( 'NONE', #38453, #113196 ) ;
#83388 = CARTESIAN_POINT ( 'NONE',  ( -3.489213562373097322, -27.52281430457057709, 5.000000000000000000 ) ) ;
#83389 = DIRECTION ( 'NONE',  ( -0.7071067811865486830, -0.7071067811865464625, -0.000000000000000000 ) ) ;
#83390 = CARTESIAN_POINT ( 'NONE',  ( -25.39999999999996305, 0.000000000000000000, 0.000000000000000000 ) ) ;
#83391 = EDGE_CURVE ( 'NONE', #47602, #118704, #101103, .T. ) ;
#83392 = DIRECTION ( 'NONE',  ( 0.7071067811865487940, -0.7071067811865463515, 0.000000000000000000 ) ) ;
#83393 = VECTOR ( 'NONE', #96942, 1000.000000000000000 ) ;
#83394 = LINE ( 'NONE', #63092, #100151 ) ;
#83395 = VECTOR ( 'NONE', #127915, 1000.000000000000000 ) ;
#83396 = SURFACE_SIDE_STYLE ('',( #26159 ) ) ;
#83397 = CARTESIAN_POINT ( 'NONE',  ( 9.473360963642086574, -5.240707523384232402, 16.25846745537497995 ) ) ;
#83398 = FACE_OUTER_BOUND ( 'NONE', #108347, .T. ) ;
#83399 = VERTEX_POINT ( 'NONE', #35893 ) ;
#83400 = VECTOR ( 'NONE', #9817, 1000.000000000000000 ) ;
#83401 = ORIENTED_EDGE ( 'NONE', *, *, #60897, .T. ) ;
#83402 = VERTEX_POINT ( 'NONE', #48168 ) ;
#83403 = ORIENTED_EDGE ( 'NONE', *, *, #120092, .T. ) ;
#83404 = DIRECTION ( 'NONE',  ( 0.7071067811865487940, 0.7071067811865463515, 0.000000000000000000 ) ) ;
#83405 = ORIENTED_EDGE ( 'NONE', *, *, #20383, .T. ) ;
#83406 = CIRCLE ( 'NONE', #67159, 2.500000000000000888 ) ;
#83408 = VERTEX_POINT ( 'NONE', #24271 ) ;
#83407 = ADVANCED_FACE ( 'NONE', ( #37290 ), #81539, .F. ) ;
#83409 = DIRECTION ( 'NONE',  ( 0.000000000000000000, 0.000000000000000000, -1.000000000000000000 ) ) ;
#83410 = DIRECTION ( 'NONE',  ( -0.6830127018922180770, -0.6830127018922204085, -0.2588190451025213501 ) ) ;
#83411 = EDGE_CURVE ( 'NONE', #25811, #118828, #134473, .T. ) ;
#83412 = ADVANCED_FACE ( 'NONE', ( #93096 ), #47501, .F. ) ;
#83413 = VECTOR ( 'NONE', #126558, 1000.000000000000000 ) ;
#83414 = FACE_OUTER_BOUND ( 'NONE', #5075, .T. ) ;
#83415 = VERTEX_POINT ( 'NONE', #91662 ) ;
#83416 = DIRECTION ( 'NONE',  ( 0.3543493200069164351, 2.781805975412904658E-17, -0.9351131265310288487 ) ) ;
#83417 = ORIENTED_EDGE ( 'NONE', *, *, #133286, .F. ) ;
#83419 = EDGE_CURVE ( 'NONE', #119897, #93928, #13933, .T. ) ;
#83418 = FACE_OUTER_BOUND ( 'NONE', #99472, .T. ) ;
#83420 = EDGE_CURVE ( 'NONE', #91475, #98898, #125005, .T. ) ;
#83421 = CARTESIAN_POINT ( 'NONE',  ( 34.92499999999998295, 8.816654386410357702, 4.500000000000000888 ) ) ;
#83422 = AXIS2_PLACEMENT_3D ( 'NONE', #6817, #95295, #96002 ) ;
#83423 = SURFACE_STYLE_USAGE ( .BOTH. , #114590 ) ;
#83424 = VERTEX_POINT ( 'NONE', #128577 ) ;
#83426 = DIRECTION ( 'NONE',  ( -0.6830127018922181881, 0.6830127018922202975, -0.2588190451025214056 ) ) ;
#83425 = CARTESIAN_POINT ( 'NONE',  ( 104.0370968585647802, -3.054999999999999272, -5.291415217122919401 ) ) ;
#83427 = EDGE_CURVE ( 'NONE', #100333, #11776, #115510, .T. ) ;
#83428 = DIRECTION ( 'NONE',  ( -1.000000000000000000, -0.000000000000000000, -0.000000000000000000 ) ) ;
#83429 = VERTEX_POINT ( 'NONE', #138752 ) ;
#83430 = ORIENTED_EDGE ( 'NONE', *, *, #5836, .T. ) ;
#83431 = LINE ( 'NONE', #126894, #40371 ) ;
#83432 = VECTOR ( 'NONE', #119801, 1000.000000000000000 ) ;
#83433 = ORIENTED_EDGE ( 'NONE', *, *, #133355, .T. ) ;
#83434 =( LENGTH_UNIT ( ) NAMED_UNIT ( * ) SI_UNIT ( .MILLI., .METRE. ) );
#83435 = CARTESIAN_POINT ( 'NONE',  ( -11.99999999999991296, 1.761378380278670663, -6.096875308897281798 ) ) ;
#83436 = CARTESIAN_POINT ( 'NONE',  ( 14.20710678118644665, -8.240707523384200428, 5.000000000000000000 ) ) ;
#83437 = CARTESIAN_POINT ( 'NONE',  ( 180.5530070941699705, -49.14999999999999147, -40.56450646616441702 ) ) ;
#83438 = VERTEX_POINT ( 'NONE', #40857 ) ;
#83439 = DIRECTION ( 'NONE',  ( 0.7071067811865486830, -0.7071067811865464625, -0.000000000000000000 ) ) ;
#83440 = EDGE_CURVE ( 'NONE', #93458, #85512, #40177, .T. ) ;
#83441 = CARTESIAN_POINT ( 'NONE',  ( 0.000000000000000000, 0.000000000000000000, 5.000000000000000000 ) ) ;
#83442 = VERTEX_POINT ( 'NONE', #72097 ) ;
#83443 = CARTESIAN_POINT ( 'NONE',  ( 6.792893218813413014, -8.240707523384202204, 5.000000000000000000 ) ) ;
#83444 = COLOUR_RGB ( '', 0.31764706, 0.68627451, 0.89019608) ;
#83445 = CARTESIAN_POINT ( 'NONE',  ( -33.48921356237309510, -27.52281430457078670, 5.000000000000000000 ) ) ;
#83446 = EDGE_LOOP ( 'NONE', ( #105411, #7902, #13018, #101429 ) ) ;
#83448 = VERTEX_POINT ( 'NONE', #85063 ) ;
#83447 = FACE_OUTER_BOUND ( 'NONE', #986, .T. ) ;
#83449 = ORIENTED_EDGE ( 'NONE', *, *, #109740, .T. ) ;
#83450 = LINE ( 'NONE', #59572, #97992 ) ;
#83451 = ADVANCED_FACE ( 'NONE', ( #73494 ), #83676, .F. ) ;
#83453 = ORIENTED_EDGE ( 'NONE', *, *, #71048, .F. ) ;
#83452 = VECTOR ( 'NONE', #80107, 1000.000000000000000 ) ;
#83454 = DIRECTION ( 'NONE',  ( 0.7071067811865486830, -0.7071067811865464625, -0.000000000000000000 ) ) ;
#83455 = CARTESIAN_POINT ( 'NONE',  ( 27.18398860626900060, 28.73617430169806042, 5.000000000000000000 ) ) ;
#83456 = SURFACE_SIDE_STYLE ('',( #18145 ) ) ;
#83457 = ORIENTED_EDGE ( 'NONE', *, *, #25896, .T. ) ;
#83458 = FACE_OUTER_BOUND ( 'NONE', #134488, .T. ) ;
#83459 = LINE ( 'NONE', #28367, #113545 ) ;
#83460 = CARTESIAN_POINT ( 'NONE',  ( 2.625000000000000000, 6.094999999999989981, -1.119633336120465690E-15 ) ) ;
#83462 = EDGE_CURVE ( 'NONE', #66788, #108741, #127134, .T. ) ;
#83461 = CARTESIAN_POINT ( 'NONE',  ( 47.52083333333332860, 7.949999999999998401, 2.130196079827431532 ) ) ;
#83463 = CARTESIAN_POINT ( 'NONE',  ( 11.29298673570687050, -21.74070752338406365, 4.999753212805220670 ) ) ;
#83464 = FACE_OUTER_BOUND ( 'NONE', #62014, .T. ) ;
#83465 = VECTOR ( 'NONE', #58661, 1000.000000000000000 ) ;
#83466 = DIRECTION ( 'NONE',  ( 0.000000000000000000, -1.000000000000000000, 0.000000000000000000 ) ) ;
#83467 = SURFACE_STYLE_FILL_AREA ( #40678 ) ;
#83468 = EDGE_LOOP ( 'NONE', ( #124094, #31917, #101491, #69173 ) ) ;
#83469 =( BOUNDED_CURVE ( )  B_SPLINE_CURVE ( 3, ( #61000, #138514, #94975, #27587 ),
 .UNSPECIFIED., .F., .F. ) 
 B_SPLINE_CURVE_WITH_KNOTS ( ( 4, 4 ),
 ( 1.964434688349496083, 3.503810798801452187 ),
 .UNSPECIFIED. ) 
 CURVE ( )  GEOMETRIC_REPRESENTATION_ITEM ( )  RATIONAL_B_SPLINE_CURVE ( ( 1.000000000000000000, 0.8120851936182298392, 0.8120851936182298392, 1.000000000000000000 ) ) 
 REPRESENTATION_ITEM ( '' )  );
#83470 = ORIENTED_EDGE ( 'NONE', *, *, #108740, .T. ) ;
#83471 = ORIENTED_EDGE ( 'NONE', *, *, #36274, .F. ) ;
#83472 = ADVANCED_FACE ( 'NONE', ( #49628 ), #84387, .F. ) ;
#83473 = CARTESIAN_POINT ( 'NONE',  ( 115.1874999999999716, -5.819803920172573086, 5.819803920172572198 ) ) ;
#83474 = AXIS2_PLACEMENT_3D ( 'NONE', #21292, #85111, #129319 ) ;
#83475 = ORIENTED_EDGE ( 'NONE', *, *, #67997, .F. ) ;
#83476 = VERTEX_POINT ( 'NONE', #5342 ) ;
#83477 = EDGE_CURVE ( 'NONE', #67994, #59910, #60235, .T. ) ;
#83478 = VERTEX_POINT ( 'NONE', #93802 ) ;
#83479 = DIRECTION ( 'NONE',  ( 0.7071067811865487940, 0.7071067811865463515, -0.000000000000000000 ) ) ;
#83480 = LINE ( 'NONE', #137867, #30073 ) ;
#83481 = VECTOR ( 'NONE', #72402, 1000.000000000000000 ) ;
#83482 = PRESENTATION_LAYER_ASSIGNMENT (  '', '', ( #104343 ) ) ;
#83483 = VECTOR ( 'NONE', #93409, 1000.000000000000000 ) ;
#83484 = VECTOR ( 'NONE', #113631, 1000.000000000000000 ) ;
#83485 = ORIENTED_EDGE ( 'NONE', *, *, #61257, .T. ) ;
#83486 =( BOUNDED_CURVE ( )  B_SPLINE_CURVE ( 3, ( #57843, #68709, #102033, #90439 ),
 .UNSPECIFIED., .F., .T. ) 
 B_SPLINE_CURVE_WITH_KNOTS ( ( 4, 4 ),
 ( 0.4286956587950770392, 0.5111536932531050015 ),
 .UNSPECIFIED. ) 
 CURVE ( )  GEOMETRIC_REPRESENTATION_ITEM ( )  RATIONAL_B_SPLINE_CURVE ( ( 1.000000000000000000, 0.9994334696367943582, 0.9994334696367943582, 1.000000000000000000 ) ) 
 REPRESENTATION_ITEM ( '' )  );
#83487 = CARTESIAN_POINT ( 'NONE',  ( 0.000000000000000000, 0.000000000000000000, 5.000000000000000000 ) ) ;
#83488 = EDGE_CURVE ( 'NONE', #72014, #105080, #29958, .T. ) ;
#83489 = VECTOR ( 'NONE', #66114, 999.9999999999998863 ) ;
#83490 = FILL_AREA_STYLE ('',( #29091 ) ) ;
#83491 = DIRECTION ( 'NONE',  ( -0.000000000000000000, -0.3543493200069152693, 0.9351131265310292928 ) ) ;
#83492 = PLANE ( 'NONE',  #90483 ) ;
#83493 = CARTESIAN_POINT ( 'NONE',  ( 113.7504301918981042, 3.055000000000002824, -5.291415217122919401 ) ) ;
#83494 = VERTEX_POINT ( 'NONE', #106070 ) ;
#83495 = CARTESIAN_POINT ( 'NONE',  ( -13.69211732441125662, 5.972909523125048636, -31.41169802726832927 ) ) ;
#83496 = DIRECTION ( 'NONE',  ( 0.7071067811865487940, 0.7071067811865463515, -0.000000000000000000 ) ) ;
#83497 = CIRCLE ( 'NONE', #102001, 2.055000000000001048 ) ;
#83498 = CARTESIAN_POINT ( 'NONE',  ( -2.999999999999981792, 5.966399257802200040, 5.000000000000000000 ) ) ;
#83499 = FACE_OUTER_BOUND ( 'NONE', #41988, .T. ) ;
#83500 = EDGE_CURVE ( 'NONE', #77065, #77128, #39449, .T. ) ;
#83501 = PLANE ( 'NONE',  #123304 ) ;
#83502 = CARTESIAN_POINT ( 'NONE',  ( -5.163471288734476694, 15.75929247661555976, 9.299976744542908236 ) ) ;
#83503 = CARTESIAN_POINT ( 'NONE',  ( 38.28752705046288440, 0.000000000000000000, -7.949999999999998401 ) ) ;
#83504 = FACE_OUTER_BOUND ( 'NONE', #128002, .T. ) ;
#83505 = DIRECTION ( 'NONE',  ( -0.000000000000000000, -0.000000000000000000, 1.000000000000000000 ) ) ;
#83506 = EDGE_LOOP ( 'NONE', ( #26579, #17552, #9333, #90975 ) ) ;
#83507 = ORIENTED_EDGE ( 'NONE', *, *, #135008, .T. ) ;
#83508 = CARTESIAN_POINT ( 'NONE',  ( 31.91666666666666430, -6.884901960086287076, -3.975000000000000977 ) ) ;
#83509 = ORIENTED_EDGE ( 'NONE', *, *, #574, .F. ) ;
#83510 = EDGE_CURVE ( 'NONE', #1974, #55061, #28565, .T. ) ;
#83511 = DIRECTION ( 'NONE',  ( 0.5735764363510451602, 0.8191520442889924647, 0.000000000000000000 ) ) ;
#83512 = VECTOR ( 'NONE', #120690, 1000.000000000000000 ) ;
#83513 = CARTESIAN_POINT ( 'NONE',  ( 40.03752705046288440, -9.735942053221456900E-16, 7.949999999999998401 ) ) ;
#83514 = CARTESIAN_POINT ( 'NONE',  ( 25.99384647351989130, 22.22500000000000142, -18.08442819488239195 ) ) ;
#83515 = CARTESIAN_POINT ( 'NONE',  ( -9.183988606268997046, 28.73617430169793607, 5.000000000000000000 ) ) ;
#83516 = CARTESIAN_POINT ( 'NONE',  ( -22.82816939922337340, -20.24070752338407075, 4.000000000000000000 ) ) ;
#83517 = DIRECTION ( 'NONE',  ( 0.7071067811865487940, 0.7071067811865463515, 0.000000000000000000 ) ) ;
#83518 = AXIS2_PLACEMENT_3D ( 'NONE', #124539, #1991, #111513 ) ;
#83519 = VECTOR ( 'NONE', #75538, 1000.000000000000000 ) ;
#83520 = CARTESIAN_POINT ( 'NONE',  ( 30.33376352523143993, 6.110000000000001208, 1.122388791418549305E-15 ) ) ;
#83521 = EDGE_CURVE ( 'NONE', #28383, #21537, #62621, .T. ) ;
#83522 = VERTEX_POINT ( 'NONE', #116975 ) ;
#83523 = VECTOR ( 'NONE', #60324, 1000.000000000000227 ) ;
#83524 = CARTESIAN_POINT ( 'NONE',  ( -25.49999999999981881, 4.466399257802215139, 5.000000000000000000 ) ) ;
#83525 = ORIENTED_EDGE ( 'NONE', *, *, #47910, .T. ) ;
#83526 = CARTESIAN_POINT ( 'NONE',  ( -33.29974487139158867, -27.71228299555229313, 4.000000000000000000 ) ) ;
#83527 = VECTOR ( 'NONE', #122120, 1000.000000000000000 ) ;
#83528 = CARTESIAN_POINT ( 'NONE',  ( -28.17183060077627133, -14.24070752338413648, 4.000000000000000000 ) ) ;
#83529 = CARTESIAN_POINT ( 'NONE',  ( -4.499999999999966249, -2.947814304570802513, 5.000000000000000000 ) ) ;
#83530 = CARTESIAN_POINT ( 'NONE',  ( 63.41666666666666430, -6.884901960086287076, -3.975000000000000977 ) ) ;
#83531 = VERTEX_POINT ( 'NONE', #61236 ) ;
#83532 = EDGE_CURVE ( 'NONE', #89577, #9427, #29251, .T. ) ;
#83533 = CARTESIAN_POINT ( 'NONE',  ( 54.68793019189810423, 6.110000000000002984, -1.637169565754156730 ) ) ;
#83534 = VERTEX_POINT ( 'NONE', #105381 ) ;
#83535 = DIRECTION ( 'NONE',  ( 0.7071067811865487940, 0.7071067811865463515, 0.000000000000000000 ) ) ;
#83536 = DIRECTION ( 'NONE',  ( 1.000000000000000000, 0.000000000000000000, 0.000000000000000000 ) ) ;
#83537 = ADVANCED_FACE ( 'NONE', ( #19095 ), #50313, .F. ) ;
#83538 = CARTESIAN_POINT ( 'NONE',  ( 36.48921356237310221, -27.52281430457080802, 5.000000000000000000 ) ) ;
#83539 = CARTESIAN_POINT ( 'NONE',  ( 32.21837311707483309, 21.74787736706806740, 4.999607392498048419 ) ) ;
#83540 = EDGE_CURVE ( 'NONE', #44583, #136777, #61916, .T. ) ;
#83541 = AXIS2_PLACEMENT_3D ( 'NONE', #86500, #118379, #39433 ) ;
#83543 = EDGE_CURVE ( 'NONE', #140063, #19565, #11249, .T. ) ;
#83542 = CARTESIAN_POINT ( 'NONE',  ( 47.45376352523145158, -6.109999999999998543, -3.741295971395162543E-16 ) ) ;
#83544 = ORIENTED_EDGE ( 'NONE', *, *, #112372, .F. ) ;
#83545 = DIRECTION ( 'NONE',  ( 0.7071067811865486830, -0.7071067811865464625, -0.000000000000000000 ) ) ;
#83546 = LINE ( 'NONE', #127754, #8514 ) ;
#83547 = ORIENTED_EDGE ( 'NONE', *, *, #4330, .T. ) ;
#83548 = ORIENTED_EDGE ( 'NONE', *, *, #134654, .F. ) ;
#83549 = VECTOR ( 'NONE', #56607, 1000.000000000000227 ) ;
#83550 = CARTESIAN_POINT ( 'NONE',  ( -21.32816939922338406, 11.25929247661560240, 4.000000000000000000 ) ) ;
#83551 = ORIENTED_EDGE ( 'NONE', *, *, #94880, .T. ) ;
#83552 = EDGE_CURVE ( 'NONE', #89048, #108692, #22627, .T. ) ;
#83553 = LINE ( 'NONE', #61126, #30624 ) ;
#83554 = UNCERTAINTY_MEASURE_WITH_UNIT (LENGTH_MEASURE( 1.000000000000000082E-05 ), #20034, 'distance_accuracy_value', 'NONE');
#83555 = EDGE_LOOP ( 'NONE', ( #114808, #134262, #108253, #44325 ) ) ;
#83556 = AXIS2_PLACEMENT_3D ( 'NONE', #38310, #25271, #69530 ) ;
#83557 = DIRECTION ( 'NONE',  ( 0.7071067811865486830, -0.7071067811865464625, -0.000000000000000000 ) ) ;
#83558 = FACE_BOUND ( 'NONE', #96339, .T. ) ;
#83559 = EDGE_CURVE ( 'NONE', #115805, #122150, #65497, .T. ) ;
#83560 = CARTESIAN_POINT ( 'NONE',  ( -17.99999999999986855, 10.55218569542905804, 5.000000000000000000 ) ) ;
#83561 = FACE_OUTER_BOUND ( 'NONE', #988, .T. ) ;
#83562 = DIRECTION ( 'NONE',  ( 0.7071067811865486830, -0.7071067811865464625, -0.000000000000000000 ) ) ;
#83563 = EDGE_LOOP ( 'NONE', ( #132433, #59590, #96502, #66791, #1134 ) ) ;
#83564 =( LENGTH_UNIT ( ) NAMED_UNIT ( * ) SI_UNIT ( .MILLI., .METRE. ) );
#83566 = ORIENTED_EDGE ( 'NONE', *, *, #14352, .F. ) ;
#83565 = DIRECTION ( 'NONE',  ( 0.7071067811865486830, -0.7071067811865464625, -0.000000000000000000 ) ) ;
#83567 = ORIENTED_EDGE ( 'NONE', *, *, #101946, .T. ) ;
#83568 = VECTOR ( 'NONE', #11761, 1000.000000000000000 ) ;
#83569 = CARTESIAN_POINT ( 'NONE',  ( 20.51159235450331764, 9.902892378096218942E-16, 0.000000000000000000 ) ) ;
#83570 = ORIENTED_EDGE ( 'NONE', *, *, #19857, .F. ) ;
#83571 = VERTEX_POINT ( 'NONE', #53134 ) ;
#83572 = CARTESIAN_POINT ( 'NONE',  ( 67.43293019189810877, 1.637169565754156508, 6.110000000000000320 ) ) ;
#83573 = ORIENTED_EDGE ( 'NONE', *, *, #53699, .T. ) ;
#83574 = CARTESIAN_POINT ( 'NONE',  ( 0.000000000000000000, 0.000000000000000000, 0.000000000000000000 ) ) ;
#83575 = FACE_OUTER_BOUND ( 'NONE', #69499, .T. ) ;
#83576 = ORIENTED_EDGE ( 'NONE', *, *, #58108, .T. ) ;
#83577 = VECTOR ( 'NONE', #2983, 1000.000000000000000 ) ;
#83578 = VECTOR ( 'NONE', #92446, 1000.000000000000000 ) ;
#83579 = VECTOR ( 'NONE', #126309, 1000.000000000000000 ) ;
#83580 = CARTESIAN_POINT ( 'NONE',  ( 34.97916666666665009, -7.950000000000000178, 2.130196079827424427 ) ) ;
#83581 = CARTESIAN_POINT ( 'NONE',  ( 101.7708333333333428, -7.949999999999998401, -2.130196079827426203 ) ) ;
#83582 = CARTESIAN_POINT ( 'NONE',  ( -12.69999999999998153, 0.000000000000000000, 0.000000000000000000 ) ) ;
#83583 = LINE ( 'NONE', #37201, #49331 ) ;
#83584 = EDGE_CURVE ( 'NONE', #80245, #13520, #87922, .T. ) ;
#83585 = ORIENTED_EDGE ( 'NONE', *, *, #125783, .T. ) ;
#83586 = AXIS2_PLACEMENT_3D ( 'NONE', #28522, #81490, #16917 ) ;
#83587 = VECTOR ( 'NONE', #28558, 999.9999999999998863 ) ;
#83588 = VECTOR ( 'NONE', #63504, 1000.000000000000000 ) ;
#83589 = VERTEX_POINT ( 'NONE', #53901 ) ;
#83590 = VECTOR ( 'NONE', #79651, 1000.000000000000000 ) ;
#83591 = CARTESIAN_POINT ( 'NONE',  ( -4.499999999999966249, -1.912538124160739095, 4.000000000000000000 ) ) ;
#83592 = FACE_OUTER_BOUND ( 'NONE', #96051, .T. ) ;
#83593 = EDGE_LOOP ( 'NONE', ( #86874, #142381, #133088, #127054 ) ) ;
#83594 = CIRCLE ( 'NONE', #106614, 2.500000000000000444 ) ;
#83595 = ORIENTED_EDGE ( 'NONE', *, *, #81534, .T. ) ;
#83596 = EDGE_LOOP ( 'NONE', ( #48389, #10960, #27957, #87258 ) ) ;
#83597 = LINE ( 'NONE', #28497, #23464 ) ;
#83598 = DIRECTION ( 'NONE',  ( 0.7071067811865486830, -0.7071067811865464625, -0.000000000000000000 ) ) ;
#83599 = EDGE_CURVE ( 'NONE', #58716, #88957, #87215, .T. ) ;
#83600 = DIRECTION ( 'NONE',  ( 0.7071067811865487940, 0.7071067811865463515, 0.000000000000000000 ) ) ;
#83601 = EDGE_LOOP ( 'NONE', ( #138451, #83945, #69318, #80514 ) ) ;
#83602 = VECTOR ( 'NONE', #42679, 1000.000000000000227 ) ;
#83603 = FACE_OUTER_BOUND ( 'NONE', #66315, .T. ) ;
#83605 = ADVANCED_FACE ( 'NONE', ( #111073 ), #110363, .F. ) ;
#83604 = FILL_AREA_STYLE_COLOUR ( '', #21478 ) ;
#83606 = ADVANCED_FACE ( 'NONE', ( #77081 ), #42306, .F. ) ;
#83607 = CARTESIAN_POINT ( 'NONE',  ( 7.067069808101886785, 2.126176841940952134, -7.934999999999993392 ) ) ;
#83608 = LINE ( 'NONE', #114063, #17103 ) ;
#83609 = EDGE_CURVE ( 'NONE', #139694, #105592, #10211, .T. ) ;
#83610 = VERTEX_POINT ( 'NONE', #158 ) ;
#83611 = DIRECTION ( 'NONE',  ( 0.3543493200069162685, -0.000000000000000000, -0.9351131265310288487 ) ) ;
#83612 = AXIS2_PLACEMENT_3D ( 'NONE', #97034, #107920, #99754 ) ;
#83613 = EDGE_CURVE ( 'NONE', #94785, #120961, #31412, .T. ) ;
#83614 = CARTESIAN_POINT ( 'NONE',  ( -28.22850677138647768, 20.25929247661551358, 7.808871592221704461 ) ) ;
#83615 = VECTOR ( 'NONE', #95016, 1000.000000000000000 ) ;
#83616 = CARTESIAN_POINT ( 'NONE',  ( 0.000000000000000000, 21.72500000000000142, 4.500000000000000888 ) ) ;
#83618 = ORIENTED_EDGE ( 'NONE', *, *, #138625, .T. ) ;
#83617 = CARTESIAN_POINT ( 'NONE',  ( 1.042387978378689573, -0.4000000000000003553, 2.015694669338588429 ) ) ;
#83619 = CARTESIAN_POINT ( 'NONE',  ( 10.49999999999993250, 10.46639925780215563, 5.000000000000000000 ) ) ;
#83620 = ORIENTED_EDGE ( 'NONE', *, *, #112271, .T. ) ;
#83621 = ADVANCED_FACE ( 'NONE', ( #108206 ), #64751, .T. ) ;
#83622 = LINE ( 'NONE', #127832, #135275 ) ;
#83623 = DIRECTION ( 'NONE',  ( -0.6830127018922180770, -0.6830127018922204085, -0.2588190451025213501 ) ) ;
#83624 = DIRECTION ( 'NONE',  ( 1.000000000000000000, 0.000000000000000000, 0.000000000000000000 ) ) ;
#83625 = ORIENTED_EDGE ( 'NONE', *, *, #24034, .F. ) ;
#83626 = AXIS2_PLACEMENT_3D ( 'NONE', #74271, #118462, #19162 ) ;
#83627 = EDGE_CURVE ( 'NONE', #142445, #88361, #86516, .T. ) ;
#83628 = VECTOR ( 'NONE', #100969, 1000.000000000000000 ) ;
#83630 = DIRECTION ( 'NONE',  ( 0.7071067811865487940, 0.7071067811865463515, 0.000000000000000000 ) ) ;
#83629 = AXIS2_PLACEMENT_3D ( 'NONE', #132630, #77524, #67353 ) ;
#83631 = DIRECTION ( 'NONE',  ( 0.000000000000000000, 0.000000000000000000, 1.000000000000000000 ) ) ;
#83632 = DIRECTION ( 'NONE',  ( 0.6830127018922180770, -0.6830127018922204085, -0.2588190451025213501 ) ) ;
#83633 = ORIENTED_EDGE ( 'NONE', *, *, #51685, .T. ) ;
#83634 = LINE ( 'NONE', #106032, #92455 ) ;
#83635 = VECTOR ( 'NONE', #39253, 1000.000000000000000 ) ;
#83636 = LINE ( 'NONE', #28527, #7611 ) ;
#83637 = CARTESIAN_POINT ( 'NONE',  ( 5.356812572482577472, -20.24070752338407786, 21.22881796311214231 ) ) ;
#83638 = EDGE_CURVE ( 'NONE', #67930, #11479, #43707, .T. ) ;
#83639 = CARTESIAN_POINT ( 'NONE',  ( -42.48921356237308800, -27.52281430457085065, 5.000000000000000000 ) ) ;
#83640 = CARTESIAN_POINT ( 'NONE',  ( 11.99999999999992539, -0.03360074219773377668, 5.000000000000000000 ) ) ;
#83641 = ORIENTED_EDGE ( 'NONE', *, *, #9914, .F. ) ;
#83642 = CIRCLE ( 'NONE', #95184, 4.000000000000000000 ) ;
#83643 = EDGE_LOOP ( 'NONE', ( #44701, #104279, #89422, #90913 ) ) ;
#83644 = CARTESIAN_POINT ( 'NONE',  ( -39.48921356237310221, -27.52281430457082934, 5.000000000000000000 ) ) ;
#83645 = CARTESIAN_POINT ( 'NONE',  ( 12.35051985313232237, 2.500000000000000444, 0.000000000000000000 ) ) ;
#83646 = EDGE_CURVE ( 'NONE', #63837, #100283, #41551, .T. ) ;
#83647 = CARTESIAN_POINT ( 'NONE',  ( 7.124569808101887780, -6.871911579029512218, 3.967499999999996252 ) ) ;
#83648 = DIRECTION ( 'NONE',  ( 0.8571673007021110013, 0.000000000000000000, 0.5150380749100563760 ) ) ;
#83649 = VECTOR ( 'NONE', #109658, 999.9999999999998863 ) ;
#83650 = DIRECTION ( 'NONE',  ( -0.7071067811865486830, -0.7071067811865464625, -0.000000000000000000 ) ) ;
#83651 = CARTESIAN_POINT ( 'NONE',  ( 34.42499999999998295, -13.45860074219782021, 5.000000000000000000 ) ) ;
#83652 = DIRECTION ( 'NONE',  ( -0.6830127018922180770, -0.6830127018922204085, -0.2588190451025213501 ) ) ;
#83653 = ORIENTED_EDGE ( 'NONE', *, *, #53172, .T. ) ;
#83654 = CARTESIAN_POINT ( 'NONE',  ( 36.48921356237310221, -27.52281430457080802, 5.000000000000000000 ) ) ;
#83655 = DIRECTION ( 'NONE',  ( -1.000000000000000000, -1.224606353822377258E-16, -0.000000000000000000 ) ) ;
#83656 = CIRCLE ( 'NONE', #78996, 2.055000000000001048 ) ;
#83657 = DIRECTION ( 'NONE',  ( -0.7071067811865487940, 0.7071067811865463515, 0.000000000000000000 ) ) ;
#83658 = VECTOR ( 'NONE', #122279, 1000.000000000000000 ) ;
#83659 = DIRECTION ( 'NONE',  ( 0.7071067811865487940, 0.7071067811865463515, 0.000000000000000000 ) ) ;
#83660 = CARTESIAN_POINT ( 'NONE',  ( 42.49543019189810877, 5.291415217122917625, 3.055000000000002380 ) ) ;
#83661 = LINE ( 'NONE', #47486, #55684 ) ;
#83662 = ORIENTED_EDGE ( 'NONE', *, *, #88385, .F. ) ;
#83663 = CARTESIAN_POINT ( 'NONE',  ( 5.068407645496677105, 2.500000000000000888, 3.061616997868383141E-16 ) ) ;
#83664 = ORIENTED_EDGE ( 'NONE', *, *, #70832, .T. ) ;
#83665 = VECTOR ( 'NONE', #120173, 1000.000000000000000 ) ;
#83666 = ADVANCED_FACE ( 'NONE', ( #121257 ), #97339, .T. ) ;
#83667 = ORIENTED_EDGE ( 'NONE', *, *, #78185, .F. ) ;
#83668 = VECTOR ( 'NONE', #97112, 1000.000000000000000 ) ;
#83669 = CARTESIAN_POINT ( 'NONE',  ( -1.499999999999994449, 8.900465351122148761, -2.516491619111509426 ) ) ;
#83670 = EDGE_CURVE ( 'NONE', #128517, #97084, #131439, .T. ) ;
#83671 = CARTESIAN_POINT ( 'NONE',  ( 60.48921356237309510, -27.52281430457097500, 5.000000000000000000 ) ) ;
#83672 = CARTESIAN_POINT ( 'NONE',  ( 11.15159235450332176, 9.902892378096218942E-16, 0.000000000000000000 ) ) ;
#83673 = CARTESIAN_POINT ( 'NONE',  ( -6.183988606268994381, 28.73617430169791476, 5.000000000000000000 ) ) ;
#83674 = LINE ( 'NONE', #5339, #48788 ) ;
#83675 = VERTEX_POINT ( 'NONE', #76344 ) ;
#83676 = PLANE ( 'NONE',  #88056 ) ;
#83677 = PLANE ( 'NONE',  #88548 ) ;
#83678 = UNCERTAINTY_MEASURE_WITH_UNIT (LENGTH_MEASURE( 1.000000000000000082E-05 ), #33804, 'distance_accuracy_value', 'NONE');
#83679 = VECTOR ( 'NONE', #11586, 1000.000000000000000 ) ;
#83680 = CARTESIAN_POINT ( 'NONE',  ( -3.489213562373097322, -27.52281430457057709, 5.000000000000000000 ) ) ;
#83681 = DIRECTION ( 'NONE',  ( -0.7071067811865486830, -0.7071067811865464625, 0.000000000000000000 ) ) ;
#83682 = EDGE_CURVE ( 'NONE', #98608, #137664, #120512, .T. ) ;
#83683 = DIRECTION ( 'NONE',  ( -0.000000000000000000, -0.3543493200069152693, 0.9351131265310292928 ) ) ;
#83684 = CARTESIAN_POINT ( 'NONE',  ( 61.62086038379622721, -6.884901960086286188, 3.974999999999997424 ) ) ;
#83685 = PLANE ( 'NONE',  #92271 ) ;
#83686 = VERTEX_POINT ( 'NONE', #11037 ) ;
#83687 = ORIENTED_EDGE ( 'NONE', *, *, #88675, .T. ) ;
#83688 = CARTESIAN_POINT ( 'NONE',  ( 64.14583333333334281, 2.130196079827431976, -7.949999999999999289 ) ) ;
#83689 = FACE_OUTER_BOUND ( 'NONE', #66264, .T. ) ;
#83690 = EDGE_CURVE ( 'NONE', #129163, #106470, #55313, .T. ) ;
#83691 = CARTESIAN_POINT ( 'NONE',  ( -81.29974487139159578, -27.71228299555262709, 4.000000000000000000 ) ) ;
#83692 = DIRECTION ( 'NONE',  ( -0.7071067811865486830, -0.7071067811865464625, 0.000000000000000000 ) ) ;
#83693 = ORIENTED_EDGE ( 'NONE', *, *, #126223, .F. ) ;
#83694 = VECTOR ( 'NONE', #141932, 1000.000000000000000 ) ;
#83695 = DIRECTION ( 'NONE',  ( -0.000000000000000000, 0.000000000000000000, 1.000000000000000000 ) ) ;
#83696 = VECTOR ( 'NONE', #54698, 1000.000000000000000 ) ;
#83697 = VECTOR ( 'NONE', #139555, 1000.000000000000000 ) ;
#83698 = CARTESIAN_POINT ( 'NONE',  ( -59.99451991528749772, 28.92564299267980132, 4.000000000000000000 ) ) ;
#83699 = CARTESIAN_POINT ( 'NONE',  ( 58.04209685856477563, 5.291415217122923842, -3.054999999999996163 ) ) ;
#83700 = DIRECTION ( 'NONE',  ( 0.000000000000000000, -1.000000000000000000, 0.000000000000000000 ) ) ;
#83701 = ORIENTED_EDGE ( 'NONE', *, *, #47947, .F. ) ;
#83703 = ORIENTED_EDGE ( 'NONE', *, *, #127688, .F. ) ;
#83702 = COLOUR_RGB ( '', 0.72549020, 0.75294118, 0.79215686) ;
#83704 = AXIS2_PLACEMENT_3D ( 'NONE', #37491, #114314, #14991 ) ;
#83705 = MECHANICAL_DESIGN_GEOMETRIC_PRESENTATION_REPRESENTATION (  '', ( #69843 ), #120695 ) ;
#83706 = AXIS2_PLACEMENT_3D ( 'NONE', #46283, #57868, #123109 ) ;
#83707 = LINE ( 'NONE', #94523, #141880 ) ;
#83709 = FACE_OUTER_BOUND ( 'NONE', #72339, .T. ) ;
#83708 = AXIS2_PLACEMENT_3D ( 'NONE', #79894, #24041, #36350 ) ;
#83710 = CARTESIAN_POINT ( 'NONE',  ( -34.42500000000001137, 11.97718569542929856, 5.000000000000000000 ) ) ;
#83711 = PLANE ( 'NONE',  #2327 ) ;
#83712 = EDGE_CURVE ( 'NONE', #93815, #101443, #115844, .T. ) ;
#83713 = LINE ( 'NONE', #85806, #129856 ) ;
#83715 = EDGE_LOOP ( 'NONE', ( #29710, #96247, #33593, #29528 ) ) ;
#83714 = DIRECTION ( 'NONE',  ( 0.7071067811865487940, 0.7071067811865463515, 0.000000000000000000 ) ) ;
#83716 = DIRECTION ( 'NONE',  ( 0.3543493200069162685, -0.000000000000000000, -0.9351131265310288487 ) ) ;
#83717 = DIRECTION ( 'NONE',  ( -0.000000000000000000, 0.000000000000000000, 1.000000000000000000 ) ) ;
#83718 = DIRECTION ( 'NONE',  ( -0.3543493200069162685, -0.000000000000000000, -0.9351131265310288487 ) ) ;
#83719 = VECTOR ( 'NONE', #32896, 1000.000000000000000 ) ;
#83720 = LINE ( 'NONE', #30004, #6733 ) ;
#83721 = ORIENTED_EDGE ( 'NONE', *, *, #132431, .F. ) ;
#83722 = EDGE_LOOP ( 'NONE', ( #66919, #126188, #10466, #6710 ) ) ;
#83723 = STYLED_ITEM ( 'NONE', ( #45418 ), #55317 ) ;
#83724 = DIRECTION ( 'NONE',  ( 0.7071067811865486830, -0.7071067811865464625, -0.000000000000000000 ) ) ;
#83725 = DIRECTION ( 'NONE',  ( -0.7071067811865487940, 0.7071067811865463515, 0.000000000000000000 ) ) ;
#83726 = CARTESIAN_POINT ( 'NONE',  ( 34.92499999999998295, -21.72500000000000142, 5.000000000000000000 ) ) ;
#83727 = LINE ( 'NONE', #16249, #36297 ) ;
#83728 = VERTEX_POINT ( 'NONE', #78487 ) ;
#83729 = ORIENTED_EDGE ( 'NONE', *, *, #102605, .T. ) ;
#83730 = FACE_OUTER_BOUND ( 'NONE', #113195, .T. ) ;
#83731 = DIRECTION ( 'NONE',  ( -1.000000000000000000, -1.224606353822377258E-16, -0.000000000000000000 ) ) ;
#83732 = ORIENTED_EDGE ( 'NONE', *, *, #66664, .T. ) ;
#83733 = EDGE_CURVE ( 'NONE', #98565, #114933, #79952, .T. ) ;
#83734 = VECTOR ( 'NONE', #19524, 1000.000000000000000 ) ;
#83735 = ORIENTED_EDGE ( 'NONE', *, *, #136119, .F. ) ;
#83736 = VECTOR ( 'NONE', #43399, 1000.000000000000000 ) ;
#83737 = ADVANCED_FACE ( 'NONE', ( #114655 ), #1592, .F. ) ;
#83738 = DIRECTION ( 'NONE',  ( 0.3543493200069162685, -0.000000000000000000, -0.9351131265310288487 ) ) ;
#83739 = ORIENTED_EDGE ( 'NONE', *, *, #52063, .T. ) ;
#83740 = AXIS2_PLACEMENT_3D ( 'NONE', #17578, #93022, #1848 ) ;
#83741 = LINE ( 'NONE', #129334, #78121 ) ;
#83742 = DIRECTION ( 'NONE',  ( -0.000000000000000000, 0.000000000000000000, 1.000000000000000000 ) ) ;
#83743 = AXIS2_PLACEMENT_3D ( 'NONE', #3548, #15832, #60129 ) ;
#83744 = FACE_BOUND ( 'NONE', #53521, .T. ) ;
#83745 = AXIS2_PLACEMENT_3D ( 'NONE', #25686, #36565, #80810 ) ;
#83746 = EDGE_CURVE ( 'NONE', #61121, #137089, #3726, .T. ) ;
#83747 = CARTESIAN_POINT ( 'NONE',  ( 3.707013264293012256, -21.74070752338405654, 4.999753212805217117 ) ) ;
#83749 = ORIENTED_EDGE ( 'NONE', *, *, #28317, .T. ) ;
#83748 = LINE ( 'NONE', #61984, #52817 ) ;
#83750 = DIRECTION ( 'NONE',  ( -0.7071067811865487940, 0.7071067811865463515, 0.000000000000000000 ) ) ;
#83751 = SHAPE_DEFINITION_REPRESENTATION ( #65226, #118114 ) ;
#83752 = ORIENTED_EDGE ( 'NONE', *, *, #22610, .T. ) ;
#83753 = ORIENTED_EDGE ( 'NONE', *, *, #27667, .F. ) ;
#83754 = CARTESIAN_POINT ( 'NONE',  ( 90.32876352523145158, 0.000000000000000000, -6.109999999999998543 ) ) ;
#83755 = ORIENTED_EDGE ( 'NONE', *, *, #59592, .T. ) ;
#83756 = DIRECTION ( 'NONE',  ( 0.6830127018922180770, -0.6830127018922204085, -0.2588190451025213501 ) ) ;
#83757 = VECTOR ( 'NONE', #79811, 999.9999999999998863 ) ;
#83758 = CARTESIAN_POINT ( 'NONE',  ( 34.92499999999998295, 17.56110451772265080, 6.767324343803300835 ) ) ;
#83759 = VECTOR ( 'NONE', #95014, 1000.000000000000000 ) ;
#83760 = CARTESIAN_POINT ( 'NONE',  ( 8.994519915287490619, 28.92564299267944250, 4.000000000000000000 ) ) ;
#83761 = DIRECTION ( 'NONE',  ( -0.000000000000000000, -0.3543493200069153803, -0.9351131265310292928 ) ) ;
#83762 = ORIENTED_EDGE ( 'NONE', *, *, #86994, .F. ) ;
#83763 = CARTESIAN_POINT ( 'NONE',  ( 30.29974487139158867, -27.71228299555227537, 4.000000000000000000 ) ) ;
#83764 = LINE ( 'NONE', #127974, #52399 ) ;
#83765 = LINE ( 'NONE', #138116, #45812 ) ;
#83766 = AXIS2_PLACEMENT_3D ( 'NONE', #25252, #113694, #14386 ) ;
#83767 = PLANE ( 'NONE',  #119100 ) ;
#83768 = CARTESIAN_POINT ( 'NONE',  ( 21.48921356237309155, -27.52281430457070499, 5.000000000000000000 ) ) ;
#83769 = CARTESIAN_POINT ( 'NONE',  ( 180.4193221990229574, -49.14999999999999147, -40.92499999999998295 ) ) ;
#83770 = AXIS2_PLACEMENT_3D ( 'NONE', #96572, #107485, #40815 ) ;
#83771 = CARTESIAN_POINT ( 'NONE',  ( -34.92500000000001137, -9.183345613589475320, 4.500000000000000888 ) ) ;
#83772 = ORIENTED_EDGE ( 'NONE', *, *, #92454, .F. ) ;
#83773 = FACE_OUTER_BOUND ( 'NONE', #40743, .T. ) ;
#83774 = ORIENTED_EDGE ( 'NONE', *, *, #70004, .T. ) ;
#83775 = ORIENTED_EDGE ( 'NONE', *, *, #106858, .F. ) ;
#83776 = VERTEX_POINT ( 'NONE', #122682 ) ;
#83777 = CARTESIAN_POINT ( 'NONE',  ( 49.00043019189810423, -3.055000000000002380, 5.291415217122920289 ) ) ;
#83778 = AXIS2_PLACEMENT_3D ( 'NONE', #69982, #133084, #80132 ) ;
#83779 = EDGE_LOOP ( 'NONE', ( #72747, #72372, #61735, #131002 ) ) ;
#83780 = EDGE_CURVE ( 'NONE', #10035, #27758, #111832, .T. ) ;
#83781 = CARTESIAN_POINT ( 'NONE',  ( 17.25413961620377279, 3.047499999999993214, -5.278424836066146320 ) ) ;
#83782 = CARTESIAN_POINT ( 'NONE',  ( -6.713483559403754519, 11.28174313718248634, -26.16288089844056941 ) ) ;
#83783 = ADVANCED_FACE ( 'NONE', ( #135039 ), #37109, .F. ) ;
#83784 = ORIENTED_EDGE ( 'NONE', *, *, #137941, .F. ) ;
#83785 = EDGE_CURVE ( 'NONE', #115183, #115678, #112532, .T. ) ;
#83786 = LINE ( 'NONE', #40967, #139731 ) ;
#83788 = ORIENTED_EDGE ( 'NONE', *, *, #91600, .F. ) ;
#83787 = ADVANCED_FACE ( 'NONE', ( #81365 ), #134301, .F. ) ;
#83789 = DIRECTION ( 'NONE',  ( -0.3543493200069162685, -0.000000000000000000, -0.9351131265310288487 ) ) ;
#83790 = PLANE ( 'NONE',  #130820 ) ;
#83791 = CONICAL_SURFACE ( 'NONE', #18976, 2.500000000000000888, 0.9599310885968822538 ) ;
#83793 = EDGE_LOOP ( 'NONE', ( #140969, #117044, #71070, #14546 ) ) ;
#83792 = DIRECTION ( 'NONE',  ( 0.7071067811865487940, -0.7071067811865463515, 0.000000000000000000 ) ) ;
#83794 = EDGE_LOOP ( 'NONE', ( #103630, #29780, #42878, #128319 ) ) ;
#83795 = EDGE_CURVE ( 'NONE', #33310, #23228, #56775, .T. ) ;
#83796 = CARTESIAN_POINT ( 'NONE',  ( -36.48921356237310221, -27.52281430457080802, 5.000000000000000000 ) ) ;
#83797 = DIRECTION ( 'NONE',  ( -1.000000000000000000, -0.000000000000000000, -0.000000000000000000 ) ) ;
#83798 = PRESENTATION_LAYER_ASSIGNMENT (  '', '', ( #30591 ) ) ;
#83800 = VERTEX_POINT ( 'NONE', #59609 ) ;
#83799 = VECTOR ( 'NONE', #115406, 1000.000000000000227 ) ;
#83801 = FACE_OUTER_BOUND ( 'NONE', #98670, .T. ) ;
#83802 = ORIENTED_EDGE ( 'NONE', *, *, #10470, .F. ) ;
#83803 = ORIENTED_EDGE ( 'NONE', *, *, #15131, .F. ) ;
#83804 = ORIENTED_EDGE ( 'NONE', *, *, #126486, .T. ) ;
#83805 = EDGE_CURVE ( 'NONE', #20628, #35756, #35000, .T. ) ;
#83806 = EDGE_LOOP ( 'NONE', ( #97768, #38186, #91854, #117590 ) ) ;
#83807 = CARTESIAN_POINT ( 'NONE',  ( -42.29974487139158157, -27.71228299555235708, 4.000000000000000000 ) ) ;
#83808 = VECTOR ( 'NONE', #124310, 1000.000000000000227 ) ;
#83809 = VECTOR ( 'NONE', #29471, 1000.000000000000000 ) ;
#83810 = LINE ( 'NONE', #128018, #56219 ) ;
#83811 = EDGE_CURVE ( 'NONE', #65370, #24066, #45876, .T. ) ;
#83812 = CARTESIAN_POINT ( 'NONE',  ( 25.49999999999982236, 4.087461875839204062, 4.000000000000000000 ) ) ;
#83813 = LINE ( 'NONE', #104066, #20829 ) ;
#83814 = ADVANCED_FACE ( 'NONE', ( #124835 ), #90803, .F. ) ;
#83815 = ORIENTED_EDGE ( 'NONE', *, *, #120004, .T. ) ;
#83816 = CARTESIAN_POINT ( 'NONE',  ( 0.3281693992235289459, 14.25929247661556687, 4.000000000000000000 ) ) ;
#83817 = VERTEX_POINT ( 'NONE', #57466 ) ;
#83818 = CARTESIAN_POINT ( 'NONE',  ( -20.99999999999985079, -19.22509904557638549, 1.855685503482130239 ) ) ;
#83819 = EDGE_CURVE ( 'NONE', #52354, #105598, #25894, .T. ) ;
#83820 = CARTESIAN_POINT ( 'NONE',  ( 28.56206980810188512, -7.934999999999991616, -2.126176841940955242 ) ) ;
#83821 = CARTESIAN_POINT ( 'NONE',  ( 11.20710678118647330, -5.240707523384234179, 5.000000000000000000 ) ) ;
#83822 = LINE ( 'NONE', #114938, #94625 ) ;
#83823 = CARTESIAN_POINT ( 'NONE',  ( 0.000000000000000000, 0.000000000000000000, 5.000000000000000000 ) ) ;
#83824 = ORIENTED_EDGE ( 'NONE', *, *, #90182, .T. ) ;
#83825 = ORIENTED_EDGE ( 'NONE', *, *, #77518, .T. ) ;
#83826 = ORIENTED_EDGE ( 'NONE', *, *, #136469, .F. ) ;
#83827 = DIRECTION ( 'NONE',  ( -0.000000000000000000, -0.3543493200069152693, 0.9351131265310292928 ) ) ;
#83828 = FACE_OUTER_BOUND ( 'NONE', #78075, .T. ) ;
#83829 = UNCERTAINTY_MEASURE_WITH_UNIT (LENGTH_MEASURE( 1.000000000000000082E-05 ), #131855, 'distance_accuracy_value', 'NONE');
#83830 = DIRECTION ( 'NONE',  ( 0.7071067811865487940, 0.7071067811865463515, 0.000000000000000000 ) ) ;
#83831 = CARTESIAN_POINT ( 'NONE',  ( -3.328169399223503966, -6.740707523384211086, 4.000000000000000000 ) ) ;
#83832 = PRESENTATION_STYLE_ASSIGNMENT (( #46207 ) ) ;
#83833 = CARTESIAN_POINT ( 'NONE',  ( 76.47459685856476597, 1.637169565754164280, -6.109999999999997655 ) ) ;
#83834 = VECTOR ( 'NONE', #93353, 999.9999999999998863 ) ;
#83835 = DIRECTION ( 'NONE',  ( -1.000000000000000000, -1.224606353822377258E-16, -0.000000000000000000 ) ) ;
#83836 = AXIS2_PLACEMENT_3D ( 'NONE', #101877, #12719, #103291 ) ;
#83837 = DIRECTION ( 'NONE',  ( 0.7071067811865487940, 0.7071067811865463515, 0.000000000000000000 ) ) ;
#83838 = PLANE ( 'NONE',  #8419 ) ;
#83839 = FACE_OUTER_BOUND ( 'NONE', #142568, .T. ) ;
#83840 = AXIS2_PLACEMENT_3D ( 'NONE', #114422, #136893, #16519 ) ;
#83841 = FACE_OUTER_BOUND ( 'NONE', #66148, .T. ) ;
#83842 = EDGE_CURVE ( 'NONE', #17057, #20345, #24802, .T. ) ;
#83843 = ORIENTED_EDGE ( 'NONE', *, *, #116569, .T. ) ;
#83845 = VECTOR ( 'NONE', #49085, 1000.000000000000000 ) ;
#83844 = DIRECTION ( 'NONE',  ( -0.7071067811865486830, -0.7071067811865464625, 0.000000000000000000 ) ) ;
#83846 = EDGE_LOOP ( 'NONE', ( #133704, #97601, #123561, #117048, #112998, #14922 ) ) ;
#83847 = DIRECTION ( 'NONE',  ( 0.7071067811865487940, -0.7071067811865463515, 0.000000000000000000 ) ) ;
#83849 = ORIENTED_EDGE ( 'NONE', *, *, #9729, .F. ) ;
#83848 = PLANE ( 'NONE',  #44151 ) ;
#83850 = CARTESIAN_POINT ( 'NONE',  ( -23.99999999999983302, 10.55218569542905982, 5.000000000000000000 ) ) ;
#83851 = LINE ( 'NONE', #6915, #100494 ) ;
#83852 = ORIENTED_EDGE ( 'NONE', *, *, #108336, .F. ) ;
#83853 = ORIENTED_EDGE ( 'NONE', *, *, #38611, .F. ) ;
#83854 = CARTESIAN_POINT ( 'NONE',  ( 34.92499999999998295, -11.29530194282807365, 17.70209546082494967 ) ) ;
#83855 = PRESENTATION_STYLE_ASSIGNMENT (( #127311 ) ) ;
#83856 = VECTOR ( 'NONE', #64839, 1000.000000000000000 ) ;
#83857 = DIRECTION ( 'NONE',  ( 0.000000000000000000, 0.3543493200069153248, 0.9351131265310291818 ) ) ;
#83858 = EDGE_CURVE ( 'NONE', #62399, #11393, #113231, .T. ) ;
#83859 = CARTESIAN_POINT ( 'NONE',  ( 97.93336038379622721, 2.130196079827431532, -7.949999999999997513 ) ) ;
#83860 = LINE ( 'NONE', #137500, #101891 ) ;
#83861 = DIRECTION ( 'NONE',  ( -0.000000000000000000, -0.000000000000000000, -1.000000000000000000 ) ) ;
#83862 = ORIENTED_EDGE ( 'NONE', *, *, #61906, .T. ) ;
#83863 = LINE ( 'NONE', #51930, #141804 ) ;
#83864 = ADVANCED_FACE ( 'NONE', ( #103091 ), #100934, .F. ) ;
#83865 = LINE ( 'NONE', #51213, #32307 ) ;
#83867 = VECTOR ( 'NONE', #27324, 1000.000000000000000 ) ;
#83866 = CARTESIAN_POINT ( 'NONE',  ( 34.12500000000000000, 6.094999999999989981, -1.119633336120465690E-15 ) ) ;
#83869 = AXIS2_PLACEMENT_3D ( 'NONE', #71705, #4215, #126762 ) ;
#83868 = LINE ( 'NONE', #62818, #11974 ) ;
#83870 = ORIENTED_EDGE ( 'NONE', *, *, #76935, .F. ) ;
#83871 = CARTESIAN_POINT ( 'NONE',  ( 46.45419371712955581, 6.884901960086283523, 3.975000000000002753 ) ) ;
#83872 = ORIENTED_EDGE ( 'NONE', *, *, #97259, .T. ) ;
#83873 = EDGE_CURVE ( 'NONE', #74043, #57414, #48745, .T. ) ;
#83874 = CARTESIAN_POINT ( 'NONE',  ( 86.91709685856477563, 3.054999999999998828, 5.291415217122922066 ) ) ;
#83875 = CARTESIAN_POINT ( 'NONE',  ( -26.99999999999980460, -4.447814304570781196, 5.000000000000000000 ) ) ;
#83877 = AXIS2_PLACEMENT_3D ( 'NONE', #37806, #4364, #15276 ) ;
#83876 = CARTESIAN_POINT ( 'NONE',  ( 1.179999999999999272, 9.043340090917736163, 10.00000000000000000 ) ) ;
#83878 = DIRECTION ( 'NONE',  ( -0.000000000000000000, 0.3543493200069153248, 0.9351131265310292928 ) ) ;
#83879 = EDGE_LOOP ( 'NONE', ( #22823, #33263, #103902, #6493 ) ) ;
#83880 = DIRECTION ( 'NONE',  ( -0.7071067811865486830, -0.7071067811865464625, 0.000000000000000000 ) ) ;
#83881 = CARTESIAN_POINT ( 'NONE',  ( 32.99999999999976552, -1.068876922607802538, 4.000000000000000000 ) ) ;
#83882 = DIRECTION ( 'NONE',  ( 0.7071067811865487940, -0.7071067811865463515, 0.000000000000000000 ) ) ;
#83883 = EDGE_CURVE ( 'NONE', #127446, #105971, #117501, .T. ) ;
#83885 = EDGE_LOOP ( 'NONE', ( #136130, #110417, #89758, #7846, #109474 ) ) ;
#83884 = CARTESIAN_POINT ( 'NONE',  ( -14.54487008052910824, -0.7407075233842735917, 4.335043535661659675 ) ) ;
#83886 = CARTESIAN_POINT ( 'NONE',  ( 6.489213562373093325, -27.52281430457059841, 5.000000000000000000 ) ) ;
#83887 = CARTESIAN_POINT ( 'NONE',  ( -14.11732500641695509, -0.1862019290248694003, 4.000000000000000000 ) ) ;
#83888 = VECTOR ( 'NONE', #134307, 1000.000000000000000 ) ;
#83889 = CYLINDRICAL_SURFACE ( 'NONE', #91111, 6.094999999999989093 ) ;
#83890 = PRESENTATION_STYLE_ASSIGNMENT (( #117169 ) ) ;
#83891 = ORIENTED_EDGE ( 'NONE', *, *, #49665, .F. ) ;
#83892 = EDGE_LOOP ( 'NONE', ( #86533, #136899, #65396, #129210 ) ) ;
#83893 = CARTESIAN_POINT ( 'NONE',  ( 69.70876352523144703, -7.482591942790329030E-16, 6.110000000000001208 ) ) ;
#83894 = VERTEX_POINT ( 'NONE', #105222 ) ;
#83895 = PLANE ( 'NONE',  #5813 ) ;
#83896 = DIRECTION ( 'NONE',  ( 0.7071067811865486830, -0.7071067811865464625, -0.000000000000000000 ) ) ;
#83897 = DIRECTION ( 'NONE',  ( 0.3543493200069162685, -0.000000000000000000, -0.9351131265310288487 ) ) ;
#83898 = ORIENTED_EDGE ( 'NONE', *, *, #81520, .T. ) ;
#83899 = AXIS2_PLACEMENT_3D ( 'NONE', #16937, #93783, #60473 ) ;
#83900 = AXIS2_PLACEMENT_3D ( 'NONE', #31541, #103533, #42443 ) ;
#83901 = VECTOR ( 'NONE', #25203, 999.9999999999998863 ) ;
#83902 = CARTESIAN_POINT ( 'NONE',  ( -3.411614905948293863, 22.22500000000000142, 4.777194822843814137 ) ) ;
#83904 =( BOUNDED_CURVE ( )  B_SPLINE_CURVE ( 2, ( #50572, #6291, #84632, #138300, #140427, #71621, #18623, #83204, #127405, #95488, #128150, #73070, #51300 ),
 .UNSPECIFIED., .F., .F. ) 
 B_SPLINE_CURVE_WITH_KNOTS ( ( 3, 2, 2, 2, 2, 2, 3 ),
 ( 0.4000000000000001332, 0.4083333333333334370, 0.4166666666666667407, 0.4250000000000000444, 0.4333333333333334036, 0.4416666666666666519, 0.4500000000000000111 ),
 .UNSPECIFIED. ) 
 CURVE ( )  GEOMETRIC_REPRESENTATION_ITEM ( )  RATIONAL_B_SPLINE_CURVE ( ( 0.9999999999999995559, 0.9659258262890687563, 1.000000000000000000, 0.9659258262890683122, 1.000000000000000000, 0.9659258262890683122, 1.000000000000000000, 0.9659258262890683122, 1.000000000000000000, 0.9659258262890683122, 1.000000000000000000, 0.9659258262890683122, 1.000000000000000000 ) ) 
 REPRESENTATION_ITEM ( '' )  );
#83903 = CARTESIAN_POINT ( 'NONE',  ( 34.92499999999998295, -6.791953661863733949, 15.99560845316868729 ) ) ;
#83905 = AXIS2_PLACEMENT_3D ( 'NONE', #35119, #79362, #101768 ) ;
#83906 = VECTOR ( 'NONE', #120979, 1000.000000000000000 ) ;
#83907 = EDGE_LOOP ( 'NONE', ( #11720, #53820, #129370, #133942 ) ) ;
#83908 = EDGE_CURVE ( 'NONE', #113319, #132165, #6576, .T. ) ;
#83909 = EDGE_CURVE ( 'NONE', #133316, #96308, #37854, .T. ) ;
#83910 = CARTESIAN_POINT ( 'NONE',  ( -66.18398860626901126, 28.73617430169833753, 5.000000000000000000 ) ) ;
#83912 = CARTESIAN_POINT ( 'NONE',  ( -53.99451991528749062, 28.92564299267975869, 4.000000000000000000 ) ) ;
#83911 = VECTOR ( 'NONE', #115365, 1000.000000000000000 ) ;
#83913 = FACE_OUTER_BOUND ( 'NONE', #6470, .T. ) ;
#83914 = VECTOR ( 'NONE', #49629, 1000.000000000000000 ) ;
#83915 = STYLED_ITEM ( 'NONE', ( #94551 ), #143506 ) ;
#83916 = VERTEX_POINT ( 'NONE', #50852 ) ;
#83917 = ORIENTED_EDGE ( 'NONE', *, *, #85963, .F. ) ;
#83918 = ADVANCED_FACE ( 'NONE', ( #116811 ), #128420, .F. ) ;
#83919 = EDGE_CURVE ( 'NONE', #15581, #116374, #93647, .T. ) ;
#83920 = CARTESIAN_POINT ( 'NONE',  ( 5.700255128608413102, -27.71228299555201957, 4.000000000000000000 ) ) ;
#83921 = DIRECTION ( 'NONE',  ( 0.6830127018922180770, -0.6830127018922204085, -0.2588190451025213501 ) ) ;
#83922 = CARTESIAN_POINT ( 'NONE',  ( 38.99451991528749062, 28.92564299267965211, 4.000000000000000000 ) ) ;
#83923 = CARTESIAN_POINT ( 'NONE',  ( 0.7928932188134545367, -17.24070752338410628, 5.000000000000000000 ) ) ;
#83924 = CARTESIAN_POINT ( 'NONE',  ( 53.16252705046288440, 7.949999999999998401, 1.460391307983218338E-15 ) ) ;
#83925 = PLANE ( 'NONE',  #132285 ) ;
#83926 = VERTEX_POINT ( 'NONE', #140020 ) ;
#83927 = ORIENTED_EDGE ( 'NONE', *, *, #61906, .F. ) ;
#83928 = ORIENTED_EDGE ( 'NONE', *, *, #134742, .T. ) ;
#83929 = EDGE_LOOP ( 'NONE', ( #140200, #47778, #87332, #42150 ) ) ;
#83930 = EDGE_CURVE ( 'NONE', #119756, #121984, #7315, .T. ) ;
#83931 =( GEOMETRIC_REPRESENTATION_CONTEXT ( 3 ) GLOBAL_UNCERTAINTY_ASSIGNED_CONTEXT ( ( #125742 ) ) GLOBAL_UNIT_ASSIGNED_CONTEXT ( ( #130108, #8277, #64132 ) ) REPRESENTATION_CONTEXT ( 'NONE', 'WORKASPACE' ) );
#83932 = CARTESIAN_POINT ( 'NONE',  ( 25.39999999999999858, 1.399999999999986366, 20.40202195861970580 ) ) ;
#83933 = CARTESIAN_POINT ( 'NONE',  ( 20.99999999999985789, -13.97847968911258221, -0.1324546996126314546 ) ) ;
#83934 = ORIENTED_EDGE ( 'NONE', *, *, #128759, .F. ) ;
#83935 = LINE ( 'NONE', #27350, #41335 ) ;
#83936 = CARTESIAN_POINT ( 'NONE',  ( -7.499999999999951150, -4.216083040037264418, -7.486842126848642032 ) ) ;
#83937 = COLOUR_RGB ( '', 0.09019608, 0.27058824, 0.51372549) ;
#83938 = DIRECTION ( 'NONE',  ( 0.000000000000000000, 0.000000000000000000, 1.000000000000000000 ) ) ;
#83939 = CARTESIAN_POINT ( 'NONE',  ( 12.19999999999999574, -40.43000000000000682, 19.06900128115122683 ) ) ;
#83940 = AXIS2_PLACEMENT_3D ( 'NONE', #73865, #105742, #106447 ) ;
#83941 = FACE_OUTER_BOUND ( 'NONE', #54677, .T. ) ;
#83942 = VERTEX_POINT ( 'NONE', #137876 ) ;
#83943 = CARTESIAN_POINT ( 'NONE',  ( 66.29974487139159578, -27.71228299555252406, 4.000000000000000000 ) ) ;
#83944 = PLANE ( 'NONE',  #122886 ) ;
#83945 = ORIENTED_EDGE ( 'NONE', *, *, #52650, .F. ) ;
#83946 = CARTESIAN_POINT ( 'NONE',  ( -31.49999999999977973, -6.839392718269155402, -8.480912228396011443 ) ) ;
#83947 = EDGE_LOOP ( 'NONE', ( #136213, #93480, #14821, #54676 ) ) ;
#83948 = FACE_OUTER_BOUND ( 'NONE', #113922, .T. ) ;
#83949 = VERTEX_POINT ( 'NONE', #48714 ) ;
#83950 = EDGE_LOOP ( 'NONE', ( #12787, #46144, #70646, #108135, #92079 ) ) ;
#83951 = CARTESIAN_POINT ( 'NONE',  ( 68.68793019189809002, 6.110000000000002984, -1.637169565754156730 ) ) ;
#83952 = EDGE_LOOP ( 'NONE', ( #5056, #38272, #140010, #34727 ) ) ;
#83953 =( LENGTH_UNIT ( ) NAMED_UNIT ( * ) SI_UNIT ( .MILLI., .METRE. ) );
#83954 = EDGE_CURVE ( 'NONE', #22463, #76469, #92920, .T. ) ;
#83955 = DIRECTION ( 'NONE',  ( -0.000000000000000000, 0.000000000000000000, 1.000000000000000000 ) ) ;
#83956 = CARTESIAN_POINT ( 'NONE',  ( 105.2920968585647756, -5.291415217122921177, 3.054999999999999272 ) ) ;
#83957 = CARTESIAN_POINT ( 'NONE',  ( 7.980122250714476451, -17.24070752338410273, 20.23474786156470984 ) ) ;
#83958 = EDGE_CURVE ( 'NONE', #117563, #83102, #86015, .T. ) ;
#83960 = CARTESIAN_POINT ( 'NONE',  ( 8.445142094776647568, 22.22500000000000142, -11.43456810075855756 ) ) ;
#83959 = CIRCLE ( 'NONE', #81580, 0.5000000000000000000 ) ;
#83961 = CARTESIAN_POINT ( 'NONE',  ( 16.61159235450331906, 3.061616997868375253E-16, -2.500000000000001332 ) ) ;
#83962 = DIRECTION ( 'NONE',  ( 0.7071067811865486830, -0.7071067811865464625, -0.000000000000000000 ) ) ;
#83963 = VECTOR ( 'NONE', #74399, 1000.000000000000000 ) ;
#83964 = CARTESIAN_POINT ( 'NONE',  ( -33.48921356237309510, -27.52281430457078670, 5.000000000000000000 ) ) ;
#83965 = EDGE_CURVE ( 'NONE', #81560, #1788, #129113, .T. ) ;
#83966 = EDGE_CURVE ( 'NONE', #112039, #118417, #16786, .T. ) ;
#83967 = CARTESIAN_POINT ( 'NONE',  ( 24.79289321881329045, -20.24070752338406720, 5.000000000000000000 ) ) ;
#83968 = CARTESIAN_POINT ( 'NONE',  ( 6.471592354503322042, 9.902892378096218942E-16, 0.000000000000000000 ) ) ;
#83969 = ORIENTED_EDGE ( 'NONE', *, *, #70080, .T. ) ;
#83970 = DIRECTION ( 'NONE',  ( 0.7071067811865487940, 0.7071067811865463515, -0.000000000000000000 ) ) ;
#83971 = EDGE_LOOP ( 'NONE', ( #112861, #115918, #135658, #41815 ) ) ;
#83972 = ORIENTED_EDGE ( 'NONE', *, *, #128746, .F. ) ;
#83973 = CARTESIAN_POINT ( 'NONE',  ( 1.500000000000000000, 9.797174393178827630E-16, 8.000000000000001776 ) ) ;
#83975 = ORIENTED_EDGE ( 'NONE', *, *, #71713, .T. ) ;
#83974 = AXIS2_PLACEMENT_3D ( 'NONE', #141264, #30372, #40556 ) ;
#83976 = CARTESIAN_POINT ( 'NONE',  ( -20.91685193227056416, 21.75929247661549226, 7.311836541448005100 ) ) ;
#83977 = DIRECTION ( 'NONE',  ( -0.3543493200069162685, -0.000000000000000000, -0.9351131265310288487 ) ) ;
#83978 = EDGE_CURVE ( 'NONE', #49830, #139177, #95075, .T. ) ;
#83979 = CARTESIAN_POINT ( 'NONE',  ( -11.81601139373100651, 28.73617430169779041, 5.000000000000000000 ) ) ;
#83980 = EDGE_CURVE ( 'NONE', #132883, #126576, #14342, .T. ) ;
#83981 = CARTESIAN_POINT ( 'NONE',  ( 16.40633728939539537, -22.22500000000000142, 24.45136256510390993 ) ) ;
#83982 = ORIENTED_EDGE ( 'NONE', *, *, #46314, .F. ) ;
#83983 = DIRECTION ( 'NONE',  ( -1.000000000000000000, -1.224606353822377258E-16, -0.000000000000000000 ) ) ;
#83984 = CONICAL_SURFACE ( 'NONE', #132627, 2.055000000000000604, 0.9599310885968764806 ) ;
#83985 = ORIENTED_EDGE ( 'NONE', *, *, #142388, .F. ) ;
#83986 = EDGE_CURVE ( 'NONE', #132252, #33283, #129835, .T. ) ;
#83987 = CARTESIAN_POINT ( 'NONE',  ( 7.124569808101886892, -6.871911579029512218, 3.967499999999996252 ) ) ;
#83988 = CARTESIAN_POINT ( 'NONE',  ( 23.99999999999985079, 17.96639925780208458, 5.000000000000000000 ) ) ;
#83989 = CARTESIAN_POINT ( 'NONE',  ( 4.499999999999972466, -17.56887692260763956, 4.000000000000000000 ) ) ;
#83990 = CARTESIAN_POINT ( 'NONE',  ( 13.61880637382470383, -9.051169013344379621, 2.893211955101936628 ) ) ;
#83991 = VERTEX_POINT ( 'NONE', #19641 ) ;
#83992 = ORIENTED_EDGE ( 'NONE', *, *, #67634, .T. ) ;
#83993 = VERTEX_POINT ( 'NONE', #98622 ) ;
#83994 = CARTESIAN_POINT ( 'NONE',  ( -59.99451991528749772, 28.92564299267980132, 4.000000000000000000 ) ) ;
#83995 = LINE ( 'NONE', #120116, #85727 ) ;
#83996 = ADVANCED_FACE ( 'NONE', ( #119638 ), #63884, .F. ) ;
#83998 = LINE ( 'NONE', #138347, #100591 ) ;
#83997 = VECTOR ( 'NONE', #23317, 1000.000000000000000 ) ;
#83999 = AXIS2_PLACEMENT_3D ( 'NONE', #38241, #5580, #30771 ) ;
#84000 = LINE ( 'NONE', #17950, #72778 ) ;
#84001 = CARTESIAN_POINT ( 'NONE',  ( -29.29289321881324781, 14.25929247661556865, 5.000000000000000000 ) ) ;
#84002 = VECTOR ( 'NONE', #5823, 1000.000000000000000 ) ;
#84003 = DIRECTION ( 'NONE',  ( 0.7071067811865487940, 0.7071067811865463515, 0.000000000000000000 ) ) ;
#84004 = VECTOR ( 'NONE', #29874, 1000.000000000000227 ) ;
#84005 = LINE ( 'NONE', #49931, #55585 ) ;
#84006 = DIRECTION ( 'NONE',  ( -0.7071067811865487940, 0.7071067811865463515, -0.000000000000000000 ) ) ;
#84007 = ORIENTED_EDGE ( 'NONE', *, *, #15900, .F. ) ;
#84008 = CARTESIAN_POINT ( 'NONE',  ( 72.89583333333331439, -2.130196079827427091, 7.949999999999998401 ) ) ;
#84009 = AXIS2_PLACEMENT_3D ( 'NONE', #140119, #7419, #127073 ) ;
#84010 = EDGE_CURVE ( 'NONE', #111700, #122429, #142164, .T. ) ;
#84011 = FACE_OUTER_BOUND ( 'NONE', #116100, .T. ) ;
#84012 = ORIENTED_EDGE ( 'NONE', *, *, #130289, .F. ) ;
#84013 = FACE_OUTER_BOUND ( 'NONE', #46099, .T. ) ;
#84015 = VERTEX_POINT ( 'NONE', #52268 ) ;
#84014 = CARTESIAN_POINT ( 'NONE',  ( 55.95337363913751716, -51.41954113333837739, -38.53170190052302502 ) ) ;
#84016 = DIRECTION ( 'NONE',  ( 0.7071067811865487940, 0.7071067811865463515, 0.000000000000000000 ) ) ;
#84017 = ADVANCED_FACE ( 'NONE', ( #74899 ), #42850, .T. ) ;
#84019 = EDGE_CURVE ( 'NONE', #42322, #34870, #25637, .T. ) ;
#84018 = LINE ( 'NONE', #128215, #11428 ) ;
#84020 = ORIENTED_EDGE ( 'NONE', *, *, #3667, .F. ) ;
#84021 = UNCERTAINTY_MEASURE_WITH_UNIT (LENGTH_MEASURE( 1.000000000000000082E-05 ), #127952, 'distance_accuracy_value', 'NONE');
#84022 = ORIENTED_EDGE ( 'NONE', *, *, #1269, .F. ) ;
#84023 = CARTESIAN_POINT ( 'NONE',  ( -27.29974487139158512, -27.71228299555225405, 4.000000000000000000 ) ) ;
#84024 = EDGE_CURVE ( 'NONE', #29579, #41631, #43541, .T. ) ;
#84025 = CARTESIAN_POINT ( 'NONE',  ( 124.1833603837961988, -2.130196079827426203, 7.949999999999997513 ) ) ;
#84026 = DIRECTION ( 'NONE',  ( 0.3543493200069162685, -0.000000000000000000, -0.9351131265310288487 ) ) ;
#84027 = AXIS2_PLACEMENT_3D ( 'NONE', #129424, #120678, #108351 ) ;
#84028 = PLANE ( 'NONE',  #50593 ) ;
#84029 = PLANE ( 'NONE',  #65345 ) ;
#84030 = FILL_AREA_STYLE ('',( #63694 ) ) ;
#84031 = CARTESIAN_POINT ( 'NONE',  ( -2.999999999999975131, -4.068876922607777225, 4.000000000000000000 ) ) ;
#84032 = CARTESIAN_POINT ( 'NONE',  ( 31.77040314143522082, -7.934999999999989839, 2.126176841940957907 ) ) ;
#84033 = CARTESIAN_POINT ( 'NONE',  ( 4.499569808101886004, -3.967499999999998028, -6.871911579029511330 ) ) ;
#84034 = LINE ( 'NONE', #115877, #20460 ) ;
#84035 = DIRECTION ( 'NONE',  ( 1.000000000000000000, 0.000000000000000000, 0.000000000000000000 ) ) ;
#84036 = CARTESIAN_POINT ( 'NONE',  ( 72.18398860626899705, 28.73617430169837661, 5.000000000000000000 ) ) ;
#84037 = VERTEX_POINT ( 'NONE', #87760 ) ;
#84038 = VECTOR ( 'NONE', #118860, 1000.000000000000000 ) ;
#84039 = VERTEX_POINT ( 'NONE', #121090 ) ;
#84040 = CARTESIAN_POINT ( 'NONE',  ( 82.37500000000000000, 7.950000000000000178, 1.460391307983218535E-15 ) ) ;
#84041 = DIRECTION ( 'NONE',  ( -1.000000000000000000, 0.000000000000000000, -0.000000000000000000 ) ) ;
#84042 = ORIENTED_EDGE ( 'NONE', *, *, #101607, .F. ) ;
#84043 = VECTOR ( 'NONE', #117091, 1000.000000000000227 ) ;
#84044 = CARTESIAN_POINT ( 'NONE',  ( 15.18398860626900237, 28.73617430169797871, 5.000000000000000000 ) ) ;
#84045 = CARTESIAN_POINT ( 'NONE',  ( 56.99451991528749062, 28.92564299267978001, 4.000000000000000000 ) ) ;
#84046 = AXIS2_PLACEMENT_3D ( 'NONE', #80316, #124502, #119315 ) ;
#84047 = CARTESIAN_POINT ( 'NONE',  ( 30.99586038379621655, -3.974999999999998312, -6.884901960086286188 ) ) ;
#84048 = VERTEX_POINT ( 'NONE', #140695 ) ;
#84049 = LINE ( 'NONE', #48530, #104163 ) ;
#84050 = DIRECTION ( 'NONE',  ( 0.7071067811865487940, -0.7071067811865463515, 0.000000000000000000 ) ) ;
#84051 = DIRECTION ( 'NONE',  ( 0.6830127018922181881, 0.6830127018922202975, -0.2588190451025214056 ) ) ;
#84052 = LINE ( 'NONE', #99695, #2705 ) ;
#84053 = PLANE ( 'NONE',  #81789 ) ;
#84054 = DIRECTION ( 'NONE',  ( -0.3543493200069162685, -0.000000000000000000, -0.9351131265310288487 ) ) ;
#84055 = CARTESIAN_POINT ( 'NONE',  ( 75.18398860626899705, 28.73617430169839793, 5.000000000000000000 ) ) ;
#84056 = DIRECTION ( 'NONE',  ( -0.7071067811865486830, -0.7071067811865464625, 0.000000000000000000 ) ) ;
#84057 = LINE ( 'NONE', #52103, #137255 ) ;
#84058 = FACE_OUTER_BOUND ( 'NONE', #130456, .T. ) ;
#84059 = PLANE ( 'NONE',  #66133 ) ;
#84060 = CARTESIAN_POINT ( 'NONE',  ( 61.46640106136305803, -43.15000000000002700, 34.92499999999998295 ) ) ;
#84061 = VECTOR ( 'NONE', #78285, 1000.000000000000000 ) ;
#84062 = VERTEX_POINT ( 'NONE', #120340 ) ;
#84063 = ORIENTED_EDGE ( 'NONE', *, *, #41971, .F. ) ;
#84064 = CARTESIAN_POINT ( 'NONE',  ( 102.2295968585647614, -6.110000000000000320, -1.637169565754161393 ) ) ;
#84065 =( BOUNDED_CURVE ( )  B_SPLINE_CURVE ( 3, ( #12742, #125647, #15399, #43975 ),
 .UNSPECIFIED., .F., .T. ) 
 B_SPLINE_CURVE_WITH_KNOTS ( ( 4, 4 ),
 ( 0.1773996044403763073, 1.570796326794896558 ),
 .UNSPECIFIED. ) 
 CURVE ( )  GEOMETRIC_REPRESENTATION_ITEM ( )  RATIONAL_B_SPLINE_CURVE ( ( 1.000000000000000000, 0.8446433258982480874, 0.8446433258982480874, 1.000000000000000000 ) ) 
 REPRESENTATION_ITEM ( '' )  );
#84066 = VERTEX_POINT ( 'NONE', #21788 ) ;
#84067 = VECTOR ( 'NONE', #98840, 1000.000000000000000 ) ;
#84068 = CARTESIAN_POINT ( 'NONE',  ( -51.18398860626899705, 28.73617430169823095, 5.000000000000000000 ) ) ;
#84069 = AXIS2_PLACEMENT_3D ( 'NONE', #47174, #21252, #20509 ) ;
#84070 = LINE ( 'NONE', #61602, #117191 ) ;
#84071 = VERTEX_POINT ( 'NONE', #66037 ) ;
#84072 = CARTESIAN_POINT ( 'NONE',  ( 74.64583333333331439, 2.130196079827431976, -7.949999999999998401 ) ) ;
#84073 = DIRECTION ( 'NONE',  ( -0.000000000000000000, 0.000000000000000000, 1.000000000000000000 ) ) ;
#84074 = CARTESIAN_POINT ( 'NONE',  ( 98.78709685856479439, 3.054999999999997495, 5.291415217122919401 ) ) ;
#84075 = ORIENTED_EDGE ( 'NONE', *, *, #94836, .F. ) ;
#84076 = LINE ( 'NONE', #63740, #79087 ) ;
#84077 = ORIENTED_EDGE ( 'NONE', *, *, #13878, .T. ) ;
#84078 = DIRECTION ( 'NONE',  ( -1.000000000000000000, -0.000000000000000000, -0.000000000000000000 ) ) ;
#84079 = VECTOR ( 'NONE', #85280, 1000.000000000000000 ) ;
#84080 = PLANE ( 'NONE',  #21445 ) ;
#84081 = CARTESIAN_POINT ( 'NONE',  ( 78.18398860626899705, 28.73617430169841924, 5.000000000000000000 ) ) ;
#84082 = ORIENTED_EDGE ( 'NONE', *, *, #60565, .T. ) ;
#84083 = EDGE_LOOP ( 'NONE', ( #36203, #105209, #57342, #33442 ) ) ;
#84084 = ADVANCED_FACE ( 'NONE', ( #110202 ), #10874, .F. ) ;
#84085 = VERTEX_POINT ( 'NONE', #118950 ) ;
#84086 = DIRECTION ( 'NONE',  ( -0.6830127018922181881, 0.6830127018922202975, -0.2588190451025214056 ) ) ;
#84087 = EDGE_CURVE ( 'NONE', #79941, #18880, #22470, .T. ) ;
#84088 = CARTESIAN_POINT ( 'NONE',  ( 51.18398860626899705, 28.73617430169823095, 5.000000000000000000 ) ) ;
#84089 = CARTESIAN_POINT ( 'NONE',  ( 11.29623647476855375, 7.934999999999990727, -1.457635852685135314E-15 ) ) ;
#84090 = VECTOR ( 'NONE', #96283, 1000.000000000000000 ) ;
#84091 = DIRECTION ( 'NONE',  ( 0.3543493200069162685, -0.000000000000000000, -0.9351131265310288487 ) ) ;
#84092 = ORIENTED_EDGE ( 'NONE', *, *, #118683, .T. ) ;
#84094 = ORIENTED_EDGE ( 'NONE', *, *, #104839, .T. ) ;
#84093 = EDGE_CURVE ( 'NONE', #18713, #133133, #135562, .T. ) ;
#84095 = CARTESIAN_POINT ( 'NONE',  ( -60.48921356237309510, -27.52281430457097500, 5.000000000000000000 ) ) ;
#84096 = ORIENTED_EDGE ( 'NONE', *, *, #45542, .T. ) ;
#84097 = ORIENTED_EDGE ( 'NONE', *, *, #7625, .T. ) ;
#84098 = AXIS2_PLACEMENT_3D ( 'NONE', #99273, #142807, #109465 ) ;
#84099 = CARTESIAN_POINT ( 'NONE',  ( 113.9537635252314516, -6.109999999999998543, -3.741295971395162543E-16 ) ) ;
#84100 = EDGE_CURVE ( 'NONE', #66103, #62418, #75864, .T. ) ;
#84101 = VECTOR ( 'NONE', #42045, 1000.000000000000000 ) ;
#84102 = CARTESIAN_POINT ( 'NONE',  ( 71.99451991528749772, 28.92564299267988304, 4.000000000000000000 ) ) ;
#84103 = CARTESIAN_POINT ( 'NONE',  ( 21.79289321881330821, 15.75929247661555799, 5.000000000000000000 ) ) ;
#84104 = EDGE_LOOP ( 'NONE', ( #20946, #83507, #6894, #133832 ) ) ;
#84105 = CARTESIAN_POINT ( 'NONE',  ( -5.018447346356667893, 18.75929247661552424, 20.33588619593443880 ) ) ;
#84106 = CARTESIAN_POINT ( 'NONE',  ( 60.18398860626900415, 28.73617430169829490, 5.000000000000000000 ) ) ;
#84107 = VECTOR ( 'NONE', #9838, 1000.000000000000000 ) ;
#84108 = CARTESIAN_POINT ( 'NONE',  ( 32.99999999999976552, 15.45873954670188155, -0.03131636524301723706 ) ) ;
#84109 = EDGE_CURVE ( 'NONE', #55527, #84757, #95320, .T. ) ;
#84110 = CARTESIAN_POINT ( 'NONE',  ( -41.99451991528749062, 28.92564299267967343, 4.000000000000000000 ) ) ;
#84111 = ORIENTED_EDGE ( 'NONE', *, *, #50421, .F. ) ;
#84112 = CARTESIAN_POINT ( 'NONE',  ( 10.49999999999992539, 18.05218569542898521, 5.000000000000000000 ) ) ;
#84113 = CARTESIAN_POINT ( 'NONE',  ( 36.58333333333332860, 6.884901960086290629, -3.974999999999994316 ) ) ;
#84114 = ORIENTED_EDGE ( 'NONE', *, *, #28303, .F. ) ;
#84115 = CARTESIAN_POINT ( 'NONE',  ( 8.999999999999934275, 7.588810512006216591, -3.013526669885247866 ) ) ;
#84116 = LINE ( 'NONE', #92802, #89691 ) ;
#84117 = VERTEX_POINT ( 'NONE', #11588 ) ;
#84118 = DIRECTION ( 'NONE',  ( 0.7071067811865487940, -0.7071067811865463515, 0.000000000000000000 ) ) ;
#84119 = ORIENTED_EDGE ( 'NONE', *, *, #129757, .F. ) ;
#84120 = ORIENTED_EDGE ( 'NONE', *, *, #93584, .F. ) ;
#84121 = ORIENTED_EDGE ( 'NONE', *, *, #5818, .T. ) ;
#84122 = CARTESIAN_POINT ( 'NONE',  ( 31.55793019189810522, 6.110000000000000320, -1.637169565754156064 ) ) ;
#84123 = VECTOR ( 'NONE', #56024, 1000.000000000000000 ) ;
#84124 = CARTESIAN_POINT ( 'NONE',  ( -4.828169399223495084, -2.240707523384262601, 4.000000000000000000 ) ) ;
#84125 = DIRECTION ( 'NONE',  ( 0.5735764363510448272, -0.8191520442889927978, 1.003171929053526103E-16 ) ) ;
#84126 = CARTESIAN_POINT ( 'NONE',  ( -34.42500000000001137, -3.022814304570547783, 5.000000000000000000 ) ) ;
#84127 = DIRECTION ( 'NONE',  ( 0.7071067811865486830, -0.7071067811865464625, -0.000000000000000000 ) ) ;
#84128 = EDGE_CURVE ( 'NONE', #27164, #84039, #90631, .T. ) ;
#84129 = LINE ( 'NONE', #63791, #94483 ) ;
#84130 = FACE_OUTER_BOUND ( 'NONE', #99026, .T. ) ;
#84132 = DIRECTION ( 'NONE',  ( -0.7071067811865486830, -0.7071067811865464625, 0.000000000000000000 ) ) ;
#84131 = AXIS2_PLACEMENT_3D ( 'NONE', #42599, #131016, #76648 ) ;
#84133 = ADVANCED_FACE ( 'NONE', ( #56612 ), #2130, .T. ) ;
#84134 = ADVANCED_FACE ( 'NONE', ( #133420 ), #2877, .F. ) ;
#84135 = FACE_OUTER_BOUND ( 'NONE', #65802, .T. ) ;
#84136 = CARTESIAN_POINT ( 'NONE',  ( -10.49999999999993960, 16.08746187583909659, 4.000000000000000000 ) ) ;
#84137 = AXIS2_PLACEMENT_3D ( 'NONE', #117611, #16913, #114763 ) ;
#84138 = DIRECTION ( 'NONE',  ( 0.7071067811865487940, 0.7071067811865463515, 0.000000000000000000 ) ) ;
#84139 = ORIENTED_EDGE ( 'NONE', *, *, #139969, .F. ) ;
#84140 = ORIENTED_EDGE ( 'NONE', *, *, #36190, .T. ) ;
#84141 = EDGE_LOOP ( 'NONE', ( #30676, #106675, #65919, #20103 ) ) ;
#84142 = ORIENTED_EDGE ( 'NONE', *, *, #132746, .T. ) ;
#84143 = CARTESIAN_POINT ( 'NONE',  ( -1.277985381820198496, 0.3445797145511038106, 3.790392630796158624 ) ) ;
#84144 = ORIENTED_EDGE ( 'NONE', *, *, #100503, .T. ) ;
#84145 = EDGE_CURVE ( 'NONE', #84071, #116810, #13734, .T. ) ;
#84146 = VECTOR ( 'NONE', #111971, 1000.000000000000000 ) ;
#84147 = EDGE_LOOP ( 'NONE', ( #58752, #102679, #102723, #9366 ) ) ;
#84148 = CARTESIAN_POINT ( 'NONE',  ( 0.000000000000000000, 0.000000000000000000, 5.000000000000000000 ) ) ;
#84149 = ADVANCED_FACE ( 'NONE', ( #36245 ), #89887, .F. ) ;
#84150 = EDGE_CURVE ( 'NONE', #129167, #46218, #110121, .T. ) ;
#84151 = CARTESIAN_POINT ( 'NONE',  ( 18.48921356237309510, -27.52281430457068367, 5.000000000000000000 ) ) ;
#84152 = ORIENTED_EDGE ( 'NONE', *, *, #87190, .T. ) ;
#84153 = CARTESIAN_POINT ( 'NONE',  ( -42.18398860626899705, 28.73617430169816700, 5.000000000000000000 ) ) ;
#84154 = EDGE_LOOP ( 'NONE', ( #8856, #82360, #63987, #124230 ) ) ;
#84156 = VECTOR ( 'NONE', #79501, 1000.000000000000114 ) ;
#84155 = LINE ( 'NONE', #72585, #123107 ) ;
#84157 = DIRECTION ( 'NONE',  ( -0.000000000000000000, 0.3543493200069153248, 0.9351131265310292928 ) ) ;
#84158 = VECTOR ( 'NONE', #51164, 999.9999999999998863 ) ;
#84159 = CARTESIAN_POINT ( 'NONE',  ( 7.504569808101886785, 6.871911579029510442, -3.967499999999998916 ) ) ;
#84160 = ORIENTED_EDGE ( 'NONE', *, *, #47667, .T. ) ;
#84161 = CARTESIAN_POINT ( 'NONE',  ( 105.9329301918981088, 1.637169565754156730, 6.110000000000001208 ) ) ;
#84162 = ADVANCED_FACE ( 'NONE', ( #30427 ), #76692, .T. ) ;
#84163 = LINE ( 'NONE', #139249, #4978 ) ;
#84164 = LINE ( 'NONE', #38490, #120569 ) ;
#84165 = ORIENTED_EDGE ( 'NONE', *, *, #64862, .T. ) ;
#84166 = EDGE_LOOP ( 'NONE', ( #93104, #102731, #87907, #71807 ) ) ;
#84167 = FACE_OUTER_BOUND ( 'NONE', #44760, .T. ) ;
#84168 = ORIENTED_EDGE ( 'NONE', *, *, #14513, .T. ) ;
#84170 = AXIS2_PLACEMENT_3D ( 'NONE', #115005, #93993, #47694 ) ;
#84169 = FACE_OUTER_BOUND ( 'NONE', #136509, .T. ) ;
#84171 = CARTESIAN_POINT ( 'NONE',  ( -12.85181644961847169, 17.25929247661554555, 8.802941693769172460 ) ) ;
#84173 = EDGE_CURVE ( 'NONE', #98151, #13095, #6471, .T. ) ;
#84172 = CARTESIAN_POINT ( 'NONE',  ( 61.46640106136302961, -43.14999999999999147, -34.92499999999998295 ) ) ;
#84174 = DIRECTION ( 'NONE',  ( -0.3543493200069162685, -0.000000000000000000, -0.9351131265310288487 ) ) ;
#84175 = CARTESIAN_POINT ( 'NONE',  ( 184.1499999999998067, -49.85820393249934313, -34.92499999999997584 ) ) ;
#84176 = ORIENTED_EDGE ( 'NONE', *, *, #124705, .T. ) ;
#84177 = DIRECTION ( 'NONE',  ( 0.3543493200069162685, -0.000000000000000000, -0.9351131265310288487 ) ) ;
#84178 = LINE ( 'NONE', #73285, #74375 ) ;
#84179 = DIRECTION ( 'NONE',  ( -0.6830127018922180770, -0.6830127018922204085, -0.2588190451025213501 ) ) ;
#84180 = ORIENTED_EDGE ( 'NONE', *, *, #102441, .T. ) ;
#84181 = FACE_OUTER_BOUND ( 'NONE', #61375, .T. ) ;
#84182 = AXIS2_PLACEMENT_3D ( 'NONE', #37084, #47315, #47996 ) ;
#84183 = LINE ( 'NONE', #73289, #102611 ) ;
#84184 = VERTEX_POINT ( 'NONE', #84802 ) ;
#84186 = ORIENTED_EDGE ( 'NONE', *, *, #134515, .F. ) ;
#84185 = DIRECTION ( 'NONE',  ( -0.5735764363510499342, -0.8191520442889891340, 0.000000000000000000 ) ) ;
#84187 = ORIENTED_EDGE ( 'NONE', *, *, #89638, .F. ) ;
#84188 = DIRECTION ( 'NONE',  ( -0.000000000000000000, -0.3543493200069152693, 0.9351131265310292928 ) ) ;
#84189 = LINE ( 'NONE', #30499, #143298 ) ;
#84190 = ORIENTED_EDGE ( 'NONE', *, *, #142424, .T. ) ;
#84191 = LINE ( 'NONE', #117467, #55863 ) ;
#84192 = ADVANCED_FACE ( 'NONE', ( #96351 ), #129012, .F. ) ;
#84193 = DIRECTION ( 'NONE',  ( 0.000000000000000000, 1.000000000000000000, 4.625929269271485322E-15 ) ) ;
#84194 = ADVANCED_FACE ( 'NONE', ( #63083 ), #7930, .T. ) ;
#84196 = VECTOR ( 'NONE', #33845, 1000.000000000000000 ) ;
#84195 = CARTESIAN_POINT ( 'NONE',  ( 27.18398860626900060, 28.73617430169806042, 5.000000000000000000 ) ) ;
#84197 = DIRECTION ( 'NONE',  ( -0.6830127018922180770, -0.6830127018922204085, -0.2588190451025213501 ) ) ;
#84198 = CARTESIAN_POINT ( 'NONE',  ( -29.29289321881324426, 17.25929247661553845, 5.000000000000000000 ) ) ;
#84199 = LINE ( 'NONE', #58904, #99974 ) ;
#84200 = DIRECTION ( 'NONE',  ( 0.7071067811865486830, -0.7071067811865464625, -0.000000000000000000 ) ) ;
#84201 = CARTESIAN_POINT ( 'NONE',  ( 29.99999999999979039, 19.93112307739198386, 4.000000000000000000 ) ) ;
#84202 = CARTESIAN_POINT ( 'NONE',  ( -24.29974487139158867, -27.71228299555223273, 4.000000000000000000 ) ) ;
#84203 = CARTESIAN_POINT ( 'NONE',  ( 20.99999999999985079, 8.816494571476654940, 4.604407763760433703 ) ) ;
#84204 = FACE_OUTER_BOUND ( 'NONE', #141522, .T. ) ;
#84205 = FACE_OUTER_BOUND ( 'NONE', #12247, .T. ) ;
#84206 = ORIENTED_EDGE ( 'NONE', *, *, #132773, .T. ) ;
#84207 = VECTOR ( 'NONE', #112951, 999.9999999999998863 ) ;
#84208 = ORIENTED_EDGE ( 'NONE', *, *, #108598, .F. ) ;
#84209 = VERTEX_POINT ( 'NONE', #23834 ) ;
#84210 = CARTESIAN_POINT ( 'NONE',  ( 114.7500000000000000, -9.735942053221458872E-16, 7.950000000000000178 ) ) ;
#84211 = ORIENTED_EDGE ( 'NONE', *, *, #86079, .T. ) ;
#84212 = ORIENTED_EDGE ( 'NONE', *, *, #10376, .F. ) ;
#84213 = EDGE_LOOP ( 'NONE', ( #49268, #17563, #128967, #132422 ) ) ;
#84214 = LINE ( 'NONE', #128410, #36366 ) ;
#84215 = FACE_OUTER_BOUND ( 'NONE', #57397, .T. ) ;
#84216 = CYLINDRICAL_SURFACE ( 'NONE', #32379, 2.500000000000000000 ) ;
#84217 = ORIENTED_EDGE ( 'NONE', *, *, #96901, .F. ) ;
#84218 = DIRECTION ( 'NONE',  ( -0.6830127018922181881, 0.6830127018922202975, -0.2588190451025214056 ) ) ;
#84219 = DIRECTION ( 'NONE',  ( -0.7071067811865486830, -0.7071067811865464625, -0.000000000000000000 ) ) ;
#84220 = DIRECTION ( 'NONE',  ( 0.7071067811865486830, -0.7071067811865464625, -0.000000000000000000 ) ) ;
#84221 = LINE ( 'NONE', #75465, #99778 ) ;
#84222 = CARTESIAN_POINT ( 'NONE',  ( 105.5837635252314328, -6.110000000000001208, -3.741295971395164515E-16 ) ) ;
#84223 = VERTEX_POINT ( 'NONE', #97816 ) ;
#84224 = DIRECTION ( 'NONE',  ( 1.000000000000000000, -0.000000000000000000, -0.000000000000000000 ) ) ;
#84225 = CARTESIAN_POINT ( 'NONE',  ( 32.67183060077623935, 11.25929247661559884, 4.000000000000000000 ) ) ;
#84226 = CARTESIAN_POINT ( 'NONE',  ( -24.71757738642550351, -21.73023691814493219, 5.000000000000000888 ) ) ;
#84227 = LINE ( 'NONE', #20877, #72957 ) ;
#84228 = VECTOR ( 'NONE', #128143, 1000.000000000000000 ) ;
#84229 = CARTESIAN_POINT ( 'NONE',  ( -32.99999999999976552, 8.966399257802180500, 5.000000000000000000 ) ) ;
#84230 = CARTESIAN_POINT ( 'NONE',  ( -9.707106781186476852, 2.259292476615701428, 5.000000000000000000 ) ) ;
#84231 = CARTESIAN_POINT ( 'NONE',  ( 41.20419371712954870, -6.884901960086285300, -3.975000000000000089 ) ) ;
#84232 = CARTESIAN_POINT ( 'NONE',  ( 13.96000000000000085, 9.521314400968980422E-16, 0.000000000000000000 ) ) ;
#84234 = SURFACE_STYLE_FILL_AREA ( #143386 ) ;
#84233 = VECTOR ( 'NONE', #39982, 1000.000000000000000 ) ;
#84235 = EDGE_LOOP ( 'NONE', ( #23447, #23761, #73346, #138504 ) ) ;
#84236 = ORIENTED_EDGE ( 'NONE', *, *, #14347, .T. ) ;
#84237 = CARTESIAN_POINT ( 'NONE',  ( 26.66666666666665719, 6.884901960086285300, 3.975000000000003642 ) ) ;
#84238 = ORIENTED_EDGE ( 'NONE', *, *, #107722, .F. ) ;
#84239 = CARTESIAN_POINT ( 'NONE',  ( -11.99451991528749417, 28.92564299267946382, 4.000000000000000000 ) ) ;
#84240 = EDGE_CURVE ( 'NONE', #98041, #105535, #54352, .T. ) ;
#84241 = CARTESIAN_POINT ( 'NONE',  ( -60.18398860626900415, 28.73617430169829490, 5.000000000000000000 ) ) ;
#84242 = CARTESIAN_POINT ( 'NONE',  ( 26.43999999999999773, 9.521314400968980422E-16, 0.000000000000000000 ) ) ;
#84243 = VECTOR ( 'NONE', #74144, 1000.000000000000000 ) ;
#84244 = LINE ( 'NONE', #84923, #37371 ) ;
#84245 = LINE ( 'NONE', #126984, #58161 ) ;
#84246 = CARTESIAN_POINT ( 'NONE',  ( 121.9745968585647802, 1.637169565754164058, -6.109999999999996767 ) ) ;
#84247 = VECTOR ( 'NONE', #17440, 1000.000000000000000 ) ;
#84248 = ORIENTED_EDGE ( 'NONE', *, *, #42528, .T. ) ;
#84249 = DIRECTION ( 'NONE',  ( -0.000000000000000000, 0.000000000000000000, 1.000000000000000000 ) ) ;
#84250 = ORIENTED_EDGE ( 'NONE', *, *, #10713, .T. ) ;
#84251 = DIRECTION ( 'NONE',  ( -0.7071067811865486830, -0.7071067811865464625, 0.000000000000000000 ) ) ;
#84252 = CARTESIAN_POINT ( 'NONE',  ( 57.48921356237308800, -27.52281430457095368, 5.000000000000000000 ) ) ;
#84253 = CARTESIAN_POINT ( 'NONE',  ( -32.29298673570672662, -21.74070752338405299, 4.999753212805210012 ) ) ;
#84254 = ADVANCED_FACE ( 'NONE', ( #44169 ), #89788, .T. ) ;
#84255 = FACE_OUTER_BOUND ( 'NONE', #90519, .T. ) ;
#84256 = ORIENTED_EDGE ( 'NONE', *, *, #99142, .F. ) ;
#84257 = CARTESIAN_POINT ( 'NONE',  ( 43.16709685856477563, -3.055000000000000160, -5.291415217122921177 ) ) ;
#84258 = EDGE_CURVE ( 'NONE', #125811, #142084, #23075, .T. ) ;
#84259 = ORIENTED_EDGE ( 'NONE', *, *, #109081, .F. ) ;
#84260 = LINE ( 'NONE', #93684, #49448 ) ;
#84261 = CARTESIAN_POINT ( 'NONE',  ( 27.48921356237309155, -27.52281430457074762, 5.000000000000000000 ) ) ;
#84262 = CARTESIAN_POINT ( 'NONE',  ( 57.18398860626899705, 28.73617430169827358, 5.000000000000000000 ) ) ;
#84263 = CARTESIAN_POINT ( 'NONE',  ( 32.22995720542186149, 21.73644205237997440, 5.000000000000000888 ) ) ;
#84264 = AXIS2_PLACEMENT_3D ( 'NONE', #14253, #12099, #143337 ) ;
#84266 = EDGE_CURVE ( 'NONE', #30354, #120324, #121690, .T. ) ;
#84265 = AXIS2_PLACEMENT_3D ( 'NONE', #30042, #74293, #86602 ) ;
#84267 = ADVANCED_FACE ( 'NONE', ( #65941 ), #110802, .F. ) ;
#84268 = AXIS2_PLACEMENT_3D ( 'NONE', #9356, #119555, #51495 ) ;
#84269 = CARTESIAN_POINT ( 'NONE',  ( 51.97459685856478728, 1.637169565754164058, -6.109999999999996767 ) ) ;
#84270 = ORIENTED_EDGE ( 'NONE', *, *, #88127, .F. ) ;
#84271 = DIRECTION ( 'NONE',  ( -0.000000000000000000, 0.3543493200069153248, 0.9351131265310292928 ) ) ;
#84272 = EDGE_CURVE ( 'NONE', #119001, #114079, #69772, .T. ) ;
#84273 = DIRECTION ( 'NONE',  ( -0.000000000000000000, -0.3543493200069152693, 0.9351131265310292928 ) ) ;
#84274 = ORIENTED_EDGE ( 'NONE', *, *, #70036, .T. ) ;
#84275 = VERTEX_POINT ( 'NONE', #143453 ) ;
#84276 = VECTOR ( 'NONE', #14039, 1000.000000000000227 ) ;
#84277 = VERTEX_POINT ( 'NONE', #131161 ) ;
#84278 = ADVANCED_FACE ( 'NONE', ( #12221 ), #10777, .F. ) ;
#84279 = FACE_OUTER_BOUND ( 'NONE', #59474, .T. ) ;
#84280 = ORIENTED_EDGE ( 'NONE', *, *, #11423, .T. ) ;
#84281 = CARTESIAN_POINT ( 'NONE',  ( 44.41252705046289151, -7.949999999999998401, -4.867971026610728450E-16 ) ) ;
#84282 = EDGE_CURVE ( 'NONE', #98856, #59256, #31852, .T. ) ;
#84283 = VECTOR ( 'NONE', #32996, 1000.000000000000000 ) ;
#84284 = EDGE_CURVE ( 'NONE', #57178, #51263, #76071, .T. ) ;
#84285 = FACE_BOUND ( 'NONE', #139330, .T. ) ;
#84286 = SURFACE_STYLE_FILL_AREA ( #63257 ) ;
#84287 = DIRECTION ( 'NONE',  ( 0.6830127018922181881, 0.6830127018922202975, -0.2588190451025214056 ) ) ;
#84288 = DIRECTION ( 'NONE',  ( 0.6830127018922181881, 0.6830127018922202975, -0.2588190451025214056 ) ) ;
#84289 = ORIENTED_EDGE ( 'NONE', *, *, #65669, .T. ) ;
#84290 = DIRECTION ( 'NONE',  ( -0.000000000000000000, 1.000000000000000000, -0.000000000000000000 ) ) ;
#84291 = ORIENTED_EDGE ( 'NONE', *, *, #45609, .F. ) ;
#84293 = ORIENTED_EDGE ( 'NONE', *, *, #42419, .F. ) ;
#84292 = ADVANCED_FACE ( 'NONE', ( #120238 ), #20957, .F. ) ;
#84294 = CARTESIAN_POINT ( 'NONE',  ( 26.99451991528749417, 28.92564299267956685, 4.000000000000000000 ) ) ;
#84295 = ORIENTED_EDGE ( 'NONE', *, *, #66179, .T. ) ;
#84296 = CARTESIAN_POINT ( 'NONE',  ( 52.12043019189811588, 3.055000000000001936, -5.291415217122916737 ) ) ;
#84298 = VERTEX_POINT ( 'NONE', #10084 ) ;
#84297 = AXIS2_PLACEMENT_3D ( 'NONE', #70611, #69894, #72764 ) ;
#84299 = FACE_OUTER_BOUND ( 'NONE', #40128, .T. ) ;
#84300 = CARTESIAN_POINT ( 'NONE',  ( 2.999999999999981792, 1.761378380278684430, -6.096875308897248935 ) ) ;
#84301 = EDGE_CURVE ( 'NONE', #59037, #4133, #99214, .T. ) ;
#84302 = EDGE_LOOP ( 'NONE', ( #134324, #122605, #57368, #41515 ) ) ;
#84303 = LINE ( 'NONE', #50939, #51441 ) ;
#84304 = VECTOR ( 'NONE', #47246, 999.9999999999998863 ) ;
#84305 = ADVANCED_FACE ( 'NONE', ( #98527 ), #87657, .F. ) ;
#84306 = CARTESIAN_POINT ( 'NONE',  ( 35.56249999999999289, -5.819803920172573086, -5.819803920172573974 ) ) ;
#84307 = FACE_OUTER_BOUND ( 'NONE', #140554, .T. ) ;
#84308 = FACE_OUTER_BOUND ( 'NONE', #110187, .T. ) ;
#84309 = EDGE_CURVE ( 'NONE', #141405, #76093, #89103, .T. ) ;
#84310 = DIRECTION ( 'NONE',  ( -0.7071067811865487940, 0.7071067811865463515, 0.000000000000000000 ) ) ;
#84311 = DIRECTION ( 'NONE',  ( -0.6830127018922180770, -0.6830127018922204085, -0.2588190451025213501 ) ) ;
#84312 = EDGE_LOOP ( 'NONE', ( #141571, #63271, #98421, #90326 ) ) ;
#84313 = ORIENTED_EDGE ( 'NONE', *, *, #62500, .T. ) ;
#84314 = PLANE ( 'NONE',  #63624 ) ;
#84315 = DIRECTION ( 'NONE',  ( 0.5735764363510448272, -0.8191520442889927978, 1.003171929053526103E-16 ) ) ;
#84316 = ORIENTED_EDGE ( 'NONE', *, *, #131399, .F. ) ;
#84317 = EDGE_CURVE ( 'NONE', #122980, #67467, #34005, .T. ) ;
#84318 = ORIENTED_EDGE ( 'NONE', *, *, #52306, .T. ) ;
#84319 = ORIENTED_EDGE ( 'NONE', *, *, #40922, .T. ) ;
#84320 = DIRECTION ( 'NONE',  ( -0.3543493200069163240, 0.000000000000000000, -0.9351131265310288487 ) ) ;
#84321 = CARTESIAN_POINT ( 'NONE',  ( -2.816011393730999401, 28.73617430169785436, 5.000000000000000000 ) ) ;
#84322 = ORIENTED_EDGE ( 'NONE', *, *, #4635, .T. ) ;
#84323 = DIRECTION ( 'NONE',  ( -0.7071067811865486830, -0.7071067811865464625, 0.000000000000000000 ) ) ;
#84324 = AXIS2_PLACEMENT_3D ( 'NONE', #48251, #60601, #80897 ) ;
#84325 = FACE_OUTER_BOUND ( 'NONE', #3628, .T. ) ;
#84326 = VECTOR ( 'NONE', #70144, 1000.000000000000000 ) ;
#84327 = CARTESIAN_POINT ( 'NONE',  ( 5.025403141435220711, 2.126176841940962348, 7.934999999999989839 ) ) ;
#84328 = DIRECTION ( 'NONE',  ( 0.7071067811865487940, -0.7071067811865463515, 0.000000000000000000 ) ) ;
#84329 = VERTEX_POINT ( 'NONE', #100686 ) ;
#84330 = FACE_OUTER_BOUND ( 'NONE', #28053, .T. ) ;
#84331 = ADVANCED_FACE ( 'NONE', ( #1333 ), #134029, .F. ) ;
#84332 = CARTESIAN_POINT ( 'NONE',  ( 27.29974487139158512, -27.71228299555225405, 4.000000000000000000 ) ) ;
#84333 = LINE ( 'NONE', #117602, #54244 ) ;
#84335 = ORIENTED_EDGE ( 'NONE', *, *, #8978, .F. ) ;
#84334 = CARTESIAN_POINT ( 'NONE',  ( 11.67183060077638501, 2.259292476615694323, 4.000000000000000000 ) ) ;
#84336 = CARTESIAN_POINT ( 'NONE',  ( 5.683420388672068668, -6.740707523384219968, 11.88629033278122726 ) ) ;
#84337 = ORIENTED_EDGE ( 'NONE', *, *, #59368, .T. ) ;
#84338 = LINE ( 'NONE', #106746, #119187 ) ;
#84339 = EDGE_CURVE ( 'NONE', #86087, #3663, #124571, .T. ) ;
#84340 = LINE ( 'NONE', #106024, #93277 ) ;
#84341 = DIRECTION ( 'NONE',  ( 0.6830127018922181881, 0.6830127018922202975, -0.2588190451025214056 ) ) ;
#84342 = ORIENTED_EDGE ( 'NONE', *, *, #103620, .T. ) ;
#84343 = AXIS2_PLACEMENT_3D ( 'NONE', #58705, #115121, #137647 ) ;
#84344 = VECTOR ( 'NONE', #70540, 1000.000000000000000 ) ;
#84345 = PLANE ( 'NONE',  #54174 ) ;
#84346 = LINE ( 'NONE', #71312, #10 ) ;
#84347 = CARTESIAN_POINT ( 'NONE',  ( 0.000000000000000000, 0.000000000000000000, 5.000000000000000000 ) ) ;
#84348 = ORIENTED_EDGE ( 'NONE', *, *, #141064, .F. ) ;
#84349 = CARTESIAN_POINT ( 'NONE',  ( 27.48921356237309155, -27.52281430457074762, 5.000000000000000000 ) ) ;
#84350 = PLANE ( 'NONE',  #16852 ) ;
#84351 =( BOUNDED_CURVE ( )  B_SPLINE_CURVE ( 2, ( #86315, #130537, #51547 ),
 .UNSPECIFIED., .F., .T. ) 
 B_SPLINE_CURVE_WITH_KNOTS ( ( 3, 3 ),
 ( 0.9499999999999999556, 0.9523725280802812776 ),
 .UNSPECIFIED. ) 
 CURVE ( )  GEOMETRIC_REPRESENTATION_ITEM ( )  RATIONAL_B_SPLINE_CURVE ( ( 1.000000000000000000, 0.9708969037810349922, 0.9915083049239592494 ) ) 
 REPRESENTATION_ITEM ( '' )  );
#84352 = CARTESIAN_POINT ( 'NONE',  ( -15.13499573751613347, 3.759292476615671230, 15.36553568819729421 ) ) ;
#84353 = CARTESIAN_POINT ( 'NONE',  ( -22.45764329680115878, -1.725981765586489525, 4.380536896699288363 ) ) ;
#84354 = CARTESIAN_POINT ( 'NONE',  ( -13.49999999999992184, -14.70932175296479549, -11.46312253303834616 ) ) ;
#84355 = CONICAL_SURFACE ( 'NONE', #93529, 2.500000000000000888, 0.9599310885968822538 ) ;
#84356 = ORIENTED_EDGE ( 'NONE', *, *, #12057, .T. ) ;
#84357 = EDGE_CURVE ( 'NONE', #83610, #87604, #49173, .T. ) ;
#84358 = ORIENTED_EDGE ( 'NONE', *, *, #112390, .F. ) ;
#84359 = DIRECTION ( 'NONE',  ( 0.7071067811865487940, 0.7071067811865463515, 0.000000000000000000 ) ) ;
#84360 = LINE ( 'NONE', #61884, #103844 ) ;
#84361 = VECTOR ( 'NONE', #127414, 1000.000000000000000 ) ;
#84362 = CARTESIAN_POINT ( 'NONE',  ( 14.12456980810188689, -6.871911579029512218, 3.967499999999996252 ) ) ;
#84363 = FACE_OUTER_BOUND ( 'NONE', #60061, .T. ) ;
#84364 = VECTOR ( 'NONE', #106023, 1000.000000000000000 ) ;
#84365 = LINE ( 'NONE', #126396, #115413 ) ;
#84366 = CARTESIAN_POINT ( 'NONE',  ( 0.000000000000000000, 0.000000000000000000, 5.000000000000000000 ) ) ;
#84367 = ORIENTED_EDGE ( 'NONE', *, *, #21178, .T. ) ;
#84368 = FACE_OUTER_BOUND ( 'NONE', #14631, .T. ) ;
#84369 = CARTESIAN_POINT ( 'NONE',  ( 36.09667064187383545, -2.240707523384260824, 15.26439735382760787 ) ) ;
#84370 = CARTESIAN_POINT ( 'NONE',  ( 56.99451991528749062, 28.92564299267978001, 4.000000000000000000 ) ) ;
#84371 = CARTESIAN_POINT ( 'NONE',  ( 0.000000000000000000, 0.000000000000000000, 5.000000000000000000 ) ) ;
#84372 = CARTESIAN_POINT ( 'NONE',  ( 42.34959685856478018, 6.109999999999997655, 1.637169565754163836 ) ) ;
#84373 = DIRECTION ( 'NONE',  ( 0.7071067811865487940, 0.7071067811865463515, -0.000000000000000000 ) ) ;
#84374 = EDGE_CURVE ( 'NONE', #65716, #54738, #47762, .T. ) ;
#84375 = ORIENTED_EDGE ( 'NONE', *, *, #54646, .T. ) ;
#84376 = LINE ( 'NONE', #74924, #18597 ) ;
#84377 = ORIENTED_EDGE ( 'NONE', *, *, #105076, .F. ) ;
#84378 = EDGE_LOOP ( 'NONE', ( #118876, #87509, #135368, #15176, #115972 ) ) ;
#84379 = DIRECTION ( 'NONE',  ( -0.7071067811865486830, -0.7071067811865464625, -0.000000000000000000 ) ) ;
#84380 = DIRECTION ( 'NONE',  ( -0.000000000000000000, -1.000000000000000000, -0.000000000000000000 ) ) ;
#84381 = CARTESIAN_POINT ( 'NONE',  ( -29.67183060077626422, 5.259292476615659240, 4.000000000000000000 ) ) ;
#84382 = DIRECTION ( 'NONE',  ( 0.7071067811865487940, 0.7071067811865463515, 0.000000000000000000 ) ) ;
#84383 = EDGE_CURVE ( 'NONE', #104716, #13272, #24535, .T. ) ;
#84384 = CARTESIAN_POINT ( 'NONE',  ( -33.18398860626899705, 28.73617430169810305, 5.000000000000000000 ) ) ;
#84385 = CARTESIAN_POINT ( 'NONE',  ( 19.49999999999988276, 19.08746187583905041, 4.000000000000000000 ) ) ;
#84386 = ORIENTED_EDGE ( 'NONE', *, *, #51529, .T. ) ;
#84387 = PLANE ( 'NONE',  #18579 ) ;
#84388 = DIRECTION ( 'NONE',  ( 0.000000000000000000, 1.000000000000000000, 1.301042606982605074E-16 ) ) ;
#84389 = LINE ( 'NONE', #118397, #100545 ) ;
#84390 = LINE ( 'NONE', #17648, #4479 ) ;
#84391 = PLANE ( 'NONE',  #93719 ) ;
#84392 = PLANE ( 'NONE',  #87417 ) ;
#84393 = CARTESIAN_POINT ( 'NONE',  ( 68.03752705046289861, -9.735942053221456900E-16, 7.949999999999998401 ) ) ;
#84394 = DIRECTION ( 'NONE',  ( 0.000000000000000000, 0.000000000000000000, 1.000000000000000000 ) ) ;
#84395 = VERTEX_POINT ( 'NONE', #25245 ) ;
#84396 = ORIENTED_EDGE ( 'NONE', *, *, #122794, .F. ) ;
#84397 = CARTESIAN_POINT ( 'NONE',  ( 51.74999999999999289, -9.735942053221458872E-16, 7.950000000000000178 ) ) ;
#84398 = LINE ( 'NONE', #8199, #37796 ) ;
#84399 = PLANE ( 'NONE',  #41596 ) ;
#84400 = VERTEX_POINT ( 'NONE', #4877 ) ;
#84401 = VECTOR ( 'NONE', #41288, 1000.000000000000227 ) ;
#84402 = FACE_OUTER_BOUND ( 'NONE', #34738, .T. ) ;
#84403 = ADVANCED_FACE ( 'NONE', ( #104209 ), #137598, .F. ) ;
#84404 = CARTESIAN_POINT ( 'NONE',  ( 61.39626352523143993, 4.472830434245840259, -4.472830434245839371 ) ) ;
#84405 = EDGE_LOOP ( 'NONE', ( #140683, #100135, #36927, #88092 ) ) ;
#84406 = EDGE_CURVE ( 'NONE', #86990, #50436, #48436, .T. ) ;
#84407 = CARTESIAN_POINT ( 'NONE',  ( -54.29974487139159578, -27.71228299555243879, 4.000000000000000000 ) ) ;
#84408 = ORIENTED_EDGE ( 'NONE', *, *, #24451, .T. ) ;
#84409 = VERTEX_POINT ( 'NONE', #36837 ) ;
#84410 = DIRECTION ( 'NONE',  ( -0.7071067811865486830, -0.7071067811865464625, 0.000000000000000000 ) ) ;
#84411 = LINE ( 'NONE', #94526, #47734 ) ;
#84412 = CARTESIAN_POINT ( 'NONE',  ( -36.29974487139159578, -27.71228299555231445, 4.000000000000000000 ) ) ;
#84413 = LINE ( 'NONE', #137356, #104158 ) ;
#84414 = CARTESIAN_POINT ( 'NONE',  ( 34.92499999999998295, 22.22500000000000142, 4.000000000000000000 ) ) ;
#84415 = EDGE_CURVE ( 'NONE', #135826, #108262, #58663, .T. ) ;
#84416 = EDGE_CURVE ( 'NONE', #83894, #12991, #119426, .T. ) ;
#84418 = ORIENTED_EDGE ( 'NONE', *, *, #83873, .F. ) ;
#84417 = FACE_OUTER_BOUND ( 'NONE', #93733, .T. ) ;
#84419 = DIRECTION ( 'NONE',  ( -0.2248289345038709253, -0.9743982503113675087, 2.708646368993815516E-16 ) ) ;
#84420 = CARTESIAN_POINT ( 'NONE',  ( -29.48334561358934991, 22.22500000000000142, 4.500000000000000888 ) ) ;
#84421 = LINE ( 'NONE', #70698, #137362 ) ;
#84422 = VECTOR ( 'NONE', #121876, 1000.000000000000000 ) ;
#84423 = DIRECTION ( 'NONE',  ( -0.3543493200069162685, -0.000000000000000000, -0.9351131265310288487 ) ) ;
#84425 = ORIENTED_EDGE ( 'NONE', *, *, #74291, .T. ) ;
#84424 = EDGE_CURVE ( 'NONE', #2806, #53423, #50885, .T. ) ;
#84426 = EDGE_CURVE ( 'NONE', #120806, #89946, #46337, .T. ) ;
#84427 = VECTOR ( 'NONE', #74035, 1000.000000000000000 ) ;
#84428 = EDGE_LOOP ( 'NONE', ( #136041, #17965 ) ) ;
#84429 = EDGE_CURVE ( 'NONE', #46897, #84117, #125287, .T. ) ;
#84430 = CARTESIAN_POINT ( 'NONE',  ( 88.89169371712954160, 2.130196079827421762, 7.950000000000000178 ) ) ;
#84431 = CARTESIAN_POINT ( 'NONE',  ( 72.97459685856478018, 1.637169565754164058, -6.109999999999996767 ) ) ;
#84432 = VECTOR ( 'NONE', #29964, 1000.000000000000000 ) ;
#84433 = CARTESIAN_POINT ( 'NONE',  ( -28.82816939922332011, 21.75929247661549937, 4.000000000000000000 ) ) ;
#84434 = EDGE_CURVE ( 'NONE', #139479, #21681, #136868, .T. ) ;
#84435 = FACE_OUTER_BOUND ( 'NONE', #8671, .T. ) ;
#84436 = VERTEX_POINT ( 'NONE', #37576 ) ;
#84437 = ORIENTED_EDGE ( 'NONE', *, *, #139235, .F. ) ;
#84438 = ADVANCED_FACE ( 'NONE', ( #126011 ), #26681, .T. ) ;
#84439 = PLANE ( 'NONE',  #42246 ) ;
#84440 = LINE ( 'NONE', #103288, #7375 ) ;
#84441 = VERTEX_POINT ( 'NONE', #94770 ) ;
#84442 = EDGE_CURVE ( 'NONE', #10011, #4056, #128157, .T. ) ;
#84443 = ORIENTED_EDGE ( 'NONE', *, *, #67139, .F. ) ;
#84444 = DIRECTION ( 'NONE',  ( -0.000000000000000000, 0.000000000000000000, 1.000000000000000000 ) ) ;
#84445 = ORIENTED_EDGE ( 'NONE', *, *, #101893, .F. ) ;
#84446 = DIRECTION ( 'NONE',  ( 0.6830127018922181881, 0.6830127018922202975, -0.2588190451025214056 ) ) ;
#84447 = EDGE_CURVE ( 'NONE', #94939, #84223, #28114, .T. ) ;
#84448 = FACE_BOUND ( 'NONE', #97973, .T. ) ;
#84449 = CARTESIAN_POINT ( 'NONE',  ( 0.000000000000000000, 0.000000000000000000, 5.000000000000000000 ) ) ;
#84450 = CARTESIAN_POINT ( 'NONE',  ( 10.37159235450332062, 9.902892378096218942E-16, 0.000000000000000000 ) ) ;
#84451 = CARTESIAN_POINT ( 'NONE',  ( 51.29974487139158867, -27.71228299555242103, 4.000000000000000000 ) ) ;
#84453 = ORIENTED_EDGE ( 'NONE', *, *, #102751, .T. ) ;
#84452 = CARTESIAN_POINT ( 'NONE',  ( -12.48921356237309155, -27.52281430457064104, 5.000000000000000000 ) ) ;
#84454 = ADVANCED_FACE ( 'NONE', ( #139023 ), #51305, .T. ) ;
#84455 = VECTOR ( 'NONE', #19231, 1000.000000000000000 ) ;
#84456 = ORIENTED_EDGE ( 'NONE', *, *, #121223, .F. ) ;
#84457 = VECTOR ( 'NONE', #122373, 1000.000000000000000 ) ;
#84459 = ORIENTED_EDGE ( 'NONE', *, *, #52715, .F. ) ;
#84458 = VECTOR ( 'NONE', #65988, 1000.000000000000000 ) ;
#84460 = CARTESIAN_POINT ( 'NONE',  ( 83.03709685856478018, -3.054999999999998828, -5.291415217122919401 ) ) ;
#84461 = VERTEX_POINT ( 'NONE', #85326 ) ;
#84462 = AXIS2_PLACEMENT_3D ( 'NONE', #142043, #8590, #133304 ) ;
#84463 = DIRECTION ( 'NONE',  ( -0.000000000000000000, -0.3543493200069152693, 0.9351131265310292928 ) ) ;
#84464 = CARTESIAN_POINT ( 'NONE',  ( -29.99999999999978684, -7.447814304570752775, 5.000000000000000000 ) ) ;
#84465 = DIRECTION ( 'NONE',  ( 0.6830127018922181881, 0.6830127018922202975, -0.2588190451025214056 ) ) ;
#84466 = DIRECTION ( 'NONE',  ( 0.6830127018922180770, -0.6830127018922204085, -0.2588190451025213501 ) ) ;
#84468 = ORIENTED_EDGE ( 'NONE', *, *, #41673, .T. ) ;
#84467 = EDGE_CURVE ( 'NONE', #94978, #109375, #129549, .T. ) ;
#84469 = PLANE ( 'NONE',  #96979 ) ;
#84470 = DIRECTION ( 'NONE',  ( -1.000000000000000000, 0.000000000000000000, 0.000000000000000000 ) ) ;
#84471 = FACE_OUTER_BOUND ( 'NONE', #110815, .T. ) ;
#84472 = EDGE_CURVE ( 'NONE', #136324, #30765, #117933, .T. ) ;
#84473 = CARTESIAN_POINT ( 'NONE',  ( 5.999999999999970690, 2.587461875839214720, 4.000000000000000000 ) ) ;
#84474 = CARTESIAN_POINT ( 'NONE',  ( -14.99999999999989342, -3.412538124160717778, 4.000000000000000000 ) ) ;
#84475 = CARTESIAN_POINT ( 'NONE',  ( 16.30000000000000071, -2.055000000000000160, 0.000000000000000000 ) ) ;
#84476 = EDGE_LOOP ( 'NONE', ( #113919, #10151, #39564, #61054 ) ) ;
#84477 = CARTESIAN_POINT ( 'NONE',  ( 27.48921356237309155, -27.52281430457074762, 5.000000000000000000 ) ) ;
#84478 = EDGE_CURVE ( 'NONE', #97682, #95787, #63627, .T. ) ;
#84479 = DIRECTION ( 'NONE',  ( 0.3543493200069162685, -0.000000000000000000, -0.9351131265310288487 ) ) ;
#84480 = EDGE_LOOP ( 'NONE', ( #46741, #63216, #33668, #73774, #107196 ) ) ;
#84481 = EDGE_LOOP ( 'NONE', ( #423, #24087, #129927, #43298 ) ) ;
#84482 = ORIENTED_EDGE ( 'NONE', *, *, #66863, .F. ) ;
#84483 = CARTESIAN_POINT ( 'NONE',  ( 33.68793019189809712, 6.110000000000002984, -1.637169565754156730 ) ) ;
#84484 = ORIENTED_EDGE ( 'NONE', *, *, #60963, .T. ) ;
#84485 = CARTESIAN_POINT ( 'NONE',  ( 17.83747294953710494, 6.094999999999989981, -1.119633336120465690E-15 ) ) ;
#84486 = CARTESIAN_POINT ( 'NONE',  ( -12.79760398132481392, 9.635117458823907910, -27.13457238307817576 ) ) ;
#84487 = ORIENTED_EDGE ( 'NONE', *, *, #122710, .T. ) ;
#84488 = EDGE_CURVE ( 'NONE', #48215, #112363, #2543, .T. ) ;
#84489 = CARTESIAN_POINT ( 'NONE',  ( 57.18398860626899705, 28.73617430169827358, 5.000000000000000000 ) ) ;
#84490 = ORIENTED_EDGE ( 'NONE', *, *, #54093, .F. ) ;
#84491 = CARTESIAN_POINT ( 'NONE',  ( -47.99451991528749062, 28.92564299267971251, 4.000000000000000000 ) ) ;
#84492 = DIRECTION ( 'NONE',  ( -1.000000000000000000, -1.224606353822377258E-16, -0.000000000000000000 ) ) ;
#84494 = ORIENTED_EDGE ( 'NONE', *, *, #89673, .F. ) ;
#84493 = FACE_OUTER_BOUND ( 'NONE', #56623, .T. ) ;
#84495 = ORIENTED_EDGE ( 'NONE', *, *, #20065, .T. ) ;
#84496 = VECTOR ( 'NONE', #16684, 999.9999999999998863 ) ;
#84497 = CARTESIAN_POINT ( 'NONE',  ( 11.67183060077639212, 14.25929247661557753, 4.000000000000000000 ) ) ;
#84498 = ORIENTED_EDGE ( 'NONE', *, *, #80962, .T. ) ;
#84499 = LINE ( 'NONE', #75758, #59695 ) ;
#84500 = ORIENTED_EDGE ( 'NONE', *, *, #61599, .F. ) ;
#84501 = ORIENTED_EDGE ( 'NONE', *, *, #19337, .F. ) ;
#84502 = ADVANCED_FACE ( 'NONE', ( #127413 ), #38987, .F. ) ;
#84503 = VERTEX_POINT ( 'NONE', #7761 ) ;
#84504 = VERTEX_POINT ( 'NONE', #116547 ) ;
#84505 = DIRECTION ( 'NONE',  ( -0.6830127018922181881, 0.6830127018922202975, -0.2588190451025214056 ) ) ;
#84506 = LINE ( 'NONE', #38844, #84043 ) ;
#84507 = LINE ( 'NONE', #73618, #63353 ) ;
#84508 = EDGE_CURVE ( 'NONE', #141704, #94354, #52010, .T. ) ;
#84509 = CARTESIAN_POINT ( 'NONE',  ( -5.999999999999963585, 1.761378380278677547, -6.096875308897267587 ) ) ;
#84510 = ORIENTED_EDGE ( 'NONE', *, *, #118077, .T. ) ;
#84512 = ADVANCED_FACE ( 'NONE', ( #5615 ), #105640, .F. ) ;
#84511 = CARTESIAN_POINT ( 'NONE',  ( 66.62499999999998579, -7.950000000000000178, -4.867971026610729436E-16 ) ) ;
#84513 = VERTEX_POINT ( 'NONE', #96893 ) ;
#84514 = FACE_OUTER_BOUND ( 'NONE', #91592, .T. ) ;
#84515 =( BOUNDED_SURFACE ( )  B_SPLINE_SURFACE ( 3, 2, ( 
 ( #11247, #63563, #8385 ),
 ( #52634, #53355, #41779 ),
 ( #85991, #130227, #130949 ),
 ( #9847, #54117, #98306 ) ),
 .UNSPECIFIED., .F., .F., .F. ) 
 B_SPLINE_SURFACE_WITH_KNOTS ( ( 4, 4 ),
 ( 3, 3 ),
 ( 0.000000000000000000, 0.001630001914283400570 ),
 ( 0.000000000000000000, 1.000000000000000000 ),
 .UNSPECIFIED. ) 
 GEOMETRIC_REPRESENTATION_ITEM ( )  RATIONAL_B_SPLINE_SURFACE ( (
 ( 1.000000000000000000, 0.7071067811865475727, 1.000000000000000000),
 ( 1.000000000000000000, 0.7121002461815034712, 1.000000000000000000),
 ( 1.000000000000000000, 0.7157206429707760886, 1.000000000000000000),
 ( 1.000000000000000000, 0.7180326832784531543, 1.000000000000000000) ) ) 
 REPRESENTATION_ITEM ( '' )  SURFACE ( )  );
#84516 = VECTOR ( 'NONE', #28925, 1000.000000000000000 ) ;
#84517 = CARTESIAN_POINT ( 'NONE',  ( 34.39540314143521016, 2.126176841940962348, 7.934999999999989839 ) ) ;
#84518 = EDGE_CURVE ( 'NONE', #20632, #58831, #8449, .T. ) ;
#84519 = LINE ( 'NONE', #51166, #85624 ) ;
#84520 = ORIENTED_EDGE ( 'NONE', *, *, #60446, .T. ) ;
#84521 = PLANE ( 'NONE',  #92344 ) ;
#84522 = LINE ( 'NONE', #18493, #76757 ) ;
#84523 = ORIENTED_EDGE ( 'NONE', *, *, #43411, .F. ) ;
#84524 = VECTOR ( 'NONE', #65141, 999.9999999999998863 ) ;
#84525 = VERTEX_POINT ( 'NONE', #141139 ) ;
#84526 = ORIENTED_EDGE ( 'NONE', *, *, #45467, .T. ) ;
#84527 = CARTESIAN_POINT ( 'NONE',  ( 24.79289321881328689, 9.759292476615620160, 5.000000000000000000 ) ) ;
#84528 = DIRECTION ( 'NONE',  ( -0.7071067811865486830, -0.7071067811865464625, -0.000000000000000000 ) ) ;
#84529 = DIRECTION ( 'NONE',  ( 1.000000000000000000, 0.000000000000000000, 0.000000000000000000 ) ) ;
#84530 = DIRECTION ( 'NONE',  ( 0.7071067811865486830, -0.7071067811865464625, -0.000000000000000000 ) ) ;
#84531 = PLANE ( 'NONE',  #140838 ) ;
#84532 = CARTESIAN_POINT ( 'NONE',  ( 71.95376352523145158, -6.109999999999999432, -3.741295971395163529E-16 ) ) ;
#84533 = EDGE_CURVE ( 'NONE', #33763, #11268, #41848, .T. ) ;
#84534 = DIRECTION ( 'NONE',  ( 0.000000000000000000, 0.000000000000000000, -1.000000000000000000 ) ) ;
#84535 = EDGE_CURVE ( 'NONE', #3663, #85320, #30989, .T. ) ;
#84536 = AXIS2_PLACEMENT_3D ( 'NONE', #71698, #16564, #126079 ) ;
#84537 = DIRECTION ( 'NONE',  ( 0.7071067811865487940, 0.7071067811865463515, 0.000000000000000000 ) ) ;
#84538 = CARTESIAN_POINT ( 'NONE',  ( 1.171830600776456732, 12.75929247661558996, 4.000000000000000000 ) ) ;
#84539 = FACE_OUTER_BOUND ( 'NONE', #124944, .T. ) ;
#84540 = ORIENTED_EDGE ( 'NONE', *, *, #134827, .F. ) ;
#84541 = CARTESIAN_POINT ( 'NONE',  ( -36.18398860626899705, 28.73617430169812437, 5.000000000000000000 ) ) ;
#84542 = ORIENTED_EDGE ( 'NONE', *, *, #82166, .F. ) ;
#84543 = CARTESIAN_POINT ( 'NONE',  ( -31.41009064519812455, 9.759292476615618384, 11.28811694763771634 ) ) ;
#84545 = ORIENTED_EDGE ( 'NONE', *, *, #14102, .T. ) ;
#84544 = CARTESIAN_POINT ( 'NONE',  ( -34.75611968250419892, -18.18706574529243625, 4.955485411084906033 ) ) ;
#84546 = ADVANCED_FACE ( 'NONE', ( #99048 ), #456, .F. ) ;
#84547 = LINE ( 'NONE', #14964, #111145 ) ;
#84548 = CARTESIAN_POINT ( 'NONE',  ( 8.510786437626906675, -27.52281430457049183, 5.000000000000000000 ) ) ;
#84549 = ORIENTED_EDGE ( 'NONE', *, *, #69670, .F. ) ;
#84550 = EDGE_LOOP ( 'NONE', ( #60035, #2087, #26264, #63733 ) ) ;
#84551 = DIRECTION ( 'NONE',  ( 0.7071067811865487940, 0.7071067811865463515, 0.000000000000000000 ) ) ;
#84552 = CARTESIAN_POINT ( 'NONE',  ( -72.48921356237309510, -27.52281430457106026, 5.000000000000000000 ) ) ;
#84553 = VECTOR ( 'NONE', #27126, 1000.000000000000000 ) ;
#84554 = CARTESIAN_POINT ( 'NONE',  ( 96.76669371712954160, -7.949999999999999289, 2.130196079827424427 ) ) ;
#84556 = VECTOR ( 'NONE', #95162, 1000.000000000000000 ) ;
#84555 = DIRECTION ( 'NONE',  ( -0.6830127018922180770, -0.6830127018922204085, -0.2588190451025213501 ) ) ;
#84557 = VECTOR ( 'NONE', #25076, 1000.000000000000000 ) ;
#84558 = FACE_OUTER_BOUND ( 'NONE', #67874, .T. ) ;
#84559 = EDGE_LOOP ( 'NONE', ( #104340, #143163, #125458, #27057 ) ) ;
#84560 =( GEOMETRIC_REPRESENTATION_CONTEXT ( 3 ) GLOBAL_UNCERTAINTY_ASSIGNED_CONTEXT ( ( #17457 ) ) GLOBAL_UNIT_ASSIGNED_CONTEXT ( ( #68939, #121832, #55190 ) ) REPRESENTATION_CONTEXT ( 'NONE', 'WORKASPACE' ) );
#84561 = LINE ( 'NONE', #64225, #90890 ) ;
#84562 = DIRECTION ( 'NONE',  ( 0.000000000000000000, -1.000000000000000000, 0.000000000000000000 ) ) ;
#84563 = CARTESIAN_POINT ( 'NONE',  ( -34.92500000000001137, 22.22500000000000142, 4.500000000000000888 ) ) ;
#84564 = CARTESIAN_POINT ( 'NONE',  ( -69.48921356237309510, -27.52281430457103895, 5.000000000000000000 ) ) ;
#84565 = VERTEX_POINT ( 'NONE', #67169 ) ;
#84566 = CARTESIAN_POINT ( 'NONE',  ( -35.99451991528749772, 28.92564299267963079, 4.000000000000000000 ) ) ;
#84567 = ORIENTED_EDGE ( 'NONE', *, *, #31913, .F. ) ;
#84568 = CARTESIAN_POINT ( 'NONE',  ( 84.14626352523144703, -4.472830434245840259, 4.472830434245839371 ) ) ;
#84569 = CARTESIAN_POINT ( 'NONE',  ( 24.18398860626899705, 28.73617430169804265, 5.000000000000000000 ) ) ;
#84570 = EDGE_CURVE ( 'NONE', #95348, #97698, #74409, .T. ) ;
#84571 = DIRECTION ( 'NONE',  ( 0.000000000000000000, 0.000000000000000000, -1.000000000000000000 ) ) ;
#84572 = ORIENTED_EDGE ( 'NONE', *, *, #81396, .F. ) ;
#84573 = CARTESIAN_POINT ( 'NONE',  ( 6.940000000000001279, 2.055000000000001492, 2.516649172247811554E-16 ) ) ;
#84574 = FACE_OUTER_BOUND ( 'NONE', #16150, .T. ) ;
#84575 = LINE ( 'NONE', #128087, #18467 ) ;
#84576 = ADVANCED_FACE ( 'NONE', ( #132465 ), #88941, .F. ) ;
#84578 = ORIENTED_EDGE ( 'NONE', *, *, #136069, .T. ) ;
#84577 = CARTESIAN_POINT ( 'NONE',  ( -12.18398860626900060, 28.73617430169795739, 5.000000000000000000 ) ) ;
#84579 = DIRECTION ( 'NONE',  ( 0.000000000000000000, -1.000000000000000000, 0.000000000000000000 ) ) ;
#84580 = CARTESIAN_POINT ( 'NONE',  ( -0.7071067811865415775, 17.25929247661554200, 5.000000000000000000 ) ) ;
#84581 = CARTESIAN_POINT ( 'NONE',  ( 1.743167068800034469, -4.720063557702711243, 4.254651343200441360 ) ) ;
#84582 = FILL_AREA_STYLE_COLOUR ( '', #60882 ) ;
#84583 = VERTEX_POINT ( 'NONE', #131712 ) ;
#84584 = ORIENTED_EDGE ( 'NONE', *, *, #74906, .F. ) ;
#84585 = ADVANCED_FACE ( 'NONE', ( #97641 ), #100517, .T. ) ;
#84586 = CARTESIAN_POINT ( 'NONE',  ( 72.47959685856478984, 6.109999999999999432, 1.637169565754164280 ) ) ;
#84587 = ORIENTED_EDGE ( 'NONE', *, *, #42680, .T. ) ;
#84588 = ADVANCED_FACE ( 'NONE', ( #65786 ), #111362, .F. ) ;
#84589 = CARTESIAN_POINT ( 'NONE',  ( -27.32816939922333432, 14.25929247661558286, 4.000000000000000000 ) ) ;
#84590 = ADVANCED_FACE ( 'NONE', ( #78057 ), #32407, .T. ) ;
#84591 = DIRECTION ( 'NONE',  ( -1.000000000000000000, -0.000000000000000000, -0.000000000000000000 ) ) ;
#84592 = CARTESIAN_POINT ( 'NONE',  ( -22.82816939922336630, -17.24070752338410273, 4.000000000000000000 ) ) ;
#84593 = ORIENTED_EDGE ( 'NONE', *, *, #7669, .F. ) ;
#84594 = EDGE_CURVE ( 'NONE', #138159, #103344, #64314, .T. ) ;
#84595 = FACE_OUTER_BOUND ( 'NONE', #92695, .T. ) ;
#84596 = CYLINDRICAL_SURFACE ( 'NONE', #337, 0.5000000000000004441 ) ;
#84597 = ORIENTED_EDGE ( 'NONE', *, *, #46585, .T. ) ;
#84598 = EDGE_CURVE ( 'NONE', #97938, #125706, #45443, .T. ) ;
#84599 = DIRECTION ( 'NONE',  ( -1.000000000000000000, -0.000000000000000000, -0.000000000000000000 ) ) ;
#84600 = LINE ( 'NONE', #83912, #45553 ) ;
#84601 = CARTESIAN_POINT ( 'NONE',  ( 36.18398860626899705, 28.73617430169812437, 5.000000000000000000 ) ) ;
#84602 = ORIENTED_EDGE ( 'NONE', *, *, #123223, .T. ) ;
#84603 = ORIENTED_EDGE ( 'NONE', *, *, #69820, .F. ) ;
#84604 = ADVANCED_FACE ( 'NONE', ( #121528 ), #120074, .F. ) ;
#84605 = EDGE_CURVE ( 'NONE', #136110, #61441, #1160, .T. ) ;
#84606 = LINE ( 'NONE', #60752, #77880 ) ;
#84607 = DIRECTION ( 'NONE',  ( 0.6830127018922181881, 0.6830127018922202975, -0.2588190451025214056 ) ) ;
#84608 = DIRECTION ( 'NONE',  ( -0.7071067811865486830, -0.7071067811865464625, -0.000000000000000000 ) ) ;
#84609 = DIRECTION ( 'NONE',  ( -0.000000000000000000, 0.3543493200069153248, 0.9351131265310292928 ) ) ;
#84610 = CARTESIAN_POINT ( 'NONE',  ( 13.49999999999990763, -8.568876922607724822, 4.000000000000000000 ) ) ;
#84611 = EDGE_CURVE ( 'NONE', #127621, #77870, #86788, .T. ) ;
#84612 = DIRECTION ( 'NONE',  ( 0.6830127018922180770, -0.6830127018922204085, -0.2588190451025213501 ) ) ;
#84614 = ORIENTED_EDGE ( 'NONE', *, *, #142037, .T. ) ;
#84613 = CONICAL_SURFACE ( 'NONE', #29028, 2.055000000000001048, 0.9599310885968758145 ) ;
#84615 = VERTEX_POINT ( 'NONE', #43993 ) ;
#84616 = VERTEX_POINT ( 'NONE', #89623 ) ;
#84617 = AXIS2_PLACEMENT_3D ( 'NONE', #54127, #119321, #64256 ) ;
#84618 = ORIENTED_EDGE ( 'NONE', *, *, #105814, .F. ) ;
#84619 = CARTESIAN_POINT ( 'NONE',  ( -34.92500000000001137, 3.856123077392404674, 4.000000000000000000 ) ) ;
#84620 = ORIENTED_EDGE ( 'NONE', *, *, #94563, .T. ) ;
#84621 = CARTESIAN_POINT ( 'NONE',  ( -27.48921356237309155, -27.52281430457074762, 5.000000000000000000 ) ) ;
#84622 = CARTESIAN_POINT ( 'NONE',  ( 5.292893218813425449, 5.259292476615663681, 5.000000000000000000 ) ) ;
#84623 = EDGE_CURVE ( 'NONE', #136452, #140795, #66468, .T. ) ;
#84624 = CARTESIAN_POINT ( 'NONE',  ( 6.005480084712508493, 28.92564299267933947, 4.000000000000000000 ) ) ;
#84625 = CARTESIAN_POINT ( 'NONE',  ( -32.99999999999976552, -12.41253812416063163, 4.000000000000000000 ) ) ;
#84626 = VERTEX_POINT ( 'NONE', #142594 ) ;
#84627 = CARTESIAN_POINT ( 'NONE',  ( 33.79333936457825160, 21.75929247661550647, 4.998822639870711626 ) ) ;
#84628 = CARTESIAN_POINT ( 'NONE',  ( 0.03865102804815064713, -0.4000000000000003553, 2.083945628037807030 ) ) ;
#84629 = VERTEX_POINT ( 'NONE', #11311 ) ;
#84630 = CARTESIAN_POINT ( 'NONE',  ( 3.398789304146613510, 2.055000000000001048, 0.000000000000000000 ) ) ;
#84631 = ORIENTED_EDGE ( 'NONE', *, *, #83930, .F. ) ;
#84632 = CARTESIAN_POINT ( 'NONE',  ( 12.00413961620377279, -3.047499999999994547, 5.278424836066145431 ) ) ;
#84633 = ORIENTED_EDGE ( 'NONE', *, *, #104414, .F. ) ;
#84634 = CARTESIAN_POINT ( 'NONE',  ( 72.18793019189810423, 6.110000000000002984, -1.637169565754156730 ) ) ;
#84635 = ORIENTED_EDGE ( 'NONE', *, *, #11933, .F. ) ;
#84636 = ORIENTED_EDGE ( 'NONE', *, *, #90760, .F. ) ;
#84637 = VECTOR ( 'NONE', #85423, 1000.000000000000000 ) ;
#84638 = DIRECTION ( 'NONE',  ( -0.7071067811865487940, 0.7071067811865463515, 0.000000000000000000 ) ) ;
#84639 = VECTOR ( 'NONE', #128949, 1000.000000000000000 ) ;
#84640 = DIRECTION ( 'NONE',  ( 1.000000000000000000, -0.000000000000000000, 0.000000000000000000 ) ) ;
#84641 = CARTESIAN_POINT ( 'NONE',  ( 113.3129301918981042, -1.637169565754159617, -6.110000000000001208 ) ) ;
#84642 = LINE ( 'NONE', #127416, #40218 ) ;
#84643 = VECTOR ( 'NONE', #80587, 1000.000000000000000 ) ;
#84644 = EDGE_CURVE ( 'NONE', #108030, #26817, #75212, .T. ) ;
#84645 = CARTESIAN_POINT ( 'NONE',  ( 0.000000000000000000, 0.000000000000000000, 5.000000000000000000 ) ) ;
#84646 = FACE_OUTER_BOUND ( 'NONE', #73924, .T. ) ;
#84647 = DIRECTION ( 'NONE',  ( 0.000000000000000000, 0.3543493200069153248, 0.9351131265310291818 ) ) ;
#84648 = AXIS2_PLACEMENT_3D ( 'NONE', #30875, #141027, #65677 ) ;
#84649 = CARTESIAN_POINT ( 'NONE',  ( -9.183988606268997046, 28.73617430169793607, 5.000000000000000000 ) ) ;
#84650 = CARTESIAN_POINT ( 'NONE',  ( 91.27083333333332860, -7.949999999999998401, -2.130196079827426203 ) ) ;
#84651 = CARTESIAN_POINT ( 'NONE',  ( 77.51669371712954160, 7.950000000000000178, -2.130196079827421318 ) ) ;
#84652 = ORIENTED_EDGE ( 'NONE', *, *, #132423, .F. ) ;
#84653 = CARTESIAN_POINT ( 'NONE',  ( 26.99451991528749417, 28.92564299267956685, 4.000000000000000000 ) ) ;
#84654 = FACE_OUTER_BOUND ( 'NONE', #101661, .T. ) ;
#84655 = ADVANCED_FACE ( 'NONE', ( #99780 ), #31684, .F. ) ;
#84656 = VERTEX_POINT ( 'NONE', #78764 ) ;
#84657 = ORIENTED_EDGE ( 'NONE', *, *, #4876, .F. ) ;
#84658 = ORIENTED_EDGE ( 'NONE', *, *, #73571, .F. ) ;
#84659 = ORIENTED_EDGE ( 'NONE', *, *, #42233, .T. ) ;
#84660 = DIRECTION ( 'NONE',  ( 0.7071067811865487940, 0.7071067811865463515, -0.000000000000000000 ) ) ;
#84661 = CARTESIAN_POINT ( 'NONE',  ( -51.48921356237309510, -27.52281430457091460, 5.000000000000000000 ) ) ;
#84662 = ADVANCED_FACE ( 'NONE', ( #5969 ), #123710, .T. ) ;
#84663 = CARTESIAN_POINT ( 'NONE',  ( -5.999999999999960032, 1.931123077392169041, 4.000000000000000000 ) ) ;
#84664 = CARTESIAN_POINT ( 'NONE',  ( 128.9683591370938416, -52.14999999999999147, -41.64500000000001023 ) ) ;
#84665 = VERTEX_POINT ( 'NONE', #122975 ) ;
#84666 = CARTESIAN_POINT ( 'NONE',  ( 0.2480159638834371905, -51.74944211519454740, 38.65549799471352799 ) ) ;
#84667 = ORIENTED_EDGE ( 'NONE', *, *, #100962, .F. ) ;
#84668 = CARTESIAN_POINT ( 'NONE',  ( 4.207903141435219929, -6.871911579029513106, -3.967499999999993587 ) ) ;
#84669 = DIRECTION ( 'NONE',  ( 0.7071067811865487940, 0.7071067811865463515, -0.000000000000000000 ) ) ;
#84670 = LINE ( 'NONE', #96221, #113054 ) ;
#84671 = LINE ( 'NONE', #108516, #83694 ) ;
#84672 = ORIENTED_EDGE ( 'NONE', *, *, #83000, .T. ) ;
#84673 = ORIENTED_EDGE ( 'NONE', *, *, #18839, .F. ) ;
#84674 = ORIENTED_EDGE ( 'NONE', *, *, #56255, .F. ) ;
#84675 = DIRECTION ( 'NONE',  ( 0.7071067811865486830, -0.7071067811865464625, -0.000000000000000000 ) ) ;
#84676 = DIRECTION ( 'NONE',  ( 0.7071067811865487940, 0.7071067811865463515, -0.000000000000000000 ) ) ;
#84677 = CARTESIAN_POINT ( 'NONE',  ( 17.84878961325748037, -2.500000000000000444, 3.061616997868384127E-16 ) ) ;
#84678 = DIRECTION ( 'NONE',  ( 0.000000000000000000, -1.000000000000000000, 0.000000000000000000 ) ) ;
#84679 = LINE ( 'NONE', #41163, #69112 ) ;
#84680 = CARTESIAN_POINT ( 'NONE',  ( 3.299744871391591339, -27.71228299555208352, 4.000000000000000000 ) ) ;
#84681 = CARTESIAN_POINT ( 'NONE',  ( -23.99999999999983302, -12.41253812416062274, 4.000000000000000000 ) ) ;
#84682 = DIRECTION ( 'NONE',  ( 0.000000000000000000, -1.000000000000000000, 0.000000000000000000 ) ) ;
#84683 = EDGE_CURVE ( 'NONE', #134910, #124430, #141557, .T. ) ;
#84684 = CARTESIAN_POINT ( 'NONE',  ( 33.54209685856476852, 5.291415217122923842, -3.054999999999996163 ) ) ;
#84685 = DIRECTION ( 'NONE',  ( 0.7071067811865487940, 0.7071067811865463515, -0.000000000000000000 ) ) ;
#84686 = CARTESIAN_POINT ( 'NONE',  ( 5.848407645496676466, 3.061616997868380183E-16, -2.500000000000001332 ) ) ;
#84687 = ORIENTED_EDGE ( 'NONE', *, *, #120584, .F. ) ;
#84688 = CARTESIAN_POINT ( 'NONE',  ( -14.99451991528749595, 28.92564299267948513, 4.000000000000000000 ) ) ;
#84689 = DIRECTION ( 'NONE',  ( -1.000000000000000000, -0.000000000000000000, -0.000000000000000000 ) ) ;
#84690 = ORIENTED_EDGE ( 'NONE', *, *, #22672, .T. ) ;
#84691 = DIRECTION ( 'NONE',  ( -1.000000000000000000, -0.000000000000000000, -0.000000000000000000 ) ) ;
#84693 = ORIENTED_EDGE ( 'NONE', *, *, #28073, .T. ) ;
#84692 = DIRECTION ( 'NONE',  ( 1.000000000000000000, 0.000000000000000000, 0.000000000000000000 ) ) ;
#84694 = EDGE_CURVE ( 'NONE', #60397, #59481, #82877, .T. ) ;
#84695 = CARTESIAN_POINT ( 'NONE',  ( 29.29289321881324781, 14.25929247661557042, 5.000000000000000000 ) ) ;
#84696 = CARTESIAN_POINT ( 'NONE',  ( 26.29289321881327268, -9.740707523384187994, 5.000000000000000000 ) ) ;
#84697 = ORIENTED_EDGE ( 'NONE', *, *, #34285, .T. ) ;
#84698 = DIRECTION ( 'NONE',  ( 1.000000000000000000, 0.000000000000000000, 0.000000000000000000 ) ) ;
#84699 = ORIENTED_EDGE ( 'NONE', *, *, #43251, .T. ) ;
#84700 = PRODUCT_RELATED_PRODUCT_CATEGORY ( 'part', '', ( #44431 ) ) ;
#84701 = CARTESIAN_POINT ( 'NONE',  ( 93.26669371712955581, -7.949999999999998401, 2.130196079827423983 ) ) ;
#84702 = AXIS2_PLACEMENT_3D ( 'NONE', #137471, #47638, #25836 ) ;
#84703 = CARTESIAN_POINT ( 'NONE',  ( 122.2875270504628844, 0.000000000000000000, -7.949999999999998401 ) ) ;
#84704 = LINE ( 'NONE', #110010, #62385 ) ;
#84705 = LINE ( 'NONE', #49252, #39002 ) ;
#84706 = VECTOR ( 'NONE', #110409, 1000.000000000000000 ) ;
#84707 = FACE_OUTER_BOUND ( 'NONE', #16350, .T. ) ;
#84708 = DIRECTION ( 'NONE',  ( -0.000000000000000000, -1.000000000000000000, -0.000000000000000000 ) ) ;
#84709 = DIRECTION ( 'NONE',  ( -1.000000000000000000, -1.224606353822377258E-16, -0.000000000000000000 ) ) ;
#84710 = CARTESIAN_POINT ( 'NONE',  ( 8.458333333333333925, -3.047499999999997211, -5.278424836066143655 ) ) ;
#84711 = CARTESIAN_POINT ( 'NONE',  ( 3.187069808101886448, -2.126176841940956130, 7.934999999999990727 ) ) ;
#84712 = CARTESIAN_POINT ( 'NONE',  ( 12.18398860626900060, 28.73617430169795739, 5.000000000000000000 ) ) ;
#84713 = ORIENTED_EDGE ( 'NONE', *, *, #3995, .T. ) ;
#84714 = ADVANCED_FACE ( 'NONE', ( #49551 ), #106003, .F. ) ;
#84715 =( BOUNDED_CURVE ( )  B_SPLINE_CURVE ( 2, ( #88337, #55712, #86901, #32524, #99162, #132579, #63736, #10727, #131119, #142012, #77475, #41969, #121641 ),
 .UNSPECIFIED., .F., .F. ) 
 B_SPLINE_CURVE_WITH_KNOTS ( ( 3, 2, 2, 2, 2, 2, 3 ),
 ( 0.7333333333333333925, 0.7361111111111112715, 0.7388888888888890394, 0.7416666666666666963, 0.7444444444444444642, 0.7472222222222222321, 0.7500000000000000000 ),
 .UNSPECIFIED. ) 
 CURVE ( )  GEOMETRIC_REPRESENTATION_ITEM ( )  RATIONAL_B_SPLINE_CURVE ( ( 0.9999999999999986677, 0.9659258262890696445, 1.000000000000000000, 0.9659258262890683122, 1.000000000000000000, 0.9659258262890683122, 1.000000000000000000, 0.9659258262890683122, 1.000000000000000000, 0.9659258262890683122, 1.000000000000000000, 0.9659258262890683122, 1.000000000000000000 ) ) 
 REPRESENTATION_ITEM ( '' )  );
#84716 = ORIENTED_EDGE ( 'NONE', *, *, #99233, .F. ) ;
#84717 = CARTESIAN_POINT ( 'NONE',  ( 78.87500000000000000, 7.950000000000000178, 1.460391307983218535E-15 ) ) ;
#84718 = LINE ( 'NONE', #62267, #67551 ) ;
#84719 = ORIENTED_EDGE ( 'NONE', *, *, #7716, .F. ) ;
#84720 = VECTOR ( 'NONE', #29955, 1000.000000000000000 ) ;
#84721 = FACE_OUTER_BOUND ( 'NONE', #23929, .T. ) ;
#84722 = FACE_OUTER_BOUND ( 'NONE', #130741, .T. ) ;
#84723 = CARTESIAN_POINT ( 'NONE',  ( 13.49999999999991118, 19.08746187583904685, 4.000000000000000000 ) ) ;
#84724 = ORIENTED_EDGE ( 'NONE', *, *, #73374, .F. ) ;
#84725 = DIRECTION ( 'NONE',  ( -0.7071067811865486830, -0.7071067811865464625, 0.000000000000000000 ) ) ;
#84726 = CARTESIAN_POINT ( 'NONE',  ( -8.540161610502543965, 18.75929247661552424, 8.305906642995466882 ) ) ;
#84727 = CARTESIAN_POINT ( 'NONE',  ( 55.56056557994604361, -52.00875322212549179, -39.86617647058817937 ) ) ;
#84728 = LINE ( 'NONE', #120170, #79645 ) ;
#84730 = VERTEX_POINT ( 'NONE', #23657 ) ;
#84729 = LINE ( 'NONE', #95596, #105291 ) ;
#84731 = DIRECTION ( 'NONE',  ( 1.000000000000000000, 0.000000000000000000, 0.000000000000000000 ) ) ;
#84732 = DIRECTION ( 'NONE',  ( -0.7071067811865486830, -0.7071067811865464625, -0.000000000000000000 ) ) ;
#84733 = FACE_OUTER_BOUND ( 'NONE', #20745, .T. ) ;
#84734 = CARTESIAN_POINT ( 'NONE',  ( 27.47336096364197644, -5.240707523384228850, 16.25846745537502258 ) ) ;
#84735 = LINE ( 'NONE', #77978, #84639 ) ;
#84736 = VECTOR ( 'NONE', #68714, 1000.000000000000000 ) ;
#84737 = CARTESIAN_POINT ( 'NONE',  ( 56.45153347184072601, -50.67230138428463704, 37.61253110040618708 ) ) ;
#84738 = ORIENTED_EDGE ( 'NONE', *, *, #13932, .T. ) ;
#84739 = VERTEX_POINT ( 'NONE', #34539 ) ;
#84741 = ADVANCED_FACE ( 'NONE', ( #79523 ), #6673, .F. ) ;
#84740 = STYLED_ITEM ( 'NONE', ( #40204 ), #108314 ) ;
#84742 = CARTESIAN_POINT ( 'NONE',  ( 105.1462635252314612, -4.472830434245840259, 4.472830434245839371 ) ) ;
#84743 = ORIENTED_EDGE ( 'NONE', *, *, #72810, .F. ) ;
#84744 = EDGE_CURVE ( 'NONE', #72622, #65156, #95150, .T. ) ;
#84745 = VECTOR ( 'NONE', #78326, 999.9999999999998863 ) ;
#84746 = CARTESIAN_POINT ( 'NONE',  ( 130.2059003229213658, -48.16486758952235903, 37.61253110040621550 ) ) ;
#84747 =( GEOMETRIC_REPRESENTATION_CONTEXT ( 3 ) GLOBAL_UNCERTAINTY_ASSIGNED_CONTEXT ( ( #114273 ) ) GLOBAL_UNIT_ASSIGNED_CONTEXT ( ( #50834, #74750, #85579 ) ) REPRESENTATION_CONTEXT ( 'NONE', 'WORKASPACE' ) );
#84748 = CARTESIAN_POINT ( 'NONE',  ( 7.000000000000000888, 0.000000000000000000, 6.094999999999989981 ) ) ;
#84749 = ORIENTED_EDGE ( 'NONE', *, *, #46183, .F. ) ;
#84750 = EDGE_CURVE ( 'NONE', #93317, #121222, #50955, .T. ) ;
#84751 = ADVANCED_FACE ( 'NONE', ( #4511 ), #60426, .T. ) ;
#84752 = DIRECTION ( 'NONE',  ( -0.7071067811865486830, -0.7071067811865464625, 0.000000000000000000 ) ) ;
#84753 = CARTESIAN_POINT ( 'NONE',  ( -25.49999999999982236, 8.319652575858368593, -8.582050562765886070 ) ) ;
#84754 = CARTESIAN_POINT ( 'NONE',  ( 95.43293019189809456, 1.637169565754156508, 6.110000000000000320 ) ) ;
#84755 = ORIENTED_EDGE ( 'NONE', *, *, #36486, .F. ) ;
#84756 = LINE ( 'NONE', #83337, #102244 ) ;
#84757 = VERTEX_POINT ( 'NONE', #67924 ) ;
#84758 = CARTESIAN_POINT ( 'NONE',  ( 156.1499999999997783, -52.14999999999999147, 34.92500000000004690 ) ) ;
#84759 = DIRECTION ( 'NONE',  ( 0.5735764363510451602, 0.8191520442889924647, 0.000000000000000000 ) ) ;
#84760 = LINE ( 'NONE', #107214, #124956 ) ;
#84761 = ORIENTED_EDGE ( 'NONE', *, *, #53086, .T. ) ;
#84762 = ORIENTED_EDGE ( 'NONE', *, *, #20971, .T. ) ;
#84763 = ADVANCED_FACE ( 'NONE', ( #37947 ), #57034, .F. ) ;
#84764 = ORIENTED_EDGE ( 'NONE', *, *, #57935, .F. ) ;
#84765 = DIRECTION ( 'NONE',  ( 0.7071067811865487940, 0.7071067811865463515, 0.000000000000000000 ) ) ;
#84766 = ADVANCED_FACE ( 'NONE', ( #104606 ), #112113, .T. ) ;
#84767 = PLANE ( 'NONE',  #8293 ) ;
#84768 = CARTESIAN_POINT ( 'NONE',  ( 5.900403141435219823, -7.934999999999988951, 2.126176841940957907 ) ) ;
#84769 = DIRECTION ( 'NONE',  ( -0.7071067811865486830, -0.7071067811865464625, -0.000000000000000000 ) ) ;
#84770 = EDGE_CURVE ( 'NONE', #35713, #112904, #59701, .T. ) ;
#84771 =( NAMED_UNIT ( * ) SI_UNIT ( $, .STERADIAN. ) SOLID_ANGLE_UNIT ( ) );
#84772 = EDGE_LOOP ( 'NONE', ( #111393, #76803, #65106, #76483 ) ) ;
#84773 = ORIENTED_EDGE ( 'NONE', *, *, #128575, .T. ) ;
#84774 = FACE_OUTER_BOUND ( 'NONE', #73230, .T. ) ;
#84775 = ORIENTED_EDGE ( 'NONE', *, *, #27406, .T. ) ;
#84776 = ORIENTED_EDGE ( 'NONE', *, *, #30632, .T. ) ;
#84777 = EDGE_CURVE ( 'NONE', #58187, #19888, #105313, .T. ) ;
#84778 = VECTOR ( 'NONE', #51226, 1000.000000000000000 ) ;
#84779 = CARTESIAN_POINT ( 'NONE',  ( 18.08333333333333215, -5.278424836066144543, 3.047499999999995879 ) ) ;
#84780 = CARTESIAN_POINT ( 'NONE',  ( 12.32816939922344623, 11.25929247661559884, 4.000000000000000000 ) ) ;
#84781 = ORIENTED_EDGE ( 'NONE', *, *, #11689, .F. ) ;
#84782 = LINE ( 'NONE', #106492, #89971 ) ;
#84783 = CARTESIAN_POINT ( 'NONE',  ( 9.792893218813388145, 6.759292476615649470, 5.000000000000000000 ) ) ;
#84784 = ADVANCED_FACE ( 'NONE', ( #115440 ), #134585, .F. ) ;
#84785 = CIRCLE ( 'NONE', #57083, 2.500000000000000444 ) ;
#84786 = DIRECTION ( 'NONE',  ( -0.000000000000000000, -0.3543493200069152693, 0.9351131265310292928 ) ) ;
#84787 = CARTESIAN_POINT ( 'NONE',  ( 12.69999999999999574, -21.76999999999999247, -40.00000000000000000 ) ) ;
#84788 = ORIENTED_EDGE ( 'NONE', *, *, #142397, .F. ) ;
#84789 = CARTESIAN_POINT ( 'NONE',  ( -30.29974487139158867, -27.71228299555227537, 4.000000000000000000 ) ) ;
#84790 = CARTESIAN_POINT ( 'NONE',  ( -47.99451991528749062, 28.92564299267971251, 4.000000000000000000 ) ) ;
#84791 = VERTEX_POINT ( 'NONE', #16893 ) ;
#84792 = CARTESIAN_POINT ( 'NONE',  ( -32.16347128873431416, 15.75929247661555443, 9.299976744542847840 ) ) ;
#84793 = LINE ( 'NONE', #39155, #24902 ) ;
#84794 = CYLINDRICAL_SURFACE ( 'NONE', #44589, 2.999999999999999112 ) ;
#84795 = ORIENTED_EDGE ( 'NONE', *, *, #71161, .F. ) ;
#84796 = DIRECTION ( 'NONE',  ( -0.6830127018922180770, -0.6830127018922204085, -0.2588190451025213501 ) ) ;
#84797 = ORIENTED_EDGE ( 'NONE', *, *, #71672, .T. ) ;
#84798 = ORIENTED_EDGE ( 'NONE', *, *, #108085, .F. ) ;
#84799 = ORIENTED_EDGE ( 'NONE', *, *, #28506, .F. ) ;
#84800 = EDGE_CURVE ( 'NONE', #41198, #101203, #61165, .T. ) ;
#84801 = VECTOR ( 'NONE', #3127, 999.9999999999998863 ) ;
#84802 = CARTESIAN_POINT ( 'NONE',  ( 34.42499999999998295, -21.72500000000000142, 5.000000000000000000 ) ) ;
#84803 = CARTESIAN_POINT ( 'NONE',  ( -20.84387692260743918, -22.22500000000000142, 4.000000000000000000 ) ) ;
#84804 = CARTESIAN_POINT ( 'NONE',  ( 3.299744871391591339, -27.71228299555208352, 4.000000000000000000 ) ) ;
#84805 = VECTOR ( 'NONE', #102067, 999.9999999999998863 ) ;
#84806 = DIRECTION ( 'NONE',  ( -0.000000000000000000, 0.000000000000000000, 1.000000000000000000 ) ) ;
#84807 = CARTESIAN_POINT ( 'NONE',  ( 0.000000000000000000, 0.000000000000000000, 5.000000000000000000 ) ) ;
#84808 = PLANE ( 'NONE',  #34377 ) ;
#84810 = CARTESIAN_POINT ( 'NONE',  ( -24.75860074219779605, 21.72500000000000853, 5.000000000000000000 ) ) ;
#84809 = PLANE ( 'NONE',  #29583 ) ;
#84811 = CARTESIAN_POINT ( 'NONE',  ( -12.48921356237309155, -27.52281430457064104, 5.000000000000000000 ) ) ;
#84812 = CARTESIAN_POINT ( 'NONE',  ( 38.99451991528749062, 28.92564299267965211, 4.000000000000000000 ) ) ;
#84813 = CARTESIAN_POINT ( 'NONE',  ( 33.29974487139158867, -27.71228299555229313, 4.000000000000000000 ) ) ;
#84814 = DIRECTION ( 'NONE',  ( -1.000000000000000000, -1.224606353822377258E-16, -0.000000000000000000 ) ) ;
#84815 = VECTOR ( 'NONE', #11289, 1000.000000000000000 ) ;
#84816 = EDGE_CURVE ( 'NONE', #49512, #79543, #83597, .T. ) ;
#84817 = ORIENTED_EDGE ( 'NONE', *, *, #129572, .F. ) ;
#84818 = ORIENTED_EDGE ( 'NONE', *, *, #122931, .T. ) ;
#84819 = ORIENTED_EDGE ( 'NONE', *, *, #3223, .F. ) ;
#84820 = ORIENTED_EDGE ( 'NONE', *, *, #10092, .F. ) ;
#84821 = DIRECTION ( 'NONE',  ( 0.6830127018922181881, 0.6830127018922202975, -0.2588190451025214056 ) ) ;
#84822 = ORIENTED_EDGE ( 'NONE', *, *, #49900, .F. ) ;
#84823 = ORIENTED_EDGE ( 'NONE', *, *, #35640, .F. ) ;
#84824 = DIRECTION ( 'NONE',  ( -0.7071067811865487940, 0.7071067811865463515, 0.000000000000000000 ) ) ;
#84825 = FACE_OUTER_BOUND ( 'NONE', #21903, .T. ) ;
#84826 = VECTOR ( 'NONE', #103455, 1000.000000000000000 ) ;
#84827 = ADVANCED_FACE ( 'NONE', ( #95866 ), #42231, .F. ) ;
#84828 = DIRECTION ( 'NONE',  ( 0.7071067811865487940, 0.7071067811865463515, 0.000000000000000000 ) ) ;
#84829 = ORIENTED_EDGE ( 'NONE', *, *, #6836, .T. ) ;
#84830 = DIRECTION ( 'NONE',  ( -0.3543493200069162685, -0.000000000000000000, -0.9351131265310288487 ) ) ;
#84831 = VERTEX_POINT ( 'NONE', #120434 ) ;
#84832 = AXIS2_PLACEMENT_3D ( 'NONE', #117013, #20538, #8222 ) ;
#84834 = DIRECTION ( 'NONE',  ( -0.7071067811865486830, 0.7071067811865464625, 0.000000000000000000 ) ) ;
#84833 = VECTOR ( 'NONE', #26995, 1000.000000000000000 ) ;
#84835 = LINE ( 'NONE', #52886, #38085 ) ;
#84836 = VECTOR ( 'NONE', #79568, 1000.000000000000227 ) ;
#84837 = CARTESIAN_POINT ( 'NONE',  ( 11.87956980810188767, 3.967499999999998916, 6.871911579029510442 ) ) ;
#84838 = ORIENTED_EDGE ( 'NONE', *, *, #117272, .F. ) ;
#84839 = CARTESIAN_POINT ( 'NONE',  ( 88.87043019189810877, -3.055000000000001936, 5.291415217122918513 ) ) ;
#84840 = CARTESIAN_POINT ( 'NONE',  ( 19.04500000000000881, 3.130000000000007887, -22.35000000000000142 ) ) ;
#84841 = ORIENTED_EDGE ( 'NONE', *, *, #50801, .T. ) ;
#84842 = ORIENTED_EDGE ( 'NONE', *, *, #34294, .F. ) ;
#84843 = CARTESIAN_POINT ( 'NONE',  ( -20.20710678118640757, 15.75929247661555976, 5.000000000000000000 ) ) ;
#84844 = EDGE_LOOP ( 'NONE', ( #90944, #74680, #121498 ) ) ;
#84845 = DIRECTION ( 'NONE',  ( 0.7071067811865487940, 0.7071067811865463515, -0.000000000000000000 ) ) ;
#84846 = FACE_OUTER_BOUND ( 'NONE', #56855, .T. ) ;
#84847 = VECTOR ( 'NONE', #6378, 999.9999999999998863 ) ;
#84848 = DIRECTION ( 'NONE',  ( -0.7071067811865487940, 0.7071067811865463515, 0.000000000000000000 ) ) ;
#84849 = DIRECTION ( 'NONE',  ( 0.7071067811865486830, -0.7071067811865464625, -0.000000000000000000 ) ) ;
#84850 = ORIENTED_EDGE ( 'NONE', *, *, #85678, .T. ) ;
#84851 = CARTESIAN_POINT ( 'NONE',  ( 77.99451991528749772, 28.92564299267992567, 4.000000000000000000 ) ) ;
#84852 = EDGE_CURVE ( 'NONE', #73074, #108741, #25022, .T. ) ;
#84853 = PLANE ( 'NONE',  #39708 ) ;
#84854 = FACE_OUTER_BOUND ( 'NONE', #142530, .T. ) ;
#84855 = ORIENTED_EDGE ( 'NONE', *, *, #125888, .T. ) ;
#84856 = PLANE ( 'NONE',  #28169 ) ;
#84857 = DIRECTION ( 'NONE',  ( 0.7071067811865486830, -0.7071067811865464625, -0.000000000000000000 ) ) ;
#84858 = ORIENTED_EDGE ( 'NONE', *, *, #50535, .F. ) ;
#84859 = EDGE_CURVE ( 'NONE', #143176, #48427, #64680, .T. ) ;
#84861 = ORIENTED_EDGE ( 'NONE', *, *, #133193, .T. ) ;
#84860 = DIRECTION ( 'NONE',  ( -0.7071067811865486830, 0.7071067811865464625, 0.000000000000000000 ) ) ;
#84862 = VERTEX_POINT ( 'NONE', #74128 ) ;
#84863 = EDGE_CURVE ( 'NONE', #55719, #7189, #98022, .T. ) ;
#84864 = LINE ( 'NONE', #11549, #104918 ) ;
#84865 = CARTESIAN_POINT ( 'NONE',  ( -5.999999999999960032, -3.485240976185084882, -4.108735105802409748 ) ) ;
#84866 = ORIENTED_EDGE ( 'NONE', *, *, #51620, .T. ) ;
#84867 = DIRECTION ( 'NONE',  ( 0.7071067811865487940, -0.7071067811865463515, 0.000000000000000000 ) ) ;
#84868 = CARTESIAN_POINT ( 'NONE',  ( -24.21271579574130683, 0.1791150535437372460, 5.000000000000000000 ) ) ;
#84869 = AXIS2_PLACEMENT_3D ( 'NONE', #15093, #103524, #60808 ) ;
#84870 = PLANE ( 'NONE',  #55355 ) ;
#84871 = EDGE_CURVE ( 'NONE', #104733, #60519, #65742, .T. ) ;
#84872 = CARTESIAN_POINT ( 'NONE',  ( 0.000000000000000000, 0.000000000000000000, 5.000000000000000000 ) ) ;
#84873 = CARTESIAN_POINT ( 'NONE',  ( 23.99999999999984013, 11.96639925780213964, 5.000000000000000000 ) ) ;
#84874 = CARTESIAN_POINT ( 'NONE',  ( -22.49999999999984723, -11.56887692260769640, 4.000000000000000000 ) ) ;
#84875 = CARTESIAN_POINT ( 'NONE',  ( 46.64583333333333570, 2.130196079827508360, -7.949999999999954881 ) ) ;
#84876 = PLANE ( 'NONE',  #132257 ) ;
#84877 = FACE_OUTER_BOUND ( 'NONE', #85711, .T. ) ;
#84879 = VECTOR ( 'NONE', #137890, 999.9999999999998863 ) ;
#84878 = CARTESIAN_POINT ( 'NONE',  ( 19.41999999999999815, 2.055000000000001492, 2.516649172247811554E-16 ) ) ;
#84880 = CARTESIAN_POINT ( 'NONE',  ( 26.77392480454907897, 6.350000000000003197, 1.166476076187854416E-15 ) ) ;
#84881 = DIRECTION ( 'NONE',  ( -1.301042606982605074E-16, 1.000000000000000000, 0.000000000000000000 ) ) ;
#84882 = DIRECTION ( 'NONE',  ( -0.000000000000000000, -0.3543493200069152693, 0.9351131265310292928 ) ) ;
#84883 = ORIENTED_EDGE ( 'NONE', *, *, #22758, .T. ) ;
#84884 = EDGE_CURVE ( 'NONE', #96223, #82006, #85979, .T. ) ;
#84885 = ORIENTED_EDGE ( 'NONE', *, *, #61737, .T. ) ;
#84886 = EDGE_LOOP ( 'NONE', ( #62024, #83049, #122148, #76543 ) ) ;
#84887 = CARTESIAN_POINT ( 'NONE',  ( 107.1666666666666572, 6.884901960086285300, 3.975000000000003642 ) ) ;
#84888 = ORIENTED_EDGE ( 'NONE', *, *, #82969, .T. ) ;
#84889 = ORIENTED_EDGE ( 'NONE', *, *, #135286, .T. ) ;
#84890 = VERTEX_POINT ( 'NONE', #40793 ) ;
#84891 = FACE_OUTER_BOUND ( 'NONE', #130869, .T. ) ;
#84892 = VERTEX_POINT ( 'NONE', #31341 ) ;
#84893 = CARTESIAN_POINT ( 'NONE',  ( 15.18079593298623564, 4.202752102959690472E-16, 0.000000000000000000 ) ) ;
#84894 = LINE ( 'NONE', #96445, #134355 ) ;
#84896 = AXIS2_PLACEMENT_3D ( 'NONE', #32737, #9501, #122560 ) ;
#84895 = LINE ( 'NONE', #106616, #111184 ) ;
#84897 = CARTESIAN_POINT ( 'NONE',  ( -0.7928932188134485415, 15.75929247661555443, 5.000000000000000000 ) ) ;
#84898 = CARTESIAN_POINT ( 'NONE',  ( 106.3129301918981042, -1.637169565754159617, -6.110000000000001208 ) ) ;
#84899 = ORIENTED_EDGE ( 'NONE', *, *, #10991, .T. ) ;
#84900 = CARTESIAN_POINT ( 'NONE',  ( 34.92499999999998295, 22.22500000000000142, 4.500000000000000888 ) ) ;
#84901 = CARTESIAN_POINT ( 'NONE',  ( -6.640000000000001457, -34.51840020119762187, 17.97447928118982929 ) ) ;
#84902 = CARTESIAN_POINT ( 'NONE',  ( -2.999999999999973355, 2.587461875839211167, 4.000000000000000000 ) ) ;
#84903 = DIRECTION ( 'NONE',  ( -1.000000000000000000, -0.000000000000000000, -0.000000000000000000 ) ) ;
#84904 = DIRECTION ( 'NONE',  ( 0.6830127018922181881, 0.6830127018922202975, -0.2588190451025214056 ) ) ;
#84905 = SURFACE_STYLE_FILL_AREA ( #140700 ) ;
#84906 = PLANE ( 'NONE',  #12702 ) ;
#84907 = CIRCLE ( 'NONE', #75707, 2.500000000000000444 ) ;
#84908 = PLANE ( 'NONE',  #30530 ) ;
#84909 = LINE ( 'NONE', #7324, #69447 ) ;
#84910 = ORIENTED_EDGE ( 'NONE', *, *, #60055, .F. ) ;
#84911 = ORIENTED_EDGE ( 'NONE', *, *, #36778, .T. ) ;
#84912 = ADVANCED_FACE ( 'NONE', ( #19728 ), #108856, .T. ) ;
#84913 = CARTESIAN_POINT ( 'NONE',  ( 27.68749999999998579, -5.819803920172573086, 5.819803920172572198 ) ) ;
#84914 = CIRCLE ( 'NONE', #133557, 2.055000000000001048 ) ;
#84915 = ORIENTED_EDGE ( 'NONE', *, *, #51267, .T. ) ;
#84916 = FACE_OUTER_BOUND ( 'NONE', #120975, .T. ) ;
#84917 = EDGE_CURVE ( 'NONE', #110456, #135979, #53063, .T. ) ;
#84918 = CARTESIAN_POINT ( 'NONE',  ( -30.70710678118632231, -0.7407075233842788098, 5.000000000000000000 ) ) ;
#84919 = CARTESIAN_POINT ( 'NONE',  ( -25.39999999999996305, 0.000000000000000000, 0.000000000000000000 ) ) ;
#84921 = EDGE_CURVE ( 'NONE', #113570, #48874, #84995, .T. ) ;
#84920 = CARTESIAN_POINT ( 'NONE',  ( 15.18398860626900237, 28.73617430169797871, 5.000000000000000000 ) ) ;
#84922 = EDGE_CURVE ( 'NONE', #35574, #16896, #10273, .T. ) ;
#84923 = CARTESIAN_POINT ( 'NONE',  ( -34.92500000000001137, -22.22500000000000142, 4.000000000000000000 ) ) ;
#84924 = CARTESIAN_POINT ( 'NONE',  ( -39.18398860626899705, 28.73617430169814568, 5.000000000000000000 ) ) ;
#84925 = CARTESIAN_POINT ( 'NONE',  ( 123.1412635252314374, 4.472830434245836706, 4.472830434245840259 ) ) ;
#84926 = ORIENTED_EDGE ( 'NONE', *, *, #30094, .T. ) ;
#84927 = LINE ( 'NONE', #129139, #135868 ) ;
#84928 = ORIENTED_EDGE ( 'NONE', *, *, #43361, .F. ) ;
#84929 = FACE_OUTER_BOUND ( 'NONE', #14686, .T. ) ;
#84930 = DIRECTION ( 'NONE',  ( -0.7071067811865486830, 0.7071067811865464625, 0.000000000000000000 ) ) ;
#84931 = CARTESIAN_POINT ( 'NONE',  ( 32.71998032010576196, 0.7592924766157138627, 14.27032725228016474 ) ) ;
#84932 = CARTESIAN_POINT ( 'NONE',  ( 29.20666063542132207, 21.75929247661549581, 4.998822639870703632 ) ) ;
#84933 = VERTEX_POINT ( 'NONE', #107452 ) ;
#84935 = EDGE_CURVE ( 'NONE', #127280, #52226, #9547, .T. ) ;
#84934 = CARTESIAN_POINT ( 'NONE',  ( 48.41709685856476852, 3.054999999999998828, 5.291415217122922066 ) ) ;
#84936 = ORIENTED_EDGE ( 'NONE', *, *, #3516, .F. ) ;
#84937 = DIRECTION ( 'NONE',  ( -0.7071067811865486830, -0.7071067811865464625, -0.000000000000000000 ) ) ;
#84938 = ADVANCED_FACE ( 'NONE', ( #52362 ), #40106, .F. ) ;
#84939 = CARTESIAN_POINT ( 'NONE',  ( 36.48921356237310221, -27.52281430457080802, 5.000000000000000000 ) ) ;
#84940 = LINE ( 'NONE', #73372, #138134 ) ;
#84941 = FACE_OUTER_BOUND ( 'NONE', #96091, .T. ) ;
#84942 = AXIS2_PLACEMENT_3D ( 'NONE', #118258, #105950, #141468 ) ;
#84943 = CONICAL_SURFACE ( 'NONE', #133593, 2.055000000000001048, 0.9599310885968758145 ) ;
#84944 = VECTOR ( 'NONE', #11059, 1000.000000000000000 ) ;
#84945 = EDGE_CURVE ( 'NONE', #76170, #98656, #119044, .T. ) ;
#84946 = CARTESIAN_POINT ( 'NONE',  ( 42.64126352523145158, 4.472830434245836706, 4.472830434245840259 ) ) ;
#84947 = VERTEX_POINT ( 'NONE', #119732 ) ;
#84948 = AXIS2_PLACEMENT_3D ( 'NONE', #28929, #82598, #92740 ) ;
#84949 = LINE ( 'NONE', #118265, #22397 ) ;
#84950 = ORIENTED_EDGE ( 'NONE', *, *, #3880, .F. ) ;
#84951 = EDGE_LOOP ( 'NONE', ( #19106, #111812, #107784, #35262 ) ) ;
#84952 = AXIS2_PLACEMENT_3D ( 'NONE', #95799, #108067, #139346 ) ;
#84953 = EDGE_CURVE ( 'NONE', #1660, #35704, #32045, .T. ) ;
#84954 = ORIENTED_EDGE ( 'NONE', *, *, #73083, .T. ) ;
#84955 = DIRECTION ( 'NONE',  ( 0.7071067811865487940, -0.7071067811865463515, 0.000000000000000000 ) ) ;
#84956 = ORIENTED_EDGE ( 'NONE', *, *, #94309, .T. ) ;
#84957 = ADVANCED_FACE ( 'NONE', ( #117588 ), #76277, .F. ) ;
#84958 = LINE ( 'NONE', #129164, #94528 ) ;
#84959 = CARTESIAN_POINT ( 'NONE',  ( 174.7500000000000000, 7.919999999999947526, -21.52769999999994965 ) ) ;
#84960 = FACE_BOUND ( 'NONE', #110240, .T. ) ;
#84961 = ORIENTED_EDGE ( 'NONE', *, *, #40496, .T. ) ;
#84962 = FACE_OUTER_BOUND ( 'NONE', #119960, .T. ) ;
#84963 = DIRECTION ( 'NONE',  ( 0.7071067811865486830, -0.7071067811865464625, -0.000000000000000000 ) ) ;
#84964 = FACE_OUTER_BOUND ( 'NONE', #11629, .T. ) ;
#84965 = ORIENTED_EDGE ( 'NONE', *, *, #51208, .T. ) ;
#84966 = CARTESIAN_POINT ( 'NONE',  ( 16.75173015016484968, -2.055000000000000160, 0.000000000000000000 ) ) ;
#84967 = VERTEX_POINT ( 'NONE', #1518 ) ;
#84969 = EDGE_CURVE ( 'NONE', #101903, #142842, #77705, .T. ) ;
#84968 = VECTOR ( 'NONE', #91763, 1000.000000000000000 ) ;
#84970 = ORIENTED_EDGE ( 'NONE', *, *, #23717, .T. ) ;
#84971 = LINE ( 'NONE', #95120, #74910 ) ;
#84972 = ORIENTED_EDGE ( 'NONE', *, *, #70273, .T. ) ;
#84973 = ADVANCED_FACE ( 'NONE', ( #100170 ), #121180, .T. ) ;
#84974 = CARTESIAN_POINT ( 'NONE',  ( 58.53709685856478728, -3.054999999999998828, -5.291415217122919401 ) ) ;
#84975 = VECTOR ( 'NONE', #394, 999.9999999999998863 ) ;
#84976 = EDGE_LOOP ( 'NONE', ( #24216, #131151, #81419, #36731 ) ) ;
#84977 = CARTESIAN_POINT ( 'NONE',  ( -19.49999999999986500, 21.05218569542895679, 5.000000000000000000 ) ) ;
#84978 = DIRECTION ( 'NONE',  ( -0.6830127018922180770, -0.6830127018922204085, -0.2588190451025213501 ) ) ;
#84979 = ORIENTED_EDGE ( 'NONE', *, *, #27720, .T. ) ;
#84980 = CARTESIAN_POINT ( 'NONE',  ( 25.49999999999981526, 7.087461875839178305, 4.000000000000000000 ) ) ;
#84981 = STYLED_ITEM ( 'NONE', ( #123586 ), #13691 ) ;
#84982 = ADVANCED_FACE ( 'NONE', ( #11679 ), #112463, .F. ) ;
#84983 = PLANE ( 'NONE',  #73342 ) ;
#84984 = DIRECTION ( 'NONE',  ( -0.000000000000000000, -0.3543493200069152693, 0.9351131265310292928 ) ) ;
#84985 = CARTESIAN_POINT ( 'NONE',  ( 33.72281430457037743, -21.72499999999999432, 5.000000000000000000 ) ) ;
#84986 = CARTESIAN_POINT ( 'NONE',  ( -24.29974487139158867, -27.71228299555223273, 4.000000000000000000 ) ) ;
#84987 = ORIENTED_EDGE ( 'NONE', *, *, #9853, .T. ) ;
#84988 = VECTOR ( 'NONE', #111649, 1000.000000000000000 ) ;
#84989 = ORIENTED_EDGE ( 'NONE', *, *, #111411, .T. ) ;
#84990 = CARTESIAN_POINT ( 'NONE',  ( -23.99451991528749062, 28.92564299267954908, 4.000000000000000000 ) ) ;
#84991 = DIRECTION ( 'NONE',  ( 0.6830127018922181881, 0.6830127018922202975, -0.2588190451025214056 ) ) ;
#84992 = ORIENTED_EDGE ( 'NONE', *, *, #57272, .F. ) ;
#84993 = VERTEX_POINT ( 'NONE', #45108 ) ;
#84994 = VERTEX_POINT ( 'NONE', #133508 ) ;
#84995 = LINE ( 'NONE', #7413, #32811 ) ;
#84996 = CARTESIAN_POINT ( 'NONE',  ( 26.99999999999981171, -12.41253812416062985, 4.000000000000000000 ) ) ;
#84997 = ORIENTED_EDGE ( 'NONE', *, *, #18424, .F. ) ;
#84998 = CARTESIAN_POINT ( 'NONE',  ( 25.39999999999999858, -14.29000000000013593, 12.69999999999954632 ) ) ;
#84999 =( NAMED_UNIT ( * ) PLANE_ANGLE_UNIT ( ) SI_UNIT ( $, .RADIAN. ) );
#85000 = CARTESIAN_POINT ( 'NONE',  ( 20.04623647476855197, -7.934999999999990727, 4.858786175617117713E-16 ) ) ;
#85001 = LINE ( 'NONE', #63298, #79666 ) ;
#85002 = VERTEX_POINT ( 'NONE', #2228 ) ;
#85003 = CARTESIAN_POINT ( 'NONE',  ( 124.5995968585647944, -6.109999999999998543, -1.637169565754160727 ) ) ;
#85004 = VECTOR ( 'NONE', #61809, 1000.000000000000000 ) ;
#85006 = EDGE_CURVE ( 'NONE', #143110, #70428, #135301, .T. ) ;
#85005 = CARTESIAN_POINT ( 'NONE',  ( -12.69999999999998153, -0.4000000000000004108, 2.467792535850613866 ) ) ;
#85007 = CARTESIAN_POINT ( 'NONE',  ( -33.29974487139158867, -27.71228299555229313, 4.000000000000000000 ) ) ;
#85009 = EDGE_LOOP ( 'NONE', ( #137492, #25948, #36377, #7829 ) ) ;
#85008 = DIRECTION ( 'NONE',  ( -0.000000000000000000, 0.3543493200069153248, 0.9351131265310292928 ) ) ;
#85010 = DIRECTION ( 'NONE',  ( -0.000000000000000000, 0.000000000000000000, 1.000000000000000000 ) ) ;
#85011 = ORIENTED_EDGE ( 'NONE', *, *, #3822, .T. ) ;
#85012 = CARTESIAN_POINT ( 'NONE',  ( 75.32919371712957002, -3.975000000000001865, 6.884901960086284411 ) ) ;
#85013 = DIRECTION ( 'NONE',  ( 0.7071067811865486830, -0.7071067811865464625, -0.000000000000000000 ) ) ;
#85014 = DIRECTION ( 'NONE',  ( 0.000000000000000000, -1.000000000000000000, 0.000000000000000000 ) ) ;
#85015 = ORIENTED_EDGE ( 'NONE', *, *, #14695, .F. ) ;
#85016 = PLANE ( 'NONE',  #19462 ) ;
#85017 = FACE_OUTER_BOUND ( 'NONE', #65526, .T. ) ;
#85018 = CARTESIAN_POINT ( 'NONE',  ( -19.39744865953807818, 0.5628245286959329130, -30.75764528037382561 ) ) ;
#85019 = ORIENTED_EDGE ( 'NONE', *, *, #76377, .T. ) ;
#85020 = CARTESIAN_POINT ( 'NONE',  ( 48.29974487139158867, -27.71228299555239971, 4.000000000000000000 ) ) ;
#85021 = CARTESIAN_POINT ( 'NONE',  ( -11.99999999999991296, -7.447814304570750998, 5.000000000000000000 ) ) ;
#85022 = DIRECTION ( 'NONE',  ( -1.000000000000000000, -1.224606353822377258E-16, -0.000000000000000000 ) ) ;
#85023 = PLANE ( 'NONE',  #116600 ) ;
#85024 = VECTOR ( 'NONE', #118814, 1000.000000000000000 ) ;
#85025 = DIRECTION ( 'NONE',  ( 0.7071067811865486830, -0.7071067811865464625, -0.000000000000000000 ) ) ;
#85026 = EDGE_CURVE ( 'NONE', #118046, #135054, #134960, .T. ) ;
#85027 = ORIENTED_EDGE ( 'NONE', *, *, #39376, .T. ) ;
#85029 = ORIENTED_EDGE ( 'NONE', *, *, #103889, .T. ) ;
#85028 = EDGE_CURVE ( 'NONE', #90677, #23319, #124053, .T. ) ;
#85030 = DIRECTION ( 'NONE',  ( 0.7071067811865486830, -0.7071067811865464625, -0.000000000000000000 ) ) ;
#85031 = DIRECTION ( 'NONE',  ( -0.7071067811865486830, -0.7071067811865464625, 0.000000000000000000 ) ) ;
#85032 = VECTOR ( 'NONE', #12720, 1000.000000000000000 ) ;
#85034 = EDGE_CURVE ( 'NONE', #49673, #9354, #12419, .T. ) ;
#85033 = VECTOR ( 'NONE', #73205, 999.9999999999998863 ) ;
#85035 = CARTESIAN_POINT ( 'NONE',  ( 11.93706980810188689, 2.126176841940952134, -7.934999999999993392 ) ) ;
#85036 = LINE ( 'NONE', #16178, #75956 ) ;
#85037 = AXIS2_PLACEMENT_3D ( 'NONE', #64598, #87066, #22483 ) ;
#85038 = CARTESIAN_POINT ( 'NONE',  ( 14.99999999999989519, 7.559798855135672291, 4.979909187984731922 ) ) ;
#85039 = CARTESIAN_POINT ( 'NONE',  ( 0.000000000000000000, 0.000000000000000000, 0.000000000000000000 ) ) ;
#85040 = EDGE_LOOP ( 'NONE', ( #108961, #57259, #53216, #85382 ) ) ;
#85041 = ADVANCED_FACE ( 'NONE', ( #24727 ), #7302, .F. ) ;
#85042 = CARTESIAN_POINT ( 'NONE',  ( 26.99999999999999645, 5.837062628940091535, 2.500239961634333596 ) ) ;
#85043 = FACE_OUTER_BOUND ( 'NONE', #131212, .T. ) ;
#85044 = LINE ( 'NONE', #53873, #109544 ) ;
#85045 = VECTOR ( 'NONE', #78896, 999.9999999999998863 ) ;
#85046 = PLANE ( 'NONE',  #25153 ) ;
#85047 = CARTESIAN_POINT ( 'NONE',  ( 35.93293019189811588, 1.637169565754156730, 6.110000000000001208 ) ) ;
#85048 = CARTESIAN_POINT ( 'NONE',  ( 12.18398860626900060, 28.73617430169795739, 5.000000000000000000 ) ) ;
#85049 = ADVANCED_FACE ( 'NONE', ( #91432 ), #25429, .F. ) ;
#85050 = ORIENTED_EDGE ( 'NONE', *, *, #29537, .F. ) ;
#85051 = CARTESIAN_POINT ( 'NONE',  ( 0.000000000000000000, 0.000000000000000000, 5.000000000000000000 ) ) ;
#85052 = ORIENTED_EDGE ( 'NONE', *, *, #127825, .F. ) ;
#85053 = EDGE_LOOP ( 'NONE', ( #132481, #139197, #131941, #88958 ) ) ;
#85054 = LINE ( 'NONE', #28556, #112626 ) ;
#85055 = CARTESIAN_POINT ( 'NONE',  ( -29.99999999999979039, 4.384688058510544550, -7.090945410444755126 ) ) ;
#85056 = ADVANCED_FACE ( 'NONE', ( #104420 ), #126194, .F. ) ;
#85057 = PLANE ( 'NONE',  #124793 ) ;
#85058 = CARTESIAN_POINT ( 'NONE',  ( -5.816011393731002066, 28.73617430169783304, 5.000000000000000000 ) ) ;
#85059 = DIRECTION ( 'NONE',  ( 0.7071067811865487940, 0.7071067811865463515, -0.000000000000000000 ) ) ;
#85060 = CARTESIAN_POINT ( 'NONE',  ( 0.000000000000000000, 0.000000000000000000, 5.000000000000000000 ) ) ;
#85061 = LINE ( 'NONE', #130002, #105593 ) ;
#85062 = ORIENTED_EDGE ( 'NONE', *, *, #25728, .T. ) ;
#85063 = CARTESIAN_POINT ( 'NONE',  ( 34.92499999999998295, 8.816654386410357702, 4.500000000000000888 ) ) ;
#85064 = DIRECTION ( 'NONE',  ( 0.7071067811865486830, -0.7071067811865464625, -0.000000000000000000 ) ) ;
#85065 = AXIS2_PLACEMENT_3D ( 'NONE', #85886, #64153, #5446 ) ;
#85066 = EDGE_CURVE ( 'NONE', #88846, #82235, #5083, .T. ) ;
#85067 = CARTESIAN_POINT ( 'NONE',  ( -34.92500000000001137, -22.22500000000000142, 4.000000000000000000 ) ) ;
#85068 = ADVANCED_FACE ( 'NONE', ( #127626 ), #26171, .F. ) ;
#85069 = FACE_OUTER_BOUND ( 'NONE', #88954, .T. ) ;
#85070 = DIRECTION ( 'NONE',  ( 0.000000000000000000, 0.000000000000000000, 1.000000000000000000 ) ) ;
#85071 = PLANE ( 'NONE',  #8696 ) ;
#85072 = CARTESIAN_POINT ( 'NONE',  ( 58.41252705046289151, -7.949999999999998401, -4.867971026610728450E-16 ) ) ;
#85073 = VECTOR ( 'NONE', #9201, 1000.000000000000000 ) ;
#85074 = CARTESIAN_POINT ( 'NONE',  ( -2.700255128608413990, -27.71228299555204089, 4.000000000000000000 ) ) ;
#85075 = EDGE_LOOP ( 'NONE', ( #15888, #128090, #48493, #134400, #136804, #70630 ) ) ;
#85076 = EDGE_LOOP ( 'NONE', ( #106926, #19572, #12800, #50128 ) ) ;
#85077 = CARTESIAN_POINT ( 'NONE',  ( 52.33333333333332860, -6.884901960086287964, 3.974999999999998312 ) ) ;
#85078 = CARTESIAN_POINT ( 'NONE',  ( -32.14114312045509081, 22.22500000000000142, 6.054907437694478034 ) ) ;
#85079 = CARTESIAN_POINT ( 'NONE',  ( 11.99451991528749417, 28.92564299267946382, 4.000000000000000000 ) ) ;
#85080 = EDGE_CURVE ( 'NONE', #109962, #119435, #60986, .T. ) ;
#85081 = VECTOR ( 'NONE', #63576, 1000.000000000000000 ) ;
#85082 = DIRECTION ( 'NONE',  ( -0.7071067811865487940, 0.7071067811865463515, -0.000000000000000000 ) ) ;
#85083 = VERTEX_POINT ( 'NONE', #80565 ) ;
#85085 = EDGE_CURVE ( 'NONE', #21635, #86313, #70437, .T. ) ;
#85084 = LINE ( 'NONE', #129289, #25929 ) ;
#85086 = EDGE_CURVE ( 'NONE', #113725, #130192, #49051, .T. ) ;
#85087 = CARTESIAN_POINT ( 'NONE',  ( 51.33376352523143282, 6.110000000000001208, 1.122388791418549305E-15 ) ) ;
#85088 = ORIENTED_EDGE ( 'NONE', *, *, #475, .T. ) ;
#85089 = DIRECTION ( 'NONE',  ( -0.7071067811865486830, -0.7071067811865464625, 0.000000000000000000 ) ) ;
#85090 = ORIENTED_EDGE ( 'NONE', *, *, #103393, .F. ) ;
#85091 = ORIENTED_EDGE ( 'NONE', *, *, #58353, .T. ) ;
#85092 = PLANE ( 'NONE',  #116401 ) ;
#85093 = ADVANCED_FACE ( 'NONE', ( #114581 ), #93566, .F. ) ;
#85094 = DIRECTION ( 'NONE',  ( 0.7071067811865486830, -0.7071067811865464625, -0.000000000000000000 ) ) ;
#85095 = SURFACE_STYLE_USAGE ( .BOTH. , #29993 ) ;
#85096 = ORIENTED_EDGE ( 'NONE', *, *, #45079, .T. ) ;
#85097 = EDGE_CURVE ( 'NONE', #8017, #139436, #104596, .T. ) ;
#85098 = CARTESIAN_POINT ( 'NONE',  ( 1.629999999999999893, 0.3999999999999995226, 2.303088455023526215 ) ) ;
#85100 = EDGE_LOOP ( 'NONE', ( #65900, #19919, #115296, #71650, #98515 ) ) ;
#85099 = LINE ( 'NONE', #95967, #103127 ) ;
#85101 = DIRECTION ( 'NONE',  ( 0.000000000000000000, 1.000000000000000000, 0.000000000000000000 ) ) ;
#85102 = CARTESIAN_POINT ( 'NONE',  ( 27.32816939922333432, 11.25929247661560950, 4.000000000000000000 ) ) ;
#85103 = DIRECTION ( 'NONE',  ( -0.7071067811865487940, 0.7071067811865463515, 0.000000000000000000 ) ) ;
#85104 = CARTESIAN_POINT ( 'NONE',  ( 2.999999999999983569, -0.4125381241607568028, 4.000000000000000000 ) ) ;
#85105 = VERTEX_POINT ( 'NONE', #50071 ) ;
#85106 = ORIENTED_EDGE ( 'NONE', *, *, #49012, .T. ) ;
#85107 = STYLED_ITEM ( 'NONE', ( #22886 ), #93057 ) ;
#85108 = ADVANCED_FACE ( 'NONE', ( #138501 ), #37033, .F. ) ;
#85109 =( LENGTH_UNIT ( ) NAMED_UNIT ( * ) SI_UNIT ( .MILLI., .METRE. ) );
#85110 = CARTESIAN_POINT ( 'NONE',  ( 63.05793019189810877, 6.110000000000000320, -1.637169565754156064 ) ) ;
#85111 = DIRECTION ( 'NONE',  ( -0.000000000000000000, 0.000000000000000000, 1.000000000000000000 ) ) ;
#85112 = CARTESIAN_POINT ( 'NONE',  ( -57.18398860626899705, 28.73617430169827358, 5.000000000000000000 ) ) ;
#85113 = DIRECTION ( 'NONE',  ( 1.000000000000000000, 0.000000000000000000, 0.000000000000000000 ) ) ;
#85114 = ORIENTED_EDGE ( 'NONE', *, *, #131351, .F. ) ;
#85115 = ORIENTED_EDGE ( 'NONE', *, *, #33104, .T. ) ;
#85116 = DIRECTION ( 'NONE',  ( 0.3543493200069162685, -0.000000000000000000, -0.9351131265310288487 ) ) ;
#85117 = EDGE_CURVE ( 'NONE', #69618, #42560, #39188, .T. ) ;
#85118 = ORIENTED_EDGE ( 'NONE', *, *, #1478, .T. ) ;
#85119 = ORIENTED_EDGE ( 'NONE', *, *, #13618, .F. ) ;
#85120 = CIRCLE ( 'NONE', #6310, 2.500000000000000888 ) ;
#85121 = DIRECTION ( 'NONE',  ( -0.6830127018922180770, -0.6830127018922204085, -0.2588190451025213501 ) ) ;
#85122 = ORIENTED_EDGE ( 'NONE', *, *, #98737, .T. ) ;
#85123 = CARTESIAN_POINT ( 'NONE',  ( 65.75000000000000000, -9.735942053221458872E-16, 7.950000000000000178 ) ) ;
#85124 = PLANE ( 'NONE',  #75735 ) ;
#85125 = CIRCLE ( 'NONE', #38877, 28.00000000000002487 ) ;
#85126 = PLANE ( 'NONE',  #4784 ) ;
#85127 = VECTOR ( 'NONE', #80173, 1000.000000000000000 ) ;
#85128 = FACE_BOUND ( 'NONE', #31637, .T. ) ;
#85129 = CARTESIAN_POINT ( 'NONE',  ( -10.77325839282159592, -11.24070752338416135, 18.24660765846980226 ) ) ;
#85130 = CARTESIAN_POINT ( 'NONE',  ( 40.32919371712954870, -3.975000000000001865, 6.884901960086284411 ) ) ;
#85131 = CARTESIAN_POINT ( 'NONE',  ( -2.186508646023597624, -15.74070752338412760, 8.904080028138945835 ) ) ;
#85133 = ORIENTED_EDGE ( 'NONE', *, *, #24714, .T. ) ;
#85132 = CARTESIAN_POINT ( 'NONE',  ( 7.139999999999956160, -60.26999999999998892, -7.899272885403742173 ) ) ;
#85134 = AXIS2_PLACEMENT_3D ( 'NONE', #126847, #40592, #29678 ) ;
#85135 = VECTOR ( 'NONE', #40073, 1000.000000000000227 ) ;
#85136 = PLANE ( 'NONE',  #101930 ) ;
#85137 = ORIENTED_EDGE ( 'NONE', *, *, #26978, .T. ) ;
#85138 = EDGE_CURVE ( 'NONE', #78369, #125176, #4333, .T. ) ;
#85139 = EDGE_LOOP ( 'NONE', ( #113728, #8368, #92478, #48992 ) ) ;
#85140 = CARTESIAN_POINT ( 'NONE',  ( 82.01626352523143737, -4.472830434245838482, 4.472830434245838482 ) ) ;
#85141 = ORIENTED_EDGE ( 'NONE', *, *, #71450, .F. ) ;
#85142 = DIRECTION ( 'NONE',  ( 1.000000000000000000, 0.000000000000000000, 0.000000000000000000 ) ) ;
#85143 = CARTESIAN_POINT ( 'NONE',  ( 18.01107201284014536, 2.499999999999998224, 3.061616997868380183E-16 ) ) ;
#85144 = DIRECTION ( 'NONE',  ( 0.7071067811865486830, -0.7071067811865464625, -0.000000000000000000 ) ) ;
#85145 = DIRECTION ( 'NONE',  ( 0.7071067811865487940, 0.7071067811865463515, 0.000000000000000000 ) ) ;
#85146 = CARTESIAN_POINT ( 'NONE',  ( 24.18398860626899705, 28.73617430169804265, 5.000000000000000000 ) ) ;
#85147 = DIRECTION ( 'NONE',  ( 0.7071067811865487940, -0.7071067811865463515, 0.000000000000000000 ) ) ;
#85148 = FACE_OUTER_BOUND ( 'NONE', #63144, .T. ) ;
#85149 = PLANE ( 'NONE',  #32359 ) ;
#85150 = CARTESIAN_POINT ( 'NONE',  ( 0.000000000000000000, 0.000000000000000000, 5.000000000000000000 ) ) ;
#85151 = ORIENTED_EDGE ( 'NONE', *, *, #142880, .T. ) ;
#85152 = CARTESIAN_POINT ( 'NONE',  ( -28.49999999999980460, -8.568876922607733704, 4.000000000000000000 ) ) ;
#85153 =( BOUNDED_CURVE ( )  B_SPLINE_CURVE ( 2, ( #102366, #110513, #86667, #76511, #54754, #33724, #130893, #99649, #14617, #103058, #33022, #119951, #10495 ),
 .UNSPECIFIED., .F., .T. ) 
 B_SPLINE_CURVE_WITH_KNOTS ( ( 3, 2, 2, 2, 2, 2, 3 ),
 ( 0.7000000000000000666, 0.7027777777777778345, 0.7055555555555557135, 0.7083333333333334814, 0.7111111111111112493, 0.7138888888888890172, 0.7166666666666667851 ),
 .UNSPECIFIED. ) 
 CURVE ( )  GEOMETRIC_REPRESENTATION_ITEM ( )  RATIONAL_B_SPLINE_CURVE ( ( 0.9999999999999986677, 0.9659258262890696445, 1.000000000000000000, 0.9659258262890683122, 1.000000000000000000, 0.9659258262890683122, 1.000000000000000000, 0.9659258262890683122, 1.000000000000000000, 0.9659258262890683122, 1.000000000000000000, 0.9659258262890669799, 1.000000000000001332 ) ) 
 REPRESENTATION_ITEM ( '' )  );
#85154 = LINE ( 'NONE', #129367, #23423 ) ;
#85155 = EDGE_LOOP ( 'NONE', ( #51518, #29053, #115908, #121309 ) ) ;
#85156 = VERTEX_POINT ( 'NONE', #48635 ) ;
#85157 = VERTEX_POINT ( 'NONE', #3648 ) ;
#85158 = CARTESIAN_POINT ( 'NONE',  ( 39.08376352523143282, -6.110000000000001208, -3.741295971395164515E-16 ) ) ;
#85159 = VECTOR ( 'NONE', #78395, 1000.000000000000000 ) ;
#85160 = ORIENTED_EDGE ( 'NONE', *, *, #19415, .T. ) ;
#85161 = CARTESIAN_POINT ( 'NONE',  ( 46.20833333333332149, -3.974999999999999201, -6.884901960086287964 ) ) ;
#85162 = CARTESIAN_POINT ( 'NONE',  ( 24.54580628287043709, 5.278424836066143655, -3.047499999999997655 ) ) ;
#85163 = CARTESIAN_POINT ( 'NONE',  ( 9.194147813897108890, 10.01345926878055792, -26.94908941227603094 ) ) ;
#85164 = EDGE_LOOP ( 'NONE', ( #133800, #42583, #119623, #43973, #85563 ) ) ;
#85165 = DIRECTION ( 'NONE',  ( 0.3543493200069162685, -0.000000000000000000, -0.9351131265310288487 ) ) ;
#85166 = ORIENTED_EDGE ( 'NONE', *, *, #59628, .T. ) ;
#85167 = CARTESIAN_POINT ( 'NONE',  ( 22.82816939922337340, 9.759292476615614831, 4.000000000000000000 ) ) ;
#85168 = DIRECTION ( 'NONE',  ( -0.7071067811865487940, 0.7071067811865463515, 0.000000000000000000 ) ) ;
#85170 = ORIENTED_EDGE ( 'NONE', *, *, #68662, .T. ) ;
#85169 = DIRECTION ( 'NONE',  ( -0.3543493200069162685, -0.000000000000000000, -0.9351131265310288487 ) ) ;
#85171 = ORIENTED_EDGE ( 'NONE', *, *, #74189, .T. ) ;
#85172 = LINE ( 'NONE', #120646, #90924 ) ;
#85173 = CARTESIAN_POINT ( 'NONE',  ( -4.809818324255480171, -18.74070752338408852, 7.910009926591521356 ) ) ;
#85174 = ORIENTED_EDGE ( 'NONE', *, *, #46855, .T. ) ;
#85175 = DIRECTION ( 'NONE',  ( -0.7071067811865486830, -0.7071067811865464625, -0.000000000000000000 ) ) ;
#85176 = EDGE_LOOP ( 'NONE', ( #117734, #75687, #137688, #30824 ) ) ;
#85177 = ORIENTED_EDGE ( 'NONE', *, *, #5956, .T. ) ;
#85178 = ORIENTED_EDGE ( 'NONE', *, *, #135104, .F. ) ;
#85179 = CARTESIAN_POINT ( 'NONE',  ( -31.92499999999997584, -6.270000000000012008, -37.00000000000000000 ) ) ;
#85180 = CYLINDRICAL_SURFACE ( 'NONE', #72359, 0.5000000000000004441 ) ;
#85181 = LINE ( 'NONE', #130151, #95443 ) ;
#85182 = EDGE_CURVE ( 'NONE', #9777, #44135, #137796, .T. ) ;
#85183 = CIRCLE ( 'NONE', #22657, 8.094999999999991758 ) ;
#85184 = CARTESIAN_POINT ( 'NONE',  ( -21.72281430457044493, -21.72500000000000142, 5.000000000000000000 ) ) ;
#85185 = CARTESIAN_POINT ( 'NONE',  ( -34.42500000000001137, -4.458600742197945443, 5.000000000000000000 ) ) ;
#85186 = EDGE_CURVE ( 'NONE', #56636, #874, #15952, .T. ) ;
#85188 = ORIENTED_EDGE ( 'NONE', *, *, #31553, .F. ) ;
#85187 = EDGE_CURVE ( 'NONE', #121799, #118878, #37773, .T. ) ;
#85189 = DIRECTION ( 'NONE',  ( -0.000000000000000000, 0.3543493200069153248, 0.9351131265310292928 ) ) ;
#85190 = ORIENTED_EDGE ( 'NONE', *, *, #9462, .F. ) ;
#85191 = CARTESIAN_POINT ( 'NONE',  ( 60.48921356237309510, -27.52281430457097500, 5.000000000000000000 ) ) ;
#85192 = ADVANCED_FACE ( 'NONE', ( #27569 ), #116002, .T. ) ;
#85193 = ADVANCED_FACE ( 'NONE', ( #129031 ), #28239, .T. ) ;
#85194 = CARTESIAN_POINT ( 'NONE',  ( 29.58290314143522082, 3.967499999999992699, -6.871911579029513994 ) ) ;
#85195 = ORIENTED_EDGE ( 'NONE', *, *, #73955, .F. ) ;
#85196 = LINE ( 'NONE', #129417, #69207 ) ;
#85197 = VECTOR ( 'NONE', #7400, 1000.000000000000000 ) ;
#85198 = LINE ( 'NONE', #30107, #60617 ) ;
#85199 = VERTEX_POINT ( 'NONE', #63806 ) ;
#85200 = ORIENTED_EDGE ( 'NONE', *, *, #82342, .T. ) ;
#85201 = EDGE_CURVE ( 'NONE', #30701, #91520, #119559, .T. ) ;
#85202 = DIRECTION ( 'NONE',  ( -0.7071067811865487940, 0.7071067811865463515, -0.000000000000000000 ) ) ;
#85203 = LINE ( 'NONE', #30111, #106715 ) ;
#85204 = PLANE ( 'NONE',  #81755 ) ;
#85205 = DIRECTION ( 'NONE',  ( -0.000000000000000000, -0.3543493200069153248, -0.9351131265310291818 ) ) ;
#85206 = CARTESIAN_POINT ( 'NONE',  ( 66.84959685856479439, 6.109999999999997655, 1.637169565754163836 ) ) ;
#85207 = CARTESIAN_POINT ( 'NONE',  ( -4.628234450443816428, -8.240707523384200428, 11.38925528200753590 ) ) ;
#85208 = EDGE_CURVE ( 'NONE', #51865, #72597, #7953, .T. ) ;
#85209 = FACE_OUTER_BOUND ( 'NONE', #49168, .T. ) ;
#85210 = CARTESIAN_POINT ( 'NONE',  ( 7.940000000000001279, -33.26999999999999602, -11.89864999999999462 ) ) ;
#85211 = CARTESIAN_POINT ( 'NONE',  ( 26.99451991528749417, 28.92564299267956685, 4.000000000000000000 ) ) ;
#85212 = EDGE_LOOP ( 'NONE', ( #125718, #28913, #42666, #67515 ) ) ;
#85213 = DIRECTION ( 'NONE',  ( -0.6830127018922180770, -0.6830127018922204085, -0.2588190451025213501 ) ) ;
#85214 = EDGE_LOOP ( 'NONE', ( #74965, #101048, #142522, #84356, #133869 ) ) ;
#85215 = DIRECTION ( 'NONE',  ( 0.000000000000000000, -1.000000000000000000, 0.000000000000000000 ) ) ;
#85216 = CARTESIAN_POINT ( 'NONE',  ( -5.510786437626906675, -27.52281430457051314, 5.000000000000000000 ) ) ;
#85217 = ORIENTED_EDGE ( 'NONE', *, *, #47757, .F. ) ;
#85218 = COLOUR_RGB ( '', 0.72549020, 0.75294118, 0.79215686) ;
#85219 = DIRECTION ( 'NONE',  ( -0.5735764363510499342, -0.8191520442889891340, 0.000000000000000000 ) ) ;
#85221 = VERTEX_POINT ( 'NONE', #6494 ) ;
#85220 = CARTESIAN_POINT ( 'NONE',  ( -34.92500000000001137, -18.18334561358938473, 4.500000000000000888 ) ) ;
#85222 = VECTOR ( 'NONE', #47402, 1000.000000000000000 ) ;
#85223 = CARTESIAN_POINT ( 'NONE',  ( 53.49999999999999289, 0.000000000000000000, -7.950000000000000178 ) ) ;
#85224 = LINE ( 'NONE', #86687, #10133 ) ;
#85225 = VERTEX_POINT ( 'NONE', #18837 ) ;
#85226 = VERTEX_POINT ( 'NONE', #118132 ) ;
#85227 =( NAMED_UNIT ( * ) PLANE_ANGLE_UNIT ( ) SI_UNIT ( $, .RADIAN. ) );
#85228 = DIRECTION ( 'NONE',  ( 0.000000000000000000, -1.000000000000000000, 0.000000000000000000 ) ) ;
#85229 = UNCERTAINTY_MEASURE_WITH_UNIT (LENGTH_MEASURE( 1.000000000000000082E-05 ), #73057, 'distance_accuracy_value', 'NONE');
#85230 = ADVANCED_FACE ( 'NONE', ( #31873 ), #63108, .T. ) ;
#85231 = VECTOR ( 'NONE', #72744, 1000.000000000000000 ) ;
#85232 = VECTOR ( 'NONE', #39896, 1000.000000000000000 ) ;
#85233 = CARTESIAN_POINT ( 'NONE',  ( 6.639999999999993463, -34.51840020119762897, 17.97447928118983285 ) ) ;
#85234 = CARTESIAN_POINT ( 'NONE',  ( 92.39169371712955581, 2.130196079827421762, 7.950000000000001066 ) ) ;
#85235 = PLANE ( 'NONE',  #18448 ) ;
#85236 = LINE ( 'NONE', #121439, #27492 ) ;
#85237 = ORIENTED_EDGE ( 'NONE', *, *, #10721, .T. ) ;
#85238 = CARTESIAN_POINT ( 'NONE',  ( -33.18398860626899705, 28.73617430169810305, 5.000000000000000000 ) ) ;
#85239 = CARTESIAN_POINT ( 'NONE',  ( 23.99999999999983658, -6.412538124160691133, 4.000000000000000000 ) ) ;
#85240 = CARTESIAN_POINT ( 'NONE',  ( 150.3000000000000114, 0.000000000000000000, 0.000000000000000000 ) ) ;
#85241 = EDGE_CURVE ( 'NONE', #76159, #104096, #73253, .T. ) ;
#85242 = LINE ( 'NONE', #16398, #97664 ) ;
#85243 = EDGE_LOOP ( 'NONE', ( #19225, #135096, #34910, #41966, #103616, #88477 ) ) ;
#85244 = EDGE_CURVE ( 'NONE', #94538, #42016, #105831, .T. ) ;
#85245 = ORIENTED_EDGE ( 'NONE', *, *, #118777, .T. ) ;
#85246 = CARTESIAN_POINT ( 'NONE',  ( 71.02126352523144703, -4.472830434245839371, -4.472830434245840259 ) ) ;
#85247 = EDGE_CURVE ( 'NONE', #142848, #80772, #142088, .T. ) ;
#85248 = PLANE ( 'NONE',  #75580 ) ;
#85249 = CARTESIAN_POINT ( 'NONE',  ( -26.29387692260786125, 22.22500000000000142, 4.000000000000000000 ) ) ;
#85250 = ORIENTED_EDGE ( 'NONE', *, *, #58773, .F. ) ;
#85251 = CARTESIAN_POINT ( 'NONE',  ( -15.51665438641034989, 22.22500000000000142, 4.500000000000000888 ) ) ;
#85253 = ADVANCED_FACE ( 'NONE', ( #117419 ), #96375, .T. ) ;
#85252 = VECTOR ( 'NONE', #68490, 1000.000000000000000 ) ;
#85254 = CARTESIAN_POINT ( 'NONE',  ( -27.18398860626900060, 28.73617430169806042, 5.000000000000000000 ) ) ;
#85255 = CARTESIAN_POINT ( 'NONE',  ( -8.999999999999936051, -18.41253812416056235, 4.000000000000000000 ) ) ;
#85257 = VERTEX_POINT ( 'NONE', #97846 ) ;
#85256 = DIRECTION ( 'NONE',  ( -0.7071067811865486830, 0.7071067811865464625, 0.000000000000000000 ) ) ;
#85258 = DIRECTION ( 'NONE',  ( 0.000000000000000000, -1.000000000000000000, 0.000000000000000000 ) ) ;
#85259 = DIRECTION ( 'NONE',  ( -0.3543493200069162685, -0.000000000000000000, -0.9351131265310288487 ) ) ;
#85260 = ADVANCED_FACE ( 'NONE', ( #30452 ), #42055, .F. ) ;
#85261 = CARTESIAN_POINT ( 'NONE',  ( 60.35416666666666430, -2.130196079827425759, -7.950000000000000178 ) ) ;
#85262 = ORIENTED_EDGE ( 'NONE', *, *, #21271, .T. ) ;
#85263 = EDGE_LOOP ( 'NONE', ( #56869, #101376, #34986, #32358 ) ) ;
#85264 = CARTESIAN_POINT ( 'NONE',  ( 77.00043019189811844, -3.055000000000002380, 5.291415217122920289 ) ) ;
#85265 = B_SPLINE_CURVE_WITH_KNOTS ( 'NONE', 3,
 ( #123611, #24265, #68512, #88100 ),
 .UNSPECIFIED., .F., .F.,
 ( 4, 4 ),
 ( 0.003615568590623256025, 0.004164643302645746128 ),
 .UNSPECIFIED. ) ;
#85266 = ORIENTED_EDGE ( 'NONE', *, *, #116135, .T. ) ;
#85267 = EDGE_CURVE ( 'NONE', #42437, #106359, #139946, .T. ) ;
#85268 = CARTESIAN_POINT ( 'NONE',  ( 7.499999999999951150, 1.030536316426518884, -5.498701923753815279 ) ) ;
#85269 = CARTESIAN_POINT ( 'NONE',  ( -5.671830600776424092, -6.740707523384212863, 4.000000000000000000 ) ) ;
#85270 = CARTESIAN_POINT ( 'NONE',  ( 24.55388970886357569, 5.485012786255876627, 4.000000000000000000 ) ) ;
#85271 = DIRECTION ( 'NONE',  ( -0.9659258262890677571, 0.000000000000000000, 0.2588190451025225713 ) ) ;
#85272 = ORIENTED_EDGE ( 'NONE', *, *, #58193, .T. ) ;
#85273 = VECTOR ( 'NONE', #53622, 1000.000000000000227 ) ;
#85274 = DIRECTION ( 'NONE',  ( 0.7071067811865487940, 0.7071067811865463515, -0.000000000000000000 ) ) ;
#85275 = DIRECTION ( 'NONE',  ( -1.000000000000000000, -0.000000000000000000, -0.000000000000000000 ) ) ;
#85276 = MECHANICAL_DESIGN_GEOMETRIC_PRESENTATION_REPRESENTATION (  '', ( #62131 ), #92210 ) ;
#85277 = ORIENTED_EDGE ( 'NONE', *, *, #102150, .T. ) ;
#85278 = DIRECTION ( 'NONE',  ( -0.000000000000000000, -0.3543493200069152693, 0.9351131265310292928 ) ) ;
#85279 = DIRECTION ( 'NONE',  ( 0.000000000000000000, -1.000000000000000000, 0.000000000000000000 ) ) ;
#85280 = DIRECTION ( 'NONE',  ( 0.7071067811865487940, 0.7071067811865463515, -0.000000000000000000 ) ) ;
#85281 = ORIENTED_EDGE ( 'NONE', *, *, #43186, .F. ) ;
#85282 = ORIENTED_EDGE ( 'NONE', *, *, #85374, .T. ) ;
#85283 = ADVANCED_FACE ( 'NONE', ( #94964 ), #75386, .F. ) ;
#85284 = DIRECTION ( 'NONE',  ( 0.7071067811865487940, 0.7071067811865463515, 0.000000000000000000 ) ) ;
#85285 = CARTESIAN_POINT ( 'NONE',  ( 8.671830600776411657, 11.25929247661560062, 4.000000000000000000 ) ) ;
#85286 = LINE ( 'NONE', #74454, #7255 ) ;
#85287 =( NAMED_UNIT ( * ) PLANE_ANGLE_UNIT ( ) SI_UNIT ( $, .RADIAN. ) );
#85288 = CARTESIAN_POINT ( 'NONE',  ( 52.57919371712956291, 3.975000000000002753, -6.884901960086283523 ) ) ;
#85289 = CARTESIAN_POINT ( 'NONE',  ( 7.499999999999951150, 0.4497235411627525936, -5.599840258123523817 ) ) ;
#85290 = PRESENTATION_STYLE_ASSIGNMENT (( #107059 ) ) ;
#85291 = VERTEX_POINT ( 'NONE', #9360 ) ;
#85292 = ORIENTED_EDGE ( 'NONE', *, *, #29937, .F. ) ;
#85293 = VERTEX_POINT ( 'NONE', #39930 ) ;
#85294 = ORIENTED_EDGE ( 'NONE', *, *, #45630, .F. ) ;
#85295 = CARTESIAN_POINT ( 'NONE',  ( 181.0893910107582485, -48.47007572038052103, 38.12657027910874774 ) ) ;
#85296 = ADVANCED_FACE ( 'NONE', ( #7226 ), #86966, .T. ) ;
#85297 = CARTESIAN_POINT ( 'NONE',  ( -20.29289321881331531, 14.25929247661557042, 5.000000000000000000 ) ) ;
#85299 = EDGE_CURVE ( 'NONE', #18953, #67945, #129748, .T. ) ;
#85298 = PLANE ( 'NONE',  #28571 ) ;
#85300 = ORIENTED_EDGE ( 'NONE', *, *, #55099, .F. ) ;
#85301 = CARTESIAN_POINT ( 'NONE',  ( 34.49999999999975842, -19.53574439159931231, 4.994342998332164107 ) ) ;
#85302 = CARTESIAN_POINT ( 'NONE',  ( 15.48921356237309510, -27.52281430457066236, 5.000000000000000000 ) ) ;
#85303 = VECTOR ( 'NONE', #69002, 1000.000000000000000 ) ;
#85304 = DIRECTION ( 'NONE',  ( 0.7071067811865486830, -0.7071067811865464625, -0.000000000000000000 ) ) ;
#85305 = LINE ( 'NONE', #84624, #131809 ) ;
#85306 = CIRCLE ( 'NONE', #22783, 2.500000000000000444 ) ;
#85307 = VECTOR ( 'NONE', #80763, 999.9999999999998863 ) ;
#85308 = CARTESIAN_POINT ( 'NONE',  ( 26.99999999999998579, -5.652181678087170091, -4.022882452454510371 ) ) ;
#85309 = VECTOR ( 'NONE', #99364, 1000.000000000000227 ) ;
#85310 = VERTEX_POINT ( 'NONE', #29706 ) ;
#85311 = DIRECTION ( 'NONE',  ( 0.6830127018922180770, -0.6830127018922204085, -0.2588190451025214056 ) ) ;
#85312 = CARTESIAN_POINT ( 'NONE',  ( 11.62000000000000099, 9.521314400968980422E-16, 0.000000000000000000 ) ) ;
#85313 = VECTOR ( 'NONE', #89582, 999.9999999999998863 ) ;
#85314 = ORIENTED_EDGE ( 'NONE', *, *, #138454, .F. ) ;
#85315 = CARTESIAN_POINT ( 'NONE',  ( 23.63159235450331863, 9.902892378096218942E-16, 0.000000000000000000 ) ) ;
#85316 = VERTEX_POINT ( 'NONE', #74690 ) ;
#85317 = ADVANCED_FACE ( 'NONE', ( #107963 ), #73953, .F. ) ;
#85318 = AXIS2_PLACEMENT_3D ( 'NONE', #117274, #31028, #20109 ) ;
#85319 = CARTESIAN_POINT ( 'NONE',  ( -34.92500000000001137, -22.22500000000000142, 4.000000000000000000 ) ) ;
#85320 = VERTEX_POINT ( 'NONE', #23098 ) ;
#85321 = CARTESIAN_POINT ( 'NONE',  ( 61.54209685856476852, 5.291415217122923842, -3.054999999999996163 ) ) ;
#85322 = VECTOR ( 'NONE', #93555, 999.9999999999998863 ) ;
#85323 = VERTEX_POINT ( 'NONE', #132655 ) ;
#85324 = EDGE_LOOP ( 'NONE', ( #53011, #60136, #23014, #37777 ) ) ;
#85325 = VECTOR ( 'NONE', #112675, 1000.000000000000000 ) ;
#85326 = CARTESIAN_POINT ( 'NONE',  ( -30.72281430457039875, -21.72499999999999432, 5.000000000000000000 ) ) ;
#85327 = LINE ( 'NONE', #51306, #84361 ) ;
#85328 = CARTESIAN_POINT ( 'NONE',  ( 102.0837635252314328, -6.110000000000001208, -3.741295971395164515E-16 ) ) ;
#85329 = PLANE ( 'NONE',  #128158 ) ;
#85330 = CARTESIAN_POINT ( 'NONE',  ( -14.99451991528749595, 28.92564299267948513, 4.000000000000000000 ) ) ;
#85331 = LINE ( 'NONE', #52709, #18548 ) ;
#85332 = CARTESIAN_POINT ( 'NONE',  ( -14.95136400821897205, -1.164498636767092865, 4.123993368336923204 ) ) ;
#85333 = AXIS2_PLACEMENT_3D ( 'NONE', #18313, #48142, #3859 ) ;
#85334 = CARTESIAN_POINT ( 'NONE',  ( 0.000000000000000000, 0.000000000000000000, 5.000000000000000000 ) ) ;
#85335 = CARTESIAN_POINT ( 'NONE',  ( 28.36246187583882161, 22.22500000000000853, 4.000000000000000000 ) ) ;
#85336 = CARTESIAN_POINT ( 'NONE',  ( 78.39169371712955581, 2.130196079827421762, 7.950000000000000178 ) ) ;
#85337 = ORIENTED_EDGE ( 'NONE', *, *, #38620, .F. ) ;
#85338 = AXIS2_PLACEMENT_3D ( 'NONE', #82946, #116278, #61243 ) ;
#85339 = CARTESIAN_POINT ( 'NONE',  ( 30.52400138585428024, 22.03583458319437938, 4.979811245910086726 ) ) ;
#85340 = VERTEX_POINT ( 'NONE', #121711 ) ;
#85341 = ORIENTED_EDGE ( 'NONE', *, *, #8422, .F. ) ;
#85342 = ORIENTED_EDGE ( 'NONE', *, *, #139666, .T. ) ;
#85343 = AXIS2_PLACEMENT_3D ( 'NONE', #78468, #122659, #34977 ) ;
#85344 = ORIENTED_EDGE ( 'NONE', *, *, #35578, .F. ) ;
#85345 = VECTOR ( 'NONE', #87775, 1000.000000000000000 ) ;
#85346 = VECTOR ( 'NONE', #26572, 1000.000000000000000 ) ;
#85347 = CARTESIAN_POINT ( 'NONE',  ( -7.140000000000001457, -35.14999999999999147, -11.72188031596275337 ) ) ;
#85348 = DIRECTION ( 'NONE',  ( 0.7071067811865487940, 0.7071067811865463515, 0.000000000000000000 ) ) ;
#85349 = AXIS2_PLACEMENT_3D ( 'NONE', #87670, #57215, #10788 ) ;
#85350 = CARTESIAN_POINT ( 'NONE',  ( 42.48921356237308800, -27.52281430457085065, 5.000000000000000000 ) ) ;
#85351 = EDGE_CURVE ( 'NONE', #19753, #64278, #90548, .T. ) ;
#85352 = ORIENTED_EDGE ( 'NONE', *, *, #104428, .F. ) ;
#85353 = CARTESIAN_POINT ( 'NONE',  ( -1.180000000000000604, 9.043340090917736163, 6.750000000000000888 ) ) ;
#85354 = ORIENTED_EDGE ( 'NONE', *, *, #38711, .T. ) ;
#85355 = VECTOR ( 'NONE', #3544, 1000.000000000000000 ) ;
#85356 = VECTOR ( 'NONE', #94243, 1000.000000000000000 ) ;
#85357 = EDGE_CURVE ( 'NONE', #45681, #113219, #110124, .T. ) ;
#85358 = ADVANCED_FACE ( 'NONE', ( #110821 ), #99235, .T. ) ;
#85359 = CARTESIAN_POINT ( 'NONE',  ( 5.812069808101887780, 7.934999999999993392, 2.126176841940951689 ) ) ;
#85360 = ADVANCED_FACE ( 'NONE', ( #10798 ), #111570, .F. ) ;
#85361 = DIRECTION ( 'NONE',  ( 0.6830127018922180770, -0.6830127018922204085, -0.2588190451025213501 ) ) ;
#85362 = PLANE ( 'NONE',  #320 ) ;
#85363 = ORIENTED_EDGE ( 'NONE', *, *, #143104, .T. ) ;
#85364 = ORIENTED_EDGE ( 'NONE', *, *, #99630, .F. ) ;
#85365 = EDGE_CURVE ( 'NONE', #75031, #119204, #11506, .T. ) ;
#85366 = ORIENTED_EDGE ( 'NONE', *, *, #90345, .F. ) ;
#85367 = DIRECTION ( 'NONE',  ( -1.000000000000000000, -1.224606353822377258E-16, -0.000000000000000000 ) ) ;
#85368 = CARTESIAN_POINT ( 'NONE',  ( -4.433128002487388919, -21.74070752338405299, 6.915939825044087108 ) ) ;
#85370 = VECTOR ( 'NONE', #47464, 1000.000000000000000 ) ;
#85369 = DIRECTION ( 'NONE',  ( 0.3543493200069162685, -0.000000000000000000, -0.9351131265310288487 ) ) ;
#85371 = EDGE_CURVE ( 'NONE', #24456, #77699, #112301, .T. ) ;
#85372 = CARTESIAN_POINT ( 'NONE',  ( -27.32816939922334143, -3.740707523384241728, 4.000000000000000000 ) ) ;
#85373 = CARTESIAN_POINT ( 'NONE',  ( -34.92500000000001137, -22.22500000000000142, 4.000000000000000000 ) ) ;
#85374 = EDGE_CURVE ( 'NONE', #45102, #79366, #2051, .T. ) ;
#85375 = CARTESIAN_POINT ( 'NONE',  ( 23.12514619309220976, -14.24070752338412937, 9.401115078912607004 ) ) ;
#85376 = CARTESIAN_POINT ( 'NONE',  ( 34.41709685856476852, 3.054999999999998828, 5.291415217122922066 ) ) ;
#85377 = DIRECTION ( 'NONE',  ( -0.000000000000000000, -1.000000000000000000, -0.000000000000000000 ) ) ;
#85378 = DIRECTION ( 'NONE',  ( -1.000000000000000000, -1.224606353822377258E-16, -0.000000000000000000 ) ) ;
#85379 = VERTEX_POINT ( 'NONE', #65965 ) ;
#85380 = DIRECTION ( 'NONE',  ( 0.7071067811865487940, 0.7071067811865463515, 0.000000000000000000 ) ) ;
#85381 = PLANE ( 'NONE',  #37830 ) ;
#85382 = ORIENTED_EDGE ( 'NONE', *, *, #88302, .F. ) ;
#85383 = EDGE_CURVE ( 'NONE', #22682, #143327, #44945, .T. ) ;
#85384 = LINE ( 'NONE', #74548, #39122 ) ;
#85386 = ORIENTED_EDGE ( 'NONE', *, *, #47220, .F. ) ;
#85385 = CARTESIAN_POINT ( 'NONE',  ( 56.10188787153389711, -51.19676978474460327, -38.21513923099966092 ) ) ;
#85387 = PLANE ( 'NONE',  #14423 ) ;
#85388 = CARTESIAN_POINT ( 'NONE',  ( 2.510786437626908008, -27.52281430457053446, 5.000000000000000000 ) ) ;
#85389 = ORIENTED_EDGE ( 'NONE', *, *, #9795, .T. ) ;
#85390 = DIRECTION ( 'NONE',  ( -0.7071067811865486830, -0.7071067811865464625, 0.000000000000000000 ) ) ;
#85391 = ORIENTED_EDGE ( 'NONE', *, *, #46958, .F. ) ;
#85392 = EDGE_CURVE ( 'NONE', #108519, #23652, #142772, .T. ) ;
#85393 = PLANE ( 'NONE',  #59104 ) ;
#85394 = CARTESIAN_POINT ( 'NONE',  ( 119.3708603837962272, 6.884901960086289741, -3.974999999999993427 ) ) ;
#85395 = CARTESIAN_POINT ( 'NONE',  ( 28.49999999999980815, 16.46639925780209168, 5.000000000000000000 ) ) ;
#85396 = DIRECTION ( 'NONE',  ( 1.000000000000000000, 0.000000000000000000, 0.000000000000000000 ) ) ;
#85397 = DIRECTION ( 'NONE',  ( 1.000000000000000000, 0.000000000000000000, 0.000000000000000000 ) ) ;
#85398 = LINE ( 'NONE', #129623, #87856 ) ;
#85399 = CARTESIAN_POINT ( 'NONE',  ( 8.604166666666667851, -1.633150327867691987, -6.094999999999989093 ) ) ;
#85400 = CARTESIAN_POINT ( 'NONE',  ( 14.27040314143522082, -7.934999999999988951, 2.126176841940957907 ) ) ;
#85401 = DIRECTION ( 'NONE',  ( -0.7071067811865486830, -0.7071067811865464625, 0.000000000000000000 ) ) ;
#85402 = CARTESIAN_POINT ( 'NONE',  ( 34.42499999999998295, 14.97718569542923994, 5.000000000000000000 ) ) ;
#85403 = EDGE_LOOP ( 'NONE', ( #137988, #42581, #31411, #121593 ) ) ;
#85404 = ORIENTED_EDGE ( 'NONE', *, *, #136043, .F. ) ;
#85405 = DIRECTION ( 'NONE',  ( 0.000000000000000000, -1.016133275908817741E-16, 1.000000000000000000 ) ) ;
#85406 = ORIENTED_EDGE ( 'NONE', *, *, #33742, .F. ) ;
#85407 = EDGE_CURVE ( 'NONE', #126528, #48470, #87680, .T. ) ;
#85408 = DIRECTION ( 'NONE',  ( -0.000000000000000000, -0.3543493200069152693, 0.9351131265310292928 ) ) ;
#85409 = FILL_AREA_STYLE_COLOUR ( '', #99604 ) ;
#85410 = DIRECTION ( 'NONE',  ( -0.6830127018922180770, -0.6830127018922204085, -0.2588190451025213501 ) ) ;
#85411 = VERTEX_POINT ( 'NONE', #76838 ) ;
#85412 = AXIS2_PLACEMENT_3D ( 'NONE', #57719, #43974, #12741 ) ;
#85413 = AXIS2_PLACEMENT_3D ( 'NONE', #114266, #101245, #135335 ) ;
#85414 =( GEOMETRIC_REPRESENTATION_CONTEXT ( 3 ) GLOBAL_UNCERTAINTY_ASSIGNED_CONTEXT ( ( #143354 ) ) GLOBAL_UNIT_ASSIGNED_CONTEXT ( ( #87968, #31452, #11081 ) ) REPRESENTATION_CONTEXT ( 'NONE', 'WORKASPACE' ) );
#85415 = DIRECTION ( 'NONE',  ( 0.6830127018922180770, -0.6830127018922204085, -0.2588190451025213501 ) ) ;
#85416 = AXIS2_PLACEMENT_3D ( 'NONE', #7912, #41265, #118834 ) ;
#85417 = LINE ( 'NONE', #143385, #92776 ) ;
#85418 = CARTESIAN_POINT ( 'NONE',  ( -4.499999999999976019, -12.08601207473290451, -10.46905243149093678 ) ) ;
#85419 = CARTESIAN_POINT ( 'NONE',  ( 0.1164707300447353766, -51.38852430739341770, 37.54101415799218699 ) ) ;
#85421 = EDGE_LOOP ( 'NONE', ( #137818, #37124, #42527, #14396 ) ) ;
#85420 = LINE ( 'NONE', #63714, #63724 ) ;
#85422 = CARTESIAN_POINT ( 'NONE',  ( 39.93750000000000000, 5.819803920172574863, -5.819803920172573086 ) ) ;
#85423 = DIRECTION ( 'NONE',  ( 0.7071067811865486830, -0.7071067811865464625, -0.000000000000000000 ) ) ;
#85424 = CARTESIAN_POINT ( 'NONE',  ( 26.99999999999981526, 10.55218569542905982, 5.000000000000000000 ) ) ;
#85425 = DIRECTION ( 'NONE',  ( 0.6830127018922181881, 0.6830127018922202975, -0.2588190451025214056 ) ) ;
#85426 = EDGE_CURVE ( 'NONE', #16634, #25329, #46364, .T. ) ;
#85427 = DIRECTION ( 'NONE',  ( -0.7071067811865486830, -0.7071067811865464625, -0.000000000000000000 ) ) ;
#85428 = EDGE_LOOP ( 'NONE', ( #130961, #126174, #4468, #107660 ) ) ;
#85429 = ORIENTED_EDGE ( 'NONE', *, *, #95723, .F. ) ;
#85430 = ORIENTED_EDGE ( 'NONE', *, *, #12935, .T. ) ;
#85431 = CARTESIAN_POINT ( 'NONE',  ( 103.6879301918981042, 6.110000000000002984, -1.637169565754156730 ) ) ;
#85432 = ORIENTED_EDGE ( 'NONE', *, *, #121301, .F. ) ;
#85433 = EDGE_CURVE ( 'NONE', #86890, #125242, #88414, .T. ) ;
#85434 = CARTESIAN_POINT ( 'NONE',  ( 125.9798776214791900, -48.09441802426615453, 35.89947574910151928 ) ) ;
#85435 = VECTOR ( 'NONE', #16749, 1000.000000000000227 ) ;
#85436 = CARTESIAN_POINT ( 'NONE',  ( 7.145833333333334814, -1.633150327867700202, 6.094999999999985540 ) ) ;
#85437 = ORIENTED_EDGE ( 'NONE', *, *, #29230, .T. ) ;
#85438 = CARTESIAN_POINT ( 'NONE',  ( 76.25000000000000000, -9.735942053221458872E-16, 7.950000000000000178 ) ) ;
#85439 = CARTESIAN_POINT ( 'NONE',  ( 5.281315875828549444, 3.061616997868382648E-16, -2.500000000000000444 ) ) ;
#85440 = VECTOR ( 'NONE', #95947, 1000.000000000000000 ) ;
#85441 = CARTESIAN_POINT ( 'NONE',  ( 92.80793019189812298, -6.109999999999998543, 1.637169565754158063 ) ) ;
#85442 = ORIENTED_EDGE ( 'NONE', *, *, #126407, .T. ) ;
#85443 = EDGE_CURVE ( 'NONE', #108968, #20344, #12248, .T. ) ;
#85444 = CARTESIAN_POINT ( 'NONE',  ( 34.98012225071431658, -17.24070752338409562, 20.23474786156477023 ) ) ;
#85445 = DIRECTION ( 'NONE',  ( 0.6830127018922180770, -0.6830127018922204085, -0.2588190451025213501 ) ) ;
#85446 = CARTESIAN_POINT ( 'NONE',  ( 127.2293817626157164, 0.000000000000000000, -7.030000000000000249 ) ) ;
#85447 = VECTOR ( 'NONE', #48928, 1000.000000000000000 ) ;
#85448 = DIRECTION ( 'NONE',  ( 0.7071067811865487940, 0.7071067811865463515, 0.000000000000000000 ) ) ;
#85449 = CIRCLE ( 'NONE', #127162, 2.500000000000000888 ) ;
#85450 = VECTOR ( 'NONE', #14952, 999.9999999999998863 ) ;
#85451 = ORIENTED_EDGE ( 'NONE', *, *, #124396, .T. ) ;
#85452 = ORIENTED_EDGE ( 'NONE', *, *, #121442, .T. ) ;
#85453 = EDGE_CURVE ( 'NONE', #69350, #132873, #12949, .T. ) ;
#85454 = EDGE_LOOP ( 'NONE', ( #40176, #89898, #4664, #25300 ) ) ;
#85455 = LINE ( 'NONE', #97776, #116563 ) ;
#85456 = DIRECTION ( 'NONE',  ( -0.000000000000000000, -0.000000000000000000, -1.000000000000000000 ) ) ;
#85457 = CARTESIAN_POINT ( 'NONE',  ( 20.04623647476855197, -7.934999999999990727, 4.858786175617117713E-16 ) ) ;
#85458 = AXIS2_PLACEMENT_3D ( 'NONE', #142662, #132537, #33228 ) ;
#85459 = VECTOR ( 'NONE', #68630, 1000.000000000000000 ) ;
#85460 = CARTESIAN_POINT ( 'NONE',  ( -28.49999999999980105, 3.653845994658365459, -4.504631822206305536 ) ) ;
#85461 = ADVANCED_FACE ( 'NONE', ( #89809 ), #57224, .T. ) ;
#85462 = ORIENTED_EDGE ( 'NONE', *, *, #7212, .T. ) ;
#85463 = ORIENTED_EDGE ( 'NONE', *, *, #35822, .T. ) ;
#85464 = CARTESIAN_POINT ( 'NONE',  ( -42.18398860626899705, 28.73617430169816700, 5.000000000000000000 ) ) ;
#85465 = ORIENTED_EDGE ( 'NONE', *, *, #574, .T. ) ;
#85466 = ORIENTED_EDGE ( 'NONE', *, *, #105519, .F. ) ;
#85467 = VECTOR ( 'NONE', #78451, 1000.000000000000000 ) ;
#85468 = ADVANCED_FACE ( 'NONE', ( #101402 ), #123184, .F. ) ;
#85469 = LINE ( 'NONE', #128987, #127679 ) ;
#85471 = EDGE_CURVE ( 'NONE', #141889, #114933, #65243, .T. ) ;
#85470 = DIRECTION ( 'NONE',  ( -0.7071067811865486830, 0.7071067811865464625, 0.000000000000000000 ) ) ;
#85472 = ORIENTED_EDGE ( 'NONE', *, *, #110757, .F. ) ;
#85473 = FACE_OUTER_BOUND ( 'NONE', #80310, .T. ) ;
#85474 = CARTESIAN_POINT ( 'NONE',  ( -12.33010218547257786, 17.25929247661554555, 19.83885114516074211 ) ) ;
#85475 = DIRECTION ( 'NONE',  ( 0.000000000000000000, -1.000000000000000000, 0.000000000000000000 ) ) ;
#85476 = DIRECTION ( 'NONE',  ( 0.6830127018922181881, 0.6830127018922202975, -0.2588190451025214056 ) ) ;
#85477 = LINE ( 'NONE', #84787, #76791 ) ;
#85478 = ORIENTED_EDGE ( 'NONE', *, *, #108437, .F. ) ;
#85479 = DIRECTION ( 'NONE',  ( -0.000000000000000000, 0.3543493200069152138, -0.9351131265310292928 ) ) ;
#85480 = FACE_BOUND ( 'NONE', #63173, .T. ) ;
#85481 = EDGE_LOOP ( 'NONE', ( #128034, #100116, #8466, #82443 ) ) ;
#85482 = CARTESIAN_POINT ( 'NONE',  ( 25.40000000000000213, 2.120873585778977333, -7.657087335400156292 ) ) ;
#85483 = DIRECTION ( 'NONE',  ( 0.000000000000000000, 0.000000000000000000, -1.000000000000000000 ) ) ;
#85484 = DIRECTION ( 'NONE',  ( 0.7071067811865487940, 0.7071067811865463515, -0.000000000000000000 ) ) ;
#85485 = EDGE_CURVE ( 'NONE', #76457, #48400, #92656, .T. ) ;
#85486 = ORIENTED_EDGE ( 'NONE', *, *, #38715, .T. ) ;
#85487 = CARTESIAN_POINT ( 'NONE',  ( 22.13389675353461072, 22.22500000000000142, 26.62174895348230308 ) ) ;
#85488 = VERTEX_POINT ( 'NONE', #47784 ) ;
#85489 = ORIENTED_EDGE ( 'NONE', *, *, #93759, .F. ) ;
#85490 = ORIENTED_EDGE ( 'NONE', *, *, #11271, .T. ) ;
#85491 = CARTESIAN_POINT ( 'NONE',  ( 0.000000000000000000, 0.000000000000000000, 5.000000000000000000 ) ) ;
#85492 = CARTESIAN_POINT ( 'NONE',  ( 19.88982677111775033, -22.22500000000000142, 4.785647885939350310 ) ) ;
#85493 = DIRECTION ( 'NONE',  ( 0.6830127018922180770, -0.6830127018922204085, -0.2588190451025213501 ) ) ;
#85494 = DIRECTION ( 'NONE',  ( 0.000000000000000000, -1.000000000000000000, 0.000000000000000000 ) ) ;
#85495 = DIRECTION ( 'NONE',  ( -0.7071067811865486830, -0.7071067811865464625, 0.000000000000000000 ) ) ;
#85496 = DIRECTION ( 'NONE',  ( 0.7071067811865486830, -0.7071067811865464625, -0.000000000000000000 ) ) ;
#85497 = CARTESIAN_POINT ( 'NONE',  ( 0.000000000000000000, 0.000000000000000000, 5.000000000000000000 ) ) ;
#85498 = CARTESIAN_POINT ( 'NONE',  ( 30.70710678118633297, -0.7407075233842753681, 5.000000000000000000 ) ) ;
#85499 = LINE ( 'NONE', #73241, #20465 ) ;
#85500 = DIRECTION ( 'NONE',  ( 0.7071067811865486830, -0.7071067811865464625, -0.000000000000000000 ) ) ;
#85501 = CARTESIAN_POINT ( 'NONE',  ( 12.79289321881336861, 3.759292476615681888, 5.000000000000000000 ) ) ;
#85502 = EDGE_LOOP ( 'NONE', ( #95976, #26426, #42981, #74110 ) ) ;
#85503 = EDGE_LOOP ( 'NONE', ( #55936, #602, #97550, #18090 ) ) ;
#85504 = ORIENTED_EDGE ( 'NONE', *, *, #107044, .T. ) ;
#85505 = EDGE_LOOP ( 'NONE', ( #24511, #27101, #57147, #129099 ) ) ;
#85506 = DIRECTION ( 'NONE',  ( 0.7071067811865487940, 0.7071067811865463515, 0.000000000000000000 ) ) ;
#85507 = VECTOR ( 'NONE', #50247, 1000.000000000000000 ) ;
#85508 = PRESENTATION_LAYER_ASSIGNMENT (  '', '', ( #67022 ) ) ;
#85509 = ORIENTED_EDGE ( 'NONE', *, *, #142211, .T. ) ;
#85510 = VECTOR ( 'NONE', #79284, 999.9999999999998863 ) ;
#85512 = VERTEX_POINT ( 'NONE', #38304 ) ;
#85511 = VECTOR ( 'NONE', #20051, 1000.000000000000000 ) ;
#85513 = CARTESIAN_POINT ( 'NONE',  ( 12.18398860626900060, 28.73617430169795739, 5.000000000000000000 ) ) ;
#85514 = PRESENTATION_STYLE_ASSIGNMENT (( #7227 ) ) ;
#85515 = DIRECTION ( 'NONE',  ( 0.7071067811865487940, 0.7071067811865463515, 0.000000000000000000 ) ) ;
#85516 = VERTEX_POINT ( 'NONE', #103523 ) ;
#85517 = DIRECTION ( 'NONE',  ( -0.6830127018922181881, 0.6830127018922202975, -0.2588190451025214056 ) ) ;
#85518 = ORIENTED_EDGE ( 'NONE', *, *, #138877, .F. ) ;
#85519 = FACE_BOUND ( 'NONE', #20977, .T. ) ;
#85520 = CARTESIAN_POINT ( 'NONE',  ( 21.29159235450332233, -3.851859888774471706E-31, 2.500000000000001332 ) ) ;
#85521 = ADVANCED_FACE ( 'NONE', ( #4163 ), #48455, .F. ) ;
#85523 = AXIS2_PLACEMENT_3D ( 'NONE', #80767, #78613, #124957 ) ;
#85522 = CARTESIAN_POINT ( 'NONE',  ( 5.608736474768551972, -5.808823158059033709, 5.808823158059035485 ) ) ;
#85524 = VERTEX_POINT ( 'NONE', #24555 ) ;
#85525 = CARTESIAN_POINT ( 'NONE',  ( 94.12043019189810877, 3.055000000000002380, -5.291415217122917625 ) ) ;
#85526 = DIRECTION ( 'NONE',  ( 0.7071067811865487940, 0.7071067811865463515, -0.000000000000000000 ) ) ;
#85527 = EDGE_CURVE ( 'NONE', #373, #86911, #60065, .T. ) ;
#85528 = CARTESIAN_POINT ( 'NONE',  ( -2.999999999999978240, -7.068876922607738145, 4.000000000000000000 ) ) ;
#85529 = DIRECTION ( 'NONE',  ( -8.817971600062198362E-18, -0.3543493200069152693, 0.9351131265310292928 ) ) ;
#85530 = VERTEX_POINT ( 'NONE', #79717 ) ;
#85531 = VERTEX_POINT ( 'NONE', #81841 ) ;
#85532 = ADVANCED_FACE ( 'NONE', ( #126034 ), #115813, .T. ) ;
#85533 = DIRECTION ( 'NONE',  ( 1.000000000000000000, -0.000000000000000000, 0.000000000000000000 ) ) ;
#85534 = ORIENTED_EDGE ( 'NONE', *, *, #71336, .F. ) ;
#85535 = AXIS2_PLACEMENT_3D ( 'NONE', #1225, #67991, #33214 ) ;
#85536 = CARTESIAN_POINT ( 'NONE',  ( 60.29974487139158867, -27.71228299555248142, 4.000000000000000000 ) ) ;
#85538 = LINE ( 'NONE', #84171, #115902 ) ;
#85537 = AXIS2_PLACEMENT_3D ( 'NONE', #86532, #87233, #97357 ) ;
#85539 = CARTESIAN_POINT ( 'NONE',  ( -1.499999999999994449, 1.030536316426501564, -5.498701923753798404 ) ) ;
#85540 = EDGE_CURVE ( 'NONE', #68848, #93995, #91951, .T. ) ;
#85541 = CARTESIAN_POINT ( 'NONE',  ( 183.9820196591281842, -48.55783623716401820, -38.28685941347310973 ) ) ;
#85543 = ORIENTED_EDGE ( 'NONE', *, *, #80512, .T. ) ;
#85542 =( BOUNDED_CURVE ( )  B_SPLINE_CURVE ( 3, ( #59689, #37200, #114736, #48092 ),
 .UNSPECIFIED., .F., .F. ) 
 B_SPLINE_CURVE_WITH_KNOTS ( ( 4, 4 ),
 ( 1.964434688349479652, 3.503810798801450854 ),
 .UNSPECIFIED. ) 
 CURVE ( )  GEOMETRIC_REPRESENTATION_ITEM ( )  RATIONAL_B_SPLINE_CURVE ( ( 1.000000000000000000, 0.8120851936182262865, 0.8120851936182262865, 1.000000000000000000 ) ) 
 REPRESENTATION_ITEM ( '' )  );
#85544 = DIRECTION ( 'NONE',  ( -1.000000000000000000, -1.224606353822377258E-16, -0.000000000000000000 ) ) ;
#85545 = VECTOR ( 'NONE', #70168, 1000.000000000000000 ) ;
#85546 = LINE ( 'NONE', #129778, #139268 ) ;
#85547 = CYLINDRICAL_SURFACE ( 'NONE', #70017, 7.950000000000000178 ) ;
#85548 = EDGE_LOOP ( 'NONE', ( #50974, #124798, #135814, #64411 ) ) ;
#85549 = LINE ( 'NONE', #129782, #83668 ) ;
#85550 = VECTOR ( 'NONE', #100973, 1000.000000000000000 ) ;
#85552 = COLOUR_RGB ( '', 0.31764706, 0.68627451, 0.89019608) ;
#85551 = CARTESIAN_POINT ( 'NONE',  ( 17.81601139373099940, 28.73617430169775133, 5.000000000000000000 ) ) ;
#85553 = EDGE_LOOP ( 'NONE', ( #22144, #107467, #42611, #8300 ) ) ;
#85554 = VECTOR ( 'NONE', #21027, 1000.000000000000000 ) ;
#85555 = ADVANCED_FACE ( 'NONE', ( #49908 ), #3490, .F. ) ;
#85557 = ORIENTED_EDGE ( 'NONE', *, *, #121798, .T. ) ;
#85556 = DIRECTION ( 'NONE',  ( 0.6830127018922181881, 0.6830127018922202975, -0.2588190451025214056 ) ) ;
#85558 = VERTEX_POINT ( 'NONE', #102852 ) ;
#85559 = EDGE_CURVE ( 'NONE', #106514, #130620, #136175, .T. ) ;
#85560 = CARTESIAN_POINT ( 'NONE',  ( -2.999999999999981792, -10.77435723561695902, -9.972017380717224100 ) ) ;
#85561 = CIRCLE ( 'NONE', #62421, 2.552699999999990865 ) ;
#85562 = CARTESIAN_POINT ( 'NONE',  ( -48.18398860626899705, 28.73617430169820608, 5.000000000000000000 ) ) ;
#85563 = ORIENTED_EDGE ( 'NONE', *, *, #140730, .F. ) ;
#85564 = CARTESIAN_POINT ( 'NONE',  ( 11.70025512860841133, -27.71228299555198049, 4.000000000000000000 ) ) ;
#85565 = ADVANCED_FACE ( 'NONE', ( #104968 ), #113712, .F. ) ;
#85566 = CARTESIAN_POINT ( 'NONE',  ( 14.29289321881336683, -15.74070752338412404, 5.000000000000000000 ) ) ;
#85567 = DIRECTION ( 'NONE',  ( -0.3543493200069162685, -0.000000000000000000, -0.9351131265310288487 ) ) ;
#85568 = CARTESIAN_POINT ( 'NONE',  ( 152.4000000000000057, -16.48000000000005016, 12.69999999999954632 ) ) ;
#85569 = CARTESIAN_POINT ( 'NONE',  ( 0.1600000000000008915, -5.960583198795250226, -5.280645022235340491 ) ) ;
#85570 = CARTESIAN_POINT ( 'NONE',  ( -22.49999999999984013, -7.420205493532918695, -2.617629953481305893 ) ) ;
#85571 = CARTESIAN_POINT ( 'NONE',  ( 47.08333333333332149, 6.884901960086290629, -3.974999999999994316 ) ) ;
#85572 = CARTESIAN_POINT ( 'NONE',  ( 34.92499999999998295, -21.72500000000000142, 5.000000000000000000 ) ) ;
#85573 = ADVANCED_FACE ( 'NONE', ( #126706 ), #70944, .F. ) ;
#85575 = AXIS2_PLACEMENT_3D ( 'NONE', #26746, #5684, #126080 ) ;
#85574 = CARTESIAN_POINT ( 'NONE',  ( -26.20666063542134339, 21.75929247661549226, 4.998822639870711626 ) ) ;
#85576 = DIRECTION ( 'NONE',  ( 0.7071067811865487940, 0.7071067811865463515, -0.000000000000000000 ) ) ;
#85577 = CARTESIAN_POINT ( 'NONE',  ( -6.328169399223483538, 17.25929247661554200, 4.000000000000000000 ) ) ;
#85578 = CARTESIAN_POINT ( 'NONE',  ( -12.48921356237309155, -27.52281430457064104, 5.000000000000000000 ) ) ;
#85579 =( NAMED_UNIT ( * ) SI_UNIT ( $, .STERADIAN. ) SOLID_ANGLE_UNIT ( ) );
#85580 = VERTEX_POINT ( 'NONE', #91278 ) ;
#85581 = ORIENTED_EDGE ( 'NONE', *, *, #19747, .F. ) ;
#85582 = VERTEX_POINT ( 'NONE', #80397 ) ;
#85583 = CARTESIAN_POINT ( 'NONE',  ( 109.9375000000000000, 5.819803920172573974, -5.819803920172572198 ) ) ;
#85584 = ORIENTED_EDGE ( 'NONE', *, *, #5839, .T. ) ;
#85585 = ORIENTED_EDGE ( 'NONE', *, *, #43186, .T. ) ;
#85586 = VERTEX_POINT ( 'NONE', #4899 ) ;
#85587 = ADVANCED_FACE ( 'NONE', ( #135488 ), #59366, .F. ) ;
#85588 = CARTESIAN_POINT ( 'NONE',  ( -17.70025512860841488, -27.71228299555193786, 4.000000000000000000 ) ) ;
#85589 = DIRECTION ( 'NONE',  ( 0.5735764363510451602, 0.8191520442889924647, 0.000000000000000000 ) ) ;
#85590 = ORIENTED_EDGE ( 'NONE', *, *, #53136, .T. ) ;
#85591 = DIRECTION ( 'NONE',  ( -0.6830127018922180770, -0.6830127018922204085, -0.2588190451025213501 ) ) ;
#85592 = LINE ( 'NONE', #129829, #78774 ) ;
#85593 = LINE ( 'NONE', #142850, #85738 ) ;
#85594 = DIRECTION ( 'NONE',  ( 0.000000000000000000, -1.000000000000000000, 0.000000000000000000 ) ) ;
#85595 = CARTESIAN_POINT ( 'NONE',  ( 100.0420968585647756, 5.291415217122923842, -3.054999999999996163 ) ) ;
#85596 = EDGE_LOOP ( 'NONE', ( #137513, #108578, #73422, #111144 ) ) ;
#85597 = CARTESIAN_POINT ( 'NONE',  ( -3.295843663686523595, 12.28244488499750275, -27.01195477951401713 ) ) ;
#85598 = LINE ( 'NONE', #108047, #1069 ) ;
#85599 = DIRECTION ( 'NONE',  ( -0.000000000000000000, 0.000000000000000000, 1.000000000000000000 ) ) ;
#85600 = DIRECTION ( 'NONE',  ( -0.5735764363510507113, 0.8191520442889885789, 1.003171929053520926E-16 ) ) ;
#85601 = FACE_OUTER_BOUND ( 'NONE', #94117, .T. ) ;
#85602 = CARTESIAN_POINT ( 'NONE',  ( 0.000000000000000000, 9.735942053221458872E-16, -7.950000000000000178 ) ) ;
#85603 = CARTESIAN_POINT ( 'NONE',  ( 32.60002705046289151, 5.819803920172570422, 5.819803920172574863 ) ) ;
#85604 = EDGE_CURVE ( 'NONE', #98637, #764, #88479, .T. ) ;
#85605 = FACE_OUTER_BOUND ( 'NONE', #21223, .T. ) ;
#85606 = ORIENTED_EDGE ( 'NONE', *, *, #62139, .T. ) ;
#85607 = ORIENTED_EDGE ( 'NONE', *, *, #114496, .T. ) ;
#85608 = CARTESIAN_POINT ( 'NONE',  ( 126.7295968585647614, -6.110000000000000320, -1.637169565754161393 ) ) ;
#85609 = ORIENTED_EDGE ( 'NONE', *, *, #43837, .F. ) ;
#85610 = LINE ( 'NONE', #108059, #141241 ) ;
#85611 = ADVANCED_FACE ( 'NONE', ( #112988 ), #104235, .F. ) ;
#85612 = DIRECTION ( 'NONE',  ( -0.7071067811865487940, 0.7071067811865463515, 0.000000000000000000 ) ) ;
#85613 = CARTESIAN_POINT ( 'NONE',  ( 13.49159235450332162, -2.500000000000000444, 3.061616997868384620E-16 ) ) ;
#85614 = DIRECTION ( 'NONE',  ( 0.7071067811865487940, 0.7071067811865463515, 0.000000000000000000 ) ) ;
#85615 = CARTESIAN_POINT ( 'NONE',  ( 42.18398860626899705, 28.73617430169816700, 5.000000000000000000 ) ) ;
#85616 =( NAMED_UNIT ( * ) PLANE_ANGLE_UNIT ( ) SI_UNIT ( $, .RADIAN. ) );
#85617 = CARTESIAN_POINT ( 'NONE',  ( 124.1620968585647944, -5.291415217122919401, 3.054999999999997939 ) ) ;
#85618 = ORIENTED_EDGE ( 'NONE', *, *, #5537, .T. ) ;
#85619 = ADVANCED_FACE ( 'NONE', ( #102142 ), #2798, .T. ) ;
#85620 = LINE ( 'NONE', #28419, #78034 ) ;
#85621 = VERTEX_POINT ( 'NONE', #85347 ) ;
#85622 = DIRECTION ( 'NONE',  ( -0.6830127018922180770, -0.6830127018922204085, -0.2588190451025213501 ) ) ;
#85623 = VECTOR ( 'NONE', #71839, 999.9999999999998863 ) ;
#85624 = VECTOR ( 'NONE', #38153, 1000.000000000000000 ) ;
#85625 = VECTOR ( 'NONE', #43487, 1000.000000000000000 ) ;
#85626 = CARTESIAN_POINT ( 'NONE',  ( 71.99451991528749772, 28.92564299267988304, 4.000000000000000000 ) ) ;
#85627 = DIRECTION ( 'NONE',  ( 0.3543493200069163240, 0.000000000000000000, 0.9351131265310288487 ) ) ;
#85628 = AXIS2_PLACEMENT_3D ( 'NONE', #117750, #62717, #129364 ) ;
#85629 = CARTESIAN_POINT ( 'NONE',  ( 29.21837311707485085, 21.74787736706806385, 4.999607392498049308 ) ) ;
#85630 = VERTEX_POINT ( 'NONE', #41144 ) ;
#85631 = CARTESIAN_POINT ( 'NONE',  ( 46.66709685856476852, -3.055000000000000160, -5.291415217122921177 ) ) ;
#85632 = EDGE_CURVE ( 'NONE', #91948, #40577, #17252, .T. ) ;
#85633 = VERTEX_POINT ( 'NONE', #86091 ) ;
#85634 = DIRECTION ( 'NONE',  ( -1.000000000000000000, -0.000000000000000000, -0.000000000000000000 ) ) ;
#85635 = LINE ( 'NONE', #75499, #101712 ) ;
#85636 = LINE ( 'NONE', #118991, #98785 ) ;
#85637 = CARTESIAN_POINT ( 'NONE',  ( 30.18398860626900060, 28.73617430169808173, 5.000000000000000000 ) ) ;
#85638 = VECTOR ( 'NONE', #56938, 1000.000000000000000 ) ;
#85639 = CARTESIAN_POINT ( 'NONE',  ( 41.32876352523144448, 0.000000000000000000, -6.109999999999998543 ) ) ;
#85640 = ORIENTED_EDGE ( 'NONE', *, *, #57493, .T. ) ;
#85641 = EDGE_CURVE ( 'NONE', #22050, #108173, #107106, .T. ) ;
#85642 = DIRECTION ( 'NONE',  ( 0.7071067811865486830, -0.7071067811865464625, -0.000000000000000000 ) ) ;
#85643 = ORIENTED_EDGE ( 'NONE', *, *, #15169, .F. ) ;
#85644 = ORIENTED_EDGE ( 'NONE', *, *, #32868, .F. ) ;
#85645 = CIRCLE ( 'NONE', #50906, 2.500000000000000888 ) ;
#85646 = ORIENTED_EDGE ( 'NONE', *, *, #115572, .T. ) ;
#85647 = MECHANICAL_DESIGN_GEOMETRIC_PRESENTATION_REPRESENTATION (  '', ( #44078 ), #125083 ) ;
#85648 = LINE ( 'NONE', #9497, #37222 ) ;
#85649 = EDGE_CURVE ( 'NONE', #53505, #135463, #61513, .T. ) ;
#85650 = ORIENTED_EDGE ( 'NONE', *, *, #69240, .T. ) ;
#85651 = DIRECTION ( 'NONE',  ( -0.7071067811865487940, 0.7071067811865463515, 0.000000000000000000 ) ) ;
#85652 = FACE_OUTER_BOUND ( 'NONE', #103435, .T. ) ;
#85653 = AXIS2_PLACEMENT_3D ( 'NONE', #26771, #17995, #128245 ) ;
#85654 = CARTESIAN_POINT ( 'NONE',  ( 0.000000000000000000, 0.000000000000000000, 5.000000000000000000 ) ) ;
#85655 = EDGE_CURVE ( 'NONE', #46033, #123098, #7782, .T. ) ;
#85656 = FACE_BOUND ( 'NONE', #39973, .T. ) ;
#85657 = EDGE_LOOP ( 'NONE', ( #124352, #132514, #53383, #63468 ) ) ;
#85658 = FACE_OUTER_BOUND ( 'NONE', #58917, .T. ) ;
#85659 = VECTOR ( 'NONE', #102048, 1000.000000000000000 ) ;
#85660 = CARTESIAN_POINT ( 'NONE',  ( -10.49999999999992539, -19.53360074219753884, 5.000000000000000000 ) ) ;
#85662 = EDGE_CURVE ( 'NONE', #53640, #47010, #116567, .T. ) ;
#85661 = CARTESIAN_POINT ( 'NONE',  ( -25.39999999999996305, 3.061616997868383141E-16, -2.500000000000000000 ) ) ;
#85663 = ORIENTED_EDGE ( 'NONE', *, *, #115749, .F. ) ;
#85664 = DIRECTION ( 'NONE',  ( -0.7071067811865487940, 0.7071067811865463515, -0.000000000000000000 ) ) ;
#85665 = ORIENTED_EDGE ( 'NONE', *, *, #77083, .F. ) ;
#85666 = AXIS2_PLACEMENT_3D ( 'NONE', #27668, #4423, #137889 ) ;
#85667 = ORIENTED_EDGE ( 'NONE', *, *, #73548, .F. ) ;
#85668 = CARTESIAN_POINT ( 'NONE',  ( -24.08491323193747036, -12.74070752338414891, 18.74364270924348830 ) ) ;
#85669 = ORIENTED_EDGE ( 'NONE', *, *, #55165, .T. ) ;
#85670 = CARTESIAN_POINT ( 'NONE',  ( 59.70376352523145158, 6.109999999999998543, 1.122388791418548911E-15 ) ) ;
#85671 = VERTEX_POINT ( 'NONE', #72399 ) ;
#85672 = VECTOR ( 'NONE', #114718, 1000.000000000000000 ) ;
#85673 = PLANE ( 'NONE',  #71943 ) ;
#85674 = FACE_OUTER_BOUND ( 'NONE', #53445, .T. ) ;
#85675 = ORIENTED_EDGE ( 'NONE', *, *, #47312, .F. ) ;
#85676 = CARTESIAN_POINT ( 'NONE',  ( 75.29974487139158157, -27.71228299555258445, 4.000000000000000000 ) ) ;
#85677 = VECTOR ( 'NONE', #85059, 1000.000000000000000 ) ;
#85678 = EDGE_CURVE ( 'NONE', #26874, #123294, #30271, .T. ) ;
#85679 = LINE ( 'NONE', #32029, #138205 ) ;
#85680 = LINE ( 'NONE', #98702, #20406 ) ;
#85681 = CARTESIAN_POINT ( 'NONE',  ( -14.21837311707495743, 21.74787736706806385, 4.999607392498048419 ) ) ;
#85682 = LINE ( 'NONE', #141515, #30901 ) ;
#85683 = DIRECTION ( 'NONE',  ( -0.7071067811865487940, 0.7071067811865463515, -0.000000000000000000 ) ) ;
#85684 = ORIENTED_EDGE ( 'NONE', *, *, #44495, .T. ) ;
#85685 = VECTOR ( 'NONE', #85881, 1000.000000000000227 ) ;
#85686 = ORIENTED_EDGE ( 'NONE', *, *, #68813, .T. ) ;
#85687 = LINE ( 'NONE', #131355, #100653 ) ;
#85688 = PLANE ( 'NONE',  #25803 ) ;
#85689 = ORIENTED_EDGE ( 'NONE', *, *, #110487, .F. ) ;
#85690 = VERTEX_POINT ( 'NONE', #62931 ) ;
#85691 = ORIENTED_EDGE ( 'NONE', *, *, #93745, .T. ) ;
#85692 = CARTESIAN_POINT ( 'NONE',  ( -26.58838509405149964, 22.22500000000000142, 4.777194822843817690 ) ) ;
#85693 = PLANE ( 'NONE',  #105837 ) ;
#85694 = CARTESIAN_POINT ( 'NONE',  ( 9.005480084712511157, 28.92564299267931816, 4.000000000000000000 ) ) ;
#85695 = ORIENTED_EDGE ( 'NONE', *, *, #512, .F. ) ;
#85696 = CARTESIAN_POINT ( 'NONE',  ( -0.7071067811865329178, -18.74070752338408852, 5.000000000000000000 ) ) ;
#85697 = VECTOR ( 'NONE', #70819, 1000.000000000000000 ) ;
#85698 = LINE ( 'NONE', #30646, #5298 ) ;
#85699 = CARTESIAN_POINT ( 'NONE',  ( 22.81706980810188767, -2.126176841940956130, 7.934999999999991616 ) ) ;
#85700 = EDGE_CURVE ( 'NONE', #42461, #18783, #18656, .T. ) ;
#85701 = LINE ( 'NONE', #129946, #137567 ) ;
#85702 = ORIENTED_EDGE ( 'NONE', *, *, #138609, .T. ) ;
#85703 = CARTESIAN_POINT ( 'NONE',  ( 124.1620968585647944, -5.291415217122919401, 3.054999999999998384 ) ) ;
#85704 =( BOUNDED_CURVE ( )  B_SPLINE_CURVE ( 3, ( #84172, #3677, #71860, #39210 ),
 .UNSPECIFIED., .F., .T. ) 
 B_SPLINE_CURVE_WITH_KNOTS ( ( 4, 4 ),
 ( 4.712388980384689674, 6.105785702739209952 ),
 .UNSPECIFIED. ) 
 CURVE ( )  GEOMETRIC_REPRESENTATION_ITEM ( )  RATIONAL_B_SPLINE_CURVE ( ( 1.000000000000000000, 0.8446433258982480874, 0.8446433258982480874, 1.000000000000000000 ) ) 
 REPRESENTATION_ITEM ( '' )  );
#85705 = ADVANCED_FACE ( 'NONE', ( #6321 ), #106363, .F. ) ;
#85706 = CARTESIAN_POINT ( 'NONE',  ( -34.42500000000001137, 22.22500000000000142, 5.000000000000000000 ) ) ;
#85707 = FACE_OUTER_BOUND ( 'NONE', #44958, .T. ) ;
#85709 = ORIENTED_EDGE ( 'NONE', *, *, #36533, .F. ) ;
#85708 = DIRECTION ( 'NONE',  ( 0.7071067811865487940, -0.7071067811865463515, 0.000000000000000000 ) ) ;
#85710 = DIRECTION ( 'NONE',  ( 0.7071067811865487940, 0.7071067811865463515, 0.000000000000000000 ) ) ;
#85711 = EDGE_LOOP ( 'NONE', ( #101747, #48327, #125556, #111300 ) ) ;
#85712 = CARTESIAN_POINT ( 'NONE',  ( -34.42499999999997584, -21.76999999999999247, -37.00000000000000000 ) ) ;
#85713 = PRESENTATION_LAYER_ASSIGNMENT (  '', '', ( #111157 ) ) ;
#85714 = CYLINDRICAL_SURFACE ( 'NONE', #118719, 0.5000000000000004441 ) ;
#85715 = EDGE_CURVE ( 'NONE', #2907, #61841, #63646, .T. ) ;
#85716 = EDGE_CURVE ( 'NONE', #40019, #44445, #41875, .T. ) ;
#85717 = DIRECTION ( 'NONE',  ( 0.3543493200069162685, -0.000000000000000000, -0.9351131265310288487 ) ) ;
#85718 = ORIENTED_EDGE ( 'NONE', *, *, #2153, .T. ) ;
#85719 = AXIS2_PLACEMENT_3D ( 'NONE', #26832, #39890, #17383 ) ;
#85720 = VECTOR ( 'NONE', #69526, 999.9999999999998863 ) ;
#85721 = DIRECTION ( 'NONE',  ( -0.7071067811865487940, 0.7071067811865463515, 0.000000000000000000 ) ) ;
#85722 = CARTESIAN_POINT ( 'NONE',  ( -25.49999999999981526, 19.46639925780206326, 5.000000000000000000 ) ) ;
#85723 = AXIS2_PLACEMENT_3D ( 'NONE', #61786, #118259, #107400 ) ;
#85724 = ORIENTED_EDGE ( 'NONE', *, *, #54320, .T. ) ;
#85725 = VECTOR ( 'NONE', #86968, 1000.000000000000227 ) ;
#85726 = VECTOR ( 'NONE', #89843, 1000.000000000000000 ) ;
#85727 = VECTOR ( 'NONE', #117270, 999.9999999999998863 ) ;
#85728 = CARTESIAN_POINT ( 'NONE',  ( -25.00193056682080339, -22.22500000000000142, 4.500000000000000888 ) ) ;
#85729 = AXIS2_PLACEMENT_3D ( 'NONE', #126296, #39305, #47371 ) ;
#85730 = CARTESIAN_POINT ( 'NONE',  ( 0.7228143045705931469, -21.72500000000000142, 5.000000000000000000 ) ) ;
#85731 = VECTOR ( 'NONE', #7768, 1000.000000000000000 ) ;
#85732 = DIRECTION ( 'NONE',  ( -0.7071067811865486830, -0.7071067811865464625, -0.000000000000000000 ) ) ;
#85733 = ADVANCED_FACE ( 'NONE', ( #39011 ), #75232, .T. ) ;
#85734 = ORIENTED_EDGE ( 'NONE', *, *, #118294, .T. ) ;
#85735 = EDGE_CURVE ( 'NONE', #81832, #23063, #128179, .T. ) ;
#85736 = ORIENTED_EDGE ( 'NONE', *, *, #121765, .F. ) ;
#85737 = CARTESIAN_POINT ( 'NONE',  ( 21.00548008471250938, 28.92564299267923644, 4.000000000000000000 ) ) ;
#85738 = VECTOR ( 'NONE', #141423, 1000.000000000000227 ) ;
#85739 = LINE ( 'NONE', #42271, #136265 ) ;
#85740 = EDGE_CURVE ( 'NONE', #5013, #78734, #93210, .T. ) ;
#85741 = CARTESIAN_POINT ( 'NONE',  ( 10.33290314143522082, -3.967499999999994476, 6.871911579029513106 ) ) ;
#85742 = DIRECTION ( 'NONE',  ( -0.000000000000000000, 0.3543493200069153248, 0.9351131265310292928 ) ) ;
#85743 = FACE_OUTER_BOUND ( 'NONE', #67103, .T. ) ;
#85744 = CARTESIAN_POINT ( 'NONE',  ( -3.005480084712505828, 28.92564299267936079, 4.000000000000000000 ) ) ;
#85745 = ORIENTED_EDGE ( 'NONE', *, *, #57047, .T. ) ;
#85746 = FILL_AREA_STYLE_COLOUR ( '', #92803 ) ;
#85747 = DIRECTION ( 'NONE',  ( 0.7071067811865486830, -0.7071067811865464625, -0.000000000000000000 ) ) ;
#85748 = CARTESIAN_POINT ( 'NONE',  ( 6.170806282870438864, -3.047499999999997211, -5.278424836066143655 ) ) ;
#85749 = VECTOR ( 'NONE', #94115, 999.9999999999998863 ) ;
#85750 = ADVANCED_FACE ( 'NONE', ( #127440 ), #29538, .F. ) ;
#85751 = CARTESIAN_POINT ( 'NONE',  ( 126.8603669610315308, -5.004565729002734109, -4.329968208352205750 ) ) ;
#85752 = CARTESIAN_POINT ( 'NONE',  ( 41.62043019189810877, 3.055000000000002380, -5.291415217122917625 ) ) ;
#85753 = CARTESIAN_POINT ( 'NONE',  ( -6.640000000000001457, -40.42999999999999261, -40.00000000000000000 ) ) ;
#85754 = VECTOR ( 'NONE', #108073, 1000.000000000000000 ) ;
#85755 = ORIENTED_EDGE ( 'NONE', *, *, #131259, .T. ) ;
#85756 = CARTESIAN_POINT ( 'NONE',  ( 19.10813147593277250, -2.055000000000000160, 2.789133085058097101E-16 ) ) ;
#85757 = CIRCLE ( 'NONE', #104260, 2.500000000000000888 ) ;
#85758 = ORIENTED_EDGE ( 'NONE', *, *, #73012, .F. ) ;
#85759 = VECTOR ( 'NONE', #32859, 1000.000000000000000 ) ;
#85760 = ORIENTED_EDGE ( 'NONE', *, *, #122336, .F. ) ;
#85761 = EDGE_CURVE ( 'NONE', #14566, #139810, #83231, .T. ) ;
#85762 = DIRECTION ( 'NONE',  ( -0.3543493200069162685, -0.000000000000000000, -0.9351131265310288487 ) ) ;
#85763 = DIRECTION ( 'NONE',  ( 0.7071067811865486830, -0.7071067811865464625, -0.000000000000000000 ) ) ;
#85764 = AXIS2_PLACEMENT_3D ( 'NONE', #62600, #95206, #73477 ) ;
#85765 = EDGE_LOOP ( 'NONE', ( #480, #98649, #99477, #52469 ) ) ;
#85766 = CARTESIAN_POINT ( 'NONE',  ( 0.000000000000000000, 8.616843969807042924, 4.000000000000000000 ) ) ;
#85767 = CARTESIAN_POINT ( 'NONE',  ( 5.994519915287488843, 28.92564299267942118, 4.000000000000000000 ) ) ;
#85768 = LINE ( 'NONE', #30709, #50940 ) ;
#85769 = CARTESIAN_POINT ( 'NONE',  ( -24.98358986394466186, 3.827854121229849582, 4.315828149752543474 ) ) ;
#85770 = CARTESIAN_POINT ( 'NONE',  ( 26.99999999999980105, -22.22500000000000142, 4.412002311789987807 ) ) ;
#85771 = CIRCLE ( 'NONE', #104275, 9.119999999999999218 ) ;
#85772 = ORIENTED_EDGE ( 'NONE', *, *, #87487, .F. ) ;
#85773 = EDGE_CURVE ( 'NONE', #122378, #94920, #139045, .T. ) ;
#85774 = CARTESIAN_POINT ( 'NONE',  ( -6.121473163371429216, -20.24070752338407431, 7.412974875817805120 ) ) ;
#85775 = LINE ( 'NONE', #95222, #65381 ) ;
#85776 = EDGE_CURVE ( 'NONE', #17549, #59338, #12181, .T. ) ;
#85777 = CARTESIAN_POINT ( 'NONE',  ( 0.000000000000000000, 0.000000000000000000, 5.000000000000000000 ) ) ;
#85778 = CARTESIAN_POINT ( 'NONE',  ( 15.18398860626900237, 28.73617430169797871, 5.000000000000000000 ) ) ;
#85779 = LINE ( 'NONE', #8190, #105192 ) ;
#85780 = FACE_OUTER_BOUND ( 'NONE', #40198, .T. ) ;
#85781 = LINE ( 'NONE', #128582, #115194 ) ;
#85782 = CARTESIAN_POINT ( 'NONE',  ( 57.24586038379622721, 3.974999999999996980, 6.884901960086287964 ) ) ;
#85783 = ADVANCED_FACE ( 'NONE', ( #96213 ), #23679, .F. ) ;
#85784 = CARTESIAN_POINT ( 'NONE',  ( 51.29974487139158867, -27.71228299555242103, 4.000000000000000000 ) ) ;
#85785 = AXIS2_PLACEMENT_3D ( 'NONE', #46030, #101810, #2467 ) ;
#85786 = ORIENTED_EDGE ( 'NONE', *, *, #27161, .T. ) ;
#85787 = ORIENTED_EDGE ( 'NONE', *, *, #46347, .T. ) ;
#85788 = CARTESIAN_POINT ( 'NONE',  ( 50.58333333333332860, 6.884901960086290629, -3.974999999999994316 ) ) ;
#85789 = PLANE ( 'NONE',  #67935 ) ;
#85790 = CARTESIAN_POINT ( 'NONE',  ( -33.29974487139158867, -27.71228299555229313, 4.000000000000000000 ) ) ;
#85791 = VECTOR ( 'NONE', #42677, 1000.000000000000227 ) ;
#85792 =( NAMED_UNIT ( * ) SI_UNIT ( $, .STERADIAN. ) SOLID_ANGLE_UNIT ( ) );
#85793 = ORIENTED_EDGE ( 'NONE', *, *, #63226, .F. ) ;
#85794 = DIRECTION ( 'NONE',  ( 0.7071067811865487940, 0.7071067811865463515, 0.000000000000000000 ) ) ;
#85795 = CARTESIAN_POINT ( 'NONE',  ( 47.83376352523143993, 6.110000000000001208, 1.122388791418549305E-15 ) ) ;
#85796 = ORIENTED_EDGE ( 'NONE', *, *, #57818, .T. ) ;
#85797 = DIRECTION ( 'NONE',  ( 0.000000000000000000, 0.000000000000000000, 1.000000000000000000 ) ) ;
#85798 = ORIENTED_EDGE ( 'NONE', *, *, #98573, .F. ) ;
#85799 = ORIENTED_EDGE ( 'NONE', *, *, #38859, .T. ) ;
#85800 = VECTOR ( 'NONE', #56541, 999.9999999999998863 ) ;
#85801 = CARTESIAN_POINT ( 'NONE',  ( -26.29298673570676925, -21.74070752338405299, 4.999753212805220670 ) ) ;
#85802 = LINE ( 'NONE', #130039, #126426 ) ;
#85803 = CARTESIAN_POINT ( 'NONE',  ( 23.84387692260742142, -22.22500000000000142, 4.000000000000000000 ) ) ;
#85804 = CARTESIAN_POINT ( 'NONE',  ( 14.51078643762690490, -27.52281430457045275, 5.000000000000000000 ) ) ;
#85805 = ORIENTED_EDGE ( 'NONE', *, *, #29731, .F. ) ;
#85806 = CARTESIAN_POINT ( 'NONE',  ( -1.499999999999984013, 14.14708470758591119, -0.5283514160166523643 ) ) ;
#85808 = ORIENTED_EDGE ( 'NONE', *, *, #19747, .T. ) ;
#85807 = DIRECTION ( 'NONE',  ( -0.000000000000000000, -0.3543493200069152693, 0.9351131265310292928 ) ) ;
#85809 = CARTESIAN_POINT ( 'NONE',  ( 86.33376352523144703, 6.110000000000001208, 1.122388791418549305E-15 ) ) ;
#85810 = DIRECTION ( 'NONE',  ( 0.7071067811865487940, 0.7071067811865463515, 0.000000000000000000 ) ) ;
#85811 = DIRECTION ( 'NONE',  ( -0.7071067811865487940, 0.7071067811865463515, 0.000000000000000000 ) ) ;
#85812 = CARTESIAN_POINT ( 'NONE',  ( 15.96626304157554266, 2.055000000000001048, 2.516649172247811554E-16 ) ) ;
#85813 = AXIS2_PLACEMENT_3D ( 'NONE', #91659, #14809, #125737 ) ;
#85814 = CARTESIAN_POINT ( 'NONE',  ( 34.49999999999975842, 19.46425560840029689, 4.994342998332160555 ) ) ;
#85815 = VECTOR ( 'NONE', #6515, 1000.000000000000114 ) ;
#85816 = ORIENTED_EDGE ( 'NONE', *, *, #31839, .F. ) ;
#85817 = CARTESIAN_POINT ( 'NONE',  ( 71.37043019189812298, -3.055000000000001492, 5.291415217122917625 ) ) ;
#85818 = DIRECTION ( 'NONE',  ( 0.7071067811865486830, -0.7071067811865464625, -0.000000000000000000 ) ) ;
#85819 = EDGE_CURVE ( 'NONE', #60588, #6025, #67949, .T. ) ;
#85820 = DIRECTION ( 'NONE',  ( -0.7071067811865486830, 0.7071067811865464625, 0.000000000000000000 ) ) ;
#85821 = FACE_OUTER_BOUND ( 'NONE', #37555, .T. ) ;
#85822 = EDGE_LOOP ( 'NONE', ( #55934, #111538, #47720, #99450, #54532, #77003 ) ) ;
#85823 = ORIENTED_EDGE ( 'NONE', *, *, #72463, .T. ) ;
#85824 = DIRECTION ( 'NONE',  ( -0.6830127018922181881, 0.6830127018922202975, -0.2588190451025214056 ) ) ;
#85825 = AXIS2_PLACEMENT_3D ( 'NONE', #70451, #134239, #103029 ) ;
#85826 = VERTEX_POINT ( 'NONE', #1186 ) ;
#85827 = VECTOR ( 'NONE', #35448, 1000.000000000000227 ) ;
#85829 = ORIENTED_EDGE ( 'NONE', *, *, #21569, .T. ) ;
#85828 = VECTOR ( 'NONE', #50356, 1000.000000000000000 ) ;
#85830 = DIRECTION ( 'NONE',  ( -0.000000000000000000, -0.3543493200069152693, 0.9351131265310292928 ) ) ;
#85831 = ORIENTED_EDGE ( 'NONE', *, *, #112698, .T. ) ;
#85832 = CARTESIAN_POINT ( 'NONE',  ( 64.43749999999998579, 5.819803920172574863, -5.819803920172573086 ) ) ;
#85833 = CARTESIAN_POINT ( 'NONE',  ( 28.49999999999981171, 12.05218569542904739, 5.000000000000000000 ) ) ;
#85834 = VECTOR ( 'NONE', #61015, 1000.000000000000000 ) ;
#85835 = CIRCLE ( 'NONE', #41873, 5.999999999999998224 ) ;
#85836 = VECTOR ( 'NONE', #8733, 999.9999999999998863 ) ;
#85837 = AXIS2_PLACEMENT_3D ( 'NONE', #32979, #77883, #45284 ) ;
#85838 = FACE_OUTER_BOUND ( 'NONE', #52254, .T. ) ;
#85839 = EDGE_CURVE ( 'NONE', #94607, #3249, #142615, .T. ) ;
#85840 = FACE_BOUND ( 'NONE', #40745, .T. ) ;
#85841 = LINE ( 'NONE', #42371, #30481 ) ;
#85842 = ADVANCED_FACE ( 'NONE', ( #78080 ), #44015, .F. ) ;
#85844 = LINE ( 'NONE', #84451, #87324 ) ;
#85843 = AXIS2_PLACEMENT_3D ( 'NONE', #17165, #37505, #126610 ) ;
#85846 = ORIENTED_EDGE ( 'NONE', *, *, #90672, .F. ) ;
#85845 = CARTESIAN_POINT ( 'NONE',  ( 51.41252705046289861, -7.949999999999998401, -4.867971026610728450E-16 ) ) ;
#85847 = DIRECTION ( 'NONE',  ( 0.7071067811865487940, 0.7071067811865463515, -0.000000000000000000 ) ) ;
#85848 = CONTEXT_DEPENDENT_SHAPE_REPRESENTATION ( #28144, #93208 ) ;
#85849 = ORIENTED_EDGE ( 'NONE', *, *, #124152, .T. ) ;
#85850 = ORIENTED_EDGE ( 'NONE', *, *, #33969, .F. ) ;
#85851 = CARTESIAN_POINT ( 'NONE',  ( 88.57876352523145158, -7.482591942790325086E-16, 6.109999999999998543 ) ) ;
#85852 = VERTEX_POINT ( 'NONE', #120838 ) ;
#85853 = ADVANCED_FACE ( 'NONE', ( #44771 ), #21543, .T. ) ;
#85854 = LINE ( 'NONE', #100317, #18892 ) ;
#85855 = VECTOR ( 'NONE', #37458, 1000.000000000000227 ) ;
#85856 = ORIENTED_EDGE ( 'NONE', *, *, #36173, .T. ) ;
#85857 = DIRECTION ( 'NONE',  ( -0.6830127018922180770, -0.6830127018922204085, -0.2588190451025213501 ) ) ;
#85858 = ADVANCED_FACE ( 'NONE', ( #99809 ), #100538, .F. ) ;
#85859 = VECTOR ( 'NONE', #50917, 1000.000000000000227 ) ;
#85860 = CARTESIAN_POINT ( 'NONE',  ( 12.19999999999999574, -39.93000000000000682, 19.06900128115122683 ) ) ;
#85861 = DIRECTION ( 'NONE',  ( -0.3543493200069162685, -0.000000000000000000, -0.9351131265310288487 ) ) ;
#85862 = AXIS2_PLACEMENT_3D ( 'NONE', #75666, #32153, #43740 ) ;
#85863 = DIRECTION ( 'NONE',  ( 0.6830127018922180770, -0.6830127018922204085, -0.2588190451025213501 ) ) ;
#85864 = CARTESIAN_POINT ( 'NONE',  ( 31.17183060077625356, -20.24070752338407431, 4.000000000000000000 ) ) ;
#85865 = VECTOR ( 'NONE', #135467, 1000.000000000000000 ) ;
#85866 = DIRECTION ( 'NONE',  ( 1.000000000000000000, 0.000000000000000000, 0.000000000000000000 ) ) ;
#85867 = PLANE ( 'NONE',  #50886 ) ;
#85868 = VERTEX_POINT ( 'NONE', #143312 ) ;
#85869 = EDGE_CURVE ( 'NONE', #102338, #111053, #132487, .T. ) ;
#85870 = CARTESIAN_POINT ( 'NONE',  ( 8.500000000000000000, 9.521314400968980422E-16, 0.000000000000000000 ) ) ;
#85871 = ORIENTED_EDGE ( 'NONE', *, *, #45673, .F. ) ;
#85872 = VECTOR ( 'NONE', #97141, 1000.000000000000000 ) ;
#85873 = DIRECTION ( 'NONE',  ( 0.3543493200069162685, -0.000000000000000000, -0.9351131265310288487 ) ) ;
#85874 = DIRECTION ( 'NONE',  ( 0.7071067811865486830, -0.7071067811865464625, -0.000000000000000000 ) ) ;
#85875 = ORIENTED_EDGE ( 'NONE', *, *, #65932, .T. ) ;
#85876 = ORIENTED_EDGE ( 'NONE', *, *, #94677, .F. ) ;
#85877 = EDGE_LOOP ( 'NONE', ( #58623, #109377, #104870, #98767 ) ) ;
#85878 = CARTESIAN_POINT ( 'NONE',  ( 35.43793019189810423, -6.110000000000001208, 1.637169565754158951 ) ) ;
#85879 = EDGE_CURVE ( 'NONE', #40957, #114174, #56360, .T. ) ;
#85880 = ORIENTED_EDGE ( 'NONE', *, *, #18443, .F. ) ;
#85881 = DIRECTION ( 'NONE',  ( -0.3543493200069162685, -0.000000000000000000, -0.9351131265310288487 ) ) ;
#85882 = VECTOR ( 'NONE', #86029, 999.9999999999998863 ) ;
#85883 = CARTESIAN_POINT ( 'NONE',  ( 24.10830628287044419, 1.633150327867687324, -6.094999999999991758 ) ) ;
#85884 = CARTESIAN_POINT ( 'NONE',  ( 4.286292163570115221, 13.35440448566885685, -24.66944867099426375 ) ) ;
#85885 = VERTEX_POINT ( 'NONE', #77383 ) ;
#85886 = CARTESIAN_POINT ( 'NONE',  ( 12.69999999999999574, -28.33999999999998565, 13.17925390838734323 ) ) ;
#85887 = ADVANCED_FACE ( 'NONE', ( #75924 ), #65806, .F. ) ;
#85888 = ORIENTED_EDGE ( 'NONE', *, *, #98465, .T. ) ;
#85889 = DIRECTION ( 'NONE',  ( -0.7071067811865486830, 0.7071067811865464625, 0.000000000000000000 ) ) ;
#85890 = VECTOR ( 'NONE', #12851, 999.9999999999998863 ) ;
#85891 = LINE ( 'NONE', #120640, #107703 ) ;
#85893 = EDGE_LOOP ( 'NONE', ( #48433, #131613, #41506, #27969 ) ) ;
#85892 = FACE_OUTER_BOUND ( 'NONE', #131394, .T. ) ;
#85894 = VECTOR ( 'NONE', #111417, 999.9999999999998863 ) ;
#85895 = ORIENTED_EDGE ( 'NONE', *, *, #88541, .T. ) ;
#85896 = CARTESIAN_POINT ( 'NONE',  ( 0.7071067811865406894, 17.25929247661554200, 5.000000000000000000 ) ) ;
#85897 = EDGE_CURVE ( 'NONE', #3922, #103133, #22927, .T. ) ;
#85898 = EDGE_CURVE ( 'NONE', #18445, #42023, #134856, .T. ) ;
#85899 = DIRECTION ( 'NONE',  ( 1.000000000000000000, 0.000000000000000000, 0.000000000000000000 ) ) ;
#85900 = ORIENTED_EDGE ( 'NONE', *, *, #71106, .F. ) ;
#85901 = CARTESIAN_POINT ( 'NONE',  ( -23.84903741288601964, 22.22500000000000142, 0.8029037345187381991 ) ) ;
#85902 = ORIENTED_EDGE ( 'NONE', *, *, #72562, .F. ) ;
#85903 = ORIENTED_EDGE ( 'NONE', *, *, #77287, .T. ) ;
#85904 = ORIENTED_EDGE ( 'NONE', *, *, #69663, .T. ) ;
#85905 = LINE ( 'NONE', #119235, #40299 ) ;
#85906 = COLOUR_RGB ( '', 0.31764706, 0.68627451, 0.89019608) ;
#85907 = DIRECTION ( 'NONE',  ( -0.7071067811865486830, -0.7071067811865464625, -0.000000000000000000 ) ) ;
#85908 = ADVANCED_FACE ( 'NONE', ( #123001 ), #12781, .F. ) ;
#85909 = CARTESIAN_POINT ( 'NONE',  ( 17.99999999999987566, 19.93112307739198386, 4.000000000000000000 ) ) ;
#85910 = LINE ( 'NONE', #136902, #49218 ) ;
#85911 = CARTESIAN_POINT ( 'NONE',  ( 62.99451991528749772, 28.92564299267982264, 4.000000000000000000 ) ) ;
#85912 = EDGE_CURVE ( 'NONE', #18830, #21741, #478, .T. ) ;
#85913 = DIRECTION ( 'NONE',  ( -0.7071067811865487940, 0.7071067811865463515, -0.000000000000000000 ) ) ;
#85914 = ORIENTED_EDGE ( 'NONE', *, *, #18303, .F. ) ;
#85915 = EDGE_CURVE ( 'NONE', #92653, #23590, #110650, .T. ) ;
#85916 = CARTESIAN_POINT ( 'NONE',  ( 66.29974487139159578, -27.71228299555252406, 4.000000000000000000 ) ) ;
#85917 = EDGE_LOOP ( 'NONE', ( #26261, #40882, #87292, #45282 ) ) ;
#85918 = AXIS2_PLACEMENT_3D ( 'NONE', #79064, #123268, #23939 ) ;
#85919 = CARTESIAN_POINT ( 'NONE',  ( 51.18398860626899705, 28.73617430169823095, 5.000000000000000000 ) ) ;
#85920 = CARTESIAN_POINT ( 'NONE',  ( 31.91623647476855297, -7.934999999999990727, 4.858786175617117713E-16 ) ) ;
#85921 = ORIENTED_EDGE ( 'NONE', *, *, #143197, .T. ) ;
#85922 = DIRECTION ( 'NONE',  ( -0.3543493200069162685, -0.000000000000000000, -0.9351131265310288487 ) ) ;
#85923 = EDGE_CURVE ( 'NONE', #61607, #79052, #86808, .T. ) ;
#85924 = CARTESIAN_POINT ( 'NONE',  ( 21.29974487139158512, -27.71228299555221142, 4.000000000000000000 ) ) ;
#85925 = ORIENTED_EDGE ( 'NONE', *, *, #143075, .T. ) ;
#85926 = EDGE_LOOP ( 'NONE', ( #67322, #28135, #47818, #56076, #102996, #112516 ) ) ;
#85927 = CARTESIAN_POINT ( 'NONE',  ( 55.38366852087742842, -49.19090614206224643, 40.79110616923198052 ) ) ;
#85928 = CARTESIAN_POINT ( 'NONE',  ( -13.71003237941630104, 5.842153316012715258, 5.000000000000000000 ) ) ;
#85929 = CARTESIAN_POINT ( 'NONE',  ( 24.18398860626899705, 28.73617430169804265, 5.000000000000000000 ) ) ;
#85930 = DIRECTION ( 'NONE',  ( 0.7071067811865487940, 0.7071067811865463515, 0.000000000000000000 ) ) ;
#85932 = EDGE_CURVE ( 'NONE', #117254, #57105, #120098, .T. ) ;
#85931 = AXIS2_PLACEMENT_3D ( 'NONE', #22406, #111585, #78992 ) ;
#85933 = CARTESIAN_POINT ( 'NONE',  ( 61.01626352523143737, -4.472830434245839371, 4.472830434245839371 ) ) ;
#85934 = CARTESIAN_POINT ( 'NONE',  ( 19.21321903303347511, 12.75929247661559351, 10.29404684609039755 ) ) ;
#85935 = VECTOR ( 'NONE', #94756, 1000.000000000000000 ) ;
#85936 = VECTOR ( 'NONE', #83545, 1000.000000000000000 ) ;
#85937 = LINE ( 'NONE', #141771, #87756 ) ;
#85938 = LINE ( 'NONE', #130901, #53396 ) ;
#85939 = DIRECTION ( 'NONE',  ( 0.7071067811865487940, 0.7071067811865463515, 0.000000000000000000 ) ) ;
#85940 = ORIENTED_EDGE ( 'NONE', *, *, #94398, .T. ) ;
#85941 = DIRECTION ( 'NONE',  ( -1.000000000000000000, -0.000000000000000000, -0.000000000000000000 ) ) ;
#85942 = ORIENTED_EDGE ( 'NONE', *, *, #9909, .F. ) ;
#85943 = COLOUR_RGB ( '', 0.08235294, 0.09019608, 0.10196078) ;
#85944 = AXIS2_PLACEMENT_3D ( 'NONE', #86508, #74196, #132160 ) ;
#85945 = VECTOR ( 'NONE', #136728, 1000.000000000000000 ) ;
#85946 = CARTESIAN_POINT ( 'NONE',  ( -62.99451991528749772, 28.92564299267982264, 4.000000000000000000 ) ) ;
#85948 = CARTESIAN_POINT ( 'NONE',  ( -29.99999999999979039, 20.70535890316558891, 1.956823837851985548 ) ) ;
#85947 = VECTOR ( 'NONE', #89743, 1000.000000000000227 ) ;
#85949 = ORIENTED_EDGE ( 'NONE', *, *, #62047, .F. ) ;
#85950 = VECTOR ( 'NONE', #79353, 1000.000000000000000 ) ;
#85951 = LINE ( 'NONE', #29415, #4369 ) ;
#85953 = EDGE_LOOP ( 'NONE', ( #53710, #49397, #60375, #41301 ) ) ;
#85952 = CARTESIAN_POINT ( 'NONE',  ( 15.00548008471250228, 28.92564299267927552, 4.000000000000000000 ) ) ;
#85954 = FACE_OUTER_BOUND ( 'NONE', #133369, .T. ) ;
#85955 = LINE ( 'NONE', #96782, #34825 ) ;
#85956 = DIRECTION ( 'NONE',  ( 0.000000000000000000, 0.000000000000000000, 1.000000000000000000 ) ) ;
#85957 = VERTEX_POINT ( 'NONE', #109256 ) ;
#85958 = ORIENTED_EDGE ( 'NONE', *, *, #55817, .T. ) ;
#85959 = DIRECTION ( 'NONE',  ( -1.000000000000000000, -0.000000000000000000, -0.000000000000000000 ) ) ;
#85960 = CARTESIAN_POINT ( 'NONE',  ( -28.49999999999980460, -17.91344420646044711, 1.358650452708397127 ) ) ;
#85961 = VECTOR ( 'NONE', #38744, 1000.000000000000000 ) ;
#85962 = CARTESIAN_POINT ( 'NONE',  ( -51.48921356237309510, -27.52281430457091460, 5.000000000000000000 ) ) ;
#85963 = EDGE_CURVE ( 'NONE', #98880, #103456, #112822, .T. ) ;
#85964 = CARTESIAN_POINT ( 'NONE',  ( 84.66252705046289861, 7.949999999999998401, 1.460391307983218338E-15 ) ) ;
#85966 = ADVANCED_FACE ( 'NONE', ( #115641 ), #58511, .F. ) ;
#85965 = CARTESIAN_POINT ( 'NONE',  ( 15.70710678118643422, 14.25929247661556687, 5.000000000000000000 ) ) ;
#85967 = DIRECTION ( 'NONE',  ( -0.000000000000000000, 1.000000000000000000, 1.137193330093851115E-16 ) ) ;
#85968 = EDGE_LOOP ( 'NONE', ( #138864, #34943, #75595, #90904 ) ) ;
#85969 = VECTOR ( 'NONE', #91735, 1000.000000000000000 ) ;
#85970 = CARTESIAN_POINT ( 'NONE',  ( 5.691592354503320905, 3.061616997868380183E-16, -2.500000000000001332 ) ) ;
#85971 = CARTESIAN_POINT ( 'NONE',  ( -30.29974487139158867, -27.71228299555227537, 4.000000000000000000 ) ) ;
#85972 = CARTESIAN_POINT ( 'NONE',  ( 28.58333333333333570, -5.278424836066144543, 3.047499999999995879 ) ) ;
#85973 = ORIENTED_EDGE ( 'NONE', *, *, #1508, .F. ) ;
#85974 = VECTOR ( 'NONE', #55196, 1000.000000000000000 ) ;
#85975 = DIRECTION ( 'NONE',  ( -0.7071067811865486830, -0.7071067811865464625, -0.000000000000000000 ) ) ;
#85976 = EDGE_LOOP ( 'NONE', ( #85463, #42089, #112665, #41142 ) ) ;
#85977 = AXIS2_PLACEMENT_3D ( 'NONE', #131838, #133969, #1290 ) ;
#85978 = CARTESIAN_POINT ( 'NONE',  ( 77.87543019189810423, -5.291415217122920289, -3.055000000000001492 ) ) ;
#85979 = CIRCLE ( 'NONE', #127698, 8.000000000000001776 ) ;
#85980 = CARTESIAN_POINT ( 'NONE',  ( 9.682526172861077640, -2.055000000000000160, 0.000000000000000000 ) ) ;
#85981 = DIRECTION ( 'NONE',  ( -0.000000000000000000, -0.3543493200069152693, 0.9351131265310292928 ) ) ;
#85982 = ORIENTED_EDGE ( 'NONE', *, *, #54447, .F. ) ;
#85983 = CIRCLE ( 'NONE', #39750, 2.500000000000000888 ) ;
#85984 = PLANE ( 'NONE',  #74324 ) ;
#85985 = LINE ( 'NONE', #53350, #11727 ) ;
#85986 = DIRECTION ( 'NONE',  ( -0.7071067811865486830, -0.7071067811865464625, -0.000000000000000000 ) ) ;
#85987 = VECTOR ( 'NONE', #68336, 1000.000000000000000 ) ;
#85988 = DIRECTION ( 'NONE',  ( 0.7071067811865486830, -0.7071067811865464625, -0.000000000000000000 ) ) ;
#85990 = VERTEX_POINT ( 'NONE', #25086 ) ;
#85989 = DIRECTION ( 'NONE',  ( 1.000000000000000000, 0.000000000000000000, 0.000000000000000000 ) ) ;
#85991 = CARTESIAN_POINT ( 'NONE',  ( 128.6956467655712117, -52.10358567238988314, -40.45860062938062640 ) ) ;
#85992 = DIRECTION ( 'NONE',  ( -0.7071067811865487940, 0.7071067811865463515, 0.000000000000000000 ) ) ;
#85993 = CARTESIAN_POINT ( 'NONE',  ( 77.41666666666665719, -6.884901960086287076, -3.975000000000000977 ) ) ;
#85994 = CARTESIAN_POINT ( 'NONE',  ( 10.46799328145038821, 4.202752102959690472E-16, 0.000000000000000000 ) ) ;
#85995 = ORIENTED_EDGE ( 'NONE', *, *, #60532, .F. ) ;
#85996 = ORIENTED_EDGE ( 'NONE', *, *, #55572, .T. ) ;
#85997 = CARTESIAN_POINT ( 'NONE',  ( 73.06293019189811844, 1.637169565754157174, 6.110000000000002984 ) ) ;
#85998 = COLOUR_RGB ( '', 0.40784314, 0.44705882, 0.49803922) ;
#85999 = ORIENTED_EDGE ( 'NONE', *, *, #245, .T. ) ;
#86000 = DIRECTION ( 'NONE',  ( -1.000000000000000000, -0.000000000000000000, -0.000000000000000000 ) ) ;
#86001 = CARTESIAN_POINT ( 'NONE',  ( -34.92500000000001137, 17.81665438641024579, 4.500000000000000888 ) ) ;
#86002 = EDGE_CURVE ( 'NONE', #540, #133266, #91105, .T. ) ;
#86003 = VECTOR ( 'NONE', #34843, 1000.000000000000000 ) ;
#86004 = CARTESIAN_POINT ( 'NONE',  ( 59.28752705046289151, 0.000000000000000000, -7.949999999999998401 ) ) ;
#86005 = CARTESIAN_POINT ( 'NONE',  ( 27.18398860626900060, 28.73617430169806042, 5.000000000000000000 ) ) ;
#86006 = EDGE_LOOP ( 'NONE', ( #89741, #119831, #53384, #126137 ) ) ;
#86007 = CIRCLE ( 'NONE', #35020, 5.968999999999998529 ) ;
#86008 = CARTESIAN_POINT ( 'NONE',  ( -12.69999999999998153, 0.3999999999999995226, 2.467792535850613866 ) ) ;
#86009 = DIRECTION ( 'NONE',  ( -0.7071067811865487940, 0.7071067811865463515, 0.000000000000000000 ) ) ;
#86010 = ORIENTED_EDGE ( 'NONE', *, *, #100693, .T. ) ;
#86011 = CARTESIAN_POINT ( 'NONE',  ( 34.92499999999998295, -9.183345613589446899, 4.500000000000000888 ) ) ;
#86012 = DIRECTION ( 'NONE',  ( -0.7071067811865486830, -0.7071067811865464625, 0.000000000000000000 ) ) ;
#86013 = FACE_OUTER_BOUND ( 'NONE', #3309, .T. ) ;
#86014 = VECTOR ( 'NONE', #65276, 1000.000000000000227 ) ;
#86015 =( BOUNDED_CURVE ( )  B_SPLINE_CURVE ( 3, ( #40007, #94344, #61067, #39273 ),
 .UNSPECIFIED., .F., .T. ) 
 B_SPLINE_CURVE_WITH_KNOTS ( ( 4, 4 ),
 ( 5.143245962375964986, 6.645403452391247079 ),
 .UNSPECIFIED. ) 
 CURVE ( )  GEOMETRIC_REPRESENTATION_ITEM ( )  RATIONAL_B_SPLINE_CURVE ( ( 1.000000000000000000, 0.8206354192515239454, 0.8206354192515239454, 1.000000000000000000 ) ) 
 REPRESENTATION_ITEM ( '' )  );
#86016 = ORIENTED_EDGE ( 'NONE', *, *, #60183, .F. ) ;
#86017 = ORIENTED_EDGE ( 'NONE', *, *, #121146, .T. ) ;
#86018 = ADVANCED_FACE ( 'NONE', ( #101231, #69343, #136712 ), #91781, .F. ) ;
#86019 = ADVANCED_FACE ( 'NONE', ( #135324 ), #36008, .F. ) ;
#86020 = EDGE_CURVE ( 'NONE', #91527, #139662, #26538, .T. ) ;
#86021 = CARTESIAN_POINT ( 'NONE',  ( -26.99999999999981526, -0.2811185226894545863, -5.995736974527452467 ) ) ;
#86022 = LINE ( 'NONE', #55550, #43314 ) ;
#86023 = CARTESIAN_POINT ( 'NONE',  ( -18.29974487139159223, -27.71228299555219010, 4.000000000000000000 ) ) ;
#86024 = LINE ( 'NONE', #10574, #101476 ) ;
#86025 = VECTOR ( 'NONE', #101123, 999.9999999999998863 ) ;
#86026 = FACE_OUTER_BOUND ( 'NONE', #142358, .T. ) ;
#86027 = EDGE_CURVE ( 'NONE', #106514, #114480, #49024, .T. ) ;
#86028 = EDGE_CURVE ( 'NONE', #13154, #49277, #136006, .T. ) ;
#86029 = DIRECTION ( 'NONE',  ( 0.7071067811865487940, 0.7071067811865463515, 0.000000000000000000 ) ) ;
#86030 = ORIENTED_EDGE ( 'NONE', *, *, #140576, .F. ) ;
#86031 = VERTEX_POINT ( 'NONE', #92482 ) ;
#86032 = ORIENTED_EDGE ( 'NONE', *, *, #111123, .T. ) ;
#86033 = EDGE_CURVE ( 'NONE', #15696, #54913, #93216, .T. ) ;
#86034 = ORIENTED_EDGE ( 'NONE', *, *, #62050, .F. ) ;
#86035 = CARTESIAN_POINT ( 'NONE',  ( 183.9820196591358012, -48.55783623716212105, 38.28685941347691113 ) ) ;
#86036 = VECTOR ( 'NONE', #88972, 999.9999999999998863 ) ;
#86037 = LINE ( 'NONE', #20767, #131173 ) ;
#86038 = VECTOR ( 'NONE', #120622, 1000.000000000000000 ) ;
#86039 = EDGE_CURVE ( 'NONE', #62749, #121709, #113526, .T. ) ;
#86040 = AXIS2_PLACEMENT_3D ( 'NONE', #80171, #3274, #78722 ) ;
#86041 = CARTESIAN_POINT ( 'NONE',  ( -34.49999999999975131, -2.568876922607788327, 4.000000000000000000 ) ) ;
#86042 = ORIENTED_EDGE ( 'NONE', *, *, #71000, .F. ) ;
#86043 = DIRECTION ( 'NONE',  ( 0.000000000000000000, -1.000000000000000000, 0.000000000000000000 ) ) ;
#86044 = DIRECTION ( 'NONE',  ( 1.734723475976806848E-16, -1.000000000000000000, 0.000000000000000000 ) ) ;
#86045 = CARTESIAN_POINT ( 'NONE',  ( 57.68336038379621300, -2.130196079827426203, 7.949999999999996625 ) ) ;
#86046 = DIRECTION ( 'NONE',  ( 0.000000000000000000, 0.000000000000000000, -1.000000000000000000 ) ) ;
#86047 = VECTOR ( 'NONE', #30869, 1000.000000000000227 ) ;
#86048 = AXIS2_PLACEMENT_3D ( 'NONE', #141980, #42668, #75985 ) ;
#86049 = VECTOR ( 'NONE', #124630, 1000.000000000000000 ) ;
#86050 = AXIS2_PLACEMENT_3D ( 'NONE', #127363, #61448, #28063 ) ;
#86051 = EDGE_CURVE ( 'NONE', #81376, #111873, #114017, .T. ) ;
#86052 = FACE_OUTER_BOUND ( 'NONE', #29012, .T. ) ;
#86053 = ORIENTED_EDGE ( 'NONE', *, *, #40754, .T. ) ;
#86054 = VECTOR ( 'NONE', #18590, 1000.000000000000000 ) ;
#86055 = LINE ( 'NONE', #52691, #5515 ) ;
#86056 = CARTESIAN_POINT ( 'NONE',  ( 49.99999999999998579, 0.000000000000000000, -7.950000000000000178 ) ) ;
#86057 = EDGE_LOOP ( 'NONE', ( #3913, #120458, #7521, #8745, #142881, #18882 ) ) ;
#86058 = PLANE ( 'NONE',  #122259 ) ;
#86059 = VERTEX_POINT ( 'NONE', #114254 ) ;
#86060 = VERTEX_POINT ( 'NONE', #59205 ) ;
#86061 = ORIENTED_EDGE ( 'NONE', *, *, #82077, .T. ) ;
#86062 = VECTOR ( 'NONE', #116844, 1000.000000000000000 ) ;
#86063 = CARTESIAN_POINT ( 'NONE',  ( 61.97959685856476852, 6.109999999999999432, 1.637169565754164280 ) ) ;
#86064 = ADVANCED_FACE ( 'NONE', ( #14929 ), #39576, .T. ) ;
#86065 = ORIENTED_EDGE ( 'NONE', *, *, #54658, .T. ) ;
#86066 = ORIENTED_EDGE ( 'NONE', *, *, #124592, .F. ) ;
#86067 = DIRECTION ( 'NONE',  ( 0.7071067811865487940, 0.7071067811865463515, 0.000000000000000000 ) ) ;
#86068 = PRESENTATION_STYLE_ASSIGNMENT (( #41849 ) ) ;
#86069 = CARTESIAN_POINT ( 'NONE',  ( 99.75043019189810423, 3.055000000000002824, -5.291415217122919401 ) ) ;
#86070 = DIRECTION ( 'NONE',  ( 0.7071067811865487940, 0.7071067811865463515, 0.000000000000000000 ) ) ;
#86071 = LINE ( 'NONE', #30994, #111459 ) ;
#86072 = EDGE_CURVE ( 'NONE', #45062, #2478, #77000, .T. ) ;
#86073 = VERTEX_POINT ( 'NONE', #41696 ) ;
#86074 = CARTESIAN_POINT ( 'NONE',  ( -9.183988606268997046, 28.73617430169793607, 5.000000000000000000 ) ) ;
#86075 = DIRECTION ( 'NONE',  ( -0.000000000000000000, 0.000000000000000000, 1.000000000000000000 ) ) ;
#86076 = LINE ( 'NONE', #87503, #72223 ) ;
#86077 = VECTOR ( 'NONE', #88202, 1000.000000000000000 ) ;
#86079 = EDGE_CURVE ( 'NONE', #1659, #54031, #6878, .T. ) ;
#86078 = FACE_OUTER_BOUND ( 'NONE', #1139, .T. ) ;
#86080 = ORIENTED_EDGE ( 'NONE', *, *, #24417, .F. ) ;
#86081 = VECTOR ( 'NONE', #78007, 1000.000000000000000 ) ;
#86082 = PLANE ( 'NONE',  #120070 ) ;
#86083 = ORIENTED_EDGE ( 'NONE', *, *, #3010, .T. ) ;
#86084 = EDGE_CURVE ( 'NONE', #39673, #80757, #7614, .T. ) ;
#86085 = AXIS2_PLACEMENT_3D ( 'NONE', #135647, #92114, #125488 ) ;
#86086 = ORIENTED_EDGE ( 'NONE', *, *, #40865, .T. ) ;
#86087 = VERTEX_POINT ( 'NONE', #40985 ) ;
#86088 = CARTESIAN_POINT ( 'NONE',  ( 120.6620968585647802, -5.291415217122919401, 3.054999999999997939 ) ) ;
#86089 = ORIENTED_EDGE ( 'NONE', *, *, #90452, .F. ) ;
#86090 = ADVANCED_FACE ( 'NONE', ( #51155 ), #128702, .T. ) ;
#86091 = CARTESIAN_POINT ( 'NONE',  ( -3.792893218813424117, 12.75929247661558996, 5.000000000000000000 ) ) ;
#86092 = CARTESIAN_POINT ( 'NONE',  ( -26.99451991528749417, 28.92564299267956685, 4.000000000000000000 ) ) ;
#86093 = ORIENTED_EDGE ( 'NONE', *, *, #105807, .T. ) ;
#86094 = CARTESIAN_POINT ( 'NONE',  ( -21.60769999999998703, 3.130000000000008331, -22.35000000000000142 ) ) ;
#86095 = ORIENTED_EDGE ( 'NONE', *, *, #13381, .T. ) ;
#86096 = CIRCLE ( 'NONE', #23586, 1.749999999999999778 ) ;
#86097 = CARTESIAN_POINT ( 'NONE',  ( 0.4162364747685527444, -7.934999999999990727, 4.858786175617117713E-16 ) ) ;
#86098 = DIRECTION ( 'NONE',  ( 0.000000000000000000, 0.000000000000000000, 1.000000000000000000 ) ) ;
#86099 = DIRECTION ( 'NONE',  ( -0.000000000000000000, 0.3543493200069153248, 0.9351131265310292928 ) ) ;
#86100 = ADVANCED_FACE ( 'NONE', ( #30843 ), #85180, .T. ) ;
#86101 = CARTESIAN_POINT ( 'NONE',  ( 38.77083333333331439, -7.949999999999998401, -2.130196079827426203 ) ) ;
#86102 = VERTEX_POINT ( 'NONE', #129404 ) ;
#86103 = ORIENTED_EDGE ( 'NONE', *, *, #46468, .T. ) ;
#86104 = AXIS2_PLACEMENT_3D ( 'NONE', #107893, #8561, #52807 ) ;
#86105 = EDGE_LOOP ( 'NONE', ( #107373, #60852, #57483, #23772 ) ) ;
#86106 = DIRECTION ( 'NONE',  ( 0.7071067811865487940, 0.7071067811865463515, 0.000000000000000000 ) ) ;
#86107 = PLANE ( 'NONE',  #95036 ) ;
#86108 = VECTOR ( 'NONE', #140159, 999.9999999999998863 ) ;
#86109 = CARTESIAN_POINT ( 'NONE',  ( -5.994519915287488843, 28.92564299267942118, 4.000000000000000000 ) ) ;
#86110 = EDGE_CURVE ( 'NONE', #101632, #42277, #60641, .T. ) ;
#86111 = DIRECTION ( 'NONE',  ( 0.7071067811865487940, 0.7071067811865463515, 0.000000000000000000 ) ) ;
#86112 = CARTESIAN_POINT ( 'NONE',  ( -2.207106781186518596, -2.240707523384260824, 5.000000000000000000 ) ) ;
#86113 = DIRECTION ( 'NONE',  ( 0.000000000000000000, 0.000000000000000000, -1.000000000000000000 ) ) ;
#86114 = CARTESIAN_POINT ( 'NONE',  ( 29.16709685856476497, -3.055000000000000160, -5.291415217122921177 ) ) ;
#86115 =( NAMED_UNIT ( * ) SI_UNIT ( $, .STERADIAN. ) SOLID_ANGLE_UNIT ( ) );
#86116 = LINE ( 'NONE', #29571, #95202 ) ;
#86117 = VERTEX_POINT ( 'NONE', #94627 ) ;
#86118 = DIRECTION ( 'NONE',  ( -0.3543493200069162685, -0.000000000000000000, -0.9351131265310288487 ) ) ;
#86119 = MECHANICAL_DESIGN_GEOMETRIC_PRESENTATION_REPRESENTATION (  '', ( #18956 ), #137027 ) ;
#86120 = DIRECTION ( 'NONE',  ( -0.7071067811865486830, -0.7071067811865464625, 0.000000000000000000 ) ) ;
#86121 = ORIENTED_EDGE ( 'NONE', *, *, #142315, .F. ) ;
#86122 = DIRECTION ( 'NONE',  ( 0.6830127018922181881, 0.6830127018922202975, -0.2588190451025214056 ) ) ;
#86125 = EDGE_CURVE ( 'NONE', #71270, #65995, #83810, .T. ) ;
#86124 = ORIENTED_EDGE ( 'NONE', *, *, #99471, .T. ) ;
#86123 = CARTESIAN_POINT ( 'NONE',  ( 25.17183060077630330, 15.75929247661556332, 4.000000000000000000 ) ) ;
#86126 = LINE ( 'NONE', #131057, #80798 ) ;
#86127 = EDGE_CURVE ( 'NONE', #82762, #21344, #19229, .T. ) ;
#86128 = EDGE_LOOP ( 'NONE', ( #140268, #83401, #83293, #67506 ) ) ;
#86129 = CARTESIAN_POINT ( 'NONE',  ( 9.328169399223463998, -12.74070752338415247, 4.000000000000000000 ) ) ;
#86131 = ORIENTED_EDGE ( 'NONE', *, *, #48328, .T. ) ;
#86130 = VECTOR ( 'NONE', #54426, 1000.000000000000000 ) ;
#86132 = LINE ( 'NONE', #64375, #76769 ) ;
#86133 = VERTEX_POINT ( 'NONE', #5467 ) ;
#86134 = CARTESIAN_POINT ( 'NONE',  ( 92.97502705046289861, -5.819803920172573086, 5.819803920172573086 ) ) ;
#86135 = EDGE_CURVE ( 'NONE', #7775, #53800, #72943, .T. ) ;
#86136 = CARTESIAN_POINT ( 'NONE',  ( 109.7458603837962272, 3.974999999999996980, 6.884901960086287964 ) ) ;
#86137 = CARTESIAN_POINT ( 'NONE',  ( -34.92500000000001137, 7.701930566820932356, 4.500000000000000888 ) ) ;
#86138 = DIRECTION ( 'NONE',  ( -0.7071067811865487940, 0.7071067811865463515, -0.000000000000000000 ) ) ;
#86139 = CARTESIAN_POINT ( 'NONE',  ( 20.25795612380215971, -2.670494247963030698, 4.000000000000000000 ) ) ;
#86140 = CARTESIAN_POINT ( 'NONE',  ( 8.999999999999941380, -6.033600742197681832, 5.000000000000000000 ) ) ;
#86141 = DIRECTION ( 'NONE',  ( -0.000000000000000000, -1.000000000000000000, 0.000000000000000000 ) ) ;
#86142 = CARTESIAN_POINT ( 'NONE',  ( 7.000000000000000888, 0.000000000000000000, 6.094999999999989981 ) ) ;
#86143 = CARTESIAN_POINT ( 'NONE',  ( 21.41623647476855652, -7.934999999999990727, 4.858786175617117713E-16 ) ) ;
#86144 = VECTOR ( 'NONE', #33016, 1000.000000000000000 ) ;
#86145 = VECTOR ( 'NONE', #24035, 1000.000000000000000 ) ;
#86147 = CARTESIAN_POINT ( 'NONE',  ( -25.82816939922334853, 15.75929247661557042, 4.000000000000000000 ) ) ;
#86146 = VECTOR ( 'NONE', #113099, 1000.000000000000227 ) ;
#86148 = DIRECTION ( 'NONE',  ( -0.7071067811865486830, -0.7071067811865464625, 0.000000000000000000 ) ) ;
#86149 = VERTEX_POINT ( 'NONE', #85909 ) ;
#86150 = ORIENTED_EDGE ( 'NONE', *, *, #19505, .T. ) ;
#86151 = MECHANICAL_DESIGN_GEOMETRIC_PRESENTATION_REPRESENTATION (  '', ( #30591 ), #111601 ) ;
#86152 = AXIS2_PLACEMENT_3D ( 'NONE', #87109, #119695, #41447 ) ;
#86153 = EDGE_CURVE ( 'NONE', #18419, #97224, #84506, .T. ) ;
#86154 = CARTESIAN_POINT ( 'NONE',  ( 0.000000000000000000, -21.72500000000000142, 4.500000000000000888 ) ) ;
#86155 = ORIENTED_EDGE ( 'NONE', *, *, #16713, .F. ) ;
#86156 = CARTESIAN_POINT ( 'NONE',  ( 92.24586038379622721, 3.974999999999996980, 6.884901960086287964 ) ) ;
#86157 = DIRECTION ( 'NONE',  ( 0.000000000000000000, 0.000000000000000000, 1.000000000000000000 ) ) ;
#86158 = DIRECTION ( 'NONE',  ( -0.6830127018922181881, 0.6830127018922202975, -0.2588190451025214056 ) ) ;
#86159 = VECTOR ( 'NONE', #48183, 1000.000000000000000 ) ;
#86160 = AXIS2_PLACEMENT_3D ( 'NONE', #103401, #49792, #82403 ) ;
#86161 = PRESENTATION_LAYER_ASSIGNMENT (  '', '', ( #97739 ) ) ;
#86162 = ORIENTED_EDGE ( 'NONE', *, *, #143533, .F. ) ;
#86163 = CARTESIAN_POINT ( 'NONE',  ( 3.707013264293012256, -21.74070752338405654, 4.999753212805217117 ) ) ;
#86164 = CARTESIAN_POINT ( 'NONE',  ( 92.58333333333332860, 6.884901960086290629, -3.974999999999994316 ) ) ;
#86165 = EDGE_CURVE ( 'NONE', #127309, #63645, #62045, .T. ) ;
#86166 = CARTESIAN_POINT ( 'NONE',  ( 0.6713702758572441809, -52.14999999999999147, 41.05044666116288710 ) ) ;
#86168 = EDGE_LOOP ( 'NONE', ( #103272, #37591, #131533 ) ) ;
#86167 = LINE ( 'NONE', #53536, #12760 ) ;
#86169 = CARTESIAN_POINT ( 'NONE',  ( 0.000000000000000000, 21.72500000000000142, 4.500000000000000888 ) ) ;
#86170 =( NAMED_UNIT ( * ) SI_UNIT ( $, .STERADIAN. ) SOLID_ANGLE_UNIT ( ) );
#86171 = CARTESIAN_POINT ( 'NONE',  ( -5.700255128608413102, -27.71228299555201957, 4.000000000000000000 ) ) ;
#86172 = DIRECTION ( 'NONE',  ( 1.000000000000000000, 0.000000000000000000, 0.000000000000000000 ) ) ;
#86173 = LINE ( 'NONE', #118782, #42225 ) ;
#86174 = ORIENTED_EDGE ( 'NONE', *, *, #60650, .T. ) ;
#86175 = ORIENTED_EDGE ( 'NONE', *, *, #131799, .F. ) ;
#86176 = ORIENTED_EDGE ( 'NONE', *, *, #142033, .F. ) ;
#86177 = CARTESIAN_POINT ( 'NONE',  ( 99.89626352523141861, 4.472830434245840259, -4.472830434245839371 ) ) ;
#86178 = VERTEX_POINT ( 'NONE', #139618 ) ;
#86179 = CARTESIAN_POINT ( 'NONE',  ( 129.2310344399266171, -47.51495700085919083, 36.79359617903138258 ) ) ;
#86180 = DIRECTION ( 'NONE',  ( -0.6830127018922180770, -0.6830127018922204085, -0.2588190451025213501 ) ) ;
#86181 = VERTEX_POINT ( 'NONE', #106203 ) ;
#86182 = LINE ( 'NONE', #74607, #35221 ) ;
#86183 = CARTESIAN_POINT ( 'NONE',  ( 14.81601139373099585, 28.73617430169776910, 5.000000000000000000 ) ) ;
#86184 = AXIS2_PLACEMENT_3D ( 'NONE', #117214, #138291, #38970 ) ;
#86185 = CARTESIAN_POINT ( 'NONE',  ( 96.89126352523143737, -4.472830434245839371, -4.472830434245839371 ) ) ;
#86186 = VERTEX_POINT ( 'NONE', #116403 ) ;
#86187 = VECTOR ( 'NONE', #130492, 1000.000000000000000 ) ;
#86188 = DIRECTION ( 'NONE',  ( -0.7071067811865487940, 0.7071067811865463515, -0.000000000000000000 ) ) ;
#86189 = EDGE_CURVE ( 'NONE', #50892, #94083, #17092, .T. ) ;
#86190 = DIRECTION ( 'NONE',  ( -0.7071067811865486830, -0.7071067811865464625, -0.000000000000000000 ) ) ;
#86191 = CARTESIAN_POINT ( 'NONE',  ( 115.7708333333333428, -7.949999999999998401, -2.130196079827426203 ) ) ;
#86192 = VECTOR ( 'NONE', #731, 999.9999999999998863 ) ;
#86193 = CARTESIAN_POINT ( 'NONE',  ( 7.139999999999985469, -39.92999999999999972, -40.00000000000000000 ) ) ;
#86194 = EDGE_CURVE ( 'NONE', #73530, #135631, #73616, .T. ) ;
#86195 = ORIENTED_EDGE ( 'NONE', *, *, #52871, .F. ) ;
#86196 = ORIENTED_EDGE ( 'NONE', *, *, #117004, .T. ) ;
#86197 = EDGE_LOOP ( 'NONE', ( #74647, #125854, #88388 ) ) ;
#86198 = CARTESIAN_POINT ( 'NONE',  ( 0.000000000000000000, 0.000000000000000000, 5.000000000000000000 ) ) ;
#86199 = ADVANCED_FACE ( 'NONE', ( #51877 ), #140295, .F. ) ;
#86200 = EDGE_CURVE ( 'NONE', #128517, #71727, #52561, .T. ) ;
#86201 = CARTESIAN_POINT ( 'NONE',  ( 36.18398860626899705, 28.73617430169812437, 5.000000000000000000 ) ) ;
#86202 = CARTESIAN_POINT ( 'NONE',  ( 16.69206980810188767, -7.934999999999990727, -2.126176841940955242 ) ) ;
#86203 = VECTOR ( 'NONE', #100149, 999.9999999999998863 ) ;
#86204 = PLANE ( 'NONE',  #34135 ) ;
#86205 = FACE_OUTER_BOUND ( 'NONE', #84378, .T. ) ;
#86206 = EDGE_CURVE ( 'NONE', #128869, #103370, #56190, .T. ) ;
#86207 = EDGE_CURVE ( 'NONE', #112438, #89438, #1021, .T. ) ;
#86208 =( NAMED_UNIT ( * ) SI_UNIT ( $, .STERADIAN. ) SOLID_ANGLE_UNIT ( ) );
#86209 = ADVANCED_FACE ( 'NONE', ( #88061 ), #109806, .T. ) ;
#86210 = VERTEX_POINT ( 'NONE', #33002 ) ;
#86211 = ORIENTED_EDGE ( 'NONE', *, *, #7550, .T. ) ;
#86213 = EDGE_CURVE ( 'NONE', #112438, #56577, #9896, .T. ) ;
#86212 = DIRECTION ( 'NONE',  ( -0.000000000000000000, -0.3543493200069152693, 0.9351131265310292928 ) ) ;
#86214 = ORIENTED_EDGE ( 'NONE', *, *, #24513, .F. ) ;
#86215 = VERTEX_POINT ( 'NONE', #120658 ) ;
#86216 = VECTOR ( 'NONE', #54135, 1000.000000000000000 ) ;
#86217 = VECTOR ( 'NONE', #79036, 1000.000000000000227 ) ;
#86218 = EDGE_CURVE ( 'NONE', #5541, #69693, #31540, .T. ) ;
#86219 = EDGE_CURVE ( 'NONE', #66330, #76165, #21376, .T. ) ;
#86220 = CARTESIAN_POINT ( 'NONE',  ( 7.799999601179139042, -2.500000000000000444, 0.000000000000000000 ) ) ;
#86221 = EDGE_LOOP ( 'NONE', ( #6759, #6693, #98857, #39098 ) ) ;
#86222 = DIRECTION ( 'NONE',  ( -1.000000000000000000, -1.224606353822377258E-16, -0.000000000000000000 ) ) ;
#86223 = SPHERICAL_SURFACE ( 'NONE', #57788, 0.5000000000000000000 ) ;
#86224 = CARTESIAN_POINT ( 'NONE',  ( 8.816011393731004731, 28.73617430169781173, 5.000000000000000000 ) ) ;
#86225 = VECTOR ( 'NONE', #42087, 1000.000000000000000 ) ;
#86226 = DIRECTION ( 'NONE',  ( 3.071323233543530392E-32, -2.242629915582283412E-16, 1.000000000000000000 ) ) ;
#86227 = AXIS2_PLACEMENT_3D ( 'NONE', #131123, #110753, #99917 ) ;
#86228 = B_SPLINE_CURVE_WITH_KNOTS ( 'NONE', 3,
 ( #143224, #77292, #43924, #33776 ),
 .UNSPECIFIED., .F., .F.,
 ( 4, 4 ),
 ( 0.0007011148265759370056, 0.001001374831347506215 ),
 .UNSPECIFIED. ) ;
#86229 = LINE ( 'NONE', #130453, #7294 ) ;
#86230 = ORIENTED_EDGE ( 'NONE', *, *, #31670, .F. ) ;
#86231 = EDGE_CURVE ( 'NONE', #64832, #42322, #95586, .T. ) ;
#86232 =( LENGTH_UNIT ( ) NAMED_UNIT ( * ) SI_UNIT ( .MILLI., .METRE. ) );
#86233 = ORIENTED_EDGE ( 'NONE', *, *, #54657, .T. ) ;
#86234 = CARTESIAN_POINT ( 'NONE',  ( 25.40000000000001279, 6.400415038920557187, -4.708210710744500815 ) ) ;
#86235 = CARTESIAN_POINT ( 'NONE',  ( 19.88523551879106677, -2.838375494165454871, -34.13199556651682798 ) ) ;
#86236 = VERTEX_POINT ( 'NONE', #77211 ) ;
#86237 = SURFACE_STYLE_USAGE ( .BOTH. , #42021 ) ;
#86238 = EDGE_LOOP ( 'NONE', ( #134377, #96137, #25012, #114071 ) ) ;
#86239 = DIRECTION ( 'NONE',  ( -0.000000000000000000, -0.3543493200069152693, 0.9351131265310292928 ) ) ;
#86240 = EDGE_LOOP ( 'NONE', ( #111483, #101566, #15897, #29705, #58404 ) ) ;
#86241 = ORIENTED_EDGE ( 'NONE', *, *, #33444, .T. ) ;
#86242 = VECTOR ( 'NONE', #5882, 1000.000000000000000 ) ;
#86243 = EDGE_CURVE ( 'NONE', #68263, #56149, #33699, .T. ) ;
#86244 = EDGE_LOOP ( 'NONE', ( #142021, #47920, #73107, #33352 ) ) ;
#86245 = CARTESIAN_POINT ( 'NONE',  ( 28.49543019189811233, 5.291415217122916737, 3.055000000000001936 ) ) ;
#86246 = LINE ( 'NONE', #55049, #101617 ) ;
#86247 = CARTESIAN_POINT ( 'NONE',  ( 17.84878961325748037, 4.584330080086930965E-16, 0.000000000000000000 ) ) ;
#86248 = PLANE ( 'NONE',  #68272 ) ;
#86249 = DIRECTION ( 'NONE',  ( 0.7071067811865487940, 0.7071067811865463515, 0.000000000000000000 ) ) ;
#86250 = CARTESIAN_POINT ( 'NONE',  ( 72.48921356237309510, -27.52281430457106026, 5.000000000000000000 ) ) ;
#86251 = AXIS2_PLACEMENT_3D ( 'NONE', #94121, #73128, #93431 ) ;
#86252 = AXIS2_PLACEMENT_3D ( 'NONE', #42780, #65975, #10810 ) ;
#86253 = VECTOR ( 'NONE', #21998, 1000.000000000000000 ) ;
#86254 = CARTESIAN_POINT ( 'NONE',  ( -22.78678096696627264, 12.75929247661559351, 10.29404684609029985 ) ) ;
#86255 = AXIS2_PLACEMENT_3D ( 'NONE', #27778, #5289, #93758 ) ;
#86257 = EDGE_CURVE ( 'NONE', #101316, #58036, #141744, .T. ) ;
#86256 = PLANE ( 'NONE',  #57563 ) ;
#86258 = DIRECTION ( 'NONE',  ( -0.7071067811865486830, 0.7071067811865464625, 0.000000000000000000 ) ) ;
#86259 = CARTESIAN_POINT ( 'NONE',  ( 25.19159235450331735, 2.500000000000001776, 0.000000000000000000 ) ) ;
#86260 = VERTEX_POINT ( 'NONE', #130873 ) ;
#86261 = ADVANCED_FACE ( 'NONE', ( #98228 ), #43845, .F. ) ;
#86262 = ORIENTED_EDGE ( 'NONE', *, *, #12186, .T. ) ;
#86263 = CIRCLE ( 'NONE', #26031, 2.500000000000002220 ) ;
#86264 = VERTEX_POINT ( 'NONE', #122093 ) ;
#86265 = AXIS2_PLACEMENT_3D ( 'NONE', #113404, #125006, #80112 ) ;
#86266 = ORIENTED_EDGE ( 'NONE', *, *, #90707, .F. ) ;
#86267 = CARTESIAN_POINT ( 'NONE',  ( -0.5870628340341963458, 1.186303938595100860, 3.957500374151529332 ) ) ;
#86268 = VERTEX_POINT ( 'NONE', #111211 ) ;
#86269 = EDGE_CURVE ( 'NONE', #13745, #78997, #5332, .T. ) ;
#86270 = ORIENTED_EDGE ( 'NONE', *, *, #74756, .T. ) ;
#86271 = CARTESIAN_POINT ( 'NONE',  ( 57.29974487139158157, -27.71228299555246011, 4.000000000000000000 ) ) ;
#86272 = LINE ( 'NONE', #73954, #140434 ) ;
#86273 = DIRECTION ( 'NONE',  ( -0.7071067811865487940, 0.7071067811865463515, 0.000000000000000000 ) ) ;
#86274 = ORIENTED_EDGE ( 'NONE', *, *, #19290, .T. ) ;
#86275 = DIRECTION ( 'NONE',  ( -1.000000000000000000, -1.224606353822377258E-16, -0.000000000000000000 ) ) ;
#86276 = ORIENTED_EDGE ( 'NONE', *, *, #13405, .F. ) ;
#86277 = FACE_OUTER_BOUND ( 'NONE', #40684, .T. ) ;
#86278 = FACE_OUTER_BOUND ( 'NONE', #79877, .T. ) ;
#86279 = CIRCLE ( 'NONE', #40050, 2.500000000000000444 ) ;
#86280 = CARTESIAN_POINT ( 'NONE',  ( 12.17123647476855375, 0.000000000000000000, 7.934999999999990727 ) ) ;
#86281 = ORIENTED_EDGE ( 'NONE', *, *, #71649, .F. ) ;
#86282 = CARTESIAN_POINT ( 'NONE',  ( 88.14126352523143737, 4.472830434245837594, 4.472830434245841147 ) ) ;
#86283 = CARTESIAN_POINT ( 'NONE',  ( 9.745384874281414866, -8.447767063957357436, -4.346192636695838551 ) ) ;
#86285 = EDGE_CURVE ( 'NONE', #62294, #90422, #34392, .T. ) ;
#86284 = DIRECTION ( 'NONE',  ( -0.6830127018922181881, 0.6830127018922202975, -0.2588190451025214056 ) ) ;
#86286 = DIRECTION ( 'NONE',  ( -0.7071067811865487940, 0.7071067811865463515, 0.000000000000000000 ) ) ;
#86287 = VERTEX_POINT ( 'NONE', #134433 ) ;
#86288 = ORIENTED_EDGE ( 'NONE', *, *, #136879, .T. ) ;
#86289 = DIRECTION ( 'NONE',  ( 0.7071067811865487940, 0.7071067811865463515, 0.000000000000000000 ) ) ;
#86290 = ORIENTED_EDGE ( 'NONE', *, *, #27747, .T. ) ;
#86291 = CARTESIAN_POINT ( 'NONE',  ( -9.437085545171145284, -22.22500000000000142, -4.658323575210101986 ) ) ;
#86292 = LINE ( 'NONE', #63127, #7018 ) ;
#86293 = CARTESIAN_POINT ( 'NONE',  ( 2.865004262483764830, 3.759292476615685441, 15.36553568819725513 ) ) ;
#86294 = LINE ( 'NONE', #75413, #63444 ) ;
#86295 = ORIENTED_EDGE ( 'NONE', *, *, #76425, .T. ) ;
#86296 = AXIS2_PLACEMENT_3D ( 'NONE', #85150, #129365, #30052 ) ;
#86297 = DIRECTION ( 'NONE',  ( 0.000000000000000000, -1.000000000000000000, 0.000000000000000000 ) ) ;
#86298 = ADVANCED_FACE ( 'NONE', ( #135847 ), #103202, .F. ) ;
#86299 = AXIS2_PLACEMENT_3D ( 'NONE', #121551, #22226, #66488 ) ;
#86300 = CARTESIAN_POINT ( 'NONE',  ( -10.17183060077640455, -2.240707523384259492, 4.000000000000000000 ) ) ;
#86301 = CARTESIAN_POINT ( 'NONE',  ( 10.49999999999992717, 3.431123077392147724, 4.000000000000000000 ) ) ;
#86302 = EDGE_LOOP ( 'NONE', ( #141675, #57199, #7700, #126172 ) ) ;
#86303 = CARTESIAN_POINT ( 'NONE',  ( -34.92500000000001137, -22.22500000000000142, 4.500000000000000888 ) ) ;
#86304 = AXIS2_PLACEMENT_3D ( 'NONE', #20721, #133099, #33781 ) ;
#86305 = FACE_OUTER_BOUND ( 'NONE', #99084, .T. ) ;
#86306 = EDGE_LOOP ( 'NONE', ( #136332, #59740, #127697 ) ) ;
#86309 = EDGE_CURVE ( 'NONE', #19139, #24144, #24235, .T. ) ;
#86308 = ORIENTED_EDGE ( 'NONE', *, *, #37997, .F. ) ;
#86307 = CARTESIAN_POINT ( 'NONE',  ( 0.8183591370940799248, -52.14999999999999147, -41.64500000000001023 ) ) ;
#86310 = ORIENTED_EDGE ( 'NONE', *, *, #126192, .F. ) ;
#86311 = DIRECTION ( 'NONE',  ( -0.000000000000000000, 0.3543493200069153248, 0.9351131265310292928 ) ) ;
#86312 = CARTESIAN_POINT ( 'NONE',  ( 25.00000000000000000, 0.000000000000000000, 0.000000000000000000 ) ) ;
#86313 = VERTEX_POINT ( 'NONE', #3171 ) ;
#86314 = CARTESIAN_POINT ( 'NONE',  ( 19.82816939922339117, -20.24070752338407431, 4.000000000000000000 ) ) ;
#86315 = CARTESIAN_POINT ( 'NONE',  ( 27.24999999999999645, -9.735942053221458872E-16, 7.950000000000000178 ) ) ;
#86316 = EDGE_CURVE ( 'NONE', #108968, #93841, #1711, .T. ) ;
#86317 = LINE ( 'NONE', #107329, #115513 ) ;
#86318 = LINE ( 'NONE', #32650, #60145 ) ;
#86319 = CARTESIAN_POINT ( 'NONE',  ( 16.17183060077636370, 18.75929247661553134, 4.000000000000000000 ) ) ;
#86320 = DIRECTION ( 'NONE',  ( -0.000000000000000000, -0.3543493200069152693, 0.9351131265310292928 ) ) ;
#86321 = VECTOR ( 'NONE', #72708, 1000.000000000000000 ) ;
#86322 = LINE ( 'NONE', #130542, #37952 ) ;
#86323 = CARTESIAN_POINT ( 'NONE',  ( 63.18398860626900415, 28.73617430169831621, 5.000000000000000000 ) ) ;
#86324 = CARTESIAN_POINT ( 'NONE',  ( 7.171830600776425868, -8.240707523384203981, 4.000000000000000000 ) ) ;
#86325 = CARTESIAN_POINT ( 'NONE',  ( -62.99451991528749772, 28.92564299267982264, 4.000000000000000000 ) ) ;
#86326 =( GEOMETRIC_REPRESENTATION_CONTEXT ( 3 ) GLOBAL_UNCERTAINTY_ASSIGNED_CONTEXT ( ( #94125 ) ) GLOBAL_UNIT_ASSIGNED_CONTEXT ( ( #78129, #57108, #54952 ) ) REPRESENTATION_CONTEXT ( 'NONE', 'WORKASPACE' ) );
#86327 = LINE ( 'NONE', #130546, #11234 ) ;
#86328 = FACE_OUTER_BOUND ( 'NONE', #24474, .T. ) ;
#86329 = EDGE_LOOP ( 'NONE', ( #128936, #107934, #56152, #117525 ) ) ;
#86330 = ADVANCED_FACE ( 'NONE', ( #80768 ), #135163, .F. ) ;
#86331 = ORIENTED_EDGE ( 'NONE', *, *, #134343, .T. ) ;
#86332 = ORIENTED_EDGE ( 'NONE', *, *, #87918, .F. ) ;
#86333 = CARTESIAN_POINT ( 'NONE',  ( 111.5416666666666572, -3.975000000000002753, 6.884901960086286188 ) ) ;
#86334 = EDGE_CURVE ( 'NONE', #18953, #52975, #70632, .T. ) ;
#86335 = ORIENTED_EDGE ( 'NONE', *, *, #48223, .T. ) ;
#86336 = ORIENTED_EDGE ( 'NONE', *, *, #103996, .T. ) ;
#86337 = ORIENTED_EDGE ( 'NONE', *, *, #45673, .T. ) ;
#86338 = PLANE ( 'NONE',  #59470 ) ;
#86339 = CARTESIAN_POINT ( 'NONE',  ( 19.49999999999986500, -4.912538124160707120, 4.000000000000000000 ) ) ;
#86340 = VECTOR ( 'NONE', #47724, 1000.000000000000000 ) ;
#86341 = ORIENTED_EDGE ( 'NONE', *, *, #137198, .F. ) ;
#86342 = LINE ( 'NONE', #130560, #120395 ) ;
#86343 = DIRECTION ( 'NONE',  ( 0.7071067811865487940, 0.7071067811865463515, 0.000000000000000000 ) ) ;
#86344 = DIRECTION ( 'NONE',  ( 1.000000000000000000, -0.000000000000000000, 0.000000000000000000 ) ) ;
#86345 = PLANE ( 'NONE',  #32752 ) ;
#86346 = CARTESIAN_POINT ( 'NONE',  ( 99.89626352523141861, 4.472830434245840259, -4.472830434245839371 ) ) ;
#86347 = ORIENTED_EDGE ( 'NONE', *, *, #93318, .F. ) ;
#86348 = ADVANCED_FACE ( 'NONE', ( #112660 ), #124958, .F. ) ;
#86349 = CARTESIAN_POINT ( 'NONE',  ( 8.763039537514666577, 10.25773029732260611, -28.68199181715783297 ) ) ;
#86351 = AXIS2_PLACEMENT_3D ( 'NONE', #60892, #128947, #118035 ) ;
#86350 = FACE_OUTER_BOUND ( 'NONE', #135228, .T. ) ;
#86352 = PLANE ( 'NONE',  #67888 ) ;
#86353 = CARTESIAN_POINT ( 'NONE',  ( 17.20710678118643244, 18.75929247661552068, 5.000000000000000000 ) ) ;
#86354 = DIRECTION ( 'NONE',  ( 0.6830127018922180770, -0.6830127018922204085, -0.2588190451025213501 ) ) ;
#86355 = LINE ( 'NONE', #8719, #98597 ) ;
#86356 = DIRECTION ( 'NONE',  ( -0.7071067811865487940, 0.7071067811865463515, -0.000000000000000000 ) ) ;
#86357 = CARTESIAN_POINT ( 'NONE',  ( 0.000000000000000000, 0.000000000000000000, 5.000000000000000000 ) ) ;
#86358 = ORIENTED_EDGE ( 'NONE', *, *, #56704, .F. ) ;
#86359 = ORIENTED_EDGE ( 'NONE', *, *, #122350, .F. ) ;
#86360 = CARTESIAN_POINT ( 'NONE',  ( 26.37499999999999645, 7.950000000000000178, 1.460391307983218535E-15 ) ) ;
#86361 = EDGE_LOOP ( 'NONE', ( #81320, #34341, #934, #15940 ) ) ;
#86362 = LINE ( 'NONE', #42151, #96913 ) ;
#86363 = DIRECTION ( 'NONE',  ( -0.7071067811865487940, 0.7071067811865463515, -0.000000000000000000 ) ) ;
#86364 = VECTOR ( 'NONE', #95730, 1000.000000000000000 ) ;
#86365 = CARTESIAN_POINT ( 'NONE',  ( 27.32816939922334143, -0.7407075233842683737, 4.000000000000000000 ) ) ;
#86366 = LINE ( 'NONE', #8049, #123321 ) ;
#86367 = VECTOR ( 'NONE', #38498, 1000.000000000000000 ) ;
#86368 = LINE ( 'NONE', #85615, #11881 ) ;
#86370 = VECTOR ( 'NONE', #64129, 1000.000000000000000 ) ;
#86369 = CARTESIAN_POINT ( 'NONE',  ( -10.11017322888203651, -22.22500000000000497, 4.785647885939354751 ) ) ;
#86371 = CARTESIAN_POINT ( 'NONE',  ( 126.7870968585647944, 3.054999999999997495, 5.291415217122919401 ) ) ;
#86372 = EDGE_LOOP ( 'NONE', ( #127756, #52509, #134821, #22955 ) ) ;
#86373 = FACE_OUTER_BOUND ( 'NONE', #15444, .T. ) ;
#86374 = ORIENTED_EDGE ( 'NONE', *, *, #128292, .T. ) ;
#86375 = VECTOR ( 'NONE', #62217, 1000.000000000000000 ) ;
#86376 = VECTOR ( 'NONE', #7316, 1000.000000000000227 ) ;
#86377 =( GEOMETRIC_REPRESENTATION_CONTEXT ( 3 ) GLOBAL_UNCERTAINTY_ASSIGNED_CONTEXT ( ( #83554 ) ) GLOBAL_UNIT_ASSIGNED_CONTEXT ( ( #20034, #43960, #75875 ) ) REPRESENTATION_CONTEXT ( 'NONE', 'WORKASPACE' ) );
#86378 = FACE_OUTER_BOUND ( 'NONE', #41579, .T. ) ;
#86379 = LINE ( 'NONE', #109537, #57035 ) ;
#86380 = CARTESIAN_POINT ( 'NONE',  ( 0.000000000000000000, 0.000000000000000000, 5.000000000000000000 ) ) ;
#86381 = ORIENTED_EDGE ( 'NONE', *, *, #101785, .F. ) ;
#86382 = CARTESIAN_POINT ( 'NONE',  ( 49.43793019189809002, -6.110000000000001208, 1.637169565754158951 ) ) ;
#86383 = ORIENTED_EDGE ( 'NONE', *, *, #112748, .T. ) ;
#86384 = DIRECTION ( 'NONE',  ( 0.7071067811865486830, -0.7071067811865464625, -0.000000000000000000 ) ) ;
#86385 = DIRECTION ( 'NONE',  ( -1.000000000000000000, 0.000000000000000000, 0.000000000000000000 ) ) ;
#86386 = PRESENTATION_STYLE_ASSIGNMENT (( #55179 ) ) ;
#86387 = EDGE_CURVE ( 'NONE', #23874, #116753, #114091, .T. ) ;
#86388 = AXIS2_PLACEMENT_3D ( 'NONE', #43685, #132143, #101624 ) ;
#86389 = CARTESIAN_POINT ( 'NONE',  ( 36.22459685856478728, -1.637169565754160949, 6.109999999999997655 ) ) ;
#86390 = EDGE_CURVE ( 'NONE', #101224, #79010, #57596, .T. ) ;
#86391 = ORIENTED_EDGE ( 'NONE', *, *, #68503, .T. ) ;
#86393 = EDGE_CURVE ( 'NONE', #6561, #93928, #37765, .T. ) ;
#86392 = DIRECTION ( 'NONE',  ( 0.000000000000000000, -1.000000000000000000, 0.000000000000000000 ) ) ;
#86394 = ORIENTED_EDGE ( 'NONE', *, *, #114991, .F. ) ;
#86395 = ORIENTED_EDGE ( 'NONE', *, *, #11552, .F. ) ;
#86396 = ORIENTED_EDGE ( 'NONE', *, *, #68805, .F. ) ;
#86397 = EDGE_CURVE ( 'NONE', #99826, #86478, #2443, .T. ) ;
#86398 = AXIS2_PLACEMENT_3D ( 'NONE', #109953, #132473, #86798 ) ;
#86399 = PRODUCT_DEFINITION_SHAPE ( 'NONE', 'NONE',  #143557 ) ;
#86400 = DIRECTION ( 'NONE',  ( 1.000000000000000000, -0.000000000000000000, -0.000000000000000000 ) ) ;
#86401 = ORIENTED_EDGE ( 'NONE', *, *, #6116, .F. ) ;
#86402 = VECTOR ( 'NONE', #125701, 1000.000000000000000 ) ;
#86403 = CARTESIAN_POINT ( 'NONE',  ( -9.183988606268997046, 28.73617430169793607, 5.000000000000000000 ) ) ;
#86404 = EDGE_CURVE ( 'NONE', #108193, #6023, #69175, .T. ) ;
#86405 = CARTESIAN_POINT ( 'NONE',  ( -17.67183060077635304, -9.740707523384180888, 4.000000000000000000 ) ) ;
#86406 = DIRECTION ( 'NONE',  ( -0.7071067811865486830, -0.7071067811865464625, 0.000000000000000000 ) ) ;
#86407 = EDGE_CURVE ( 'NONE', #116521, #26660, #122827, .T. ) ;
#86408 = FACE_BOUND ( 'NONE', #6365, .T. ) ;
#86409 = ORIENTED_EDGE ( 'NONE', *, *, #36977, .F. ) ;
#86410 = EDGE_CURVE ( 'NONE', #23670, #65156, #3849, .T. ) ;
#86411 = DIRECTION ( 'NONE',  ( 0.7071067811865487940, -0.7071067811865463515, 0.000000000000000000 ) ) ;
#86412 = CARTESIAN_POINT ( 'NONE',  ( 3.345840036506269488, -49.02495722182847260, 39.69341335395905190 ) ) ;
#86413 = VERTEX_POINT ( 'NONE', #92314 ) ;
#86414 = DIRECTION ( 'NONE',  ( -0.7071067811865486830, 0.7071067811865464625, 0.000000000000000000 ) ) ;
#86415 = ORIENTED_EDGE ( 'NONE', *, *, #62804, .T. ) ;
#86416 = ORIENTED_EDGE ( 'NONE', *, *, #83216, .F. ) ;
#86417 = CARTESIAN_POINT ( 'NONE',  ( -34.92500000000001137, -22.22500000000000142, 4.000000000000000000 ) ) ;
#86418 = EDGE_CURVE ( 'NONE', #41631, #61971, #81496, .T. ) ;
#86419 = ORIENTED_EDGE ( 'NONE', *, *, #111637, .T. ) ;
#86420 = AXIS2_PLACEMENT_3D ( 'NONE', #32643, #112336, #131958 ) ;
#86421 = CARTESIAN_POINT ( 'NONE',  ( 55.76626352523145158, 4.472830434245838482, -4.472830434245837594 ) ) ;
#86423 = ORIENTED_EDGE ( 'NONE', *, *, #62976, .F. ) ;
#86422 = AXIS2_PLACEMENT_3D ( 'NONE', #33010, #121393, #118539 ) ;
#86424 = CARTESIAN_POINT ( 'NONE',  ( -25.82816939922335209, -17.24070752338409918, 4.000000000000000000 ) ) ;
#86425 = LINE ( 'NONE', #11659, #3229 ) ;
#86426 = EDGE_LOOP ( 'NONE', ( #19288, #4943, #83, #110914 ) ) ;
#86427 = DIRECTION ( 'NONE',  ( 0.6830127018922180770, -0.6830127018922204085, -0.2588190451025213501 ) ) ;
#86428 = DIRECTION ( 'NONE',  ( -1.000000000000000000, -0.000000000000000000, -0.000000000000000000 ) ) ;
#86429 = VECTOR ( 'NONE', #40873, 1000.000000000000000 ) ;
#86430 =( BOUNDED_CURVE ( )  B_SPLINE_CURVE ( 3, ( #99724, #24317, #79465, #122919 ),
 .UNSPECIFIED., .F., .F. ) 
 B_SPLINE_CURVE_WITH_KNOTS ( ( 4, 4 ),
 ( 1.864375635226932282, 1.933014472006575613 ),
 .UNSPECIFIED. ) 
 CURVE ( )  GEOMETRIC_REPRESENTATION_ITEM ( )  RATIONAL_B_SPLINE_CURVE ( ( 1.000000000000000000, 0.9996074310407760954, 0.9996074310407760954, 1.000000000000000000 ) ) 
 REPRESENTATION_ITEM ( '' )  );
#86431 = CARTESIAN_POINT ( 'NONE',  ( -0.1839886062690032631, 28.73617430169787568, 5.000000000000000000 ) ) ;
#86432 = DIRECTION ( 'NONE',  ( -1.000000000000000000, -0.000000000000000000, -0.000000000000000000 ) ) ;
#86433 = DIRECTION ( 'NONE',  ( -0.3543493200069162685, -0.000000000000000000, -0.9351131265310288487 ) ) ;
#86434 = LINE ( 'NONE', #19719, #9320 ) ;
#86435 = ORIENTED_EDGE ( 'NONE', *, *, #114929, .F. ) ;
#86436 = EDGE_CURVE ( 'NONE', #119557, #50386, #37247, .T. ) ;
#86438 = VERTEX_POINT ( 'NONE', #103896 ) ;
#86437 = VECTOR ( 'NONE', #59585, 1000.000000000000000 ) ;
#86439 = ORIENTED_EDGE ( 'NONE', *, *, #52929, .F. ) ;
#86440 = DIRECTION ( 'NONE',  ( 0.7071067811865487940, -0.7071067811865463515, 0.000000000000000000 ) ) ;
#86441 = ORIENTED_EDGE ( 'NONE', *, *, #75603, .F. ) ;
#86442 = ORIENTED_EDGE ( 'NONE', *, *, #36590, .T. ) ;
#86443 = VERTEX_POINT ( 'NONE', #4543 ) ;
#86444 = CARTESIAN_POINT ( 'NONE',  ( 4.998069433178977228, -22.22500000000000142, 4.500000000000000888 ) ) ;
#86445 = PLANE ( 'NONE',  #10841 ) ;
#86446 = LINE ( 'NONE', #85694, #74058 ) ;
#86447 = AXIS2_PLACEMENT_3D ( 'NONE', #55521, #143228, #107728 ) ;
#86448 = ORIENTED_EDGE ( 'NONE', *, *, #86501, .T. ) ;
#86449 = CARTESIAN_POINT ( 'NONE',  ( -1.179999999999998606, -6.391994993740215847, 10.00000000000000000 ) ) ;
#86450 = EDGE_CURVE ( 'NONE', #120495, #135320, #48852, .T. ) ;
#86451 = DIRECTION ( 'NONE',  ( 0.000000000000000000, 0.000000000000000000, 1.000000000000000000 ) ) ;
#86452 = CARTESIAN_POINT ( 'NONE',  ( 13.92123647476855197, -9.717572351234235426E-16, -7.934999999999990727 ) ) ;
#86453 = CARTESIAN_POINT ( 'NONE',  ( 2.999999999999975131, 7.007997736742450634, -8.085015511992105885 ) ) ;
#86454 = VERTEX_POINT ( 'NONE', #67780 ) ;
#86455 = CARTESIAN_POINT ( 'NONE',  ( 121.3912635252314374, -4.472830434245839371, -4.472830434245839371 ) ) ;
#86457 = EDGE_CURVE ( 'NONE', #103754, #73407, #12623, .T. ) ;
#86456 = FACE_OUTER_BOUND ( 'NONE', #113049, .T. ) ;
#86458 = LINE ( 'NONE', #95881, #139911 ) ;
#86459 = VECTOR ( 'NONE', #139813, 1000.000000000000000 ) ;
#86461 = ORIENTED_EDGE ( 'NONE', *, *, #82591, .T. ) ;
#86460 = DIRECTION ( 'NONE',  ( 0.7071067811865487940, 0.7071067811865463515, -0.000000000000000000 ) ) ;
#86462 = CARTESIAN_POINT ( 'NONE',  ( 68.03752705046289861, -9.735942053221456900E-16, 7.949999999999998401 ) ) ;
#86463 = ORIENTED_EDGE ( 'NONE', *, *, #96361, .T. ) ;
#86464 = CARTESIAN_POINT ( 'NONE',  ( -22.49999999999984368, -1.695981523266240076, 4.571483868317929300 ) ) ;
#86465 = CARTESIAN_POINT ( 'NONE',  ( -21.18398860626899349, 28.73617430169802134, 5.000000000000000000 ) ) ;
#86466 = LINE ( 'NONE', #97280, #86605 ) ;
#86467 = ORIENTED_EDGE ( 'NONE', *, *, #114378, .T. ) ;
#86468 = EDGE_CURVE ( 'NONE', #31906, #141911, #40819, .T. ) ;
#86469 = LINE ( 'NONE', #142284, #60415 ) ;
#86470 = DIRECTION ( 'NONE',  ( -0.5735764363510499342, -0.8191520442889891340, 0.000000000000000000 ) ) ;
#86471 = AXIS2_PLACEMENT_3D ( 'NONE', #108793, #31981, #8063 ) ;
#86472 = VERTEX_POINT ( 'NONE', #106033 ) ;
#86473 = CARTESIAN_POINT ( 'NONE',  ( -3.328169399223498637, -3.740707523384246613, 4.000000000000000000 ) ) ;
#86474 = CARTESIAN_POINT ( 'NONE',  ( -2.999999999999981792, -0.8619312979532001151, -5.102805207349832450 ) ) ;
#86475 = EDGE_LOOP ( 'NONE', ( #62531, #23018, #35138, #120675, #116770, #133500, #73180, #13068 ) ) ;
#86476 = CARTESIAN_POINT ( 'NONE',  ( 5.104166666666668739, -1.633150327867687102, -6.094999999999992646 ) ) ;
#86477 = CARTESIAN_POINT ( 'NONE',  ( 18.29974487139159223, -27.71228299555219010, 4.000000000000000000 ) ) ;
#86479 = ADVANCED_FACE ( 'NONE', ( #117618 ), #39403, .F. ) ;
#86478 = VERTEX_POINT ( 'NONE', #5302 ) ;
#86480 = ORIENTED_EDGE ( 'NONE', *, *, #126945, .T. ) ;
#86481 = DIRECTION ( 'NONE',  ( -0.7071067811865487940, 0.7071067811865463515, -0.000000000000000000 ) ) ;
#86482 = DIRECTION ( 'NONE',  ( 1.000000000000000000, 0.000000000000000000, 0.000000000000000000 ) ) ;
#86483 = VECTOR ( 'NONE', #10247, 999.9999999999998863 ) ;
#86484 = CARTESIAN_POINT ( 'NONE',  ( 9.895403141435220817, 2.126176841940962348, 7.934999999999989839 ) ) ;
#86485 = CARTESIAN_POINT ( 'NONE',  ( 13.49999999999990408, -19.91253812416055879, 4.000000000000000000 ) ) ;
#86486 = VECTOR ( 'NONE', #118751, 1000.000000000000227 ) ;
#86487 = PLANE ( 'NONE',  #124674 ) ;
#86488 = LINE ( 'NONE', #95194, #58362 ) ;
#86489 = ORIENTED_EDGE ( 'NONE', *, *, #83638, .T. ) ;
#86490 = CYLINDRICAL_SURFACE ( 'NONE', #16415, 2.552699999999959779 ) ;
#86491 = CARTESIAN_POINT ( 'NONE',  ( 31.17183060077625356, 18.75929247661552068, 4.000000000000000000 ) ) ;
#86492 = CARTESIAN_POINT ( 'NONE',  ( 5.733306282870439752, -6.094999999999989981, -1.633150327867689322 ) ) ;
#86493 = SURFACE_STYLE_FILL_AREA ( #55292 ) ;
#86494 = CARTESIAN_POINT ( 'NONE',  ( 34.32876352523143737, 0.000000000000000000, -6.109999999999999432 ) ) ;
#86495 = VECTOR ( 'NONE', #98384, 999.9999999999998863 ) ;
#86496 = CARTESIAN_POINT ( 'NONE',  ( -31.49999999999977973, -11.94781430457070392, 5.000000000000000000 ) ) ;
#86497 = EDGE_CURVE ( 'NONE', #110441, #91654, #51707, .T. ) ;
#86498 = VERTEX_POINT ( 'NONE', #61193 ) ;
#86499 = VERTEX_POINT ( 'NONE', #49584 ) ;
#86500 = CARTESIAN_POINT ( 'NONE',  ( 75.18398860626899705, 28.73617430169839793, 5.000000000000000000 ) ) ;
#86501 = EDGE_CURVE ( 'NONE', #123401, #72522, #82906, .T. ) ;
#86502 = AXIS2_PLACEMENT_3D ( 'NONE', #121375, #54024, #11153 ) ;
#86503 = ORIENTED_EDGE ( 'NONE', *, *, #125721, .F. ) ;
#86504 = ORIENTED_EDGE ( 'NONE', *, *, #19150, .F. ) ;
#86505 = CARTESIAN_POINT ( 'NONE',  ( 20.20519093902540320, 4.584330080086930965E-16, 0.000000000000000000 ) ) ;
#86506 = CARTESIAN_POINT ( 'NONE',  ( 32.27718569542918203, -21.72500000000000142, 5.000000000000000000 ) ) ;
#86507 = VERTEX_POINT ( 'NONE', #105344 ) ;
#86509 = VECTOR ( 'NONE', #37982, 1000.000000000000000 ) ;
#86508 = CARTESIAN_POINT ( 'NONE',  ( -19.05000000000000071, 3.174999999999997158, 5.000000000000000000 ) ) ;
#86510 = CARTESIAN_POINT ( 'NONE',  ( 29.20710678118634007, 0.7592924766157052030, 5.000000000000000000 ) ) ;
#86511 = EDGE_CURVE ( 'NONE', #11859, #80263, #94463, .T. ) ;
#86512 = FACE_OUTER_BOUND ( 'NONE', #59202, .T. ) ;
#86513 = DIRECTION ( 'NONE',  ( 0.7071067811865487940, 0.7071067811865463515, 0.000000000000000000 ) ) ;
#86514 = ORIENTED_EDGE ( 'NONE', *, *, #117840, .F. ) ;
#86515 = EDGE_CURVE ( 'NONE', #63026, #56797, #95179, .T. ) ;
#86516 = LINE ( 'NONE', #9623, #141332 ) ;
#86517 = DIRECTION ( 'NONE',  ( 0.000000000000000000, -1.301042606982605074E-16, 1.000000000000000000 ) ) ;
#86518 = DIRECTION ( 'NONE',  ( -0.7071067811865486830, -0.7071067811865464625, 0.000000000000000000 ) ) ;
#86519 = LINE ( 'NONE', #110365, #50358 ) ;
#86520 = CARTESIAN_POINT ( 'NONE',  ( 5.999999999999961808, -3.033600742197710254, 5.000000000000000000 ) ) ;
#86521 = CARTESIAN_POINT ( 'NONE',  ( -22.49999999999983302, -1.912538124160733766, 4.000000000000000000 ) ) ;
#86522 = VECTOR ( 'NONE', #10430, 1000.000000000000114 ) ;
#86523 = CARTESIAN_POINT ( 'NONE',  ( 57.10002705046289861, 5.819803920172570422, 5.819803920172574863 ) ) ;
#86524 = AXIS2_PLACEMENT_3D ( 'NONE', #63105, #74687, #40618 ) ;
#86525 = CARTESIAN_POINT ( 'NONE',  ( -20.01844734635657730, 18.75929247661551713, 20.33588619593447433 ) ) ;
#86526 = ORIENTED_EDGE ( 'NONE', *, *, #50816, .F. ) ;
#86527 = ORIENTED_EDGE ( 'NONE', *, *, #109942, .T. ) ;
#86528 = CARTESIAN_POINT ( 'NONE',  ( 57.58333333333333570, 6.884901960086290629, -3.974999999999994316 ) ) ;
#86529 = CARTESIAN_POINT ( 'NONE',  ( -57.18398860626899705, 28.73617430169827358, 5.000000000000000000 ) ) ;
#86530 = DIRECTION ( 'NONE',  ( -0.000000000000000000, -0.3543493200069152693, 0.9351131265310292928 ) ) ;
#86531 = CIRCLE ( 'NONE', #56457, 3.000000000000000000 ) ;
#86532 = CARTESIAN_POINT ( 'NONE',  ( 61.46640106136302961, -57.15000000000009805, -40.92499999999998295 ) ) ;
#86533 = ORIENTED_EDGE ( 'NONE', *, *, #25842, .T. ) ;
#86534 = DIRECTION ( 'NONE',  ( 0.7071067811865487940, -0.7071067811865463515, 0.000000000000000000 ) ) ;
#86535 = ADVANCED_FACE ( 'NONE', ( #16923 ), #84350, .F. ) ;
#86536 = LINE ( 'NONE', #98115, #79371 ) ;
#86537 = CARTESIAN_POINT ( 'NONE',  ( 46.37543019189810423, -5.291415217122920289, -3.055000000000001492 ) ) ;
#86538 = EDGE_LOOP ( 'NONE', ( #68551, #130607, #113881, #71854 ) ) ;
#86539 = DIRECTION ( 'NONE',  ( 0.000000000000000000, -1.000000000000000000, 0.000000000000000000 ) ) ;
#86540 = EDGE_LOOP ( 'NONE', ( #76312, #22833, #809, #22220 ) ) ;
#86541 = ORIENTED_EDGE ( 'NONE', *, *, #22522, .F. ) ;
#86542 = AXIS2_PLACEMENT_3D ( 'NONE', #64890, #22060, #75068 ) ;
#86543 = CARTESIAN_POINT ( 'NONE',  ( 24.41159235450331977, 9.902892378096218942E-16, 0.000000000000000000 ) ) ;
#86544 = DIRECTION ( 'NONE',  ( -1.000000000000000000, 0.000000000000000000, 0.000000000000000000 ) ) ;
#86545 = LINE ( 'NONE', #53932, #30385 ) ;
#86546 = LINE ( 'NONE', #77116, #101908 ) ;
#86547 = EDGE_LOOP ( 'NONE', ( #143433, #18571, #45385, #34596, #115568 ) ) ;
#86548 = DIRECTION ( 'NONE',  ( 0.7071067811865486830, -0.7071067811865464625, -0.000000000000000000 ) ) ;
#86550 = ORIENTED_EDGE ( 'NONE', *, *, #82617, .T. ) ;
#86549 = FACE_OUTER_BOUND ( 'NONE', #72148, .T. ) ;
#86551 = CARTESIAN_POINT ( 'NONE',  ( 85.60459685856477563, 1.637169565754164946, -6.109999999999999432 ) ) ;
#86552 = DIRECTION ( 'NONE',  ( -0.7071067811865487940, 0.7071067811865463515, 0.000000000000000000 ) ) ;
#86553 = CARTESIAN_POINT ( 'NONE',  ( -51.18398860626899705, 28.73617430169823095, 5.000000000000000000 ) ) ;
#86554 = LINE ( 'NONE', #75672, #116332 ) ;
#86555 = CARTESIAN_POINT ( 'NONE',  ( 10.49999999999992895, -20.56887692260759337, 4.000000000000000000 ) ) ;
#86556 = DIRECTION ( 'NONE',  ( -1.000000000000000000, 2.775557561562888827E-14, 0.000000000000000000 ) ) ;
#86557 = EDGE_CURVE ( 'NONE', #20222, #57263, #38676, .T. ) ;
#86558 = EDGE_LOOP ( 'NONE', ( #121578, #112913, #9392, #41076 ) ) ;
#86559 = VECTOR ( 'NONE', #82502, 1000.000000000000000 ) ;
#86560 = DIRECTION ( 'NONE',  ( 0.000000000000000000, -1.000000000000000000, 0.000000000000000000 ) ) ;
#86561 = CARTESIAN_POINT ( 'NONE',  ( 71.95376352523145158, -6.109999999999998543, -3.741295971395162543E-16 ) ) ;
#86562 = EDGE_CURVE ( 'NONE', #111382, #124741, #83636, .T. ) ;
#86563 = LINE ( 'NONE', #109721, #101978 ) ;
#86564 = LINE ( 'NONE', #139540, #22297 ) ;
#86565 = PLANE ( 'NONE',  #108075 ) ;
#86566 = ORIENTED_EDGE ( 'NONE', *, *, #64445, .F. ) ;
#86567 = VERTEX_POINT ( 'NONE', #82212 ) ;
#86568 = DIRECTION ( 'NONE',  ( -0.3543493200069162685, -0.000000000000000000, -0.9351131265310288487 ) ) ;
#86569 = FILL_AREA_STYLE_COLOUR ( '', #74579 ) ;
#86570 = VERTEX_POINT ( 'NONE', #104634 ) ;
#86571 = EDGE_CURVE ( 'NONE', #115190, #28781, #17607, .T. ) ;
#86572 = ADVANCED_FACE ( 'NONE', ( #93768 ), #67909, .T. ) ;
#86573 = VECTOR ( 'NONE', #133334, 1000.000000000000000 ) ;
#86574 = EDGE_LOOP ( 'NONE', ( #72020, #20104, #93982, #105977 ) ) ;
#86575 = DIRECTION ( 'NONE',  ( -0.000000000000000000, -0.000000000000000000, 1.000000000000000000 ) ) ;
#86576 = VERTEX_POINT ( 'NONE', #85021 ) ;
#86577 = CARTESIAN_POINT ( 'NONE',  ( -17.78795468754224629, 22.22500000000000142, -1.493867085284279028 ) ) ;
#86578 = CARTESIAN_POINT ( 'NONE',  ( 6.005480084712508493, 28.92564299267933947, 4.000000000000000000 ) ) ;
#86579 = CARTESIAN_POINT ( 'NONE',  ( -16.49999999999988276, 15.43112307739202471, 4.000000000000000000 ) ) ;
#86580 = EDGE_CURVE ( 'NONE', #74550, #116562, #29211, .T. ) ;
#86581 = FACE_BOUND ( 'NONE', #585, .T. ) ;
#86582 = EDGE_CURVE ( 'NONE', #75761, #83246, #27071, .T. ) ;
#86583 =( NAMED_UNIT ( * ) PLANE_ANGLE_UNIT ( ) SI_UNIT ( $, .RADIAN. ) );
#86584 = PLANE ( 'NONE',  #67542 ) ;
#86585 = CARTESIAN_POINT ( 'NONE',  ( 11.81601139373100651, 28.73617430169779041, 5.000000000000000000 ) ) ;
#86587 = ORIENTED_EDGE ( 'NONE', *, *, #67699, .F. ) ;
#86586 = DIRECTION ( 'NONE',  ( -0.000000000000000000, -0.3543493200069152693, 0.9351131265310292928 ) ) ;
#86588 = AXIS2_PLACEMENT_3D ( 'NONE', #70059, #91748, #36652 ) ;
#86589 = LINE ( 'NONE', #75705, #18491 ) ;
#86590 = EDGE_CURVE ( 'NONE', #117979, #46897, #16165, .T. ) ;
#86591 = VERTEX_POINT ( 'NONE', #25381 ) ;
#86592 = VECTOR ( 'NONE', #24107, 1000.000000000000000 ) ;
#86593 = ORIENTED_EDGE ( 'NONE', *, *, #47471, .F. ) ;
#86594 = CARTESIAN_POINT ( 'NONE',  ( 80.99543019189810877, 5.291415217122916737, 3.055000000000001936 ) ) ;
#86595 = ORIENTED_EDGE ( 'NONE', *, *, #41759, .F. ) ;
#86596 = FACE_OUTER_BOUND ( 'NONE', #135591, .T. ) ;
#86597 = DIRECTION ( 'NONE',  ( 0.7071067811865487940, 0.7071067811865463515, -0.000000000000000000 ) ) ;
#86598 = ORIENTED_EDGE ( 'NONE', *, *, #10111, .F. ) ;
#86599 = CARTESIAN_POINT ( 'NONE',  ( -23.36654548503486950, 7.297668562427137573, 4.000000000000000000 ) ) ;
#86600 = EDGE_CURVE ( 'NONE', #123534, #84565, #102273, .T. ) ;
#86601 = AXIS2_PLACEMENT_3D ( 'NONE', #140800, #55250, #52375 ) ;
#86602 = DIRECTION ( 'NONE',  ( -0.7071067811865486830, 0.7071067811865464625, 0.000000000000000000 ) ) ;
#86603 = LINE ( 'NONE', #131520, #76129 ) ;
#86604 = DIRECTION ( 'NONE',  ( 0.7071067811865487940, 0.7071067811865463515, -0.000000000000000000 ) ) ;
#86605 = VECTOR ( 'NONE', #142280, 999.9999999999998863 ) ;
#86606 = CARTESIAN_POINT ( 'NONE',  ( -9.489213562373095101, -27.52281430457062328, 5.000000000000000000 ) ) ;
#86607 = LINE ( 'NONE', #31499, #137274 ) ;
#86608 = CARTESIAN_POINT ( 'NONE',  ( 4.499999999999976019, -20.94781430457061333, 5.000000000000000000 ) ) ;
#86609 = ORIENTED_EDGE ( 'NONE', *, *, #4997, .F. ) ;
#86610 = EDGE_CURVE ( 'NONE', #52838, #13117, #36288, .T. ) ;
#86611 = DIRECTION ( 'NONE',  ( -0.6830127018922180770, -0.6830127018922204085, -0.2588190451025213501 ) ) ;
#86612 = VERTEX_POINT ( 'NONE', #38427 ) ;
#86613 = CARTESIAN_POINT ( 'NONE',  ( 123.7458603837962272, 3.974999999999996980, 6.884901960086287964 ) ) ;
#86614 = DIRECTION ( 'NONE',  ( 0.7071067811865486830, -0.7071067811865464625, -0.000000000000000000 ) ) ;
#86615 = AXIS2_PLACEMENT_3D ( 'NONE', #9589, #108175, #8840 ) ;
#86616 = ORIENTED_EDGE ( 'NONE', *, *, #24406, .F. ) ;
#86617 = VERTEX_POINT ( 'NONE', #2173 ) ;
#86618 = AXIS2_PLACEMENT_3D ( 'NONE', #114598, #3672, #135667 ) ;
#86619 = ORIENTED_EDGE ( 'NONE', *, *, #95368, .F. ) ;
#86620 = EDGE_CURVE ( 'NONE', #2255, #138900, #92069, .T. ) ;
#86621 = CARTESIAN_POINT ( 'NONE',  ( 37.33376352523143282, 6.110000000000001208, 1.122388791418549305E-15 ) ) ;
#86622 = ORIENTED_EDGE ( 'NONE', *, *, #13326, .T. ) ;
#86623 = CARTESIAN_POINT ( 'NONE',  ( 0.000000000000000000, 0.000000000000000000, 5.000000000000000000 ) ) ;
#86624 =( BOUNDED_CURVE ( )  B_SPLINE_CURVE ( 2, ( #130167, #33722, #110510, #67046, #1036, #125535, #47987, #64911, #56909, #77236, #101080, #92155, #111231 ),
 .UNSPECIFIED., .F., .T. ) 
 B_SPLINE_CURVE_WITH_KNOTS ( ( 3, 2, 2, 2, 2, 2, 3 ),
 ( 0.1333333333333333037, 0.1361111111111110716, 0.1388888888888888673, 0.1416666666666666630, 0.1444444444444444309, 0.1472222222222222265, 0.1499999999999999944 ),
 .UNSPECIFIED. ) 
 CURVE ( )  GEOMETRIC_REPRESENTATION_ITEM ( )  RATIONAL_B_SPLINE_CURVE ( ( 1.000000000000000444, 0.9659258262890679791, 1.000000000000000000, 0.9659258262890683122, 1.000000000000000000, 0.9659258262890683122, 1.000000000000000000, 0.9659258262890683122, 1.000000000000000000, 0.9659258262890683122, 1.000000000000000000, 0.9659258262890683122, 1.000000000000000000 ) ) 
 REPRESENTATION_ITEM ( '' )  );
#86625 = AXIS2_PLACEMENT_3D ( 'NONE', #3802, #52170, #107257 ) ;
#86626 = ADVANCED_FACE ( 'NONE', ( #58806 ), #104369, .F. ) ;
#86627 = PLANE ( 'NONE',  #132648 ) ;
#86628 = VECTOR ( 'NONE', #104625, 1000.000000000000000 ) ;
#86629 = CARTESIAN_POINT ( 'NONE',  ( 29.50413961620377279, -3.047499999999994547, 5.278424836066145431 ) ) ;
#86630 = CARTESIAN_POINT ( 'NONE',  ( 7.528865486064717061, 10.89722440034706885, -26.40697315731449990 ) ) ;
#86631 = VERTEX_POINT ( 'NONE', #49330 ) ;
#86632 = DIRECTION ( 'NONE',  ( 1.000000000000000000, 0.000000000000000000, 0.000000000000000000 ) ) ;
#86633 = ORIENTED_EDGE ( 'NONE', *, *, #125074, .T. ) ;
#86634 = FACE_OUTER_BOUND ( 'NONE', #78401, .T. ) ;
#86636 = ORIENTED_EDGE ( 'NONE', *, *, #126985, .F. ) ;
#86635 = LINE ( 'NONE', #32236, #141977 ) ;
#86637 = ORIENTED_EDGE ( 'NONE', *, *, #2060, .F. ) ;
#86638 = PLANE ( 'NONE',  #139924 ) ;
#86639 = CARTESIAN_POINT ( 'NONE',  ( -24.27121408575940009, 22.22500000000000142, 9.037117742336768345 ) ) ;
#86640 = CARTESIAN_POINT ( 'NONE',  ( 11.29320749275918701, 20.25929247661551358, 20.83292124670812129 ) ) ;
#86641 = ORIENTED_EDGE ( 'NONE', *, *, #34298, .T. ) ;
#86642 = CARTESIAN_POINT ( 'NONE',  ( 108.4333603837962272, 2.130196079827431532, -7.949999999999996625 ) ) ;
#86643 = VERTEX_POINT ( 'NONE', #4286 ) ;
#86644 = VERTEX_POINT ( 'NONE', #113832 ) ;
#86645 = VERTEX_POINT ( 'NONE', #37725 ) ;
#86646 = ADVANCED_FACE ( 'NONE', ( #80519 ), #115218, .F. ) ;
#86647 = CARTESIAN_POINT ( 'NONE',  ( -33.18398860626899705, 28.73617430169810305, 5.000000000000000000 ) ) ;
#86648 = CIRCLE ( 'NONE', #70431, 2.055000000000000604 ) ;
#86649 = CARTESIAN_POINT ( 'NONE',  ( 15.98840764549667703, 3.061616997868380183E-16, -2.500000000000001332 ) ) ;
#86650 = DIRECTION ( 'NONE',  ( -0.3543493200069162685, -0.000000000000000000, -0.9351131265310288487 ) ) ;
#86651 = LINE ( 'NONE', #43141, #777 ) ;
#86652 = CARTESIAN_POINT ( 'NONE',  ( -34.92500000000001847, 19.80009451602700210, 4.759050581649337808 ) ) ;
#86654 = ADVANCED_FACE ( 'NONE', ( #48584 ), #135602, .F. ) ;
#86653 = ORIENTED_EDGE ( 'NONE', *, *, #24956, .T. ) ;
#86655 = CARTESIAN_POINT ( 'NONE',  ( -39.70679250724050746, 20.25929247661551358, 20.83292124670823853 ) ) ;
#86656 = VERTEX_POINT ( 'NONE', #79835 ) ;
#86657 = DIRECTION ( 'NONE',  ( -1.000000000000000000, -0.000000000000000000, -0.000000000000000000 ) ) ;
#86658 = DIRECTION ( 'NONE',  ( 0.6830127018922181881, 0.6830127018922202975, -0.2588190451025214056 ) ) ;
#86659 = EDGE_LOOP ( 'NONE', ( #90730, #81644, #11336, #94021 ) ) ;
#86660 = CARTESIAN_POINT ( 'NONE',  ( 36.45983838949717892, 18.75929247661552779, 8.305906642995569911 ) ) ;
#86661 = CYLINDRICAL_SURFACE ( 'NONE', #46874, 34.92999999999999261 ) ;
#86662 = EDGE_LOOP ( 'NONE', ( #130242, #80005, #92263, #112956, #118517 ) ) ;
#86663 = ORIENTED_EDGE ( 'NONE', *, *, #99609, .T. ) ;
#86664 = LINE ( 'NONE', #19945, #139086 ) ;
#86665 = CARTESIAN_POINT ( 'NONE',  ( 122.6835989386367771, -57.15000000000009805, -40.92499999999998295 ) ) ;
#86666 = DIRECTION ( 'NONE',  ( -0.7071067811865486830, -0.7071067811865464625, -0.000000000000000000 ) ) ;
#86667 = CARTESIAN_POINT ( 'NONE',  ( 53.20833333333332860, -3.974999999999999201, -6.884901960086287964 ) ) ;
#86668 = FACE_OUTER_BOUND ( 'NONE', #2813, .T. ) ;
#86669 = CARTESIAN_POINT ( 'NONE',  ( 67.87043019189812298, -3.055000000000001936, 5.291415217122918513 ) ) ;
#86670 = LINE ( 'NONE', #64916, #32602 ) ;
#86671 = LINE ( 'NONE', #51903, #111000 ) ;
#86672 = CARTESIAN_POINT ( 'NONE',  ( 15.18398860626900237, 28.73617430169797871, 5.000000000000000000 ) ) ;
#86673 = CARTESIAN_POINT ( 'NONE',  ( 2.999999999999976463, 15.45873954670185846, -0.03131636524294698076 ) ) ;
#86674 = ADVANCED_FACE ( 'NONE', ( #15209 ), #46493, .F. ) ;
#86675 = VERTEX_POINT ( 'NONE', #134915 ) ;
#86676 = CARTESIAN_POINT ( 'NONE',  ( -27.48921356237309155, -27.52281430457074762, 5.000000000000000000 ) ) ;
#86677 = ORIENTED_EDGE ( 'NONE', *, *, #122579, .T. ) ;
#86678 = CARTESIAN_POINT ( 'NONE',  ( 122.6835989386367345, -43.14999999999999147, 34.92499999999998295 ) ) ;
#86679 = LINE ( 'NONE', #63520, #100884 ) ;
#86680 = EDGE_LOOP ( 'NONE', ( #64763, #36770, #138030, #86337 ) ) ;
#86681 = DIRECTION ( 'NONE',  ( -8.817971600062199903E-18, 0.3543493200069153248, 0.9351131265310292928 ) ) ;
#86683 = EDGE_LOOP ( 'NONE', ( #107102, #4155, #74688, #23675 ) ) ;
#86682 = LINE ( 'NONE', #119967, #11826 ) ;
#86684 = FACE_OUTER_BOUND ( 'NONE', #9943, .T. ) ;
#86685 = EDGE_CURVE ( 'NONE', #52354, #12991, #114211, .T. ) ;
#86686 = DIRECTION ( 'NONE',  ( 0.7071067811865487940, 0.7071067811865463515, 0.000000000000000000 ) ) ;
#86687 = CARTESIAN_POINT ( 'NONE',  ( -5.510786437626906675, -27.52281430457051314, 5.000000000000000000 ) ) ;
#86688 = ORIENTED_EDGE ( 'NONE', *, *, #56425, .T. ) ;
#86689 = ADVANCED_FACE ( 'NONE', ( #59487 ), #93515, .F. ) ;
#86690 = ORIENTED_EDGE ( 'NONE', *, *, #104586, .T. ) ;
#86691 = LINE ( 'NONE', #31588, #62608 ) ;
#86692 = CARTESIAN_POINT ( 'NONE',  ( -30.18398860626900060, 28.73617430169808173, 5.000000000000000000 ) ) ;
#86693 = VECTOR ( 'NONE', #134398, 1000.000000000000000 ) ;
#86694 = DIRECTION ( 'NONE',  ( 0.000000000000000000, 0.000000000000000000, 1.000000000000000000 ) ) ;
#86695 = DIRECTION ( 'NONE',  ( -0.000000000000000000, 1.137193330093850868E-16, -1.000000000000000000 ) ) ;
#86696 = CARTESIAN_POINT ( 'NONE',  ( 82.76669371712952739, -7.949999999999999289, 2.130196079827424427 ) ) ;
#86697 = LINE ( 'NONE', #139668, #41665 ) ;
#86698 = VECTOR ( 'NONE', #134869, 1000.000000000000000 ) ;
#86699 = PLANE ( 'NONE',  #87746 ) ;
#86700 = ORIENTED_EDGE ( 'NONE', *, *, #92613, .F. ) ;
#86701 = ADVANCED_FACE ( 'NONE', ( #124011 ), #2922, .T. ) ;
#86702 = FACE_OUTER_BOUND ( 'NONE', #139699, .T. ) ;
#86703 = AXIS2_PLACEMENT_3D ( 'NONE', #99490, #56053, #90056 ) ;
#86704 = DIRECTION ( 'NONE',  ( -3.071323233543530392E-32, 2.242629915582283412E-16, -1.000000000000000000 ) ) ;
#86705 = CARTESIAN_POINT ( 'NONE',  ( 13.79551713769220811, 6.008391563887172993, 4.335713449946892339 ) ) ;
#86706 = ORIENTED_EDGE ( 'NONE', *, *, #16527, .T. ) ;
#86707 = EDGE_CURVE ( 'NONE', #71142, #22022, #36978, .T. ) ;
#86708 = CARTESIAN_POINT ( 'NONE',  ( -51.18398860626899705, 28.73617430169823095, 5.000000000000000000 ) ) ;
#86709 = ORIENTED_EDGE ( 'NONE', *, *, #79307, .F. ) ;
#86710 = VECTOR ( 'NONE', #121738, 1000.000000000000000 ) ;
#86711 = CARTESIAN_POINT ( 'NONE',  ( 74.08376352523143282, -6.110000000000001208, -3.741295971395164515E-16 ) ) ;
#86712 = CARTESIAN_POINT ( 'NONE',  ( -66.48921356237309510, -27.52281430457101763, 5.000000000000000000 ) ) ;
#86713 = CARTESIAN_POINT ( 'NONE',  ( 6.489213562373093325, -27.52281430457059841, 5.000000000000000000 ) ) ;
#86714 = EDGE_LOOP ( 'NONE', ( #93512, #11273, #32901, #111223 ) ) ;
#86715 = ADVANCED_FACE ( 'NONE', ( #57348 ), #101523, .F. ) ;
#86716 = CARTESIAN_POINT ( 'NONE',  ( 7.499999999999952927, -4.912538124160708897, 4.000000000000000000 ) ) ;
#86717 = LINE ( 'NONE', #75835, #53460 ) ;
#86718 = LINE ( 'NONE', #87427, #37135 ) ;
#86719 = DIRECTION ( 'NONE',  ( -0.7071067811865487940, 0.7071067811865463515, 0.000000000000000000 ) ) ;
#86721 = ORIENTED_EDGE ( 'NONE', *, *, #128418, .T. ) ;
#86720 = DIRECTION ( 'NONE',  ( -0.6830127018922180770, 0.6830127018922202975, -0.2588190451025213501 ) ) ;
#86722 = CARTESIAN_POINT ( 'NONE',  ( 2.999999999999999112, 0.000000000000000000, -4.750000000000000000 ) ) ;
#86723 = CARTESIAN_POINT ( 'NONE',  ( 76.39583333333332860, -2.130196079827427091, 7.949999999999998401 ) ) ;
#86724 = DIRECTION ( 'NONE',  ( -1.000000000000000000, 0.000000000000000000, 0.000000000000000000 ) ) ;
#86725 = VECTOR ( 'NONE', #127635, 1000.000000000000000 ) ;
#86726 = ORIENTED_EDGE ( 'NONE', *, *, #70071, .T. ) ;
#86727 = ORIENTED_EDGE ( 'NONE', *, *, #131427, .T. ) ;
#86728 = CARTESIAN_POINT ( 'NONE',  ( 67.22959685856476142, -6.110000000000000320, -1.637169565754161393 ) ) ;
#86729 = VECTOR ( 'NONE', #40809, 1000.000000000000000 ) ;
#86730 = VECTOR ( 'NONE', #15108, 1000.000000000000227 ) ;
#86731 = ORIENTED_EDGE ( 'NONE', *, *, #51867, .F. ) ;
#86732 = CYLINDRICAL_SURFACE ( 'NONE', #19813, 7.950000000000000178 ) ;
#86733 = ADVANCED_FACE ( 'NONE', ( #68938 ), #13775, .F. ) ;
#86734 = CARTESIAN_POINT ( 'NONE',  ( -12.69999999999998153, 0.000000000000000000, 0.000000000000000000 ) ) ;
#86735 = CARTESIAN_POINT ( 'NONE',  ( 10.37159235450332062, 9.902892378096218942E-16, 0.000000000000000000 ) ) ;
#86736 = FACE_OUTER_BOUND ( 'NONE', #127564, .T. ) ;
#86737 = ORIENTED_EDGE ( 'NONE', *, *, #104971, .T. ) ;
#86738 = DIRECTION ( 'NONE',  ( -0.000000000000000000, 0.3543493200069153248, 0.9351131265310292928 ) ) ;
#86739 = DIRECTION ( 'NONE',  ( -0.7071067811865486830, -0.7071067811865464625, 0.000000000000000000 ) ) ;
#86740 = EDGE_CURVE ( 'NONE', #42201, #99199, #40977, .T. ) ;
#86741 = ADVANCED_FACE ( 'NONE', ( #141731 ), #98217, .F. ) ;
#86742 = VERTEX_POINT ( 'NONE', #108324 ) ;
#86743 = CARTESIAN_POINT ( 'NONE',  ( -34.92500000000001137, -22.22500000000000142, 4.500000000000000888 ) ) ;
#86744 = CARTESIAN_POINT ( 'NONE',  ( 23.99999999999984013, -1.447814304570811617, 5.000000000000000000 ) ) ;
#86745 = CARTESIAN_POINT ( 'NONE',  ( -8.292986735706895374, -21.74070752338406010, 4.999753212805224223 ) ) ;
#86746 = EDGE_CURVE ( 'NONE', #96318, #138853, #42431, .T. ) ;
#86747 = ORIENTED_EDGE ( 'NONE', *, *, #65939, .T. ) ;
#86748 = ORIENTED_EDGE ( 'NONE', *, *, #43969, .F. ) ;
#86749 = EDGE_CURVE ( 'NONE', #135705, #75982, #12376, .T. ) ;
#86750 = FACE_BOUND ( 'NONE', #31791, .T. ) ;
#86751 = EDGE_CURVE ( 'NONE', #6180, #55828, #109796, .T. ) ;
#86752 = FACE_OUTER_BOUND ( 'NONE', #8880, .T. ) ;
#86753 = DIRECTION ( 'NONE',  ( -0.7071067811865486830, -0.7071067811865464625, 0.000000000000000000 ) ) ;
#86754 = DIRECTION ( 'NONE',  ( -0.7071067811865486830, -0.7071067811865464625, 0.000000000000000000 ) ) ;
#86755 = CARTESIAN_POINT ( 'NONE',  ( -24.48921356237309510, -27.52281430457072631, 5.000000000000000000 ) ) ;
#86756 = CARTESIAN_POINT ( 'NONE',  ( 0.4425134659199910780, -0.6000000000000000888, 4.147378741781976075 ) ) ;
#86757 = ORIENTED_EDGE ( 'NONE', *, *, #139122, .F. ) ;
#86758 = EDGE_CURVE ( 'NONE', #45664, #80973, #30834, .T. ) ;
#86759 = ORIENTED_EDGE ( 'NONE', *, *, #49939, .T. ) ;
#86760 = CARTESIAN_POINT ( 'NONE',  ( 114.8287635252314516, 0.000000000000000000, -6.109999999999998543 ) ) ;
#86761 = ORIENTED_EDGE ( 'NONE', *, *, #9622, .T. ) ;
#86762 = ADVANCED_FACE ( 'NONE', ( #22056 ), #140977, .T. ) ;
#86763 = ORIENTED_EDGE ( 'NONE', *, *, #79755, .F. ) ;
#86764 = CARTESIAN_POINT ( 'NONE',  ( 181.1395720402183258, -48.08977582060966682, 37.49964900842703486 ) ) ;
#86765 = EDGE_CURVE ( 'NONE', #95628, #270, #130138, .T. ) ;
#86766 = CARTESIAN_POINT ( 'NONE',  ( 15.51665438641034633, 22.22500000000000142, 4.500000000000000888 ) ) ;
#86767 = CARTESIAN_POINT ( 'NONE',  ( -29.99999999999978328, -22.22500000000000853, 4.412002311790081954 ) ) ;
#86768 = VERTEX_POINT ( 'NONE', #109064 ) ;
#86769 = CARTESIAN_POINT ( 'NONE',  ( 68.62086038379622721, -6.884901960086286188, 3.974999999999997424 ) ) ;
#86770 = CARTESIAN_POINT ( 'NONE',  ( 38.99451991528749062, 28.92564299267965211, 4.000000000000000000 ) ) ;
#86772 = CARTESIAN_POINT ( 'NONE',  ( 33.18398860626899705, 28.73617430169810305, 5.000000000000000000 ) ) ;
#86771 = CARTESIAN_POINT ( 'NONE',  ( -38.99451991528749062, 28.92564299267965211, 4.000000000000000000 ) ) ;
#86773 = CARTESIAN_POINT ( 'NONE',  ( -32.67183060077624646, -15.74070752338412404, 4.000000000000000000 ) ) ;
#86774 = EDGE_CURVE ( 'NONE', #55801, #12165, #98902, .T. ) ;
#86775 = DIRECTION ( 'NONE',  ( 0.7071067811865487940, 0.7071067811865463515, 0.000000000000000000 ) ) ;
#86776 = EDGE_LOOP ( 'NONE', ( #54408, #122455, #99333, #129766 ) ) ;
#86777 = DIRECTION ( 'NONE',  ( 0.7071067811865487940, 0.7071067811865463515, -0.000000000000000000 ) ) ;
#86778 = FACE_OUTER_BOUND ( 'NONE', #58999, .T. ) ;
#86779 = ORIENTED_EDGE ( 'NONE', *, *, #133996, .F. ) ;
#86780 = CARTESIAN_POINT ( 'NONE',  ( -25.00442415654155681, 3.591886032380943838, 4.000000000000000000 ) ) ;
#86781 = EDGE_LOOP ( 'NONE', ( #37007, #80620, #74846, #114926 ) ) ;
#86782 = VERTEX_POINT ( 'NONE', #43129 ) ;
#86783 = ORIENTED_EDGE ( 'NONE', *, *, #115823, .F. ) ;
#86784 = CARTESIAN_POINT ( 'NONE',  ( 62.41709685856476852, 3.054999999999998828, 5.291415217122922066 ) ) ;
#86785 = EDGE_CURVE ( 'NONE', #18390, #42437, #10463, .T. ) ;
#86786 = ORIENTED_EDGE ( 'NONE', *, *, #57784, .T. ) ;
#86787 = ORIENTED_EDGE ( 'NONE', *, *, #58039, .F. ) ;
#86788 = LINE ( 'NONE', #54879, #109153 ) ;
#86789 = EDGE_CURVE ( 'NONE', #99104, #10403, #135164, .T. ) ;
#86790 = CIRCLE ( 'NONE', #52108, 2.999999999999999112 ) ;
#86791 = CARTESIAN_POINT ( 'NONE',  ( 100.7712635252314328, 4.472830434245838482, 4.472830434245842035 ) ) ;
#86792 = CARTESIAN_POINT ( 'NONE',  ( 2.301729841053981929, -2.500000000000000444, 0.000000000000000000 ) ) ;
#86793 = COLOUR_RGB ( '', 0.31764706, 0.68627451, 0.89019608) ;
#86794 = DIRECTION ( 'NONE',  ( -0.7071067811865487940, 0.7071067811865463515, 0.000000000000000000 ) ) ;
#86795 = ORIENTED_EDGE ( 'NONE', *, *, #127643, .F. ) ;
#86796 = LINE ( 'NONE', #109952, #129706 ) ;
#86797 = ADVANCED_FACE ( 'NONE', ( #53256 ), #66312, .F. ) ;
#86798 = DIRECTION ( 'NONE',  ( 0.7071067811865487940, 0.7071067811865463515, 0.000000000000000000 ) ) ;
#86799 = CARTESIAN_POINT ( 'NONE',  ( 90.25000000000000000, -9.735942053221458872E-16, 7.950000000000000178 ) ) ;
#86800 = DIRECTION ( 'NONE',  ( -1.000000000000000000, -1.224606353822377258E-16, -0.000000000000000000 ) ) ;
#86801 = EDGE_LOOP ( 'NONE', ( #34688, #18745, #50430, #49783 ) ) ;
#86802 = CARTESIAN_POINT ( 'NONE',  ( 42.29974487139158157, -27.71228299555235708, 4.000000000000000000 ) ) ;
#86803 = ORIENTED_EDGE ( 'NONE', *, *, #84594, .T. ) ;
#86804 = ORIENTED_EDGE ( 'NONE', *, *, #120403, .F. ) ;
#86805 = ORIENTED_EDGE ( 'NONE', *, *, #119718, .T. ) ;
#86806 = CARTESIAN_POINT ( 'NONE',  ( 117.5995968585647944, -6.109999999999997655, -1.637169565754160283 ) ) ;
#86807 = VERTEX_POINT ( 'NONE', #32241 ) ;
#86808 = LINE ( 'NONE', #31704, #79301 ) ;
#86809 = FACE_OUTER_BOUND ( 'NONE', #38649, .T. ) ;
#86810 = VERTEX_POINT ( 'NONE', #9757 ) ;
#86811 = LINE ( 'NONE', #64453, #19655 ) ;
#86812 = DIRECTION ( 'NONE',  ( -0.7071067811865487940, 0.7071067811865463515, 0.000000000000000000 ) ) ;
#86813 = ORIENTED_EDGE ( 'NONE', *, *, #60548, .F. ) ;
#86814 = VECTOR ( 'NONE', #104690, 1000.000000000000000 ) ;
#86815 = AXIS2_PLACEMENT_3D ( 'NONE', #11882, #78596, #113338 ) ;
#86816 = CARTESIAN_POINT ( 'NONE',  ( 12.52040314143522082, 7.934999999999989839, -2.126176841940961904 ) ) ;
#86817 = DIRECTION ( 'NONE',  ( -0.000000000000000000, 0.3543493200069153248, 0.9351131265310292928 ) ) ;
#86818 = AXIS2_PLACEMENT_3D ( 'NONE', #128169, #107098, #128852 ) ;
#86819 = DIRECTION ( 'NONE',  ( -0.7071067811865486830, 0.7071067811865464625, 0.000000000000000000 ) ) ;
#86820 = AXIS2_PLACEMENT_3D ( 'NONE', #22342, #110781, #44902 ) ;
#86821 = CARTESIAN_POINT ( 'NONE',  ( -31.49999999999977973, 5.696342897626483825, -7.587980461218473138 ) ) ;
#86822 = ORIENTED_EDGE ( 'NONE', *, *, #78765, .T. ) ;
#86823 = EDGE_LOOP ( 'NONE', ( #39579, #45725, #84631, #90659, #95519, #37062 ) ) ;
#86824 = EDGE_CURVE ( 'NONE', #70917, #37150, #1712, .T. ) ;
#86825 = ADVANCED_FACE ( 'NONE', ( #76478 ), #110483, .F. ) ;
#86826 = EDGE_LOOP ( 'NONE', ( #72398, #138979, #132304, #103121 ) ) ;
#86827 = DIRECTION ( 'NONE',  ( 0.7071067811865487940, -0.7071067811865463515, 0.000000000000000000 ) ) ;
#86828 = DIRECTION ( 'NONE',  ( -1.000000000000000000, -1.224606353822377258E-16, -0.000000000000000000 ) ) ;
#86829 = CARTESIAN_POINT ( 'NONE',  ( 0.2100385299584287269, -0.4000000000000003553, 2.083955186700111373 ) ) ;
#86830 = CARTESIAN_POINT ( 'NONE',  ( -30.18398860626900060, 28.73617430169808173, 5.000000000000000000 ) ) ;
#86831 = DIRECTION ( 'NONE',  ( -0.000000000000000000, -0.3543493200069152693, 0.9351131265310292928 ) ) ;
#86832 = CARTESIAN_POINT ( 'NONE',  ( 19.05000000000000071, 3.174999999999997158, 4.000000000000000000 ) ) ;
#86833 = CARTESIAN_POINT ( 'NONE',  ( 26.54209685856477563, 5.291415217122923842, -3.054999999999996163 ) ) ;
#86834 = LINE ( 'NONE', #139808, #141628 ) ;
#86835 = DIRECTION ( 'NONE',  ( 0.7071067811865487940, 0.7071067811865463515, 0.000000000000000000 ) ) ;
#86836 = ORIENTED_EDGE ( 'NONE', *, *, #16416, .F. ) ;
#86837 = DIRECTION ( 'NONE',  ( 0.7071067811865487940, 0.7071067811865463515, -0.000000000000000000 ) ) ;
#86838 = ORIENTED_EDGE ( 'NONE', *, *, #76217, .T. ) ;
#86839 = DIRECTION ( 'NONE',  ( 0.6830127018922180770, -0.6830127018922204085, -0.2588190451025213501 ) ) ;
#86840 = ORIENTED_EDGE ( 'NONE', *, *, #42750, .F. ) ;
#86841 = EDGE_CURVE ( 'NONE', #40570, #27504, #63477, .T. ) ;
#86842 = CARTESIAN_POINT ( 'NONE',  ( 18.18398860626898994, 28.73617430169800002, 5.000000000000000000 ) ) ;
#86844 = ORIENTED_EDGE ( 'NONE', *, *, #25023, .T. ) ;
#86843 = DIRECTION ( 'NONE',  ( 1.000000000000000000, 0.000000000000000000, 0.000000000000000000 ) ) ;
#86845 = ADVANCED_FACE ( 'NONE', ( #111955 ), #135154, .F. ) ;
#86846 = DIRECTION ( 'NONE',  ( 0.7071067811865487940, 0.7071067811865463515, 0.000000000000000000 ) ) ;
#86847 = EDGE_LOOP ( 'NONE', ( #47067, #43821, #46872, #106604 ) ) ;
#86848 = CARTESIAN_POINT ( 'NONE',  ( 34.49999999999975842, -4.216083040037219121, -7.486842126848736179 ) ) ;
#86849 = EDGE_LOOP ( 'NONE', ( #51343, #99467, #137933, #63617 ) ) ;
#86850 = DIRECTION ( 'NONE',  ( -1.000000000000000000, 1.743732761913359971E-15, 0.000000000000000000 ) ) ;
#86851 = UNCERTAINTY_MEASURE_WITH_UNIT (LENGTH_MEASURE( 1.000000000000000082E-05 ), #47663, 'distance_accuracy_value', 'NONE');
#86852 = VERTEX_POINT ( 'NONE', #78601 ) ;
#86853 = EDGE_CURVE ( 'NONE', #92018, #42749, #46744, .T. ) ;
#86854 = EDGE_CURVE ( 'NONE', #15339, #9148, #111961, .T. ) ;
#86855 = DIRECTION ( 'NONE',  ( -0.7071067811865486830, -0.7071067811865464625, 0.000000000000000000 ) ) ;
#86856 = CARTESIAN_POINT ( 'NONE',  ( 110.7666937171295558, -7.949999999999999289, 2.130196079827424427 ) ) ;
#86857 = DIRECTION ( 'NONE',  ( -0.7071067811865486830, -0.7071067811865464625, -0.000000000000000000 ) ) ;
#86858 = CARTESIAN_POINT ( 'NONE',  ( -39.18398860626899705, 28.73617430169814568, 5.000000000000000000 ) ) ;
#86859 = ADVANCED_FACE ( 'NONE', ( #69166 ), #35848, .F. ) ;
#86860 = CARTESIAN_POINT ( 'NONE',  ( 9.005480084712511157, 28.92564299267931816, 4.000000000000000000 ) ) ;
#86861 = CARTESIAN_POINT ( 'NONE',  ( -20.29387692260790388, 22.22500000000000142, 4.000000000000000000 ) ) ;
#86862 = FACE_OUTER_BOUND ( 'NONE', #76746, .T. ) ;
#86863 = CARTESIAN_POINT ( 'NONE',  ( 9.479166666666666075, 6.094999999999988205, -1.633150327867694651 ) ) ;
#86864 = CARTESIAN_POINT ( 'NONE',  ( 20.10373647476855297, 5.808823158059035485, 5.808823158059032821 ) ) ;
#86865 = LINE ( 'NONE', #44073, #18797 ) ;
#86866 = DIRECTION ( 'NONE',  ( -1.000000000000000000, 0.000000000000000000, 0.000000000000000000 ) ) ;
#86867 = EDGE_LOOP ( 'NONE', ( #49996, #45416, #86938, #19498 ) ) ;
#86868 = ORIENTED_EDGE ( 'NONE', *, *, #41566, .F. ) ;
#86869 = EDGE_CURVE ( 'NONE', #109420, #61439, #14031, .T. ) ;
#86870 = FACE_OUTER_BOUND ( 'NONE', #38975, .T. ) ;
#86871 = ORIENTED_EDGE ( 'NONE', *, *, #127346, .T. ) ;
#86872 = CARTESIAN_POINT ( 'NONE',  ( 18.66846741159845635, -18.74070752338408852, 20.73178291233845627 ) ) ;
#86873 = CARTESIAN_POINT ( 'NONE',  ( -27.18398860626900060, 28.73617430169806042, 5.000000000000000000 ) ) ;
#86874 = ORIENTED_EDGE ( 'NONE', *, *, #51874, .F. ) ;
#86875 = EDGE_CURVE ( 'NONE', #110155, #57989, #101047, .T. ) ;
#86876 = CARTESIAN_POINT ( 'NONE',  ( 31.49999999999978684, 0.4497235411627769075, -5.599840258123467862 ) ) ;
#86877 = DIRECTION ( 'NONE',  ( -0.7071067811865486830, 0.7071067811865464625, 0.000000000000000000 ) ) ;
#86878 =( BOUNDED_CURVE ( )  B_SPLINE_CURVE ( 2, ( #59331, #103483, #115057, #4122, #120797, #73729, #140415, #54860, #86769, #120051, #96868, #143268, #99034 ),
 .UNSPECIFIED., .F., .T. ) 
 B_SPLINE_CURVE_WITH_KNOTS ( ( 3, 2, 2, 2, 2, 2, 3 ),
 ( 0.5666666666666666519, 0.5694444444444444198, 0.5722222222222221877, 0.5749999999999999556, 0.5777777777777777235, 0.5805555555555556024, 0.5833333333333333703 ),
 .UNSPECIFIED. ) 
 CURVE ( )  GEOMETRIC_REPRESENTATION_ITEM ( )  RATIONAL_B_SPLINE_CURVE ( ( 1.000000000000000000, 0.9659258262890683122, 1.000000000000000000, 0.9659258262890683122, 1.000000000000000000, 0.9659258262890683122, 1.000000000000000000, 0.9659258262890683122, 1.000000000000000000, 0.9659258262890683122, 1.000000000000000000, 0.9659258262890683122, 1.000000000000000000 ) ) 
 REPRESENTATION_ITEM ( '' )  );
#86879 = CARTESIAN_POINT ( 'NONE',  ( 18.63425672184678916, 0.000000000000000000, 2.500000000000000444 ) ) ;
#86880 = CARTESIAN_POINT ( 'NONE',  ( 14.24715658456393541, 6.719242673238161601, 5.000000000000000000 ) ) ;
#86882 = EDGE_LOOP ( 'NONE', ( #30915, #67307, #122796, #17604 ) ) ;
#86881 = DIRECTION ( 'NONE',  ( -0.7071067811865486830, 0.7071067811865464625, 0.000000000000000000 ) ) ;
#86883 = CARTESIAN_POINT ( 'NONE',  ( -11.99999999999991296, -5.527737879153202805, -7.983877177622344057 ) ) ;
#86884 = ADVANCED_FACE ( 'NONE', ( #13313 ), #17051, .T. ) ;
#86885 = CYLINDRICAL_SURFACE ( 'NONE', #98494, 6.094999999999989093 ) ;
#86886 =( LENGTH_UNIT ( ) NAMED_UNIT ( * ) SI_UNIT ( .MILLI., .METRE. ) );
#86887 = ADVANCED_FACE ( 'NONE', ( #124241 ), #45997, .T. ) ;
#86888 = DIRECTION ( 'NONE',  ( -0.000000000000000000, -0.3543493200069152693, 0.9351131265310292928 ) ) ;
#86889 = CARTESIAN_POINT ( 'NONE',  ( 34.49999999999975842, -7.535744391599426883, 4.994342998332164107 ) ) ;
#86890 = VERTEX_POINT ( 'NONE', #35121 ) ;
#86891 = AXIS2_PLACEMENT_3D ( 'NONE', #72133, #16996, #54632 ) ;
#86892 = ORIENTED_EDGE ( 'NONE', *, *, #91337, .T. ) ;
#86893 = EDGE_LOOP ( 'NONE', ( #61106, #103793, #91308, #8116 ) ) ;
#86894 = CARTESIAN_POINT ( 'NONE',  ( 91.43793019189810423, -6.110000000000001208, 1.637169565754158951 ) ) ;
#86895 = ORIENTED_EDGE ( 'NONE', *, *, #7200, .T. ) ;
#86896 = EDGE_CURVE ( 'NONE', #83442, #12698, #79364, .T. ) ;
#86897 = CARTESIAN_POINT ( 'NONE',  ( 25.49999999999982947, -13.53360074219759746, 5.000000000000000000 ) ) ;
#86898 = CARTESIAN_POINT ( 'NONE',  ( -5.999999999999956479, 7.007997736742436423, -8.085015511992127202 ) ) ;
#86899 = ORIENTED_EDGE ( 'NONE', *, *, #74720, .F. ) ;
#86900 = CARTESIAN_POINT ( 'NONE',  ( 23.29289321881330110, -9.740707523384184441, 5.000000000000000000 ) ) ;
#86901 = CARTESIAN_POINT ( 'NONE',  ( 49.70833333333332860, -3.974999999999999201, -6.884901960086287964 ) ) ;
#86902 = ADVANCED_FACE ( 'NONE', ( #102514 ), #122812, .T. ) ;
#86903 = EDGE_CURVE ( 'NONE', #105802, #95196, #133703, .T. ) ;
#86904 = CARTESIAN_POINT ( 'NONE',  ( 96.01626352523143737, -4.472830434245839371, 4.472830434245839371 ) ) ;
#86905 = CIRCLE ( 'NONE', #17444, 2.999999999999999112 ) ;
#86906 = ORIENTED_EDGE ( 'NONE', *, *, #77346, .F. ) ;
#86907 = EDGE_CURVE ( 'NONE', #66460, #114269, #135835, .T. ) ;
#86908 = CARTESIAN_POINT ( 'NONE',  ( 0.4414465083558353209, 0.5999999999999986455, -4.146294842461982100 ) ) ;
#86909 = CARTESIAN_POINT ( 'NONE',  ( 7.499999999999951150, -10.53360074219763298, 5.000000000000000000 ) ) ;
#86910 = EDGE_CURVE ( 'NONE', #60012, #117767, #16950, .T. ) ;
#86911 = VERTEX_POINT ( 'NONE', #123566 ) ;
#86912 = ORIENTED_EDGE ( 'NONE', *, *, #78191, .F. ) ;
#86913 = ORIENTED_EDGE ( 'NONE', *, *, #40741, .T. ) ;
#86914 = LINE ( 'NONE', #52132, #100117 ) ;
#86915 = EDGE_CURVE ( 'NONE', #109521, #89318, #56178, .T. ) ;
#86916 = CARTESIAN_POINT ( 'NONE',  ( -51.48921356237309510, -27.52281430457091460, 5.000000000000000000 ) ) ;
#86917 = CARTESIAN_POINT ( 'NONE',  ( 17.27540314143521627, -2.126176841940958351, -7.934999999999988951 ) ) ;
#86918 = CARTESIAN_POINT ( 'NONE',  ( 30.70710678118633652, 14.25929247661556509, 5.000000000000000000 ) ) ;
#86919 = CARTESIAN_POINT ( 'NONE',  ( 0.000000000000000000, 0.000000000000000000, 0.000000000000000000 ) ) ;
#86920 = CIRCLE ( 'NONE', #107700, 2.500000000000000888 ) ;
#86921 = CARTESIAN_POINT ( 'NONE',  ( -8.816011393731004731, 28.73617430169781173, 5.000000000000000000 ) ) ;
#86922 = SURFACE_STYLE_USAGE ( .BOTH. , #33293 ) ;
#86923 = CIRCLE ( 'NONE', #80023, 2.500000000000000888 ) ;
#86924 = ORIENTED_EDGE ( 'NONE', *, *, #61807, .F. ) ;
#86926 = ORIENTED_EDGE ( 'NONE', *, *, #119227, .F. ) ;
#86925 = VECTOR ( 'NONE', #126027, 1000.000000000000227 ) ;
#86927 = EDGE_CURVE ( 'NONE', #8502, #80270, #112651, .T. ) ;
#86928 = LINE ( 'NONE', #122376, #22501 ) ;
#86929 = ORIENTED_EDGE ( 'NONE', *, *, #20429, .T. ) ;
#86930 = ORIENTED_EDGE ( 'NONE', *, *, #25339, .T. ) ;
#86931 = EDGE_CURVE ( 'NONE', #123040, #112560, #69909, .T. ) ;
#86932 = CARTESIAN_POINT ( 'NONE',  ( 15.19713381108422290, 7.733989266307781385, 4.000000000000000000 ) ) ;
#86933 = ORIENTED_EDGE ( 'NONE', *, *, #59820, .F. ) ;
#86934 = FACE_OUTER_BOUND ( 'NONE', #31206, .T. ) ;
#86935 = LINE ( 'NONE', #55029, #71057 ) ;
#86936 = PLANE ( 'NONE',  #18235 ) ;
#86937 = DIRECTION ( 'NONE',  ( 1.000000000000000000, 1.224606353822377258E-16, 0.000000000000000000 ) ) ;
#86938 = ORIENTED_EDGE ( 'NONE', *, *, #9604, .T. ) ;
#86939 = EDGE_LOOP ( 'NONE', ( #59243, #20952, #89659, #31965 ) ) ;
#86940 = CARTESIAN_POINT ( 'NONE',  ( 51.18398860626899705, 28.73617430169823095, 5.000000000000000000 ) ) ;
#86941 = VERTEX_POINT ( 'NONE', #77891 ) ;
#86942 = LINE ( 'NONE', #95658, #104761 ) ;
#86943 = ORIENTED_EDGE ( 'NONE', *, *, #49619, .T. ) ;
#86944 = CARTESIAN_POINT ( 'NONE',  ( -34.92500000000001137, -17.14387692260738305, 4.000000000000000000 ) ) ;
#86945 = VERTEX_POINT ( 'NONE', #287 ) ;
#86946 = ORIENTED_EDGE ( 'NONE', *, *, #117277, .T. ) ;
#86947 = ORIENTED_EDGE ( 'NONE', *, *, #102830, .F. ) ;
#86948 = EDGE_CURVE ( 'NONE', #47328, #22343, #1011, .T. ) ;
#86949 = DIRECTION ( 'NONE',  ( 0.000000000000000000, -1.000000000000000000, 0.000000000000000000 ) ) ;
#86950 =( LENGTH_UNIT ( ) NAMED_UNIT ( * ) SI_UNIT ( .MILLI., .METRE. ) );
#86951 = DIRECTION ( 'NONE',  ( 0.7071067811865487940, -0.7071067811865463515, 0.000000000000000000 ) ) ;
#86952 = PLANE ( 'NONE',  #27680 ) ;
#86953 = DIRECTION ( 'NONE',  ( -0.7071067811865487940, 0.7071067811865463515, -0.000000000000000000 ) ) ;
#86954 = CARTESIAN_POINT ( 'NONE',  ( -0.4892135623730947680, -27.52281430457055578, 5.000000000000000000 ) ) ;
#86955 = DIRECTION ( 'NONE',  ( -0.3543493200069162685, -0.000000000000000000, -0.9351131265310288487 ) ) ;
#86956 = CARTESIAN_POINT ( 'NONE',  ( -9.717577386425604757, -21.73023691814493574, 5.000000000000000888 ) ) ;
#86957 = DIRECTION ( 'NONE',  ( 0.7071067811865487940, 0.7071067811865463515, 0.000000000000000000 ) ) ;
#86958 = DIRECTION ( 'NONE',  ( -0.000000000000000000, -0.000000000000000000, 1.000000000000000000 ) ) ;
#86959 = DIRECTION ( 'NONE',  ( 0.3543493200069162685, -0.000000000000000000, -0.9351131265310288487 ) ) ;
#86960 = ORIENTED_EDGE ( 'NONE', *, *, #140707, .F. ) ;
#86961 = ORIENTED_EDGE ( 'NONE', *, *, #105187, .F. ) ;
#86962 = ORIENTED_EDGE ( 'NONE', *, *, #24266, .T. ) ;
#86963 = DIRECTION ( 'NONE',  ( 0.7071067811865486830, -0.7071067811865464625, -0.000000000000000000 ) ) ;
#86964 = ORIENTED_EDGE ( 'NONE', *, *, #52238, .T. ) ;
#86965 = ORIENTED_EDGE ( 'NONE', *, *, #20569, .T. ) ;
#86966 = PLANE ( 'NONE',  #23572 ) ;
#86967 = CARTESIAN_POINT ( 'NONE',  ( 44.99451991528749772, 28.92564299267969474, 4.000000000000000000 ) ) ;
#86968 = DIRECTION ( 'NONE',  ( -0.3543493200069163240, -0.000000000000000000, 0.9351131265310288487 ) ) ;
#86969 = ORIENTED_EDGE ( 'NONE', *, *, #110611, .T. ) ;
#86970 = CARTESIAN_POINT ( 'NONE',  ( 47.99451991528749062, 28.92564299267971251, 4.000000000000000000 ) ) ;
#86971 = EDGE_LOOP ( 'NONE', ( #84186, #97150, #95863 ) ) ;
#86972 = CARTESIAN_POINT ( 'NONE',  ( 19.49999999999986855, 13.46639925780212010, 5.000000000000000000 ) ) ;
#86973 = DIRECTION ( 'NONE',  ( 0.000000000000000000, -1.000000000000000000, 0.000000000000000000 ) ) ;
#86974 = CARTESIAN_POINT ( 'NONE',  ( 7.067069808101886785, 2.126176841940952134, -7.934999999999993392 ) ) ;
#86975 = VERTEX_POINT ( 'NONE', #71309 ) ;
#86976 = CARTESIAN_POINT ( 'NONE',  ( 95.43293019189809456, 1.637169565754156730, 6.110000000000001208 ) ) ;
#86977 =( BOUNDED_CURVE ( )  B_SPLINE_CURVE ( 3, ( #108453, #64290, #97607, #86766 ),
 .UNSPECIFIED., .F., .T. ) 
 B_SPLINE_CURVE_WITH_KNOTS ( ( 4, 4 ),
 ( 2.001653308786169649, 3.503810798801450854 ),
 .UNSPECIFIED. ) 
 CURVE ( )  GEOMETRIC_REPRESENTATION_ITEM ( )  RATIONAL_B_SPLINE_CURVE ( ( 1.000000000000000000, 0.8206354192515240564, 0.8206354192515240564, 1.000000000000000000 ) ) 
 REPRESENTATION_ITEM ( '' )  );
#86978 = CARTESIAN_POINT ( 'NONE',  ( 26.51078643762690845, -27.52281430457036748, 5.000000000000000000 ) ) ;
#86979 = VECTOR ( 'NONE', #91023, 1000.000000000000000 ) ;
#86980 = CARTESIAN_POINT ( 'NONE',  ( 55.38366852087663972, -49.19090614207205192, -40.79110616922474719 ) ) ;
#86981 = CARTESIAN_POINT ( 'NONE',  ( 17.54840764549667398, 9.139736423841732040E-16, 0.000000000000000000 ) ) ;
#86982 = VERTEX_POINT ( 'NONE', #125689 ) ;
#86983 = ORIENTED_EDGE ( 'NONE', *, *, #52725, .F. ) ;
#86984 = CARTESIAN_POINT ( 'NONE',  ( -62.99451991528749772, 28.92564299267982264, 4.000000000000000000 ) ) ;
#86985 = EDGE_LOOP ( 'NONE', ( #65801, #18112, #126548, #39947 ) ) ;
#86986 = CARTESIAN_POINT ( 'NONE',  ( 42.48921356237308800, -27.52281430457085065, 5.000000000000000000 ) ) ;
#86987 = DIRECTION ( 'NONE',  ( 0.7071067811865487940, 0.7071067811865463515, 0.000000000000000000 ) ) ;
#86988 = DIRECTION ( 'NONE',  ( 0.6830127018922180770, -0.6830127018922204085, -0.2588190451025213501 ) ) ;
#86989 = CARTESIAN_POINT ( 'NONE',  ( 24.41159235450331977, -2.500000000000000444, 3.061616997868384620E-16 ) ) ;
#86990 = VERTEX_POINT ( 'NONE', #115464 ) ;
#86991 = DIRECTION ( 'NONE',  ( -0.7071067811865486830, 0.7071067811865464625, 0.000000000000000000 ) ) ;
#86992 = LINE ( 'NONE', #40650, #60520 ) ;
#86993 = DIRECTION ( 'NONE',  ( 0.7071067811865487940, -0.7071067811865463515, 0.000000000000000000 ) ) ;
#86994 = EDGE_CURVE ( 'NONE', #40996, #135817, #28518, .T. ) ;
#86995 = ORIENTED_EDGE ( 'NONE', *, *, #69198, .F. ) ;
#86996 = DIRECTION ( 'NONE',  ( 1.055184596092948005E-16, -1.000000000000000000, 0.000000000000000000 ) ) ;
#86997 = PLANE ( 'NONE',  #79469 ) ;
#86998 = ORIENTED_EDGE ( 'NONE', *, *, #22193, .F. ) ;
#86999 = EDGE_CURVE ( 'NONE', #38008, #57414, #61868, .T. ) ;
#87001 = EDGE_LOOP ( 'NONE', ( #10251, #115625, #51521, #71151 ) ) ;
#87000 = DIRECTION ( 'NONE',  ( 0.7071067811865487940, -0.7071067811865463515, 0.000000000000000000 ) ) ;
#87002 = ORIENTED_EDGE ( 'NONE', *, *, #53571, .T. ) ;
#87003 = EDGE_CURVE ( 'NONE', #39324, #35758, #137987, .T. ) ;
#87004 = EDGE_CURVE ( 'NONE', #23962, #38919, #125823, .T. ) ;
#87005 = LINE ( 'NONE', #76138, #107193 ) ;
#87006 = PLANE ( 'NONE',  #117810 ) ;
#87007 = ORIENTED_EDGE ( 'NONE', *, *, #130310, .F. ) ;
#87008 = CARTESIAN_POINT ( 'NONE',  ( 31.49999999999977973, -4.216083040037219121, -7.486842126848729073 ) ) ;
#87009 = UNCERTAINTY_MEASURE_WITH_UNIT (LENGTH_MEASURE( 1.000000000000000082E-05 ), #60137, 'distance_accuracy_value', 'NONE');
#87010 = AXIS2_PLACEMENT_3D ( 'NONE', #114161, #39481, #138794 ) ;
#87011 = ADVANCED_FACE ( 'NONE', ( #128537 ), #15437, .T. ) ;
#87012 = EDGE_CURVE ( 'NONE', #125049, #61826, #15679, .T. ) ;
#87013 = CARTESIAN_POINT ( 'NONE',  ( -15.00548008471250228, 28.92564299267927552, 4.000000000000000000 ) ) ;
#87014 = AXIS2_PLACEMENT_3D ( 'NONE', #7346, #129143, #60353 ) ;
#87015 = LINE ( 'NONE', #21026, #43855 ) ;
#87016 = VECTOR ( 'NONE', #87296, 999.9999999999998863 ) ;
#87017 = DIRECTION ( 'NONE',  ( -0.5735764363510507113, 0.8191520442889885789, 1.003171929053520926E-16 ) ) ;
#87019 = VECTOR ( 'NONE', #102932, 1000.000000000000000 ) ;
#87018 = CARTESIAN_POINT ( 'NONE',  ( 0.1600000000000026401, -9.717572351234235426E-16, -7.934999999999990727 ) ) ;
#87020 = ADVANCED_FACE ( 'NONE', ( #82898 ), #37234, .F. ) ;
#87021 = LINE ( 'NONE', #31225, #76933 ) ;
#87022 = CARTESIAN_POINT ( 'NONE',  ( -19.05000000000000071, 3.174999999999997158, 4.000000000000000000 ) ) ;
#87023 = PLANE ( 'NONE',  #22837 ) ;
#87024 = LINE ( 'NONE', #10163, #98885 ) ;
#87025 = DIRECTION ( 'NONE',  ( -0.7071067811865486830, 0.7071067811865464625, 0.000000000000000000 ) ) ;
#87026 = FACE_OUTER_BOUND ( 'NONE', #7956, .T. ) ;
#87028 = ADVANCED_FACE ( 'NONE', ( #95169 ), #82203, .F. ) ;
#87027 = COLOUR_RGB ( '', 0.72549020, 0.75294118, 0.79215686) ;
#87029 = CARTESIAN_POINT ( 'NONE',  ( -34.47516574401892342, 7.490517612115540125, 4.998110765256834398 ) ) ;
#87030 = DIRECTION ( 'NONE',  ( 0.7071067811865486830, -0.7071067811865464625, -0.000000000000000000 ) ) ;
#87031 = ORIENTED_EDGE ( 'NONE', *, *, #73257, .F. ) ;
#87032 = ORIENTED_EDGE ( 'NONE', *, *, #26801, .T. ) ;
#87033 = VERTEX_POINT ( 'NONE', #81485 ) ;
#87035 = ADVANCED_FACE ( 'NONE', ( #138708 ), #27062, .T. ) ;
#87034 = CARTESIAN_POINT ( 'NONE',  ( 98.12500000000000000, -7.950000000000000178, -4.867971026610729436E-16 ) ) ;
#87036 = VERTEX_POINT ( 'NONE', #29204 ) ;
#87037 = ORIENTED_EDGE ( 'NONE', *, *, #6613, .F. ) ;
#87038 = ORIENTED_EDGE ( 'NONE', *, *, #35906, .F. ) ;
#87039 = DIRECTION ( 'NONE',  ( 0.7071067811865486830, -0.7071067811865464625, -0.000000000000000000 ) ) ;
#87040 = CARTESIAN_POINT ( 'NONE',  ( 12.19999999999999574, -22.33999999999998565, 3.000000000000000000 ) ) ;
#87041 = VERTEX_POINT ( 'NONE', #27779 ) ;
#87042 = LINE ( 'NONE', #43534, #143516 ) ;
#87043 = EDGE_CURVE ( 'NONE', #82254, #63910, #127834, .T. ) ;
#87044 = LINE ( 'NONE', #133416, #132074 ) ;
#87045 = CARTESIAN_POINT ( 'NONE',  ( 13.10530833935383299, 3.713635273109022084, 4.055062020558137803 ) ) ;
#87046 = DIRECTION ( 'NONE',  ( 0.3543493200069163240, 0.000000000000000000, 0.9351131265310288487 ) ) ;
#87047 = VERTEX_POINT ( 'NONE', #48841 ) ;
#87048 = CARTESIAN_POINT ( 'NONE',  ( 0.000000000000000000, 0.000000000000000000, 5.000000000000000000 ) ) ;
#87049 = DIRECTION ( 'NONE',  ( -0.000000000000000000, -0.3543493200069152693, 0.9351131265310292928 ) ) ;
#87050 = LINE ( 'NONE', #79793, #21587 ) ;
#87051 = ADVANCED_FACE ( 'NONE', ( #104627 ), #72043, .T. ) ;
#87052 = FACE_OUTER_BOUND ( 'NONE', #140352, .T. ) ;
#87053 = DIRECTION ( 'NONE',  ( 1.000000000000000000, 0.000000000000000000, 0.000000000000000000 ) ) ;
#87054 = CARTESIAN_POINT ( 'NONE',  ( 23.99999999999983302, -18.41253812416056590, 4.000000000000000000 ) ) ;
#87055 = CARTESIAN_POINT ( 'NONE',  ( 32.30836038379622721, 7.949999999999997513, 2.130196079827431088 ) ) ;
#87056 =( BOUNDED_CURVE ( )  B_SPLINE_CURVE ( 3, ( #118401, #52432, #116980, #116276 ),
 .UNSPECIFIED., .F., .T. ) 
 B_SPLINE_CURVE_WITH_KNOTS ( ( 4, 4 ),
 ( 1.208578181583237710, 1.359146454359470901 ),
 .UNSPECIFIED. ) 
 CURVE ( )  GEOMETRIC_REPRESENTATION_ITEM ( )  RATIONAL_B_SPLINE_CURVE ( ( 1.000000000000000000, 0.9981116584018945304, 0.9981116584018945304, 1.000000000000000000 ) ) 
 REPRESENTATION_ITEM ( '' )  );
#87057 = CARTESIAN_POINT ( 'NONE',  ( -60.29974487139158867, -27.71228299555248142, 4.000000000000000000 ) ) ;
#87058 = ORIENTED_EDGE ( 'NONE', *, *, #133187, .F. ) ;
#87059 = ORIENTED_EDGE ( 'NONE', *, *, #35912, .F. ) ;
#87060 = CARTESIAN_POINT ( 'NONE',  ( 118.4170968585647756, 3.054999999999998828, 5.291415217122922066 ) ) ;
#87061 = ORIENTED_EDGE ( 'NONE', *, *, #138241, .T. ) ;
#87062 = FACE_OUTER_BOUND ( 'NONE', #71042, .T. ) ;
#87063 = EDGE_CURVE ( 'NONE', #106536, #124008, #48123, .T. ) ;
#87064 = FACE_OUTER_BOUND ( 'NONE', #4444, .T. ) ;
#87065 = AXIS2_PLACEMENT_3D ( 'NONE', #23931, #133412, #12317 ) ;
#87066 = DIRECTION ( 'NONE',  ( 0.000000000000000000, 0.9647414015272156584, -0.2631995976047526442 ) ) ;
#87067 = LINE ( 'NONE', #74791, #72430 ) ;
#87068 = CARTESIAN_POINT ( 'NONE',  ( 10.49999999999992895, 14.14708470758592185, -0.5283514160166801199 ) ) ;
#87069 = SURFACE_SIDE_STYLE ('',( #66055 ) ) ;
#87070 = ADVANCED_FACE ( 'NONE', ( #9570 ), #31031, .T. ) ;
#87071 = CARTESIAN_POINT ( 'NONE',  ( 118.9120968585647802, 5.291415217122921177, -3.054999999999994831 ) ) ;
#87072 = ORIENTED_EDGE ( 'NONE', *, *, #69567, .T. ) ;
#87073 = EDGE_CURVE ( 'NONE', #6574, #76267, #140137, .T. ) ;
#87074 = ORIENTED_EDGE ( 'NONE', *, *, #43504, .T. ) ;
#87075 = FACE_OUTER_BOUND ( 'NONE', #56897, .T. ) ;
#87076 = CARTESIAN_POINT ( 'NONE',  ( 2.999999999999999112, -5.520864266206504263E-14, 0.000000000000000000 ) ) ;
#87077 = DIRECTION ( 'NONE',  ( -0.3543493200069162685, -0.000000000000000000, -0.9351131265310288487 ) ) ;
#87078 = EDGE_CURVE ( 'NONE', #12722, #102325, #129221, .T. ) ;
#87079 = CARTESIAN_POINT ( 'NONE',  ( -22.42820000000000036, 3.174999999999997602, 1.444000000000000394 ) ) ;
#87080 = ORIENTED_EDGE ( 'NONE', *, *, #26447, .T. ) ;
#87081 = CARTESIAN_POINT ( 'NONE',  ( 43.45876352523143993, 0.000000000000000000, -6.110000000000001208 ) ) ;
#87082 = ORIENTED_EDGE ( 'NONE', *, *, #56396, .F. ) ;
#87083 = CARTESIAN_POINT ( 'NONE',  ( 29.99451991528749417, 28.92564299267958816, 4.000000000000000000 ) ) ;
#87084 = LINE ( 'NONE', #131298, #120197 ) ;
#87085 = DIRECTION ( 'NONE',  ( 0.7071067811865486830, -0.7071067811865464625, -0.000000000000000000 ) ) ;
#87086 = SURFACE_SIDE_STYLE ('',( #31985 ) ) ;
#87087 = EDGE_CURVE ( 'NONE', #106603, #126942, #98734, .T. ) ;
#87088 = AXIS2_PLACEMENT_3D ( 'NONE', #51462, #28987, #77350 ) ;
#87089 = CARTESIAN_POINT ( 'NONE',  ( 41.03709685856478728, -3.054999999999998828, -5.291415217122919401 ) ) ;
#87090 = EDGE_LOOP ( 'NONE', ( #16580, #60875, #41025, #671 ) ) ;
#87091 = VECTOR ( 'NONE', #28962, 1000.000000000000000 ) ;
#87092 = EDGE_CURVE ( 'NONE', #125050, #42229, #125926, .T. ) ;
#87093 = CARTESIAN_POINT ( 'NONE',  ( -12.88837638105233552, 9.759292476615614831, 17.35367589129215560 ) ) ;
#87094 = ORIENTED_EDGE ( 'NONE', *, *, #111117, .F. ) ;
#87095 = ORIENTED_EDGE ( 'NONE', *, *, #97281, .F. ) ;
#87096 = ORIENTED_EDGE ( 'NONE', *, *, #15685, .T. ) ;
#87097 = DIRECTION ( 'NONE',  ( -1.000000000000000000, -1.224606353822377258E-16, -0.000000000000000000 ) ) ;
#87098 = CARTESIAN_POINT ( 'NONE',  ( -0.4892135623730947680, -27.52281430457055578, 5.000000000000000000 ) ) ;
#87099 = VERTEX_POINT ( 'NONE', #77031 ) ;
#87100 = DIRECTION ( 'NONE',  ( 0.3543493200069162685, -0.000000000000000000, -0.9351131265310288487 ) ) ;
#87101 = CARTESIAN_POINT ( 'NONE',  ( 15.48921356237309510, -27.52281430457066236, 5.000000000000000000 ) ) ;
#87102 = CARTESIAN_POINT ( 'NONE',  ( 0.000000000000000000, 0.000000000000000000, 5.000000000000000000 ) ) ;
#87103 = PLANE ( 'NONE',  #120730 ) ;
#87104 = ADVANCED_FACE ( 'NONE', ( #42255 ), #29911, .F. ) ;
#87106 = FACE_BOUND ( 'NONE', #103734, .T. ) ;
#87105 = VECTOR ( 'NONE', #65890, 1000.000000000000000 ) ;
#87107 = ORIENTED_EDGE ( 'NONE', *, *, #21447, .F. ) ;
#87108 = DIRECTION ( 'NONE',  ( -0.7071067811865486830, 0.7071067811865464625, 0.000000000000000000 ) ) ;
#87109 = CARTESIAN_POINT ( 'NONE',  ( 0.5685132242927012358, 4.584330080086930965E-16, 0.000000000000000000 ) ) ;
#87110 = ORIENTED_EDGE ( 'NONE', *, *, #67631, .T. ) ;
#87111 = CARTESIAN_POINT ( 'NONE',  ( 24.39997294953710494, 4.461849672132297329, -4.461849672132302658 ) ) ;
#87112 = ORIENTED_EDGE ( 'NONE', *, *, #44175, .F. ) ;
#87113 = VERTEX_POINT ( 'NONE', #129959 ) ;
#87114 = PLANE ( 'NONE',  #855 ) ;
#87115 = VECTOR ( 'NONE', #16832, 1000.000000000000000 ) ;
#87116 = ORIENTED_EDGE ( 'NONE', *, *, #102202, .T. ) ;
#87117 = VECTOR ( 'NONE', #95981, 1000.000000000000227 ) ;
#87118 = CARTESIAN_POINT ( 'NONE',  ( 60.57876352523145158, -7.482591942790325086E-16, 6.109999999999998543 ) ) ;
#87119 = ORIENTED_EDGE ( 'NONE', *, *, #18103, .F. ) ;
#87120 = DIRECTION ( 'NONE',  ( -0.7071067811865486830, 0.7071067811865464625, 0.000000000000000000 ) ) ;
#87121 = VERTEX_POINT ( 'NONE', #142963 ) ;
#87122 = DIRECTION ( 'NONE',  ( 0.7071067811865487940, -0.7071067811865463515, 0.000000000000000000 ) ) ;
#87123 = FACE_OUTER_BOUND ( 'NONE', #42267, .T. ) ;
#87124 = ORIENTED_EDGE ( 'NONE', *, *, #61898, .T. ) ;
#87125 = CARTESIAN_POINT ( 'NONE',  ( 34.92499999999998295, -4.199905483972782072, 4.759050581649323597 ) ) ;
#87126 = CARTESIAN_POINT ( 'NONE',  ( 31.49999999999977973, -5.947814304570761657, 5.000000000000000000 ) ) ;
#87127 = COLOUR_RGB ( '', 0.09019608, 0.27058824, 0.51372549) ;
#87128 = EDGE_CURVE ( 'NONE', #40303, #20803, #74150, .T. ) ;
#87129 = EDGE_CURVE ( 'NONE', #71803, #118457, #30661, .T. ) ;
#87130 = FACE_OUTER_BOUND ( 'NONE', #86867, .T. ) ;
#87131 = PRESENTATION_STYLE_ASSIGNMENT (( #75547 ) ) ;
#87132 = LINE ( 'NONE', #55220, #55145 ) ;
#87133 = CARTESIAN_POINT ( 'NONE',  ( -2.994519915287485734, 28.92564299267940342, 4.000000000000000000 ) ) ;
#87134 = CARTESIAN_POINT ( 'NONE',  ( -39.29974487139159578, -27.71228299555233576, 4.000000000000000000 ) ) ;
#87135 = ORIENTED_EDGE ( 'NONE', *, *, #103162, .F. ) ;
#87136 = ORIENTED_EDGE ( 'NONE', *, *, #8974, .T. ) ;
#87137 = ORIENTED_EDGE ( 'NONE', *, *, #59410, .T. ) ;
#87138 = CARTESIAN_POINT ( 'NONE',  ( 20.02497294953710849, -4.461849672132299993, -4.461849672132299105 ) ) ;
#87139 = DIRECTION ( 'NONE',  ( -0.6830127018922181881, 0.6830127018922202975, -0.2588190451025214056 ) ) ;
#87140 = VERTEX_POINT ( 'NONE', #52383 ) ;
#87141 = ORIENTED_EDGE ( 'NONE', *, *, #18502, .T. ) ;
#87142 = DIRECTION ( 'NONE',  ( -0.000000000000000000, 0.000000000000000000, 1.000000000000000000 ) ) ;
#87143 = CARTESIAN_POINT ( 'NONE',  ( -5.700255128608413102, -27.71228299555201957, 4.000000000000000000 ) ) ;
#87144 = ADVANCED_FACE ( 'NONE', ( #32069 ), #140806, .T. ) ;
#87145 = PLANE ( 'NONE',  #76230 ) ;
#87146 = ORIENTED_EDGE ( 'NONE', *, *, #81486, .T. ) ;
#87147 = CARTESIAN_POINT ( 'NONE',  ( -42.48921356237308800, -27.52281430457085065, 5.000000000000000000 ) ) ;
#87148 = CARTESIAN_POINT ( 'NONE',  ( 3.836528711265472236, 15.75929247661555443, 9.299976744542929552 ) ) ;
#87149 = CARTESIAN_POINT ( 'NONE',  ( 16.98373647476855197, -5.808823158059035485, -5.808823158059033709 ) ) ;
#87150 = DIRECTION ( 'NONE',  ( -0.7071067811865486830, -0.7071067811865464625, -0.000000000000000000 ) ) ;
#87151 = ORIENTED_EDGE ( 'NONE', *, *, #72562, .T. ) ;
#87152 = CARTESIAN_POINT ( 'NONE',  ( 118.4745968585647802, 1.637169565754164280, -6.109999999999997655 ) ) ;
#87153 = PLANE ( 'NONE',  #35066 ) ;
#87154 = CARTESIAN_POINT ( 'NONE',  ( 21.29974487139158512, -27.71228299555221142, 4.000000000000000000 ) ) ;
#87156 = ORIENTED_EDGE ( 'NONE', *, *, #129200, .T. ) ;
#87155 = CARTESIAN_POINT ( 'NONE',  ( -2.207106781186519928, -20.24070752338407075, 5.000000000000000000 ) ) ;
#87157 = AXIS2_PLACEMENT_3D ( 'NONE', #116466, #47684, #36071 ) ;
#87158 = PLANE ( 'NONE',  #50882 ) ;
#87159 = EDGE_LOOP ( 'NONE', ( #46603, #46220, #131409, #24819 ) ) ;
#87160 = CARTESIAN_POINT ( 'NONE',  ( -2.510786437626908008, -27.52281430457053446, 5.000000000000000000 ) ) ;
#87161 = DIRECTION ( 'NONE',  ( 0.7071067811865487940, -0.7071067811865463515, 0.000000000000000000 ) ) ;
#87162 = CARTESIAN_POINT ( 'NONE',  ( -45.18398860626900415, 28.73617430169818832, 5.000000000000000000 ) ) ;
#87163 = ORIENTED_EDGE ( 'NONE', *, *, #11279, .T. ) ;
#87164 = CARTESIAN_POINT ( 'NONE',  ( 14.99999999999990230, -22.22500000000000142, 4.412002311790040210 ) ) ;
#87166 = EDGE_CURVE ( 'NONE', #105009, #46120, #19757, .T. ) ;
#87165 = FACE_OUTER_BOUND ( 'NONE', #2548, .T. ) ;
#87167 = VECTOR ( 'NONE', #43882, 999.9999999999998863 ) ;
#87168 = VERTEX_POINT ( 'NONE', #41504 ) ;
#87169 = CARTESIAN_POINT ( 'NONE',  ( 6.229065384000522343, -2.500000000000000444, 0.000000000000000000 ) ) ;
#87170 = CARTESIAN_POINT ( 'NONE',  ( 12.00548008471251293, 28.92564299267929684, 4.000000000000000000 ) ) ;
#87171 = VERTEX_POINT ( 'NONE', #63990 ) ;
#87172 = CARTESIAN_POINT ( 'NONE',  ( -22.82816939922336985, -8.240707523384202204, 4.000000000000000000 ) ) ;
#87174 = EDGE_LOOP ( 'NONE', ( #65369, #41690, #84042, #130777 ) ) ;
#87173 = DIRECTION ( 'NONE',  ( 1.000000000000000000, 0.000000000000000000, 0.000000000000000000 ) ) ;
#87175 = EDGE_CURVE ( 'NONE', #63012, #11599, #86466, .T. ) ;
#87176 = ORIENTED_EDGE ( 'NONE', *, *, #127901, .F. ) ;
#87177 = DIRECTION ( 'NONE',  ( 0.3543493200069162685, -0.000000000000000000, -0.9351131265310288487 ) ) ;
#87178 = FILL_AREA_STYLE ('',( #64718 ) ) ;
#87179 = ORIENTED_EDGE ( 'NONE', *, *, #25151, .F. ) ;
#87180 = VECTOR ( 'NONE', #86604, 1000.000000000000000 ) ;
#87181 = FACE_OUTER_BOUND ( 'NONE', #62031, .T. ) ;
#87182 = EDGE_CURVE ( 'NONE', #125316, #137586, #95888, .T. ) ;
#87183 = EDGE_CURVE ( 'NONE', #19965, #71257, #98046, .T. ) ;
#87184 = CARTESIAN_POINT ( 'NONE',  ( 0.000000000000000000, 9.735942053221458872E-16, -7.950000000000000178 ) ) ;
#87185 = DIRECTION ( 'NONE',  ( 0.7071067811865487940, 0.7071067811865463515, -0.000000000000000000 ) ) ;
#87186 = ADVANCED_FACE ( 'NONE', ( #106749 ), #130694, .F. ) ;
#87187 = CONICAL_SURFACE ( 'NONE', #135738, 2.500000000000000888, 0.9599310885968822538 ) ;
#87188 = ORIENTED_EDGE ( 'NONE', *, *, #139126, .T. ) ;
#87189 = PLANE ( 'NONE',  #4902 ) ;
#87190 = EDGE_CURVE ( 'NONE', #121898, #71767, #75586, .T. ) ;
#87191 = PLANE ( 'NONE',  #72182 ) ;
#87192 = CARTESIAN_POINT ( 'NONE',  ( 5.149972949537104938, -4.461849672132299105, 4.461849672132299993 ) ) ;
#87193 = EDGE_CURVE ( 'NONE', #93762, #67859, #64705, .T. ) ;
#87194 = CARTESIAN_POINT ( 'NONE',  ( 40.45376352523144448, -6.109999999999999432, -3.741295971395163529E-16 ) ) ;
#87195 = CARTESIAN_POINT ( 'NONE',  ( 0.000000000000000000, 0.000000000000000000, 5.000000000000000000 ) ) ;
#87196 = ORIENTED_EDGE ( 'NONE', *, *, #121105, .T. ) ;
#87197 = ORIENTED_EDGE ( 'NONE', *, *, #55482, .F. ) ;
#87199 = EDGE_CURVE ( 'NONE', #75992, #52878, #51833, .T. ) ;
#87198 = CARTESIAN_POINT ( 'NONE',  ( 29.20710678118634007, 6.759292476615651246, 5.000000000000000000 ) ) ;
#87200 = ORIENTED_EDGE ( 'NONE', *, *, #105336, .F. ) ;
#87201 = AXIS2_PLACEMENT_3D ( 'NONE', #25767, #23630, #135963 ) ;
#87202 = EDGE_LOOP ( 'NONE', ( #6200, #31190, #9472, #23683 ) ) ;
#87203 = CARTESIAN_POINT ( 'NONE',  ( -1.171830600776461173, -17.24070752338411339, 4.000000000000000000 ) ) ;
#87204 = PLANE ( 'NONE',  #97212 ) ;
#87205 = ORIENTED_EDGE ( 'NONE', *, *, #112393, .T. ) ;
#87206 = PLANE ( 'NONE',  #143415 ) ;
#87207 = CARTESIAN_POINT ( 'NONE',  ( 69.48921356237309510, -27.52281430457103895, 5.000000000000000000 ) ) ;
#87208 = ADVANCED_FACE ( 'NONE', ( #78437 ), #55992, .F. ) ;
#87209 = FACE_OUTER_BOUND ( 'NONE', #82233, .T. ) ;
#87210 = VECTOR ( 'NONE', #80155, 1000.000000000000000 ) ;
#87211 = EDGE_CURVE ( 'NONE', #134939, #99796, #44407, .T. ) ;
#87212 = CARTESIAN_POINT ( 'NONE',  ( -24.99033360189226372, 3.759292476615678336, 4.478963035907990609 ) ) ;
#87213 = CARTESIAN_POINT ( 'NONE',  ( 127.0212635252314328, -4.472830434245839371, -4.472830434245840259 ) ) ;
#87214 = ORIENTED_EDGE ( 'NONE', *, *, #95070, .T. ) ;
#87215 = LINE ( 'NONE', #74938, #99736 ) ;
#87216 = CARTESIAN_POINT ( 'NONE',  ( 22.49999999999984723, 19.39370406404969316, 1.459788787078151406 ) ) ;
#87217 = DIRECTION ( 'NONE',  ( 0.5735764363510448272, -0.8191520442889927978, 1.003171929053526103E-16 ) ) ;
#87218 = CARTESIAN_POINT ( 'NONE',  ( 26.99999999999980105, 5.587461875839197845, 4.000000000000000000 ) ) ;
#87219 = ADVANCED_FACE ( 'NONE', ( #57412 ), #116593, .T. ) ;
#87220 = AXIS2_PLACEMENT_3D ( 'NONE', #83162, #137554, #126641 ) ;
#87221 = CARTESIAN_POINT ( 'NONE',  ( -24.70710678118636494, -0.7407075233842718154, 5.000000000000000000 ) ) ;
#87222 = LINE ( 'NONE', #65503, #1769 ) ;
#87223 = AXIS2_PLACEMENT_3D ( 'NONE', #63920, #18973, #31295 ) ;
#87224 = CARTESIAN_POINT ( 'NONE',  ( 58.12086038379622721, -6.884901960086286188, 3.974999999999997424 ) ) ;
#87225 = PRESENTATION_LAYER_ASSIGNMENT (  '', '', ( #40963 ) ) ;
#87226 = LINE ( 'NONE', #8878, #141019 ) ;
#87227 = ORIENTED_EDGE ( 'NONE', *, *, #72057, .T. ) ;
#87228 = VERTEX_POINT ( 'NONE', #132840 ) ;
#87229 = CARTESIAN_POINT ( 'NONE',  ( 55.97916666666666430, -7.950000000000001066, 2.130196079827424427 ) ) ;
#87230 = DIRECTION ( 'NONE',  ( 0.3543493200069162685, -0.000000000000000000, -0.9351131265310288487 ) ) ;
#87231 = DIRECTION ( 'NONE',  ( -0.6830127018922180770, -0.6830127018922204085, -0.2588190451025213501 ) ) ;
#87233 = DIRECTION ( 'NONE',  ( 0.000000000000000000, 1.000000000000000000, -2.556434596176436916E-15 ) ) ;
#87232 = VECTOR ( 'NONE', #54959, 1000.000000000000000 ) ;
#87234 = EDGE_LOOP ( 'NONE', ( #32374, #73913, #27736, #14916 ) ) ;
#87235 = CARTESIAN_POINT ( 'NONE',  ( 27.68840764549667455, 9.139736423841732040E-16, 0.000000000000000000 ) ) ;
#87236 = DIRECTION ( 'NONE',  ( -0.000000000000000000, 0.3543493200069153248, 0.9351131265310292928 ) ) ;
#87237 = CARTESIAN_POINT ( 'NONE',  ( 49.29209685856476852, -5.291415217122921177, 3.054999999999999272 ) ) ;
#87238 = ORIENTED_EDGE ( 'NONE', *, *, #83240, .F. ) ;
#87239 = ADVANCED_FACE ( 'NONE', ( #68312 ), #34942, .F. ) ;
#87240 = DIRECTION ( 'NONE',  ( 0.000000000000000000, 0.000000000000000000, 1.000000000000000000 ) ) ;
#87241 = ORIENTED_EDGE ( 'NONE', *, *, #88249, .F. ) ;
#87242 = ORIENTED_EDGE ( 'NONE', *, *, #34673, .T. ) ;
#87243 = CARTESIAN_POINT ( 'NONE',  ( 21.83652871126535899, 15.75929247661555443, 9.299976744542970408 ) ) ;
#87244 = CARTESIAN_POINT ( 'NONE',  ( 81.89169371712957002, 2.130196079827421762, 7.950000000000000178 ) ) ;
#87245 = DIRECTION ( 'NONE',  ( -0.7071067811865487940, 0.7071067811865463515, 0.000000000000000000 ) ) ;
#87246 = DIRECTION ( 'NONE',  ( -0.7071067811865487940, 0.7071067811865463515, 0.000000000000000000 ) ) ;
#87247 = ORIENTED_EDGE ( 'NONE', *, *, #7135, .F. ) ;
#87248 = FACE_OUTER_BOUND ( 'NONE', #92461, .T. ) ;
#87249 = DIRECTION ( 'NONE',  ( -0.7071067811865486830, -0.7071067811865464625, -0.000000000000000000 ) ) ;
#87251 = EDGE_LOOP ( 'NONE', ( #30563, #95490, #43729, #34, #42624, #133720 ) ) ;
#87250 = CARTESIAN_POINT ( 'NONE',  ( 2.671830600776449405, -3.740707523384248390, 4.000000000000000000 ) ) ;
#87252 = CARTESIAN_POINT ( 'NONE',  ( 79.33376352523144703, 6.110000000000001208, 1.122388791418549305E-15 ) ) ;
#87253 = CARTESIAN_POINT ( 'NONE',  ( -6.874853806907617049, -14.24070752338413648, 9.401115078912674505 ) ) ;
#87254 = CARTESIAN_POINT ( 'NONE',  ( 113.5375270504628986, -9.735942053221456900E-16, 7.949999999999998401 ) ) ;
#87255 = FACE_OUTER_BOUND ( 'NONE', #77723, .T. ) ;
#87256 = CARTESIAN_POINT ( 'NONE',  ( -66.18398860626901126, 28.73617430169833753, 5.000000000000000000 ) ) ;
#87257 = EDGE_CURVE ( 'NONE', #130662, #43690, #66147, .T. ) ;
#87258 = ORIENTED_EDGE ( 'NONE', *, *, #85485, .F. ) ;
#87259 = VECTOR ( 'NONE', #127181, 999.9999999999998863 ) ;
#87260 = DIRECTION ( 'NONE',  ( -0.000000000000000000, -0.000000000000000000, 1.000000000000000000 ) ) ;
#87261 = CARTESIAN_POINT ( 'NONE',  ( 71.22459685856478018, -1.637169565754160949, 6.109999999999997655 ) ) ;
#87262 = CARTESIAN_POINT ( 'NONE',  ( 17.51078643762690845, -27.52281430457043143, 5.000000000000000000 ) ) ;
#87263 = EDGE_CURVE ( 'NONE', #127403, #130838, #23304, .T. ) ;
#87264 = LINE ( 'NONE', #43757, #119569 ) ;
#87265 = DIRECTION ( 'NONE',  ( -0.6830127018922181881, 0.6830127018922202975, -0.2588190451025214056 ) ) ;
#87266 = ORIENTED_EDGE ( 'NONE', *, *, #42185, .T. ) ;
#87267 = ORIENTED_EDGE ( 'NONE', *, *, #99306, .F. ) ;
#87268 = COLOUR_RGB ( '', 0.08235294, 0.09019608, 0.10196078) ;
#87269 = CARTESIAN_POINT ( 'NONE',  ( -18.18398860626898994, 28.73617430169800002, 5.000000000000000000 ) ) ;
#87270 = CARTESIAN_POINT ( 'NONE',  ( -15.67180000000000639, 3.174999999999997158, 0.000000000000000000 ) ) ;
#87271 = EDGE_LOOP ( 'NONE', ( #137144, #72639, #10460, #107000 ) ) ;
#87272 =( BOUNDED_CURVE ( )  B_SPLINE_CURVE ( 3, ( #6781, #95260, #139530, #84420 ),
 .UNSPECIFIED., .F., .F. ) 
 B_SPLINE_CURVE_WITH_KNOTS ( ( 4, 4 ),
 ( 2.001653308786157659, 3.503810798801451742 ),
 .UNSPECIFIED. ) 
 CURVE ( )  GEOMETRIC_REPRESENTATION_ITEM ( )  RATIONAL_B_SPLINE_CURVE ( ( 1.000000000000000000, 0.8206354192515212809, 0.8206354192515212809, 1.000000000000000000 ) ) 
 REPRESENTATION_ITEM ( '' )  );
#87273 = EDGE_LOOP ( 'NONE', ( #137209, #53326, #128216, #13288 ) ) ;
#87274 = EDGE_CURVE ( 'NONE', #59884, #130856, #2994, .T. ) ;
#87275 = DIRECTION ( 'NONE',  ( -0.7071067811865487940, 0.7071067811865463515, -0.000000000000000000 ) ) ;
#87276 = ORIENTED_EDGE ( 'NONE', *, *, #124819, .F. ) ;
#87277 = DIRECTION ( 'NONE',  ( -1.000000000000000000, -0.000000000000000000, -0.000000000000000000 ) ) ;
#87278 = CARTESIAN_POINT ( 'NONE',  ( 12.79289321881336861, 0.7592924766157086447, 5.000000000000000000 ) ) ;
#87279 = VECTOR ( 'NONE', #42128, 1000.000000000000000 ) ;
#87280 =( BOUNDED_CURVE ( )  B_SPLINE_CURVE ( 3, ( #37710, #26806, #15883, #60172 ),
 .UNSPECIFIED., .F., .F. ) 
 B_SPLINE_CURVE_WITH_KNOTS ( ( 4, 4 ),
 ( 4.257860004652494368, 4.307247239014357021 ),
 .UNSPECIFIED. ) 
 CURVE ( )  GEOMETRIC_REPRESENTATION_ITEM ( )  RATIONAL_B_SPLINE_CURVE ( ( 1.000000000000000000, 0.9997967520851089862, 0.9997967520851089862, 1.000000000000000000 ) ) 
 REPRESENTATION_ITEM ( '' )  );
#87281 = FACE_OUTER_BOUND ( 'NONE', #76306, .T. ) ;
#87282 = VECTOR ( 'NONE', #22346, 1000.000000000000000 ) ;
#87283 = EDGE_CURVE ( 'NONE', #44324, #109623, #90000, .T. ) ;
#87284 = FACE_BOUND ( 'NONE', #35163, .T. ) ;
#87285 = LINE ( 'NONE', #73557, #45619 ) ;
#87286 = CARTESIAN_POINT ( 'NONE',  ( -53.99451991528749062, 28.92564299267975869, 4.000000000000000000 ) ) ;
#87287 = CARTESIAN_POINT ( 'NONE',  ( -11.93988928955972639, -9.740707523384184441, 10.89222023123383565 ) ) ;
#87289 = ORIENTED_EDGE ( 'NONE', *, *, #87684, .T. ) ;
#87288 = DIRECTION ( 'NONE',  ( -0.7071067811865486830, 0.7071067811865464625, 0.000000000000000000 ) ) ;
#87290 = DIRECTION ( 'NONE',  ( -0.7071067811865487940, 0.7071067811865463515, -0.000000000000000000 ) ) ;
#87292 = ORIENTED_EDGE ( 'NONE', *, *, #6728, .F. ) ;
#87291 = AXIS2_PLACEMENT_3D ( 'NONE', #110277, #123347, #55218 ) ;
#87293 = ORIENTED_EDGE ( 'NONE', *, *, #19322, .F. ) ;
#87294 = CARTESIAN_POINT ( 'NONE',  ( 83.91209685856479439, 5.291415217122921177, -3.054999999999994831 ) ) ;
#87295 = ORIENTED_EDGE ( 'NONE', *, *, #22055, .F. ) ;
#87296 = DIRECTION ( 'NONE',  ( -0.7071067811865487940, 0.7071067811865463515, -0.000000000000000000 ) ) ;
#87297 = VECTOR ( 'NONE', #94566, 1000.000000000000227 ) ;
#87298 = LINE ( 'NONE', #30789, #139285 ) ;
#87299 = ORIENTED_EDGE ( 'NONE', *, *, #67268, .F. ) ;
#87300 = DIRECTION ( 'NONE',  ( -1.000000000000000000, -0.000000000000000000, -0.000000000000000000 ) ) ;
#87301 = EDGE_CURVE ( 'NONE', #40245, #4422, #54138, .T. ) ;
#87302 = CARTESIAN_POINT ( 'NONE',  ( 34.92499999999998295, 12.00612307739183571, 4.000000000000000000 ) ) ;
#87303 = DIRECTION ( 'NONE',  ( -0.6830127018922181881, 0.6830127018922202975, -0.2588190451025214056 ) ) ;
#87304 = EDGE_CURVE ( 'NONE', #98171, #482, #10989, .T. ) ;
#87305 = PLANE ( 'NONE',  #110231 ) ;
#87306 = LINE ( 'NONE', #32212, #27345 ) ;
#87307 = DIRECTION ( 'NONE',  ( 0.7071067811865487940, -0.7071067811865463515, 0.000000000000000000 ) ) ;
#87308 = CARTESIAN_POINT ( 'NONE',  ( 4.499999999999968914, -16.91253812416058722, 4.000000000000000000 ) ) ;
#87309 = CARTESIAN_POINT ( 'NONE',  ( -30.48921356237309510, -27.52281430457076894, 5.000000000000000000 ) ) ;
#87310 = ORIENTED_EDGE ( 'NONE', *, *, #21404, .T. ) ;
#87311 = DIRECTION ( 'NONE',  ( 0.7071067811865487940, 0.7071067811865463515, -0.000000000000000000 ) ) ;
#87312 = ORIENTED_EDGE ( 'NONE', *, *, #130232, .T. ) ;
#87313 = DIRECTION ( 'NONE',  ( 0.7071067811865486830, -0.7071067811865464625, -0.000000000000000000 ) ) ;
#87314 = CARTESIAN_POINT ( 'NONE',  ( 36.29974487139159578, -27.71228299555231445, 4.000000000000000000 ) ) ;
#87315 = ORIENTED_EDGE ( 'NONE', *, *, #53172, .F. ) ;
#87317 = ORIENTED_EDGE ( 'NONE', *, *, #28333, .T. ) ;
#87316 = VECTOR ( 'NONE', #84769, 1000.000000000000000 ) ;
#87318 = EDGE_CURVE ( 'NONE', #133992, #23088, #122633, .T. ) ;
#87319 = CARTESIAN_POINT ( 'NONE',  ( 37.77126352523143993, 4.472830434245838482, 4.472830434245842035 ) ) ;
#87320 = ORIENTED_EDGE ( 'NONE', *, *, #109756, .F. ) ;
#87321 = DIRECTION ( 'NONE',  ( 0.3543493200069163795, -9.265275131829747941E-33, -0.9351131265310288487 ) ) ;
#87322 = VECTOR ( 'NONE', #8687, 1000.000000000000000 ) ;
#87324 = VECTOR ( 'NONE', #128645, 1000.000000000000000 ) ;
#87323 = PRODUCT_DEFINITION ( 'UNKNOWN', '', #12352, #25568 ) ;
#87325 = LINE ( 'NONE', #45279, #37731 ) ;
#87326 = AXIS2_PLACEMENT_3D ( 'NONE', #55888, #109526, #76195 ) ;
#87327 = CARTESIAN_POINT ( 'NONE',  ( 21.04580628287044064, 5.278424836066143655, -3.047499999999997655 ) ) ;
#87328 = CARTESIAN_POINT ( 'NONE',  ( 6.656140668332151122, 11.28355271028802065, -26.16006910964023291 ) ) ;
#87329 = ORIENTED_EDGE ( 'NONE', *, *, #44624, .F. ) ;
#87330 = DIRECTION ( 'NONE',  ( -0.5735764363510499342, -0.8191520442889891340, 0.000000000000000000 ) ) ;
#87331 = VECTOR ( 'NONE', #35329, 1000.000000000000000 ) ;
#87332 = ORIENTED_EDGE ( 'NONE', *, *, #50931, .F. ) ;
#87333 = SURFACE_STYLE_FILL_AREA ( #143128 ) ;
#87334 = CIRCLE ( 'NONE', #103454, 17.46000000000000085 ) ;
#87335 = CARTESIAN_POINT ( 'NONE',  ( -66.18398860626901126, 28.73617430169833753, 5.000000000000000000 ) ) ;
#87337 = ORIENTED_EDGE ( 'NONE', *, *, #135121, .T. ) ;
#87336 = FACE_OUTER_BOUND ( 'NONE', #4846, .T. ) ;
#87338 = ORIENTED_EDGE ( 'NONE', *, *, #18086, .F. ) ;
#87339 = CARTESIAN_POINT ( 'NONE',  ( -21.29974487139158512, -27.71228299555221142, 4.000000000000000000 ) ) ;
#87340 = DIRECTION ( 'NONE',  ( 0.000000000000000000, 0.000000000000000000, 1.000000000000000000 ) ) ;
#87341 = DIRECTION ( 'NONE',  ( 0.7071067811865486830, -0.7071067811865464625, -0.000000000000000000 ) ) ;
#87342 = ORIENTED_EDGE ( 'NONE', *, *, #2969, .F. ) ;
#87343 = CARTESIAN_POINT ( 'NONE',  ( -39.48921356237310221, -27.52281430457082934, 5.000000000000000000 ) ) ;
#87344 = ORIENTED_EDGE ( 'NONE', *, *, #15620, .T. ) ;
#87345 = ORIENTED_EDGE ( 'NONE', *, *, #105372, .T. ) ;
#87346 = ORIENTED_EDGE ( 'NONE', *, *, #73257, .T. ) ;
#87347 = CARTESIAN_POINT ( 'NONE',  ( 32.99999999999976552, 10.21212019023812623, -2.019456568337874458 ) ) ;
#87348 = CARTESIAN_POINT ( 'NONE',  ( 8.292893218813398803, -15.74070752338412049, 5.000000000000000000 ) ) ;
#87349 = CARTESIAN_POINT ( 'NONE',  ( -19.05000000000000071, 3.174999999999997158, 5.000000000000000000 ) ) ;
#87350 = CARTESIAN_POINT ( 'NONE',  ( -57.18398860626899705, 28.73617430169827358, 5.000000000000000000 ) ) ;
#87351 = CARTESIAN_POINT ( 'NONE',  ( -57.18398860626899705, 28.73617430169827358, 5.000000000000000000 ) ) ;
#87352 = DIRECTION ( 'NONE',  ( 0.7071067811865487940, 0.7071067811865463515, 0.000000000000000000 ) ) ;
#87353 = CARTESIAN_POINT ( 'NONE',  ( -34.92500000000001137, 19.70193056682081334, 4.500000000000000888 ) ) ;
#87354 = ORIENTED_EDGE ( 'NONE', *, *, #18444, .T. ) ;
#87355 = DIRECTION ( 'NONE',  ( -1.000000000000000000, -3.115803279706882722E-16, -0.000000000000000000 ) ) ;
#87356 = ORIENTED_EDGE ( 'NONE', *, *, #11999, .F. ) ;
#87357 = AXIS2_PLACEMENT_3D ( 'NONE', #68978, #12420, #133509 ) ;
#87358 = CARTESIAN_POINT ( 'NONE',  ( -5.510786437626906675, -27.52281430457051314, 5.000000000000000000 ) ) ;
#87359 = DIRECTION ( 'NONE',  ( -0.7071067811865486830, -0.7071067811865464625, -0.000000000000000000 ) ) ;
#87360 = EDGE_CURVE ( 'NONE', #128126, #46491, #31403, .T. ) ;
#87361 = VECTOR ( 'NONE', #7068, 1000.000000000000000 ) ;
#87362 = ORIENTED_EDGE ( 'NONE', *, *, #85097, .T. ) ;
#87363 = CARTESIAN_POINT ( 'NONE',  ( 21.18398860626899349, 28.73617430169802134, 5.000000000000000000 ) ) ;
#87364 = DIRECTION ( 'NONE',  ( 0.7071067811865487940, 0.7071067811865463515, -0.000000000000000000 ) ) ;
#87365 = PLANE ( 'NONE',  #28195 ) ;
#87366 = VERTEX_POINT ( 'NONE', #33528 ) ;
#87367 = EDGE_CURVE ( 'NONE', #63264, #124966, #34218, .T. ) ;
#87368 = EDGE_LOOP ( 'NONE', ( #85465, #141137, #38396, #16636 ) ) ;
#87369 = SURFACE_STYLE_USAGE ( .BOTH. , #98246 ) ;
#87370 = DIRECTION ( 'NONE',  ( 0.7071067811865487940, 0.7071067811865463515, 0.000000000000000000 ) ) ;
#87371 = ADVANCED_FACE ( 'NONE', ( #134248 ), #134984, .T. ) ;
#87372 = CYLINDRICAL_SURFACE ( 'NONE', #125713, 2.500000000000000000 ) ;
#87373 = CARTESIAN_POINT ( 'NONE',  ( 11.29289321881338282, 11.25929247661560773, 5.000000000000000000 ) ) ;
#87374 = CARTESIAN_POINT ( 'NONE',  ( -60.18398860626900415, 28.73617430169829490, 5.000000000000000000 ) ) ;
#87375 = EDGE_CURVE ( 'NONE', #22559, #122500, #125513, .T. ) ;
#87376 = CARTESIAN_POINT ( 'NONE',  ( 68.30793019189809456, -6.109999999999999432, 1.637169565754158507 ) ) ;
#87377 = DIRECTION ( 'NONE',  ( -1.000000000000000000, 0.000000000000000000, -0.000000000000000000 ) ) ;
#87378 = DIRECTION ( 'NONE',  ( -0.000000000000000000, -0.3543493200069152693, 0.9351131265310292928 ) ) ;
#87379 = CARTESIAN_POINT ( 'NONE',  ( 27.18398860626900060, 28.73617430169806042, 5.000000000000000000 ) ) ;
#87380 = CARTESIAN_POINT ( 'NONE',  ( 22.49999999999984368, -20.53675388469228480, 2.352720554255944840 ) ) ;
#87381 = ORIENTED_EDGE ( 'NONE', *, *, #102065, .T. ) ;
#87382 = FACE_OUTER_BOUND ( 'NONE', #136601, .T. ) ;
#87383 = COLOUR_RGB ( '', 0.40784314, 0.44705882, 0.49803922) ;
#87384 = VERTEX_POINT ( 'NONE', #94288 ) ;
#87385 = CARTESIAN_POINT ( 'NONE',  ( 17.99999999999987566, -2.904428200921286951, -6.989807076074982639 ) ) ;
#87386 = DIRECTION ( 'NONE',  ( -0.3543493200069162685, -0.000000000000000000, -0.9351131265310288487 ) ) ;
#87387 = ORIENTED_EDGE ( 'NONE', *, *, #115981, .T. ) ;
#87388 = CARTESIAN_POINT ( 'NONE',  ( -45.18398860626900415, 28.73617430169818832, 5.000000000000000000 ) ) ;
#87390 = ORIENTED_EDGE ( 'NONE', *, *, #68662, .F. ) ;
#87389 = DIRECTION ( 'NONE',  ( -0.7071067811865486830, -0.7071067811865464625, 0.000000000000000000 ) ) ;
#87391 = EDGE_CURVE ( 'NONE', #96831, #64517, #28657, .T. ) ;
#87392 = LINE ( 'NONE', #23547, #92502 ) ;
#87393 = AXIS2_PLACEMENT_3D ( 'NONE', #104931, #94051, #127393 ) ;
#87394 = EDGE_CURVE ( 'NONE', #93361, #927, #15979, .T. ) ;
#87395 = CARTESIAN_POINT ( 'NONE',  ( -9.516654386410381861, 22.22500000000000142, 4.500000000000000888 ) ) ;
#87396 = CARTESIAN_POINT ( 'NONE',  ( -48.48921356237309510, -27.52281430457089328, 5.000000000000000000 ) ) ;
#87397 = VERTEX_POINT ( 'NONE', #37057 ) ;
#87398 = VERTEX_POINT ( 'NONE', #39212 ) ;
#87399 = LINE ( 'NONE', #66364, #28140 ) ;
#87400 = DIRECTION ( 'NONE',  ( 0.7071067811865487940, -0.7071067811865463515, 0.000000000000000000 ) ) ;
#87401 = DIRECTION ( 'NONE',  ( 0.000000000000000000, -1.000000000000000000, 0.000000000000000000 ) ) ;
#87402 = EDGE_CURVE ( 'NONE', #123992, #62221, #71862, .T. ) ;
#87403 = CARTESIAN_POINT ( 'NONE',  ( 16.23330628287043353, -6.094999999999989981, -1.633150327867689322 ) ) ;
#87404 = CARTESIAN_POINT ( 'NONE',  ( 84.95419371712955581, 6.884901960086283523, 3.975000000000002753 ) ) ;
#87405 = DIRECTION ( 'NONE',  ( -0.3543493200069162685, -0.000000000000000000, -0.9351131265310288487 ) ) ;
#87406 = CARTESIAN_POINT ( 'NONE',  ( -30.70710678118633297, 20.25929247661551713, 5.000000000000000000 ) ) ;
#87407 = EDGE_LOOP ( 'NONE', ( #53603, #19688, #73274, #91611 ) ) ;
#87408 = AXIS2_PLACEMENT_3D ( 'NONE', #23246, #46509, #67523 ) ;
#87409 = MECHANICAL_DESIGN_GEOMETRIC_PRESENTATION_REPRESENTATION (  '', ( #131377 ), #82743 ) ;
#87410 = CARTESIAN_POINT ( 'NONE',  ( 87.04166666666665719, -3.975000000000002753, 6.884901960086286188 ) ) ;
#87411 = DIRECTION ( 'NONE',  ( -1.000000000000000000, -1.224606353822377258E-16, -0.000000000000000000 ) ) ;
#87412 = DIRECTION ( 'NONE',  ( 0.7071067811865487940, 0.7071067811865463515, -0.000000000000000000 ) ) ;
#87413 = EDGE_CURVE ( 'NONE', #142592, #90987, #126218, .T. ) ;
#87414 = VERTEX_POINT ( 'NONE', #137094 ) ;
#87415 = CARTESIAN_POINT ( 'NONE',  ( 39.48921356237310221, -27.52281430457082934, 5.000000000000000000 ) ) ;
#87416 = ORIENTED_EDGE ( 'NONE', *, *, #44311, .F. ) ;
#87417 = AXIS2_PLACEMENT_3D ( 'NONE', #117664, #18350, #74208 ) ;
#87418 = CARTESIAN_POINT ( 'NONE',  ( 74.22959685856476142, -6.110000000000000320, -1.637169565754161393 ) ) ;
#87419 = CARTESIAN_POINT ( 'NONE',  ( 75.18398860626899705, 28.73617430169839793, 5.000000000000000000 ) ) ;
#87420 = ADVANCED_FACE ( 'NONE', ( #70460 ), #70395, .T. ) ;
#87421 = ORIENTED_EDGE ( 'NONE', *, *, #45790, .F. ) ;
#87422 = CARTESIAN_POINT ( 'NONE',  ( 34.92499999999998295, -2.337538124160962738, 4.000000000000000000 ) ) ;
#87423 = CIRCLE ( 'NONE', #6644, 2.500000000000000888 ) ;
#87424 = CARTESIAN_POINT ( 'NONE',  ( -34.92500000000001137, -22.22500000000000142, 4.000000000000000000 ) ) ;
#87425 = DIRECTION ( 'NONE',  ( -0.7071067811865486830, -0.7071067811865464625, 0.000000000000000000 ) ) ;
#87426 = VECTOR ( 'NONE', #67889, 1000.000000000000000 ) ;
#87427 = CARTESIAN_POINT ( 'NONE',  ( -27.48921356237309155, -27.52281430457074762, 5.000000000000000000 ) ) ;
#87428 = CARTESIAN_POINT ( 'NONE',  ( 20.66840764549667497, -2.499999999999996003, 0.000000000000000000 ) ) ;
#87430 = ORIENTED_EDGE ( 'NONE', *, *, #33628, .T. ) ;
#87429 = PLANE ( 'NONE',  #5806 ) ;
#87431 =( REPRESENTATION_RELATIONSHIP ('NONE','NONE', #69070, #40289 ) REPRESENTATION_RELATIONSHIP_WITH_TRANSFORMATION ( #138099 )SHAPE_REPRESENTATION_RELATIONSHIP( ) );
#87432 =( LENGTH_UNIT ( ) NAMED_UNIT ( * ) SI_UNIT ( .MILLI., .METRE. ) );
#87433 = DIRECTION ( 'NONE',  ( 0.7071067811865487940, -0.7071067811865463515, 0.000000000000000000 ) ) ;
#87434 = CARTESIAN_POINT ( 'NONE',  ( 76.68749999999998579, -5.819803920172573974, 5.819803920172573086 ) ) ;
#87435 = VECTOR ( 'NONE', #9414, 1000.000000000000000 ) ;
#87436 = FACE_OUTER_BOUND ( 'NONE', #27775, .T. ) ;
#87437 = MECHANICAL_DESIGN_GEOMETRIC_PRESENTATION_REPRESENTATION (  '', ( #131410 ), #112970 ) ;
#87438 = ORIENTED_EDGE ( 'NONE', *, *, #27291, .T. ) ;
#87439 = EDGE_CURVE ( 'NONE', #119594, #13220, #51525, .T. ) ;
#87440 = VERTEX_POINT ( 'NONE', #119587 ) ;
#87441 = VECTOR ( 'NONE', #140541, 1000.000000000000000 ) ;
#87442 = CARTESIAN_POINT ( 'NONE',  ( 66.06293019189810423, 1.637169565754157174, 6.110000000000002984 ) ) ;
#87443 = ORIENTED_EDGE ( 'NONE', *, *, #112350, .T. ) ;
#87444 = DIRECTION ( 'NONE',  ( -1.000000000000000000, 0.000000000000000000, 0.000000000000000000 ) ) ;
#87445 = PLANE ( 'NONE',  #10952 ) ;
#87447 = AXIS2_PLACEMENT_3D ( 'NONE', #36100, #141455, #2719 ) ;
#87446 = DIRECTION ( 'NONE',  ( 0.7071067811865486830, -0.7071067811865464625, -0.000000000000000000 ) ) ;
#87448 = FACE_OUTER_BOUND ( 'NONE', #123749, .T. ) ;
#87449 = VERTEX_POINT ( 'NONE', #73979 ) ;
#87450 = EDGE_LOOP ( 'NONE', ( #113002, #134496, #38593, #103307 ) ) ;
#87451 = FACE_OUTER_BOUND ( 'NONE', #70000, .T. ) ;
#87452 = CARTESIAN_POINT ( 'NONE',  ( -48.29974487139158867, -27.71228299555239971, 4.000000000000000000 ) ) ;
#87453 = EDGE_LOOP ( 'NONE', ( #116714, #93576, #97516, #27638 ) ) ;
#87454 = EDGE_CURVE ( 'NONE', #133840, #67716, #40646, .T. ) ;
#87455 = CARTESIAN_POINT ( 'NONE',  ( -29.91685193227051087, 21.75929247661549581, 7.311836541447982007 ) ) ;
#87456 = CARTESIAN_POINT ( 'NONE',  ( 1.249915201643648111, -0.3999999999999997446, -2.317232462839658780 ) ) ;
#87457 = DIRECTION ( 'NONE',  ( -0.7071067811865486830, -0.7071067811865464625, 0.000000000000000000 ) ) ;
#87458 = VERTEX_POINT ( 'NONE', #118896 ) ;
#87459 = EDGE_CURVE ( 'NONE', #65140, #113212, #141368, .T. ) ;
#87460 = CARTESIAN_POINT ( 'NONE',  ( 54.18398860626899705, 28.73617430169825226, 5.000000000000000000 ) ) ;
#87461 = CARTESIAN_POINT ( 'NONE',  ( 181.0878408821075709, -48.47815212813055297, 38.14157743968410585 ) ) ;
#87462 = DIRECTION ( 'NONE',  ( -0.000000000000000000, -0.3543493200069152693, 0.9351131265310292928 ) ) ;
#87463 = DIRECTION ( 'NONE',  ( -0.000000000000000000, 0.000000000000000000, 1.000000000000000000 ) ) ;
#87464 = VECTOR ( 'NONE', #123697, 1000.000000000000000 ) ;
#87465 = PRESENTATION_STYLE_ASSIGNMENT (( #133126 ) ) ;
#87466 =( BOUNDED_CURVE ( )  B_SPLINE_CURVE ( 2, ( #7699, #85261, #41783, #118612, #41061, #138965, #28051, #104887, #130231, #5554, #39663, #38924, #50516 ),
 .UNSPECIFIED., .F., .T. ) 
 B_SPLINE_CURVE_WITH_KNOTS ( ( 3, 2, 2, 2, 2, 2, 3 ),
 ( 0.6333333333333333037, 0.6361111111111110716, 0.6388888888888888395, 0.6416666666666667185, 0.6444444444444444864, 0.6472222222222222543, 0.6500000000000000222 ),
 .UNSPECIFIED. ) 
 CURVE ( )  GEOMETRIC_REPRESENTATION_ITEM ( )  RATIONAL_B_SPLINE_CURVE ( ( 1.000000000000000000, 0.9659258262890683122, 1.000000000000000000, 0.9659258262890683122, 1.000000000000000000, 0.9659258262890683122, 1.000000000000000000, 0.9659258262890683122, 1.000000000000000000, 0.9659258262890683122, 1.000000000000000000, 0.9659258262890683122, 1.000000000000000000 ) ) 
 REPRESENTATION_ITEM ( '' )  );
#87467 = FACE_OUTER_BOUND ( 'NONE', #89609, .T. ) ;
#87468 = ORIENTED_EDGE ( 'NONE', *, *, #58486, .F. ) ;
#87469 = ORIENTED_EDGE ( 'NONE', *, *, #111575, .T. ) ;
#87470 = CARTESIAN_POINT ( 'NONE',  ( 111.7662635252314516, 4.472830434245838482, -4.472830434245837594 ) ) ;
#87471 = ORIENTED_EDGE ( 'NONE', *, *, #46477, .F. ) ;
#87472 = ORIENTED_EDGE ( 'NONE', *, *, #137953, .F. ) ;
#87473 = SURFACE_STYLE_USAGE ( .BOTH. , #96864 ) ;
#87474 = DIRECTION ( 'NONE',  ( -0.000000000000000000, -0.000000000000000000, 1.000000000000000000 ) ) ;
#87475 = CARTESIAN_POINT ( 'NONE',  ( 3.005480084712505828, 28.92564299267936079, 4.000000000000000000 ) ) ;
#87476 = EDGE_LOOP ( 'NONE', ( #61734, #55925, #112309, #89918 ) ) ;
#87477 = LINE ( 'NONE', #52685, #133973 ) ;
#87478 = DIRECTION ( 'NONE',  ( -0.000000000000000000, 0.3543493200069153248, 0.9351131265310292928 ) ) ;
#87479 = EDGE_CURVE ( 'NONE', #86941, #92661, #86294, .T. ) ;
#87480 = FACE_OUTER_BOUND ( 'NONE', #67946, .T. ) ;
#87481 = PLANE ( 'NONE',  #99371 ) ;
#87482 = DIRECTION ( 'NONE',  ( 0.7071067811865487940, 0.7071067811865463515, 0.000000000000000000 ) ) ;
#87483 = ORIENTED_EDGE ( 'NONE', *, *, #35728, .T. ) ;
#87484 = CARTESIAN_POINT ( 'NONE',  ( 32.99999999999977263, 16.93112307739201228, 4.000000000000000000 ) ) ;
#87485 = CARTESIAN_POINT ( 'NONE',  ( 65.99451991528749772, 28.92564299267984396, 4.000000000000000000 ) ) ;
#87486 = ORIENTED_EDGE ( 'NONE', *, *, #10259, .T. ) ;
#87487 = EDGE_CURVE ( 'NONE', #114269, #27583, #140642, .T. ) ;
#87488 = ORIENTED_EDGE ( 'NONE', *, *, #21551, .F. ) ;
#87489 = EDGE_CURVE ( 'NONE', #962, #45746, #7976, .T. ) ;
#87490 = ORIENTED_EDGE ( 'NONE', *, *, #106144, .F. ) ;
#87491 = CARTESIAN_POINT ( 'NONE',  ( 65.91709685856477563, 3.054999999999998828, 5.291415217122922066 ) ) ;
#87492 = EDGE_LOOP ( 'NONE', ( #141138, #87870, #34250, #94658 ) ) ;
#87493 = CARTESIAN_POINT ( 'NONE',  ( -7.940000000000007496, -39.92999999999999261, -10.00000000000000178 ) ) ;
#87494 = CARTESIAN_POINT ( 'NONE',  ( -63.18398860626900415, 28.73617430169831621, 5.000000000000000000 ) ) ;
#87495 = VECTOR ( 'NONE', #92080, 1000.000000000000000 ) ;
#87496 = CARTESIAN_POINT ( 'NONE',  ( 96.10459685856477563, 1.637169565754164946, -6.109999999999999432 ) ) ;
#87497 = CARTESIAN_POINT ( 'NONE',  ( 11.67183060077639212, -6.740707523384212863, 4.000000000000000000 ) ) ;
#87498 = LINE ( 'NONE', #53432, #109070 ) ;
#87499 = ORIENTED_EDGE ( 'NONE', *, *, #85453, .F. ) ;
#87500 = DIRECTION ( 'NONE',  ( 0.000000000000000000, -1.000000000000000000, 0.000000000000000000 ) ) ;
#87501 = DIRECTION ( 'NONE',  ( 0.7071067811865487940, 0.7071067811865463515, -0.000000000000000000 ) ) ;
#87502 = ADVANCED_FACE ( 'NONE', ( #10136 ), #73281, .F. ) ;
#87503 = CARTESIAN_POINT ( 'NONE',  ( 34.49999999999975131, -14.70932175296474398, -11.46312253303845274 ) ) ;
#87504 = DIRECTION ( 'NONE',  ( -0.7071067811865486830, -0.7071067811865464625, -0.000000000000000000 ) ) ;
#87505 = ORIENTED_EDGE ( 'NONE', *, *, #137949, .F. ) ;
#87506 = AXIS2_PLACEMENT_3D ( 'NONE', #108213, #34271, #109681 ) ;
#87507 = LINE ( 'NONE', #53442, #13602 ) ;
#87508 = ORIENTED_EDGE ( 'NONE', *, *, #25530, .F. ) ;
#87509 = ORIENTED_EDGE ( 'NONE', *, *, #45082, .F. ) ;
#87510 = ORIENTED_EDGE ( 'NONE', *, *, #142037, .F. ) ;
#87511 = CARTESIAN_POINT ( 'NONE',  ( 120.8079301918980946, -6.109999999999998543, 1.637169565754158507 ) ) ;
#87512 = EDGE_LOOP ( 'NONE', ( #43283, #57782, #101631, #1590 ) ) ;
#87513 = VECTOR ( 'NONE', #16329, 1000.000000000000000 ) ;
#87514 = DIRECTION ( 'NONE',  ( -0.7071067811865486830, -0.7071067811865464625, 0.000000000000000000 ) ) ;
#87515 = VECTOR ( 'NONE', #83565, 1000.000000000000000 ) ;
#87516 = FACE_OUTER_BOUND ( 'NONE', #15244, .T. ) ;
#87517 = VERTEX_POINT ( 'NONE', #8663 ) ;
#87518 = CARTESIAN_POINT ( 'NONE',  ( 10.98012225071445869, -17.24070752338409918, 20.23474786156471694 ) ) ;
#87519 = ORIENTED_EDGE ( 'NONE', *, *, #78858, .F. ) ;
#87520 = VECTOR ( 'NONE', #41115, 1000.000000000000000 ) ;
#87521 = VECTOR ( 'NONE', #102110, 1000.000000000000000 ) ;
#87522 = CARTESIAN_POINT ( 'NONE',  ( 12.81206980810188512, 7.934999999999993392, 2.126176841940951689 ) ) ;
#87523 = EDGE_CURVE ( 'NONE', #141614, #18270, #64523, .T. ) ;
#87524 = CARTESIAN_POINT ( 'NONE',  ( -8.999999999999937828, 9.631307414974314085, -9.079085613539563226 ) ) ;
#87525 = CARTESIAN_POINT ( 'NONE',  ( 38.04166666666665719, -3.975000000000002753, 6.884901960086286188 ) ) ;
#87526 = ORIENTED_EDGE ( 'NONE', *, *, #60227, .F. ) ;
#87527 = EDGE_CURVE ( 'NONE', #14243, #135923, #52900, .T. ) ;
#87528 = ORIENTED_EDGE ( 'NONE', *, *, #26830, .T. ) ;
#87529 = ORIENTED_EDGE ( 'NONE', *, *, #17027, .T. ) ;
#87530 = FACE_OUTER_BOUND ( 'NONE', #21023, .T. ) ;
#87531 = DIRECTION ( 'NONE',  ( 0.000000000000000000, 0.000000000000000000, -1.000000000000000000 ) ) ;
#87532 = PLANE ( 'NONE',  #31133 ) ;
#87533 = CARTESIAN_POINT ( 'NONE',  ( 30.29974487139158867, -27.71228299555227537, 4.000000000000000000 ) ) ;
#87534 = EDGE_CURVE ( 'NONE', #89571, #37298, #108701, .T. ) ;
#87535 = EDGE_CURVE ( 'NONE', #140583, #125898, #97871, .T. ) ;
#87536 = CARTESIAN_POINT ( 'NONE',  ( 29.99999999999981171, -19.44781430457063465, 5.000000000000000000 ) ) ;
#87537 = CARTESIAN_POINT ( 'NONE',  ( 31.50043019189810423, -3.055000000000002380, 5.291415217122920289 ) ) ;
#87538 = DIRECTION ( 'NONE',  ( 0.7071067811865487940, 0.7071067811865463515, -0.000000000000000000 ) ) ;
#87539 = CARTESIAN_POINT ( 'NONE',  ( -34.92500000000001847, -1.487538124160473707, 4.000000000000000000 ) ) ;
#87540 = ORIENTED_EDGE ( 'NONE', *, *, #138891, .T. ) ;
#87541 = DIRECTION ( 'NONE',  ( -1.000000000000000000, -1.224606353822377258E-16, -0.000000000000000000 ) ) ;
#87542 = VERTEX_POINT ( 'NONE', #86989 ) ;
#87543 = PLANE ( 'NONE',  #15184 ) ;
#87544 = ORIENTED_EDGE ( 'NONE', *, *, #5384, .F. ) ;
#87545 = VECTOR ( 'NONE', #127856, 1000.000000000000000 ) ;
#87546 = CARTESIAN_POINT ( 'NONE',  ( 18.42080628287044064, 3.047499999999997655, 5.278424836066143655 ) ) ;
#87548 = ORIENTED_EDGE ( 'NONE', *, *, #91387, .F. ) ;
#87547 = PLANE ( 'NONE',  #37205 ) ;
#87549 = ADVANCED_FACE ( 'NONE', ( #9386 ), #53666, .F. ) ;
#87550 = ADVANCED_FACE ( 'NONE', ( #21005 ), #109453, .T. ) ;
#87551 = CARTESIAN_POINT ( 'NONE',  ( 17.99999999999988987, 14.58746187583909126, 4.000000000000000000 ) ) ;
#87552 = EDGE_LOOP ( 'NONE', ( #37811, #31297, #139776, #72876 ) ) ;
#87554 = VECTOR ( 'NONE', #76079, 1000.000000000000227 ) ;
#87553 = CARTESIAN_POINT ( 'NONE',  ( -23.99451991528749062, 28.92564299267954908, 4.000000000000000000 ) ) ;
#87555 = ORIENTED_EDGE ( 'NONE', *, *, #50001, .F. ) ;
#87556 = DIRECTION ( 'NONE',  ( -0.6830127018922181881, 0.6830127018922202975, -0.2588190451025214056 ) ) ;
#87557 = ORIENTED_EDGE ( 'NONE', *, *, #26978, .F. ) ;
#87558 = DIRECTION ( 'NONE',  ( 0.000000000000000000, 0.000000000000000000, -1.000000000000000000 ) ) ;
#87559 = CARTESIAN_POINT ( 'NONE',  ( 111.7875270504628986, 0.000000000000000000, -7.949999999999998401 ) ) ;
#87560 = PLANE ( 'NONE',  #143395 ) ;
#87561 = EDGE_CURVE ( 'NONE', #39257, #68534, #142798, .T. ) ;
#87562 = CARTESIAN_POINT ( 'NONE',  ( 63.48921356237309510, -27.52281430457099631, 5.000000000000000000 ) ) ;
#87563 = PLANE ( 'NONE',  #72388 ) ;
#87564 = CARTESIAN_POINT ( 'NONE',  ( 11.72733514412567857, 2.500000000000003109, 3.061616997868386592E-16 ) ) ;
#87565 = CARTESIAN_POINT ( 'NONE',  ( 26.20710678118635784, 3.759292476615673007, 5.000000000000000000 ) ) ;
#87566 = CARTESIAN_POINT ( 'NONE',  ( 2.625000000000000000, 6.094999999999989981, -1.119633336120465690E-15 ) ) ;
#87567 = CARTESIAN_POINT ( 'NONE',  ( 21.12456980810188867, -6.871911579029512218, 3.967499999999996252 ) ) ;
#87568 = EDGE_CURVE ( 'NONE', #25152, #98769, #57251, .T. ) ;
#87569 = VECTOR ( 'NONE', #122415, 999.9999999999998863 ) ;
#87570 = DIRECTION ( 'NONE',  ( 0.7071067811865487940, 0.7071067811865463515, 0.000000000000000000 ) ) ;
#87571 = CYLINDRICAL_SURFACE ( 'NONE', #24713, 0.5000000000000004441 ) ;
#87572 = ORIENTED_EDGE ( 'NONE', *, *, #3165, .F. ) ;
#87573 = ORIENTED_EDGE ( 'NONE', *, *, #113853, .T. ) ;
#87574 = DIRECTION ( 'NONE',  ( -0.000000000000000000, 0.3543493200069152138, -0.9351131265310292928 ) ) ;
#87575 = ORIENTED_EDGE ( 'NONE', *, *, #116135, .F. ) ;
#87576 = CARTESIAN_POINT ( 'NONE',  ( 14.20710678118644843, 9.759292476615620160, 5.000000000000000000 ) ) ;
#87577 = ADVANCED_FACE ( 'NONE', ( #67407 ), #68147, .T. ) ;
#87578 = DIRECTION ( 'NONE',  ( 0.7071067811865486830, -0.7071067811865464625, -0.000000000000000000 ) ) ;
#87579 =( LENGTH_UNIT ( ) NAMED_UNIT ( * ) SI_UNIT ( .MILLI., .METRE. ) );
#87580 = VERTEX_POINT ( 'NONE', #21740 ) ;
#87581 = SURFACE_STYLE_FILL_AREA ( #27656 ) ;
#87582 = LINE ( 'NONE', #55686, #23264 ) ;
#87583 = CARTESIAN_POINT ( 'NONE',  ( 92.72916666666665719, 7.950000000000001954, -2.130196079827421762 ) ) ;
#87584 = CARTESIAN_POINT ( 'NONE',  ( 0.7586007421979610310, 21.72500000000000853, 5.000000000000000000 ) ) ;
#87585 = DIRECTION ( 'NONE',  ( 0.7071067811865486830, -0.7071067811865464625, -0.000000000000000000 ) ) ;
#87588 = VERTEX_POINT ( 'NONE', #132679 ) ;
#87587 = EDGE_CURVE ( 'NONE', #50406, #137620, #24579, .T. ) ;
#87586 = DIRECTION ( 'NONE',  ( 0.3543493200069163240, -0.000000000000000000, -0.9351131265310288487 ) ) ;
#87589 = LINE ( 'NONE', #63716, #106790 ) ;
#87590 = EDGE_CURVE ( 'NONE', #48371, #55182, #110148, .T. ) ;
#87591 = CARTESIAN_POINT ( 'NONE',  ( 70.41666666666665719, -6.884901960086287076, -3.975000000000000977 ) ) ;
#87592 = LINE ( 'NONE', #41956, #625 ) ;
#87593 = DIRECTION ( 'NONE',  ( -0.000000000000000000, 5.559056632600921604E-15, -1.000000000000000000 ) ) ;
#87594 = DIRECTION ( 'NONE',  ( -0.7071067811865487940, 0.7071067811865463515, -0.000000000000000000 ) ) ;
#87595 = ORIENTED_EDGE ( 'NONE', *, *, #125021, .F. ) ;
#87596 = EDGE_CURVE ( 'NONE', #91253, #51436, #43488, .T. ) ;
#87597 = ORIENTED_EDGE ( 'NONE', *, *, #40269, .T. ) ;
#87598 = VERTEX_POINT ( 'NONE', #134075 ) ;
#87599 = CARTESIAN_POINT ( 'NONE',  ( 90.12543019189811844, 5.291415217122919401, 3.055000000000002824 ) ) ;
#87600 = AXIS2_PLACEMENT_3D ( 'NONE', #10262, #95855, #53808 ) ;
#87601 = ORIENTED_EDGE ( 'NONE', *, *, #20375, .F. ) ;
#87602 = CARTESIAN_POINT ( 'NONE',  ( 127.4973405139117659, -50.37061236291226152, 37.32649486623495960 ) ) ;
#87603 = CARTESIAN_POINT ( 'NONE',  ( 84.22502705046288440, 5.819803920172573974, -5.819803920172573086 ) ) ;
#87604 = VERTEX_POINT ( 'NONE', #113007 ) ;
#87605 = CARTESIAN_POINT ( 'NONE',  ( 14.99999999999990230, -6.108550654416941228, -3.114665004254935088 ) ) ;
#87606 = CARTESIAN_POINT ( 'NONE',  ( -32.67183060077623935, 14.25929247661556865, 4.000000000000000000 ) ) ;
#87607 = CARTESIAN_POINT ( 'NONE',  ( 86.68293019189813720, -1.637169565754158951, -6.109999999999998543 ) ) ;
#87608 = EDGE_LOOP ( 'NONE', ( #130299, #18759, #112212, #14926 ) ) ;
#87609 = DIRECTION ( 'NONE',  ( 0.7071067811865487940, 0.7071067811865463515, -0.000000000000000000 ) ) ;
#87610 = DIRECTION ( 'NONE',  ( 0.7071067811865486830, -0.7071067811865464625, -0.000000000000000000 ) ) ;
#87611 = CIRCLE ( 'NONE', #59887, 2.500000000000000444 ) ;
#87612 = VECTOR ( 'NONE', #93044, 1000.000000000000227 ) ;
#87613 = EDGE_LOOP ( 'NONE', ( #40901, #18608, #82007, #41730, #45228, #36993 ) ) ;
#87614 = VERTEX_POINT ( 'NONE', #87702 ) ;
#87615 = CIRCLE ( 'NONE', #57528, 5.999999999999998224 ) ;
#87616 = ORIENTED_EDGE ( 'NONE', *, *, #135968, .T. ) ;
#87617 = DIRECTION ( 'NONE',  ( -0.7071067811865486830, -0.7071067811865464625, -0.000000000000000000 ) ) ;
#87618 = VECTOR ( 'NONE', #66508, 1000.000000000000000 ) ;
#87619 = DIRECTION ( 'NONE',  ( 0.7071067811865486830, -0.7071067811865464625, -0.000000000000000000 ) ) ;
#87620 = LINE ( 'NONE', #99928, #32666 ) ;
#87621 = VECTOR ( 'NONE', #141514, 1000.000000000000000 ) ;
#87622 = AXIS2_PLACEMENT_3D ( 'NONE', #70686, #114834, #15512 ) ;
#87623 = CARTESIAN_POINT ( 'NONE',  ( 162.1604124744595481, 26.96999999999993491, 34.79688855774463008 ) ) ;
#87624 = DIRECTION ( 'NONE',  ( -0.7071067811865486830, -0.7071067811865464625, 0.000000000000000000 ) ) ;
#87625 = SURFACE_SIDE_STYLE ('',( #110771 ) ) ;
#87626 = EDGE_LOOP ( 'NONE', ( #48523, #10045, #117170, #94066 ) ) ;
#87627 = ORIENTED_EDGE ( 'NONE', *, *, #116405, .T. ) ;
#87628 = LINE ( 'NONE', #9299, #110466 ) ;
#87630 = EDGE_CURVE ( 'NONE', #40076, #50446, #44224, .T. ) ;
#87629 = EDGE_LOOP ( 'NONE', ( #134718, #7088, #30034, #85430 ) ) ;
#87631 = ORIENTED_EDGE ( 'NONE', *, *, #56991, .F. ) ;
#87632 = VECTOR ( 'NONE', #77048, 1000.000000000000227 ) ;
#87633 = VECTOR ( 'NONE', #66533, 1000.000000000000000 ) ;
#87634 = CARTESIAN_POINT ( 'NONE',  ( -18.29974487139159223, -27.71228299555219010, 4.000000000000000000 ) ) ;
#87635 = ORIENTED_EDGE ( 'NONE', *, *, #9960, .F. ) ;
#87636 = DIRECTION ( 'NONE',  ( 0.000000000000000000, -1.000000000000000000, 0.000000000000000000 ) ) ;
#87637 = DIRECTION ( 'NONE',  ( 0.000000000000000000, -1.000000000000000000, 0.000000000000000000 ) ) ;
#87638 = DIRECTION ( 'NONE',  ( 0.7071067811865487940, -0.7071067811865463515, 0.000000000000000000 ) ) ;
#87639 = PLANE ( 'NONE',  #124758 ) ;
#87640 = VECTOR ( 'NONE', #55121, 1000.000000000000000 ) ;
#87641 = CARTESIAN_POINT ( 'NONE',  ( -26.99451991528749417, 28.92564299267956685, 4.000000000000000000 ) ) ;
#87642 = ORIENTED_EDGE ( 'NONE', *, *, #119286, .F. ) ;
#87643 = AXIS2_PLACEMENT_3D ( 'NONE', #104271, #81877, #60101 ) ;
#87644 = DIRECTION ( 'NONE',  ( -1.000000000000000000, -1.224606353822377258E-16, -0.000000000000000000 ) ) ;
#87645 = ORIENTED_EDGE ( 'NONE', *, *, #5726, .F. ) ;
#87646 = ADVANCED_FACE ( 'NONE', ( #13677 ), #32630, .F. ) ;
#87647 = CARTESIAN_POINT ( 'NONE',  ( -45.18398860626900415, 28.73617430169818832, 5.000000000000000000 ) ) ;
#87648 = VERTEX_POINT ( 'NONE', #11534 ) ;
#87649 = SURFACE_SIDE_STYLE ('',( #1327 ) ) ;
#87650 = ORIENTED_EDGE ( 'NONE', *, *, #129057, .T. ) ;
#87652 = EDGE_CURVE ( 'NONE', #48047, #93569, #57969, .T. ) ;
#87651 = DIRECTION ( 'NONE',  ( -0.000000000000000000, -0.3543493200069152693, 0.9351131265310292928 ) ) ;
#87653 = VERTEX_POINT ( 'NONE', #131940 ) ;
#87654 = VERTEX_POINT ( 'NONE', #46387 ) ;
#87655 = VECTOR ( 'NONE', #100049, 1000.000000000000000 ) ;
#87656 = EDGE_LOOP ( 'NONE', ( #69519, #1114, #98809, #34560 ) ) ;
#87657 = PLANE ( 'NONE',  #88264 ) ;
#87658 = DIRECTION ( 'NONE',  ( 1.000000000000000000, 0.000000000000000000, 0.000000000000000000 ) ) ;
#87659 = CARTESIAN_POINT ( 'NONE',  ( 19.99806943317887686, -22.22500000000000142, 4.500000000000000888 ) ) ;
#87660 = CARTESIAN_POINT ( 'NONE',  ( -34.92500000000001137, 1.821246448331360179, 12.73174495308782816 ) ) ;
#87661 = CARTESIAN_POINT ( 'NONE',  ( 123.6670968585647756, -3.055000000000000160, -5.291415217122921177 ) ) ;
#87662 = CARTESIAN_POINT ( 'NONE',  ( -21.75860074219781382, 21.72500000000000142, 5.000000000000000000 ) ) ;
#87663 = EDGE_CURVE ( 'NONE', #92828, #97144, #22417, .T. ) ;
#87664 = CARTESIAN_POINT ( 'NONE',  ( -65.99451991528749772, 28.92564299267984396, 4.000000000000000000 ) ) ;
#87665 = LINE ( 'NONE', #32585, #55178 ) ;
#87666 = AXIS2_PLACEMENT_3D ( 'NONE', #99629, #91630, #111214 ) ;
#87667 = PLANE ( 'NONE',  #123346 ) ;
#87668 = PRESENTATION_LAYER_ASSIGNMENT (  '', '', ( #115366 ) ) ;
#87669 = ADVANCED_FACE ( 'NONE', ( #23120 ), #133368, .F. ) ;
#87670 = CARTESIAN_POINT ( 'NONE',  ( 26.40000000000000568, -16.48000000000005016, -33.92499999999998295 ) ) ;
#87671 = DIRECTION ( 'NONE',  ( -0.000000000000000000, -0.000000000000000000, 1.000000000000000000 ) ) ;
#87672 = DIRECTION ( 'NONE',  ( -0.000000000000000000, 0.3543493200069153248, 0.9351131265310292928 ) ) ;
#87673 = ORIENTED_EDGE ( 'NONE', *, *, #59254, .T. ) ;
#87674 = ORIENTED_EDGE ( 'NONE', *, *, #20603, .T. ) ;
#87675 = ORIENTED_EDGE ( 'NONE', *, *, #126628, .F. ) ;
#87676 = LINE ( 'NONE', #101399, #44956 ) ;
#87677 = ADVANCED_FACE ( 'NONE', ( #45663 ), #12974, .F. ) ;
#87678 = ORIENTED_EDGE ( 'NONE', *, *, #61772, .T. ) ;
#87679 = EDGE_LOOP ( 'NONE', ( #26488, #54141, #20778, #77280 ) ) ;
#87680 = LINE ( 'NONE', #131910, #21305 ) ;
#87681 = LINE ( 'NONE', #112305, #85725 ) ;
#87682 = ORIENTED_EDGE ( 'NONE', *, *, #110730, .T. ) ;
#87683 = PLANE ( 'NONE',  #25571 ) ;
#87684 = EDGE_CURVE ( 'NONE', #41910, #59525, #143504, .T. ) ;
#87685 = VERTEX_POINT ( 'NONE', #110842 ) ;
#87686 = DIRECTION ( 'NONE',  ( -0.6830127018922180770, -0.6830127018922204085, -0.2588190451025213501 ) ) ;
#87687 = CARTESIAN_POINT ( 'NONE',  ( 24.18398860626899705, 28.73617430169804265, 5.000000000000000000 ) ) ;
#87688 = CARTESIAN_POINT ( 'NONE',  ( 23.54623647476855552, -7.934999999999990727, 4.858786175617117713E-16 ) ) ;
#87689 = ORIENTED_EDGE ( 'NONE', *, *, #103539, .F. ) ;
#87690 = CARTESIAN_POINT ( 'NONE',  ( 92.37043019189810877, -3.055000000000001936, 5.291415217122918513 ) ) ;
#87691 = CARTESIAN_POINT ( 'NONE',  ( 8.118486091812719962, -8.713627631029451592, -3.788380083765350737 ) ) ;
#87692 = CARTESIAN_POINT ( 'NONE',  ( 54.48921356237310221, -27.52281430457093236, 5.000000000000000000 ) ) ;
#87693 = CARTESIAN_POINT ( 'NONE',  ( 11.66989781452728359, 17.25929247661553845, 19.83885114516068526 ) ) ;
#87694 = VERTEX_POINT ( 'NONE', #34763 ) ;
#87695 = EDGE_CURVE ( 'NONE', #118868, #86890, #55815, .T. ) ;
#87696 = DIRECTION ( 'NONE',  ( -1.000000000000000000, -0.000000000000000000, -0.000000000000000000 ) ) ;
#87697 = ORIENTED_EDGE ( 'NONE', *, *, #87523, .T. ) ;
#87698 = ORIENTED_EDGE ( 'NONE', *, *, #57122, .F. ) ;
#87699 = CARTESIAN_POINT ( 'NONE',  ( -32.99999999999977263, 9.631307414974292769, -9.079085613539614741 ) ) ;
#87700 = DIRECTION ( 'NONE',  ( -0.7071067811865487940, 0.7071067811865463515, 0.000000000000000000 ) ) ;
#87701 = CARTESIAN_POINT ( 'NONE',  ( -15.79333936457836707, 21.75929247661549937, 4.998822639870700080 ) ) ;
#87702 = CARTESIAN_POINT ( 'NONE',  ( -12.70000000000000462, -22.33999999999998565, -0.5000000000000000000 ) ) ;
#87703 = VERTEX_POINT ( 'NONE', #56562 ) ;
#87704 = EDGE_CURVE ( 'NONE', #52437, #84626, #89831, .T. ) ;
#87705 = ADVANCED_FACE ( 'NONE', ( #90573 ), #134810, .T. ) ;
#87706 = LINE ( 'NONE', #31903, #57620 ) ;
#87707 = CARTESIAN_POINT ( 'NONE',  ( -28.49999999999979750, -10.53360074219763121, 5.000000000000000000 ) ) ;
#87708 = CARTESIAN_POINT ( 'NONE',  ( 29.99999999999999645, 2.375000000000000000, 4.319999999999998508 ) ) ;
#87709 = ORIENTED_EDGE ( 'NONE', *, *, #58641, .T. ) ;
#87710 = PLANE ( 'NONE',  #51262 ) ;
#87711 = VECTOR ( 'NONE', #78086, 1000.000000000000000 ) ;
#87712 = AXIS2_PLACEMENT_3D ( 'NONE', #102977, #1476, #59490 ) ;
#87714 = ADVANCED_FACE ( 'NONE', ( #102874 ), #49221, .F. ) ;
#87713 = PLANE ( 'NONE',  #104953 ) ;
#87715 = ORIENTED_EDGE ( 'NONE', *, *, #29215, .F. ) ;
#87716 = CIRCLE ( 'NONE', #22898, 2.500000000000000888 ) ;
#87718 = ORIENTED_EDGE ( 'NONE', *, *, #110406, .T. ) ;
#87717 = CARTESIAN_POINT ( 'NONE',  ( -9.299744871391588674, -27.71228299555212971, 4.000000000000000000 ) ) ;
#87720 = EDGE_LOOP ( 'NONE', ( #141736, #81935, #102697, #60280 ) ) ;
#87719 = ADVANCED_FACE ( 'NONE', ( #116587 ), #93412, .F. ) ;
#87721 = EDGE_CURVE ( 'NONE', #1792, #115214, #33441, .T. ) ;
#87722 = LINE ( 'NONE', #121752, #40079 ) ;
#87723 = DIRECTION ( 'NONE',  ( -0.000000000000000000, 0.000000000000000000, 1.000000000000000000 ) ) ;
#87724 = MECHANICAL_DESIGN_GEOMETRIC_PRESENTATION_REPRESENTATION (  '', ( #101571 ), #38777 ) ;
#87725 = ORIENTED_EDGE ( 'NONE', *, *, #50685, .F. ) ;
#87726 = DIRECTION ( 'NONE',  ( 1.000000000000000000, 0.000000000000000000, 0.000000000000000000 ) ) ;
#87727 = AXIS2_PLACEMENT_3D ( 'NONE', #10319, #53105, #21208 ) ;
#87728 = CARTESIAN_POINT ( 'NONE',  ( -12.48921356237309155, -27.52281430457064104, 5.000000000000000000 ) ) ;
#87729 = DIRECTION ( 'NONE',  ( -0.3543493200069162685, -0.000000000000000000, -0.9351131265310288487 ) ) ;
#87730 = ADVANCED_FACE ( 'NONE', ( #15109 ), #60087, .F. ) ;
#87731 = LINE ( 'NONE', #131966, #141127 ) ;
#87732 = CARTESIAN_POINT ( 'NONE',  ( 0.1600000000000024458, -7.375232382467828529, -3.003213012813335858 ) ) ;
#87733 = CARTESIAN_POINT ( 'NONE',  ( 3.208333333333333481, 3.047499999999997655, 5.278424836066143655 ) ) ;
#87734 = CARTESIAN_POINT ( 'NONE',  ( 29.99999999999979039, -6.412538124160685804, 4.000000000000000000 ) ) ;
#87735 = FACE_OUTER_BOUND ( 'NONE', #24875, .T. ) ;
#87736 = DIRECTION ( 'NONE',  ( -0.7071067811865487940, 0.7071067811865463515, 0.000000000000000000 ) ) ;
#87738 = VECTOR ( 'NONE', #29060, 1000.000000000000000 ) ;
#87737 = CARTESIAN_POINT ( 'NONE',  ( -34.92500000000001137, 10.33457404400604140, 0.4942731178106014589 ) ) ;
#87739 = LINE ( 'NONE', #53702, #120094 ) ;
#87740 = EDGE_CURVE ( 'NONE', #92540, #26964, #36873, .T. ) ;
#87741 = CARTESIAN_POINT ( 'NONE',  ( 110.3750000000000000, 7.950000000000000178, 1.460391307983218535E-15 ) ) ;
#87742 = CARTESIAN_POINT ( 'NONE',  ( -20.51078643762690490, -27.52281430457041012, 5.000000000000000000 ) ) ;
#87743 = ORIENTED_EDGE ( 'NONE', *, *, #139462, .F. ) ;
#87744 = ORIENTED_EDGE ( 'NONE', *, *, #6127, .F. ) ;
#87745 = CARTESIAN_POINT ( 'NONE',  ( 96.95833333333334281, 3.974999999999997424, 6.884901960086288852 ) ) ;
#87746 = AXIS2_PLACEMENT_3D ( 'NONE', #20697, #85967, #131624 ) ;
#87747 = ORIENTED_EDGE ( 'NONE', *, *, #86903, .T. ) ;
#87748 = VERTEX_POINT ( 'NONE', #92675 ) ;
#87749 = VERTEX_POINT ( 'NONE', #104989 ) ;
#87750 = DIRECTION ( 'NONE',  ( 0.6830127018922181881, 0.6830127018922202975, -0.2588190451025214056 ) ) ;
#87751 = FACE_OUTER_BOUND ( 'NONE', #132061, .T. ) ;
#87752 = ORIENTED_EDGE ( 'NONE', *, *, #71990, .T. ) ;
#87753 = VECTOR ( 'NONE', #128613, 1000.000000000000000 ) ;
#87754 = CARTESIAN_POINT ( 'NONE',  ( 34.42499999999998295, 22.22500000000000142, 5.000000000000000000 ) ) ;
#87755 = AXIS2_PLACEMENT_3D ( 'NONE', #130186, #119273, #19963 ) ;
#87756 = VECTOR ( 'NONE', #96083, 1000.000000000000000 ) ;
#87757 = CARTESIAN_POINT ( 'NONE',  ( 13.10742158956126246, 3.736470153597433619, 4.109745541549489012 ) ) ;
#87758 = DIRECTION ( 'NONE',  ( -0.7071067811865486830, -0.7071067811865464625, 0.000000000000000000 ) ) ;
#87759 = EDGE_LOOP ( 'NONE', ( #123255, #16115, #7756, #10063 ) ) ;
#87760 = CARTESIAN_POINT ( 'NONE',  ( 0.7071067811865432429, 11.25929247661560595, 5.000000000000000000 ) ) ;
#87761 = DIRECTION ( 'NONE',  ( 0.000000000000000000, 0.000000000000000000, -1.000000000000000000 ) ) ;
#87762 = AXIS2_PLACEMENT_3D ( 'NONE', #94679, #138937, #54099 ) ;
#87763 = CARTESIAN_POINT ( 'NONE',  ( 17.01299345043647193, -0.9444868035624204294, -36.39086428169088094 ) ) ;
#87764 = CARTESIAN_POINT ( 'NONE',  ( 23.77083333333333570, 6.094999999999991758, 1.633150327867686880 ) ) ;
#87765 = CARTESIAN_POINT ( 'NONE',  ( 54.18398860626899705, 28.73617430169825226, 5.000000000000000000 ) ) ;
#87766 = AXIS2_PLACEMENT_3D ( 'NONE', #74664, #99215, #19542 ) ;
#87767 = FACE_OUTER_BOUND ( 'NONE', #102541, .T. ) ;
#87768 = CARTESIAN_POINT ( 'NONE',  ( -20.20666063542138957, 21.75929247661549226, 4.998822639870715179 ) ) ;
#87769 = EDGE_CURVE ( 'NONE', #89080, #135397, #83252, .T. ) ;
#87770 = ADVANCED_FACE ( 'NONE', ( #15792 ), #124611, .F. ) ;
#87771 = ORIENTED_EDGE ( 'NONE', *, *, #19469, .T. ) ;
#87772 = EDGE_LOOP ( 'NONE', ( #15359, #126910, #15739, #77521 ) ) ;
#87773 = CARTESIAN_POINT ( 'NONE',  ( 122.2087635252314328, -7.482591942790329030E-16, 6.110000000000001208 ) ) ;
#87774 = EDGE_LOOP ( 'NONE', ( #142209, #75207, #2450, #122008 ) ) ;
#87775 = DIRECTION ( 'NONE',  ( -0.7071067811865486830, -0.7071067811865464625, 0.000000000000000000 ) ) ;
#87776 = DIRECTION ( 'NONE',  ( -1.000000000000000000, -0.000000000000000000, -0.000000000000000000 ) ) ;
#87777 = VECTOR ( 'NONE', #8593, 1000.000000000000000 ) ;
#87778 = DIRECTION ( 'NONE',  ( -0.6830127018922181881, 0.6830127018922202975, -0.2588190451025214056 ) ) ;
#87779 = FACE_OUTER_BOUND ( 'NONE', #104273, .T. ) ;
#87780 = LINE ( 'NONE', #42874, #9597 ) ;
#87781 = CARTESIAN_POINT ( 'NONE',  ( 112.0579301918981372, 6.110000000000000320, -1.637169565754156064 ) ) ;
#87782 = ORIENTED_EDGE ( 'NONE', *, *, #85485, .T. ) ;
#87783 = VERTEX_POINT ( 'NONE', #104256 ) ;
#87784 = CARTESIAN_POINT ( 'NONE',  ( 70.66252705046288440, 7.949999999999998401, 1.460391307983218338E-15 ) ) ;
#87785 = DIRECTION ( 'NONE',  ( -0.7071067811865487940, 0.7071067811865463515, 0.000000000000000000 ) ) ;
#87786 = VERTEX_POINT ( 'NONE', #4922 ) ;
#87787 = ORIENTED_EDGE ( 'NONE', *, *, #42272, .T. ) ;
#87788 = CARTESIAN_POINT ( 'NONE',  ( 41.12543019189809712, 5.291415217122919401, 3.055000000000002824 ) ) ;
#87789 = ORIENTED_EDGE ( 'NONE', *, *, #63957, .T. ) ;
#87790 = CARTESIAN_POINT ( 'NONE',  ( -71.99451991528749772, 28.92564299267988304, 4.000000000000000000 ) ) ;
#87791 = DIRECTION ( 'NONE',  ( -0.6830127018922180770, -0.6830127018922204085, -0.2588190451025213501 ) ) ;
#87792 = LINE ( 'NONE', #757, #90076 ) ;
#87793 = CARTESIAN_POINT ( 'NONE',  ( 42.78709685856478728, 3.054999999999997495, 5.291415217122919401 ) ) ;
#87794 = ORIENTED_EDGE ( 'NONE', *, *, #9105, .F. ) ;
#87795 = LINE ( 'NONE', #11628, #47924 ) ;
#87796 = ORIENTED_EDGE ( 'NONE', *, *, #119010, .F. ) ;
#87797 = VERTEX_POINT ( 'NONE', #4186 ) ;
#87798 = EDGE_LOOP ( 'NONE', ( #52229, #79950, #103113, #114818 ) ) ;
#87799 = PLANE ( 'NONE',  #109021 ) ;
#87800 = ORIENTED_EDGE ( 'NONE', *, *, #61206, .T. ) ;
#87801 = CARTESIAN_POINT ( 'NONE',  ( 150.3000000000000114, 0.000000000000000000, 4.749999999999997335 ) ) ;
#87802 = PLANE ( 'NONE',  #66819 ) ;
#87803 = AXIS2_PLACEMENT_3D ( 'NONE', #71813, #29003, #105127 ) ;
#87804 = AXIS2_PLACEMENT_3D ( 'NONE', #49598, #28539, #48145 ) ;
#87805 = VECTOR ( 'NONE', #138797, 1000.000000000000227 ) ;
#87806 = CARTESIAN_POINT ( 'NONE',  ( -11.99451991528749417, 28.92564299267946382, 4.000000000000000000 ) ) ;
#87808 = ADVANCED_FACE ( 'NONE', ( #135507 ), #26722, .F. ) ;
#87807 = AXIS2_PLACEMENT_3D ( 'NONE', #96873, #30972, #6283 ) ;
#87809 = FACE_BOUND ( 'NONE', #80167, .T. ) ;
#87810 = ORIENTED_EDGE ( 'NONE', *, *, #23606, .T. ) ;
#87811 = DIRECTION ( 'NONE',  ( -0.6830127018922180770, -0.6830127018922204085, -0.2588190451025213501 ) ) ;
#87812 = EDGE_CURVE ( 'NONE', #57315, #67596, #91978, .T. ) ;
#87813 = EDGE_CURVE ( 'NONE', #44987, #108750, #49927, .T. ) ;
#87814 = DIRECTION ( 'NONE',  ( 0.7071067811865486830, -0.7071067811865464625, -0.000000000000000000 ) ) ;
#87815 = DIRECTION ( 'NONE',  ( -0.6830127018922180770, -0.6830127018922204085, -0.2588190451025213501 ) ) ;
#87816 = EDGE_LOOP ( 'NONE', ( #134372, #105830, #78716 ) ) ;
#87817 = DIRECTION ( 'NONE',  ( 0.5735764363510451602, 0.8191520442889924647, 0.000000000000000000 ) ) ;
#87818 = VERTEX_POINT ( 'NONE', #27416 ) ;
#87819 = EDGE_LOOP ( 'NONE', ( #142375, #77846, #22852, #64372, #41522, #51627 ) ) ;
#87820 = VECTOR ( 'NONE', #74914, 1000.000000000000000 ) ;
#87821 = CARTESIAN_POINT ( 'NONE',  ( 14.99999999999989875, 20.96639925780205260, 5.000000000000000000 ) ) ;
#87822 = EDGE_LOOP ( 'NONE', ( #85667, #34653, #136930, #39795 ) ) ;
#87823 = ADVANCED_FACE ( 'NONE', ( #115836 ), #114441, .T. ) ;
#87824 = EDGE_CURVE ( 'NONE', #119486, #57481, #96230, .T. ) ;
#87825 = CARTESIAN_POINT ( 'NONE',  ( 49.20376352523145158, 6.109999999999998543, 1.122388791418548911E-15 ) ) ;
#87826 = ORIENTED_EDGE ( 'NONE', *, *, #4694, .T. ) ;
#87827 =( BOUNDED_CURVE ( )  B_SPLINE_CURVE ( 2, ( #47716, #135422, #89742, #136816, #125233, #123108, #57867, #23784, #35407, #103457, #102780, #25920, #79649 ),
 .UNSPECIFIED., .F., .T. ) 
 B_SPLINE_CURVE_WITH_KNOTS ( ( 3, 2, 2, 2, 2, 2, 3 ),
 ( 0.2166666666666667296, 0.2194444444444444697, 0.2222222222222222376, 0.2250000000000000056, 0.2277777777777777457, 0.2305555555555555414, 0.2333333333333332815 ),
 .UNSPECIFIED. ) 
 CURVE ( )  GEOMETRIC_REPRESENTATION_ITEM ( )  RATIONAL_B_SPLINE_CURVE ( ( 0.9999999999999993339, 0.9659258262890689783, 1.000000000000000000, 0.9659258262890683122, 1.000000000000000000, 0.9659258262890683122, 1.000000000000000000, 0.9659258262890683122, 1.000000000000000000, 0.9659258262890683122, 1.000000000000000000, 0.9659258262890689783, 0.9999999999999993339 ) ) 
 REPRESENTATION_ITEM ( '' )  );
#87828 = FACE_OUTER_BOUND ( 'NONE', #95397, .T. ) ;
#87829 = ADVANCED_FACE ( 'NONE', ( #28876 ), #107826, .F. ) ;
#87830 = DIRECTION ( 'NONE',  ( -0.000000000000000000, 0.3543493200069153248, 0.9351131265310292928 ) ) ;
#87831 = ORIENTED_EDGE ( 'NONE', *, *, #140939, .T. ) ;
#87832 = CARTESIAN_POINT ( 'NONE',  ( 3.250000000000000000, -5.000000000000000000, -6.123233995736766282E-16 ) ) ;
#87833 = PLANE ( 'NONE',  #143021 ) ;
#87834 = VECTOR ( 'NONE', #119797, 1000.000000000000000 ) ;
#87835 = ADVANCED_FACE ( 'NONE', ( #96934 ), #120117, .F. ) ;
#87836 = VECTOR ( 'NONE', #139502, 1000.000000000000227 ) ;
#87837 = CARTESIAN_POINT ( 'NONE',  ( 52.60764783923753640, -52.00875322212549179, -39.33676470588228113 ) ) ;
#87838 = CYLINDRICAL_SURFACE ( 'NONE', #62153, 0.5000000000000000000 ) ;
#87839 = CARTESIAN_POINT ( 'NONE',  ( 11.99451991528749417, 28.92564299267946382, 4.000000000000000000 ) ) ;
#87840 = PLANE ( 'NONE',  #2923 ) ;
#87841 = LINE ( 'NONE', #77697, #83489 ) ;
#87842 = ORIENTED_EDGE ( 'NONE', *, *, #13058, .F. ) ;
#87843 = EDGE_LOOP ( 'NONE', ( #140531, #16221, #7870, #53441 ) ) ;
#87844 = ORIENTED_EDGE ( 'NONE', *, *, #71887, .T. ) ;
#87845 = VECTOR ( 'NONE', #85810, 999.9999999999998863 ) ;
#87846 = CARTESIAN_POINT ( 'NONE',  ( 14.84387692260749603, -22.22499999999999432, 4.000000000000000000 ) ) ;
#87847 = CARTESIAN_POINT ( 'NONE',  ( 15.48921356237309510, -27.52281430457066236, 5.000000000000000000 ) ) ;
#87848 = VERTEX_POINT ( 'NONE', #128882 ) ;
#87849 = AXIS2_PLACEMENT_3D ( 'NONE', #17486, #118211, #61742 ) ;
#87850 = AXIS2_PLACEMENT_3D ( 'NONE', #81333, #125541, #15296 ) ;
#87851 = ORIENTED_EDGE ( 'NONE', *, *, #32017, .F. ) ;
#87852 = CARTESIAN_POINT ( 'NONE',  ( 165.4843069612475119, 26.96999999999994202, -33.83501209545872968 ) ) ;
#87853 = DIRECTION ( 'NONE',  ( 0.6830127018922181881, 0.6830127018922202975, -0.2588190451025214056 ) ) ;
#87854 = DIRECTION ( 'NONE',  ( -1.000000000000000000, -1.224606353822377258E-16, -0.000000000000000000 ) ) ;
#87855 = ORIENTED_EDGE ( 'NONE', *, *, #46178, .T. ) ;
#87856 = VECTOR ( 'NONE', #141213, 1000.000000000000000 ) ;
#87857 = DIRECTION ( 'NONE',  ( -0.7071067811865486830, -0.7071067811865464625, 0.000000000000000000 ) ) ;
#87858 = EDGE_CURVE ( 'NONE', #9764, #105676, #39886, .T. ) ;
#87859 = VECTOR ( 'NONE', #90740, 999.9999999999998863 ) ;
#87860 = LINE ( 'NONE', #65427, #81514 ) ;
#87861 = CARTESIAN_POINT ( 'NONE',  ( 18.87956980810189123, 3.967499999999998916, 6.871911579029510442 ) ) ;
#87862 = LINE ( 'NONE', #21884, #38914 ) ;
#87863 = ORIENTED_EDGE ( 'NONE', *, *, #115107, .F. ) ;
#87864 = CARTESIAN_POINT ( 'NONE',  ( 116.4329301918981088, 1.637169565754156730, 6.110000000000001208 ) ) ;
#87865 = CARTESIAN_POINT ( 'NONE',  ( 20.99451991528748707, 28.92564299267952777, 4.000000000000000000 ) ) ;
#87866 = EDGE_CURVE ( 'NONE', #4116, #45577, #52741, .T. ) ;
#87867 = DIRECTION ( 'NONE',  ( 0.7071067811865486830, -0.7071067811865464625, -0.000000000000000000 ) ) ;
#87868 = VECTOR ( 'NONE', #5338, 1000.000000000000000 ) ;
#87870 = ORIENTED_EDGE ( 'NONE', *, *, #106011, .T. ) ;
#87869 = LINE ( 'NONE', #21180, #72674 ) ;
#87871 = CARTESIAN_POINT ( 'NONE',  ( 21.18398860626899349, 28.73617430169802134, 5.000000000000000000 ) ) ;
#87872 = VERTEX_POINT ( 'NONE', #42628 ) ;
#87873 = CARTESIAN_POINT ( 'NONE',  ( -10.49999999999992184, -4.912538124160708897, 4.000000000000000000 ) ) ;
#87874 = CARTESIAN_POINT ( 'NONE',  ( 128.5894344200537773, -52.00875322212549179, -39.86617647058817226 ) ) ;
#87875 = DIRECTION ( 'NONE',  ( 0.7071067811865486830, -0.7071067811865464625, -0.000000000000000000 ) ) ;
#87876 = ORIENTED_EDGE ( 'NONE', *, *, #56116, .F. ) ;
#87877 = EDGE_CURVE ( 'NONE', #2199, #57761, #108523, .T. ) ;
#87878 = EDGE_CURVE ( 'NONE', #30701, #79059, #75943, .T. ) ;
#87879 = CARTESIAN_POINT ( 'NONE',  ( -26.99999999999981526, 9.631307414974299874, -9.079085613539605859 ) ) ;
#87880 = DIRECTION ( 'NONE',  ( -0.6830127018922180770, -0.6830127018922204085, -0.2588190451025213501 ) ) ;
#87881 = ORIENTED_EDGE ( 'NONE', *, *, #71991, .F. ) ;
#87882 = CARTESIAN_POINT ( 'NONE',  ( 7.499999999999951150, 7.087461875839168535, 4.000000000000000000 ) ) ;
#87884 = EDGE_CURVE ( 'NONE', #4046, #12348, #139067, .T. ) ;
#87883 = DIRECTION ( 'NONE',  ( 1.000000000000000000, -0.000000000000000000, -0.000000000000000000 ) ) ;
#87885 = ORIENTED_EDGE ( 'NONE', *, *, #141796, .T. ) ;
#87886 = DIRECTION ( 'NONE',  ( 0.000000000000000000, 0.000000000000000000, 1.000000000000000000 ) ) ;
#87888 = VERTEX_POINT ( 'NONE', #73801 ) ;
#87887 = FACE_OUTER_BOUND ( 'NONE', #15005, .T. ) ;
#87889 = ORIENTED_EDGE ( 'NONE', *, *, #103725, .T. ) ;
#87890 = DIRECTION ( 'NONE',  ( 1.000000000000000000, 0.000000000000000000, 0.000000000000000000 ) ) ;
#87891 = CARTESIAN_POINT ( 'NONE',  ( -21.79289321881330466, -14.24070752338413470, 5.000000000000000000 ) ) ;
#87892 = VERTEX_POINT ( 'NONE', #118717 ) ;
#87893 = DIRECTION ( 'NONE',  ( -1.000000000000000000, -0.000000000000000000, -0.000000000000000000 ) ) ;
#87894 = CARTESIAN_POINT ( 'NONE',  ( 0.4892135623730947680, -27.52281430457055578, 5.000000000000000000 ) ) ;
#87895 = ORIENTED_EDGE ( 'NONE', *, *, #136766, .T. ) ;
#87896 = EDGE_CURVE ( 'NONE', #104418, #75992, #112136, .T. ) ;
#87897 = CARTESIAN_POINT ( 'NONE',  ( -3.183988606268992161, 28.73617430169789699, 5.000000000000000000 ) ) ;
#87898 = CARTESIAN_POINT ( 'NONE',  ( 0.000000000000000000, 0.000000000000000000, 5.000000000000000000 ) ) ;
#87899 = DIRECTION ( 'NONE',  ( -0.000000000000000000, -0.000000000000000000, -1.000000000000000000 ) ) ;
#87900 = DIRECTION ( 'NONE',  ( -0.000000000000000000, -1.000000000000000000, -0.000000000000000000 ) ) ;
#87901 = CARTESIAN_POINT ( 'NONE',  ( 42.05793019189811588, 6.110000000000001208, -1.637169565754156286 ) ) ;
#87902 = DIRECTION ( 'NONE',  ( 0.3543493200069163240, -0.000000000000000000, -0.9351131265310288487 ) ) ;
#87903 = ORIENTED_EDGE ( 'NONE', *, *, #118593, .F. ) ;
#87904 = ORIENTED_EDGE ( 'NONE', *, *, #102782, .T. ) ;
#87905 = EDGE_CURVE ( 'NONE', #131559, #41660, #69521, .T. ) ;
#87906 = ORIENTED_EDGE ( 'NONE', *, *, #136078, .F. ) ;
#87907 = ORIENTED_EDGE ( 'NONE', *, *, #20410, .F. ) ;
#87908 = CARTESIAN_POINT ( 'NONE',  ( -44.99451991528749772, 28.92564299267969474, 4.000000000000000000 ) ) ;
#87909 = DIRECTION ( 'NONE',  ( 0.6830127018922180770, -0.6830127018922204085, -0.2588190451025213501 ) ) ;
#87910 = AXIS2_PLACEMENT_3D ( 'NONE', #45109, #111756, #12422 ) ;
#87911 = VECTOR ( 'NONE', #23687, 1000.000000000000227 ) ;
#87912 = AXIS2_PLACEMENT_3D ( 'NONE', #46661, #101691, #58251 ) ;
#87913 = ORIENTED_EDGE ( 'NONE', *, *, #73162, .T. ) ;
#87914 = CARTESIAN_POINT ( 'NONE',  ( 0.000000000000000000, 0.000000000000000000, 5.000000000000000000 ) ) ;
#87915 = DIRECTION ( 'NONE',  ( 0.7071067811865487940, 0.7071067811865463515, 0.000000000000000000 ) ) ;
#87916 = AXIS2_PLACEMENT_3D ( 'NONE', #63447, #62007, #259 ) ;
#87917 = CARTESIAN_POINT ( 'NONE',  ( 27.79289321881326913, 12.75929247661559351, 5.000000000000000000 ) ) ;
#87918 = EDGE_CURVE ( 'NONE', #29863, #118228, #31723, .T. ) ;
#87919 = DIRECTION ( 'NONE',  ( 0.7071067811865487940, 0.7071067811865463515, -0.000000000000000000 ) ) ;
#87920 = CARTESIAN_POINT ( 'NONE',  ( 123.2295968585647756, -6.110000000000000320, -1.637169565754161393 ) ) ;
#87921 = ORIENTED_EDGE ( 'NONE', *, *, #131677, .F. ) ;
#87922 = LINE ( 'NONE', #85774, #44188 ) ;
#87923 = CARTESIAN_POINT ( 'NONE',  ( 4.499999999999976019, -8.947814304570735899, 5.000000000000000000 ) ) ;
#87924 = DIRECTION ( 'NONE',  ( 0.000000000000000000, 1.000000000000000000, 0.000000000000000000 ) ) ;
#87925 = DIRECTION ( 'NONE',  ( 0.6830127018922180770, -0.6830127018922204085, -0.2588190451025213501 ) ) ;
#87926 = FACE_OUTER_BOUND ( 'NONE', #41082, .T. ) ;
#87927 = LINE ( 'NONE', #11044, #92140 ) ;
#87928 = CARTESIAN_POINT ( 'NONE',  ( 60.74586038379622721, 3.974999999999996980, 6.884901960086287964 ) ) ;
#87929 = FACE_BOUND ( 'NONE', #81654, .T. ) ;
#87930 = ADVANCED_FACE ( 'NONE', ( #41162 ), #20826, .F. ) ;
#87931 = CARTESIAN_POINT ( 'NONE',  ( -24.83829387547365286, -6.740707523384205757, 16.75550250614861625 ) ) ;
#87932 = AXIS2_PLACEMENT_3D ( 'NONE', #91304, #81864, #26725 ) ;
#87933 = ORIENTED_EDGE ( 'NONE', *, *, #58045, .F. ) ;
#87934 = ORIENTED_EDGE ( 'NONE', *, *, #143335, .T. ) ;
#87935 = CARTESIAN_POINT ( 'NONE',  ( 48.54166666666666430, -3.975000000000002753, 6.884901960086286188 ) ) ;
#87936 = EDGE_CURVE ( 'NONE', #74056, #94977, #84000, .T. ) ;
#87937 = DIRECTION ( 'NONE',  ( -0.6830127018922180770, -0.6830127018922204085, -0.2588190451025213501 ) ) ;
#87938 = AXIS2_PLACEMENT_3D ( 'NONE', #87040, #118941, #9431 ) ;
#87939 = LINE ( 'NONE', #132181, #122487 ) ;
#87940 = ORIENTED_EDGE ( 'NONE', *, *, #11391, .T. ) ;
#87941 = LINE ( 'NONE', #99506, #138136 ) ;
#87942 = DIRECTION ( 'NONE',  ( 0.7071067811865487940, 0.7071067811865463515, 0.000000000000000000 ) ) ;
#87943 = AXIS2_PLACEMENT_3D ( 'NONE', #51947, #18550, #139691 ) ;
#87944 = EDGE_CURVE ( 'NONE', #124953, #70498, #73112, .T. ) ;
#87945 = CARTESIAN_POINT ( 'NONE',  ( 48.56293019189809712, 1.637169565754157174, 6.110000000000002984 ) ) ;
#87946 = ORIENTED_EDGE ( 'NONE', *, *, #86869, .T. ) ;
#87947 = CARTESIAN_POINT ( 'NONE',  ( 25.39999999999999858, -7.600000000000061817, 28.92499999999998650 ) ) ;
#87948 = EDGE_LOOP ( 'NONE', ( #87135, #17450, #104056, #50599, #97478 ) ) ;
#87949 = ORIENTED_EDGE ( 'NONE', *, *, #110116, .T. ) ;
#87950 = DIRECTION ( 'NONE',  ( 0.6830127018922180770, -0.6830127018922204085, -0.2588190451025213501 ) ) ;
#87951 = AXIS2_PLACEMENT_3D ( 'NONE', #96822, #141067, #122901 ) ;
#87952 = VECTOR ( 'NONE', #44274, 1000.000000000000000 ) ;
#87953 = CARTESIAN_POINT ( 'NONE',  ( 80.28752705046289861, 0.000000000000000000, -7.949999999999998401 ) ) ;
#87954 = CARTESIAN_POINT ( 'NONE',  ( -23.99999999999982947, -3.033600742197705369, 5.000000000000000000 ) ) ;
#87955 = CARTESIAN_POINT ( 'NONE',  ( 32.99999999999976552, -13.06887692260767686, 4.000000000000000000 ) ) ;
#87956 = VERTEX_POINT ( 'NONE', #77405 ) ;
#87957 = EDGE_CURVE ( 'NONE', #129972, #103515, #55627, .T. ) ;
#87958 = CARTESIAN_POINT ( 'NONE',  ( -33.48921356237309510, -27.52281430457078670, 5.000000000000000000 ) ) ;
#87960 = ORIENTED_EDGE ( 'NONE', *, *, #116864, .T. ) ;
#87959 = CARTESIAN_POINT ( 'NONE',  ( 8.941639616203772789, -6.094999999999989093, 1.633150327867691542 ) ) ;
#87961 = AXIS2_PLACEMENT_3D ( 'NONE', #134702, #47711, #91872 ) ;
#87962 = CARTESIAN_POINT ( 'NONE',  ( 80.64626352523141861, -4.472830434245840259, 4.472830434245838482 ) ) ;
#87963 = LINE ( 'NONE', #97378, #69341 ) ;
#87964 = DIRECTION ( 'NONE',  ( 0.7071067811865487940, 0.7071067811865463515, 0.000000000000000000 ) ) ;
#87965 = DIRECTION ( 'NONE',  ( -0.000000000000000000, 0.3543493200069153248, 0.9351131265310292928 ) ) ;
#87966 = AXIS2_PLACEMENT_3D ( 'NONE', #23564, #69230, #67833 ) ;
#87967 = CARTESIAN_POINT ( 'NONE',  ( -18.18398860626898994, 28.73617430169800002, 5.000000000000000000 ) ) ;
#87968 =( LENGTH_UNIT ( ) NAMED_UNIT ( * ) SI_UNIT ( .MILLI., .METRE. ) );
#87969 = EDGE_LOOP ( 'NONE', ( #72311, #49313, #92564, #11863 ) ) ;
#87970 = CARTESIAN_POINT ( 'NONE',  ( 27.24169458425171086, 0.7592924766157138627, 14.37146558664976759 ) ) ;
#87971 = CARTESIAN_POINT ( 'NONE',  ( 66.99543019189812298, 5.291415217122916737, 3.055000000000001936 ) ) ;
#87972 = LINE ( 'NONE', #90102, #48803 ) ;
#87973 = CARTESIAN_POINT ( 'NONE',  ( -12.70710678118645021, 5.259292476615667233, 5.000000000000000000 ) ) ;
#87974 = DIRECTION ( 'NONE',  ( 0.7071067811865487940, 0.7071067811865463515, -0.000000000000000000 ) ) ;
#87975 = VERTEX_POINT ( 'NONE', #109279 ) ;
#87976 = VERTEX_POINT ( 'NONE', #79565 ) ;
#87977 = VECTOR ( 'NONE', #58923, 999.9999999999998863 ) ;
#87978 = CARTESIAN_POINT ( 'NONE',  ( -6.183988606268994381, 28.73617430169791476, 5.000000000000000000 ) ) ;
#87979 = CARTESIAN_POINT ( 'NONE',  ( 17.20829011259838026, -2.505970753447624322, 4.303104124266152297 ) ) ;
#87980 = ORIENTED_EDGE ( 'NONE', *, *, #66664, .F. ) ;
#87981 = ORIENTED_EDGE ( 'NONE', *, *, #11876, .T. ) ;
#87982 = CARTESIAN_POINT ( 'NONE',  ( -34.42500000000001137, 17.97718569542923106, 5.000000000000000000 ) ) ;
#87983 = ORIENTED_EDGE ( 'NONE', *, *, #39229, .T. ) ;
#87984 = LINE ( 'NONE', #44522, #33099 ) ;
#87985 = CARTESIAN_POINT ( 'NONE',  ( 29.67183060077626422, 14.25929247661556509, 4.000000000000000000 ) ) ;
#87986 = VECTOR ( 'NONE', #117591, 1000.000000000000000 ) ;
#87987 = ADVANCED_FACE ( 'NONE', ( #88255 ), #134628, .F. ) ;
#87988 = LINE ( 'NONE', #132238, #28029 ) ;
#87989 = FACE_BOUND ( 'NONE', #137591, .T. ) ;
#87990 = DIRECTION ( 'NONE',  ( 2.781805975412905274E-17, -0.3543493200069152138, 0.9351131265310292928 ) ) ;
#87991 = ADVANCED_FACE ( 'NONE', ( #109986 ), #11352, .F. ) ;
#87992 = DIRECTION ( 'NONE',  ( 0.000000000000000000, -2.556434596176436521E-15, -1.000000000000000000 ) ) ;
#87993 = LINE ( 'NONE', #56118, #75846 ) ;
#87995 = ORIENTED_EDGE ( 'NONE', *, *, #15532, .T. ) ;
#87994 = DIRECTION ( 'NONE',  ( -0.3543493200069162685, -0.000000000000000000, -0.9351131265310288487 ) ) ;
#87996 = AXIS2_PLACEMENT_3D ( 'NONE', #35341, #14265, #22963 ) ;
#87997 = PLANE ( 'NONE',  #81054 ) ;
#87998 = ORIENTED_EDGE ( 'NONE', *, *, #17465, .F. ) ;
#87999 = ADVANCED_FACE ( 'NONE', ( #1892 ), #87532, .F. ) ;
#88000 = EDGE_CURVE ( 'NONE', #123737, #63821, #100565, .T. ) ;
#88001 = ORIENTED_EDGE ( 'NONE', *, *, #122830, .T. ) ;
#88002 = CARTESIAN_POINT ( 'NONE',  ( 79.09959685856478018, -6.109999999999997655, -1.637169565754160283 ) ) ;
#88003 = ORIENTED_EDGE ( 'NONE', *, *, #37550, .T. ) ;
#88004 = EDGE_CURVE ( 'NONE', #69590, #115675, #54227, .T. ) ;
#88005 = CARTESIAN_POINT ( 'NONE',  ( 3.792893218813427669, 15.75929247661555976, 5.000000000000000000 ) ) ;
#88006 = ADVANCED_FACE ( 'NONE', ( #9956 ), #67208, .T. ) ;
#88007 = ORIENTED_EDGE ( 'NONE', *, *, #108330, .F. ) ;
#88008 = FACE_OUTER_BOUND ( 'NONE', #77677, .T. ) ;
#88009 = EDGE_CURVE ( 'NONE', #51675, #133359, #76683, .T. ) ;
#88010 = CARTESIAN_POINT ( 'NONE',  ( 25.39999999999999858, -1.600000000000012301, -20.40202195861969514 ) ) ;
#88011 = CARTESIAN_POINT ( 'NONE',  ( 24.18398860626899705, 28.73617430169804265, 5.000000000000000000 ) ) ;
#88012 = EDGE_CURVE ( 'NONE', #100733, #108418, #5628, .T. ) ;
#88013 = AXIS2_PLACEMENT_3D ( 'NONE', #107811, #91108, #92486 ) ;
#88014 = FACE_OUTER_BOUND ( 'NONE', #38403, .T. ) ;
#88015 = CARTESIAN_POINT ( 'NONE',  ( -9.005480084712511157, 28.92564299267931816, 4.000000000000000000 ) ) ;
#88016 = CARTESIAN_POINT ( 'NONE',  ( -6.183988606268994381, 28.73617430169791476, 5.000000000000000000 ) ) ;
#88017 = CARTESIAN_POINT ( 'NONE',  ( -24.75860074219779605, 21.72500000000000853, 5.000000000000000000 ) ) ;
#88018 = FACE_OUTER_BOUND ( 'NONE', #134763, .T. ) ;
#88019 = ORIENTED_EDGE ( 'NONE', *, *, #106579, .F. ) ;
#88020 = VECTOR ( 'NONE', #46398, 1000.000000000000000 ) ;
#88021 = DIRECTION ( 'NONE',  ( 0.000000000000000000, 0.000000000000000000, 1.000000000000000000 ) ) ;
#88022 = TOROIDAL_SURFACE ( 'NONE', #16163, 2.000000000000000000, 1.000000000000000000 ) ;
#88023 = ORIENTED_EDGE ( 'NONE', *, *, #129381, .T. ) ;
#88024 = CARTESIAN_POINT ( 'NONE',  ( -66.18398860626901126, 28.73617430169833753, 5.000000000000000000 ) ) ;
#88025 = CARTESIAN_POINT ( 'NONE',  ( -27.48921356237309155, -27.52281430457074762, 5.000000000000000000 ) ) ;
#88026 = AXIS2_PLACEMENT_3D ( 'NONE', #103511, #124578, #136161 ) ;
#88027 = EDGE_CURVE ( 'NONE', #133213, #5707, #123752, .T. ) ;
#88028 = ORIENTED_EDGE ( 'NONE', *, *, #70984, .T. ) ;
#88029 = ORIENTED_EDGE ( 'NONE', *, *, #130967, .F. ) ;
#88030 = CARTESIAN_POINT ( 'NONE',  ( 9.489213562373095101, -27.52281430457062328, 5.000000000000000000 ) ) ;
#88031 = ORIENTED_EDGE ( 'NONE', *, *, #87175, .T. ) ;
#88032 = AXIS2_PLACEMENT_3D ( 'NONE', #107702, #18528, #131623 ) ;
#88033 = CARTESIAN_POINT ( 'NONE',  ( 32.99999999999977973, -13.44781430457069149, 5.000000000000000000 ) ) ;
#88034 = EDGE_CURVE ( 'NONE', #57989, #22749, #1206, .T. ) ;
#88035 = DIRECTION ( 'NONE',  ( 0.3543493200069164351, 2.781805975412904658E-17, -0.9351131265310288487 ) ) ;
#88036 = CARTESIAN_POINT ( 'NONE',  ( 27.31663961620377634, -1.633150327867691987, -6.094999999999989093 ) ) ;
#88037 = CARTESIAN_POINT ( 'NONE',  ( 0.4249279634646616621, 12.59097312579417327, -26.73336350209328671 ) ) ;
#88038 = ORIENTED_EDGE ( 'NONE', *, *, #65211, .T. ) ;
#88039 = CARTESIAN_POINT ( 'NONE',  ( -16.49999999999987921, -8.947814304570734123, 5.000000000000000000 ) ) ;
#88040 = ORIENTED_EDGE ( 'NONE', *, *, #57801, .T. ) ;
#88041 = LINE ( 'NONE', #122074, #90511 ) ;
#88042 = CARTESIAN_POINT ( 'NONE',  ( 29.99451991528749417, 28.92564299267958816, 4.000000000000000000 ) ) ;
#88044 = ORIENTED_EDGE ( 'NONE', *, *, #24795, .F. ) ;
#88043 = FACE_OUTER_BOUND ( 'NONE', #89237, .T. ) ;
#88045 = ORIENTED_EDGE ( 'NONE', *, *, #139992, .T. ) ;
#88046 = DIRECTION ( 'NONE',  ( -0.7071067811865486830, 0.7071067811865464625, 0.000000000000000000 ) ) ;
#88047 = DIRECTION ( 'NONE',  ( 0.6830127018922181881, 0.6830127018922202975, -0.2588190451025214056 ) ) ;
#88048 = CARTESIAN_POINT ( 'NONE',  ( -19.05000000000000071, 3.174999999999997158, 5.000000000000000000 ) ) ;
#88049 = ORIENTED_EDGE ( 'NONE', *, *, #133515, .F. ) ;
#88050 = VECTOR ( 'NONE', #106838, 1000.000000000000000 ) ;
#88051 = PLANE ( 'NONE',  #140688 ) ;
#88052 = AXIS2_PLACEMENT_3D ( 'NONE', #93002, #71995, #115419 ) ;
#88053 = VERTEX_POINT ( 'NONE', #65088 ) ;
#88054 = ORIENTED_EDGE ( 'NONE', *, *, #57686, .F. ) ;
#88055 = EDGE_CURVE ( 'NONE', #120179, #70500, #12095, .T. ) ;
#88057 = CARTESIAN_POINT ( 'NONE',  ( -0.7071067811865345831, -0.7407075233842753681, 5.000000000000000000 ) ) ;
#88056 = AXIS2_PLACEMENT_3D ( 'NONE', #117658, #6037, #140175 ) ;
#88058 = CARTESIAN_POINT ( 'NONE',  ( 21.79289321881331176, -11.24070752338416845, 5.000000000000000000 ) ) ;
#88059 = DIRECTION ( 'NONE',  ( -0.3543493200069162685, -0.000000000000000000, -0.9351131265310288487 ) ) ;
#88060 = VECTOR ( 'NONE', #141769, 1000.000000000000227 ) ;
#88061 = FACE_OUTER_BOUND ( 'NONE', #140511, .T. ) ;
#88062 = EDGE_CURVE ( 'NONE', #34692, #64188, #43322, .T. ) ;
#88063 = LINE ( 'NONE', #122094, #116251 ) ;
#88064 = LINE ( 'NONE', #77904, #19333 ) ;
#88065 = DIRECTION ( 'NONE',  ( 0.7071067811865487940, 0.7071067811865463515, 0.000000000000000000 ) ) ;
#88066 = ORIENTED_EDGE ( 'NONE', *, *, #46501, .T. ) ;
#88067 = AXIS2_PLACEMENT_3D ( 'NONE', #27248, #115659, #16354 ) ;
#88068 = DIRECTION ( 'NONE',  ( 0.6830127018922181881, 0.6830127018922202975, -0.2588190451025214056 ) ) ;
#88069 = ORIENTED_EDGE ( 'NONE', *, *, #17332, .T. ) ;
#88070 = DIRECTION ( 'NONE',  ( 0.7071067811865486830, -0.7071067811865464625, -0.000000000000000000 ) ) ;
#88071 = EDGE_CURVE ( 'NONE', #36268, #48744, #101255, .T. ) ;
#88072 = CARTESIAN_POINT ( 'NONE',  ( 0.000000000000000000, 0.000000000000000000, 5.000000000000000000 ) ) ;
#88073 = DIRECTION ( 'NONE',  ( -0.6830127018922181881, 0.6830127018922202975, -0.2588190451025214056 ) ) ;
#88074 = ORIENTED_EDGE ( 'NONE', *, *, #140379, .F. ) ;
#88075 = COLOUR_RGB ( '', 0.09019608, 0.27058824, 0.51372549) ;
#88076 = CARTESIAN_POINT ( 'NONE',  ( -41.99451991528749062, 28.92564299267967343, 4.000000000000000000 ) ) ;
#88077 = DIRECTION ( 'NONE',  ( -0.3543493200069162685, -0.000000000000000000, -0.9351131265310288487 ) ) ;
#88078 = CARTESIAN_POINT ( 'NONE',  ( 25.65999999999999659, -2.055000000000000160, 0.000000000000000000 ) ) ;
#88079 = ORIENTED_EDGE ( 'NONE', *, *, #73920, .F. ) ;
#88080 = ORIENTED_EDGE ( 'NONE', *, *, #69123, .F. ) ;
#88081 = ADVANCED_FACE ( 'NONE', ( #123021 ), #12804, .F. ) ;
#88082 = LINE ( 'NONE', #99645, #90442 ) ;
#88083 = CARTESIAN_POINT ( 'NONE',  ( 34.42499999999998295, -21.02281430457037814, 5.000000000000000000 ) ) ;
#88084 = AXIS2_PLACEMENT_3D ( 'NONE', #49279, #96273, #84050 ) ;
#88085 = CARTESIAN_POINT ( 'NONE',  ( 51.48921356237309510, -27.52281430457091460, 5.000000000000000000 ) ) ;
#88086 = DIRECTION ( 'NONE',  ( -1.000000000000000000, 0.000000000000000000, 0.000000000000000000 ) ) ;
#88087 = FACE_OUTER_BOUND ( 'NONE', #51563, .T. ) ;
#88088 = CARTESIAN_POINT ( 'NONE',  ( 63.05793019189810877, 6.110000000000001208, -1.637169565754156286 ) ) ;
#88089 = CYLINDRICAL_SURFACE ( 'NONE', #27928, 7.950000000000000178 ) ;
#88090 = DIRECTION ( 'NONE',  ( -0.7071067811865486830, -0.7071067811865464625, 0.000000000000000000 ) ) ;
#88091 = DIRECTION ( 'NONE',  ( 0.000000000000000000, -1.000000000000000000, 0.000000000000000000 ) ) ;
#88092 = ORIENTED_EDGE ( 'NONE', *, *, #138169, .T. ) ;
#88093 = DIRECTION ( 'NONE',  ( -0.000000000000000000, -0.3543493200069152693, 0.9351131265310292928 ) ) ;
#88094 = ORIENTED_EDGE ( 'NONE', *, *, #22221, .T. ) ;
#88095 = CIRCLE ( 'NONE', #108850, 2.552699999999994418 ) ;
#88096 = DIRECTION ( 'NONE',  ( -0.6830127018922180770, -0.6830127018922204085, -0.2588190451025213501 ) ) ;
#88097 = CARTESIAN_POINT ( 'NONE',  ( 0.000000000000000000, 0.000000000000000000, 5.000000000000000000 ) ) ;
#88098 = LINE ( 'NONE', #133746, #113290 ) ;
#88099 = LINE ( 'NONE', #121423, #7152 ) ;
#88100 = CARTESIAN_POINT ( 'NONE',  ( 1.042387978378689350, 0.4000000000000001332, -2.015694669338588429 ) ) ;
#88101 = ADVANCED_FACE ( 'NONE', ( #65824 ), #10652, .F. ) ;
#88102 = DIRECTION ( 'NONE',  ( -0.000000000000000000, 0.3543493200069153248, 0.9351131265310292928 ) ) ;
#88103 = DIRECTION ( 'NONE',  ( 0.3543493200069162685, -0.000000000000000000, -0.9351131265310288487 ) ) ;
#88104 = ORIENTED_EDGE ( 'NONE', *, *, #13533, .F. ) ;
#88105 = EDGE_CURVE ( 'NONE', #62812, #22459, #58531, .T. ) ;
#88106 = ORIENTED_EDGE ( 'NONE', *, *, #98226, .F. ) ;
#88107 = DIRECTION ( 'NONE',  ( -1.000000000000000000, -1.224606353822377258E-16, -0.000000000000000000 ) ) ;
#88108 = FILL_AREA_STYLE ('',( #10516 ) ) ;
#88109 = UNCERTAINTY_MEASURE_WITH_UNIT (LENGTH_MEASURE( 1.000000000000000082E-05 ), #116066, 'distance_accuracy_value', 'NONE');
#88110 = VECTOR ( 'NONE', #99483, 1000.000000000000000 ) ;
#88111 = DIRECTION ( 'NONE',  ( 1.000000000000000000, 0.000000000000000000, 0.000000000000000000 ) ) ;
#88112 = LINE ( 'NONE', #132361, #45967 ) ;
#88113 = CARTESIAN_POINT ( 'NONE',  ( 85.82919371712955581, -3.975000000000001865, 6.884901960086284411 ) ) ;
#88114 = FACE_OUTER_BOUND ( 'NONE', #79642, .T. ) ;
#88115 = DIRECTION ( 'NONE',  ( -1.000000000000000000, -1.224606353822377258E-16, -0.000000000000000000 ) ) ;
#88116 = VERTEX_POINT ( 'NONE', #135344 ) ;
#88117 = CARTESIAN_POINT ( 'NONE',  ( 70.12500000000000000, -7.950000000000000178, -4.867971026610729436E-16 ) ) ;
#88118 = FACE_OUTER_BOUND ( 'NONE', #143216, .T. ) ;
#88119 = CARTESIAN_POINT ( 'NONE',  ( 174.7500000000000000, 7.919999999999947526, 21.67769999999990915 ) ) ;
#88120 = DIRECTION ( 'NONE',  ( -0.000000000000000000, -0.3543493200069152693, 0.9351131265310292928 ) ) ;
#88121 = EDGE_LOOP ( 'NONE', ( #120767, #55683, #105845 ) ) ;
#88122 =( BOUNDED_CURVE ( )  B_SPLINE_CURVE ( 2, ( #47566, #92419, #2553, #90293, #91724, #14158, #91048, #56995, #101169, #134547, #112765, #25755, #1129 ),
 .UNSPECIFIED., .F., .F. ) 
 B_SPLINE_CURVE_WITH_KNOTS ( ( 3, 2, 2, 2, 2, 2, 3 ),
 ( 0.8666666666666666963, 0.8694444444444444642, 0.8722222222222222321, 0.8750000000000000000, 0.8777777777777777679, 0.8805555555555555358, 0.8833333333333333037 ),
 .UNSPECIFIED. ) 
 CURVE ( )  GEOMETRIC_REPRESENTATION_ITEM ( )  RATIONAL_B_SPLINE_CURVE ( ( 1.000000000000000000, 0.9659258262890683122, 1.000000000000000000, 0.9659258262890683122, 1.000000000000000000, 0.9659258262890683122, 1.000000000000000000, 0.9659258262890683122, 1.000000000000000000, 0.9659258262890683122, 1.000000000000000000, 0.9659258262890683122, 1.000000000000000000 ) ) 
 REPRESENTATION_ITEM ( '' )  );
#88123 = DIRECTION ( 'NONE',  ( -0.7071067811865487940, 0.7071067811865463515, 0.000000000000000000 ) ) ;
#88124 = AXIS2_PLACEMENT_3D ( 'NONE', #1322, #133313, #46326 ) ;
#88125 = ORIENTED_EDGE ( 'NONE', *, *, #112792, .T. ) ;
#88126 = CONICAL_SURFACE ( 'NONE', #104336, 2.500000000000000888, 0.9599310885968822538 ) ;
#88127 = EDGE_CURVE ( 'NONE', #134968, #89060, #47640, .T. ) ;
#88128 = CARTESIAN_POINT ( 'NONE',  ( -21.48921356237309155, -27.52281430457070499, 5.000000000000000000 ) ) ;
#88129 = CARTESIAN_POINT ( 'NONE',  ( 78.45876352523144703, 0.000000000000000000, -6.110000000000001208 ) ) ;
#88130 = CARTESIAN_POINT ( 'NONE',  ( 26.52487387214937797, 14.25929247661557397, 9.797011795316699079 ) ) ;
#88131 = ORIENTED_EDGE ( 'NONE', *, *, #50937, .F. ) ;
#88132 = VECTOR ( 'NONE', #72605, 999.9999999999998863 ) ;
#88133 = AXIS2_PLACEMENT_3D ( 'NONE', #80965, #3362, #26573 ) ;
#88134 = VECTOR ( 'NONE', #26720, 1000.000000000000000 ) ;
#88135 = AXIS2_PLACEMENT_3D ( 'NONE', #55161, #10202, #122533 ) ;
#88136 = DIRECTION ( 'NONE',  ( -0.6830127018922180770, -0.6830127018922204085, -0.2588190451025213501 ) ) ;
#88137 =( BOUNDED_CURVE ( )  B_SPLINE_CURVE ( 3, ( #7916, #19527, #139199, #18802 ),
 .UNSPECIFIED., .F., .T. ) 
 B_SPLINE_CURVE_WITH_KNOTS ( ( 4, 4 ),
 ( 1.864375635226946049, 1.933014472006540752 ),
 .UNSPECIFIED. ) 
 CURVE ( )  GEOMETRIC_REPRESENTATION_ITEM ( )  RATIONAL_B_SPLINE_CURVE ( ( 1.000000000000000000, 0.9996074310407766506, 0.9996074310407766506, 1.000000000000000000 ) ) 
 REPRESENTATION_ITEM ( '' )  );
#88139 = CARTESIAN_POINT ( 'NONE',  ( 33.48921356237309510, -27.52281430457078670, 5.000000000000000000 ) ) ;
#88138 = VECTOR ( 'NONE', #83789, 1000.000000000000227 ) ;
#88140 =( LENGTH_UNIT ( ) NAMED_UNIT ( * ) SI_UNIT ( .MILLI., .METRE. ) );
#88141 = DIRECTION ( 'NONE',  ( -0.7071067811865487940, 0.7071067811865463515, -0.000000000000000000 ) ) ;
#88142 = EDGE_CURVE ( 'NONE', #47388, #26153, #126562, .T. ) ;
#88143 = PLANE ( 'NONE',  #69454 ) ;
#88145 = ORIENTED_EDGE ( 'NONE', *, *, #68538, .F. ) ;
#88144 = DIRECTION ( 'NONE',  ( -0.6830127018922181881, 0.6830127018922202975, -0.2588190451025214056 ) ) ;
#88146 = SURFACE_SIDE_STYLE ('',( #43926 ) ) ;
#88147 = CARTESIAN_POINT ( 'NONE',  ( -1.499999999999984013, -5.947814304570766986, 5.000000000000000000 ) ) ;
#88148 = CARTESIAN_POINT ( 'NONE',  ( 20.70025512860841133, -27.71228299555191654, 4.000000000000000000 ) ) ;
#88149 = VECTOR ( 'NONE', #90627, 1000.000000000000000 ) ;
#88150 = CARTESIAN_POINT ( 'NONE',  ( -28.49999999999980460, 9.431123077392088661, 4.000000000000000000 ) ) ;
#88151 = EDGE_LOOP ( 'NONE', ( #50741, #69834, #49839, #24551 ) ) ;
#88152 = VERTEX_POINT ( 'NONE', #27252 ) ;
#88153 = CARTESIAN_POINT ( 'NONE',  ( 65.18793019189811844, 6.110000000000002984, -1.637169565754156730 ) ) ;
#88154 = ORIENTED_EDGE ( 'NONE', *, *, #126556, .F. ) ;
#88155 = DIRECTION ( 'NONE',  ( -0.000000000000000000, 0.3543493200069153248, 0.9351131265310292928 ) ) ;
#88156 = DIRECTION ( 'NONE',  ( -1.000000000000000000, -1.224606353822377258E-16, -0.000000000000000000 ) ) ;
#88157 = VECTOR ( 'NONE', #128047, 1000.000000000000000 ) ;
#88158 = CARTESIAN_POINT ( 'NONE',  ( -34.92499999999997584, 22.27000000000000668, -0.5000000000000004441 ) ) ;
#88159 = DIRECTION ( 'NONE',  ( 0.6830127018922180770, -0.6830127018922204085, -0.2588190451025213501 ) ) ;
#88160 = ORIENTED_EDGE ( 'NONE', *, *, #114508, .F. ) ;
#88161 = EDGE_LOOP ( 'NONE', ( #3123, #139739, #112946, #26508 ) ) ;
#88162 = CARTESIAN_POINT ( 'NONE',  ( -12.20000000000000462, -22.33999999999998565, -0.5000000000000000000 ) ) ;
#88163 = LINE ( 'NONE', #31636, #7264 ) ;
#88164 = AXIS2_PLACEMENT_3D ( 'NONE', #51611, #95804, #140050 ) ;
#88165 = ORIENTED_EDGE ( 'NONE', *, *, #48184, .F. ) ;
#88166 = VECTOR ( 'NONE', #112731, 1000.000000000000000 ) ;
#88167 = CARTESIAN_POINT ( 'NONE',  ( 0.7928932188134554249, -14.24070752338414003, 5.000000000000000000 ) ) ;
#88168 = AXIS2_PLACEMENT_3D ( 'NONE', #108046, #131265, #8713 ) ;
#88169 = CARTESIAN_POINT ( 'NONE',  ( 12.08840764549667668, 9.139736423841732040E-16, 0.000000000000000000 ) ) ;
#88170 = CARTESIAN_POINT ( 'NONE',  ( -8.700255128608413102, -27.71228299555199825, 4.000000000000000000 ) ) ;
#88171 = AXIS2_PLACEMENT_3D ( 'NONE', #92335, #60482, #4567 ) ;
#88172 = ORIENTED_EDGE ( 'NONE', *, *, #103498, .T. ) ;
#88173 = FACE_BOUND ( 'NONE', #76785, .T. ) ;
#88174 = CARTESIAN_POINT ( 'NONE',  ( 18.48921356237309510, -27.52281430457068367, 5.000000000000000000 ) ) ;
#88175 = CARTESIAN_POINT ( 'NONE',  ( 128.4511022459138019, -4.648522628062369932, -4.648522628062369932 ) ) ;
#88176 = CARTESIAN_POINT ( 'NONE',  ( -24.48921356237309510, -27.52281430457072631, 5.000000000000000000 ) ) ;
#88177 = LINE ( 'NONE', #20754, #92053 ) ;
#88178 = CARTESIAN_POINT ( 'NONE',  ( 15.48921356237309510, -27.52281430457066236, 5.000000000000000000 ) ) ;
#88179 = SHAPE_REPRESENTATION_RELATIONSHIP ( 'NONE' , 'NONE' ,  #54265, #77733 ) ;
#88180 = ORIENTED_EDGE ( 'NONE', *, *, #10555, .F. ) ;
#88181 = EDGE_CURVE ( 'NONE', #136292, #70943, #25107, .T. ) ;
#88182 = ORIENTED_EDGE ( 'NONE', *, *, #28110, .F. ) ;
#88183 = CARTESIAN_POINT ( 'NONE',  ( 113.0787635252314516, -7.482591942790325086E-16, 6.109999999999998543 ) ) ;
#88184 = EDGE_LOOP ( 'NONE', ( #104143, #75522, #81279, #8307 ) ) ;
#88185 = ADVANCED_FACE ( 'NONE', ( #46939 ), #136024, .T. ) ;
#88186 = EDGE_CURVE ( 'NONE', #109145, #123719, #49770, .T. ) ;
#88187 = VERTEX_POINT ( 'NONE', #70803 ) ;
#88188 = ADVANCED_FACE ( 'NONE', ( #69368 ), #68656, .F. ) ;
#88189 = DIRECTION ( 'NONE',  ( -0.7071067811865486830, -0.7071067811865464625, 0.000000000000000000 ) ) ;
#88190 = EDGE_CURVE ( 'NONE', #37517, #93975, #70114, .T. ) ;
#88191 = PLANE ( 'NONE',  #57121 ) ;
#88192 = PLANE ( 'NONE',  #59032 ) ;
#88193 = ORIENTED_EDGE ( 'NONE', *, *, #92296, .F. ) ;
#88194 = PLANE ( 'NONE',  #59996 ) ;
#88195 = CARTESIAN_POINT ( 'NONE',  ( -66.18398860626901126, 28.73617430169833753, 5.000000000000000000 ) ) ;
#88196 = CARTESIAN_POINT ( 'NONE',  ( 37.16666666666666430, 6.884901960086285300, 3.975000000000003642 ) ) ;
#88197 = EDGE_CURVE ( 'NONE', #134440, #44739, #91801, .T. ) ;
#88199 = CARTESIAN_POINT ( 'NONE',  ( 58.26669371712954870, -7.949999999999998401, 2.130196079827423983 ) ) ;
#88198 = PLANE ( 'NONE',  #110499 ) ;
#88200 = DIRECTION ( 'NONE',  ( 0.6830127018922180770, -0.6830127018922204085, -0.2588190451025213501 ) ) ;
#88201 = VECTOR ( 'NONE', #71656, 999.9999999999998863 ) ;
#88202 = DIRECTION ( 'NONE',  ( 0.7071067811865487940, 0.7071067811865463515, -0.000000000000000000 ) ) ;
#88203 = ORIENTED_EDGE ( 'NONE', *, *, #91827, .T. ) ;
#88204 = DIRECTION ( 'NONE',  ( -0.7071067811865486830, 0.7071067811865464625, 0.000000000000000000 ) ) ;
#88205 = DIRECTION ( 'NONE',  ( 0.7071067811865487940, 0.7071067811865463515, -0.000000000000000000 ) ) ;
#88206 = EDGE_CURVE ( 'NONE', #87113, #51885, #38865, .T. ) ;
#88207 = EDGE_LOOP ( 'NONE', ( #141270, #138261, #117036, #69541 ) ) ;
#88208 = ORIENTED_EDGE ( 'NONE', *, *, #78901, .T. ) ;
#88209 = ADVANCED_FACE ( 'NONE', ( #80952 ), #83085, .T. ) ;
#88210 = VERTEX_POINT ( 'NONE', #81685 ) ;
#88211 = CARTESIAN_POINT ( 'NONE',  ( 68.10459685856474721, 1.637169565754164946, -6.109999999999999432 ) ) ;
#88212 = VECTOR ( 'NONE', #51402, 1000.000000000000000 ) ;
#88213 = ORIENTED_EDGE ( 'NONE', *, *, #36660, .F. ) ;
#88214 = ADVANCED_FACE ( 'NONE', ( #25837 ), #13507, .T. ) ;
#88215 = CARTESIAN_POINT ( 'NONE',  ( 57.18398860626899705, 28.73617430169827358, 5.000000000000000000 ) ) ;
#88216 = CARTESIAN_POINT ( 'NONE',  ( -2.141693717129561136, -1.633150327867689988, 6.094999999999989981 ) ) ;
#88217 = CARTESIAN_POINT ( 'NONE',  ( 98.58376352523144703, -6.110000000000001208, -3.741295971395164515E-16 ) ) ;
#88218 = LINE ( 'NONE', #120819, #102999 ) ;
#88219 = VERTEX_POINT ( 'NONE', #104085 ) ;
#88220 = DIRECTION ( 'NONE',  ( -0.7071067811865486830, -0.7071067811865464625, 0.000000000000000000 ) ) ;
#88221 = FACE_OUTER_BOUND ( 'NONE', #91554, .T. ) ;
#88222 = LINE ( 'NONE', #101942, #76865 ) ;
#88223 = CARTESIAN_POINT ( 'NONE',  ( 26.90156419391746923, 11.25929247661560240, 10.79108189686413333 ) ) ;
#88225 = ORIENTED_EDGE ( 'NONE', *, *, #31790, .T. ) ;
#88224 = AXIS2_PLACEMENT_3D ( 'NONE', #55013, #50902, #95095 ) ;
#88226 = VERTEX_POINT ( 'NONE', #138181 ) ;
#88227 = VERTEX_POINT ( 'NONE', #114275 ) ;
#88228 = EDGE_LOOP ( 'NONE', ( #120140, #108532, #14372, #36090 ) ) ;
#88229 = EDGE_CURVE ( 'NONE', #124891, #75364, #4738, .T. ) ;
#88230 = CARTESIAN_POINT ( 'NONE',  ( 122.2662635252314374, 4.472830434245838482, -4.472830434245837594 ) ) ;
#88231 = VECTOR ( 'NONE', #91982, 1000.000000000000000 ) ;
#88232 = AXIS2_PLACEMENT_3D ( 'NONE', #14806, #134465, #35169 ) ;
#88233 = AXIS2_PLACEMENT_3D ( 'NONE', #28717, #29399, #52581 ) ;
#88234 = VECTOR ( 'NONE', #13584, 1000.000000000000114 ) ;
#88235 = VECTOR ( 'NONE', #141543, 999.9999999999998863 ) ;
#88236 = CARTESIAN_POINT ( 'NONE',  ( 48.18398860626899705, 28.73617430169820608, 5.000000000000000000 ) ) ;
#88237 = CARTESIAN_POINT ( 'NONE',  ( -7.499999999999944045, -19.91253812416055524, 4.000000000000000000 ) ) ;
#88238 = VERTEX_POINT ( 'NONE', #114948 ) ;
#88239 = FACE_OUTER_BOUND ( 'NONE', #61335, .T. ) ;
#88241 = EDGE_LOOP ( 'NONE', ( #115050, #109254, #143052, #34288 ) ) ;
#88240 = VECTOR ( 'NONE', #9842, 1000.000000000000000 ) ;
#88242 = CARTESIAN_POINT ( 'NONE',  ( 8.728736474768551190, 5.808823158059031044, -5.808823158059038150 ) ) ;
#88243 = PLANE ( 'NONE',  #30051 ) ;
#88244 = CARTESIAN_POINT ( 'NONE',  ( 45.48921356237309510, -27.52281430457087197, 5.000000000000000000 ) ) ;
#88245 = AXIS2_PLACEMENT_3D ( 'NONE', #39526, #85142, #72901 ) ;
#88246 = PLANE ( 'NONE',  #55947 ) ;
#88247 = EDGE_LOOP ( 'NONE', ( #66117, #140174, #22238, #22258 ) ) ;
#88248 = ORIENTED_EDGE ( 'NONE', *, *, #108949, .T. ) ;
#88249 = EDGE_CURVE ( 'NONE', #23176, #79521, #15627, .T. ) ;
#88250 = ORIENTED_EDGE ( 'NONE', *, *, #28856, .T. ) ;
#88252 = COLOUR_RGB ( '', 0.66274510, 0.83137255, 0.94901961) ;
#88251 = DIRECTION ( 'NONE',  ( 0.000000000000000000, -1.000000000000000000, 0.000000000000000000 ) ) ;
#88253 = PLANE ( 'NONE',  #97291 ) ;
#88254 = UNCERTAINTY_MEASURE_WITH_UNIT (LENGTH_MEASURE( 1.000000000000000082E-05 ), #118250, 'distance_accuracy_value', 'NONE');
#88255 = FACE_OUTER_BOUND ( 'NONE', #19227, .T. ) ;
#88256 = DIRECTION ( 'NONE',  ( 1.000000000000000000, 0.000000000000000000, 0.000000000000000000 ) ) ;
#88257 = CONICAL_SURFACE ( 'NONE', #95171, 2.552699999999928693, 1.029744258676634772 ) ;
#88258 = AXIS2_PLACEMENT_3D ( 'NONE', #66586, #121647, #68743 ) ;
#88259 = DIRECTION ( 'NONE',  ( 2.781805975412906507E-17, 0.3543493200069153248, 0.9351131265310292928 ) ) ;
#88260 = CARTESIAN_POINT ( 'NONE',  ( -13.49999999999990052, -13.53360074219760278, 5.000000000000000000 ) ) ;
#88261 = ADVANCED_FACE ( 'NONE', ( #38164 ), #109868, .T. ) ;
#88262 = LINE ( 'NONE', #67217, #9652 ) ;
#88263 = LINE ( 'NONE', #132513, #83658 ) ;
#88264 = AXIS2_PLACEMENT_3D ( 'NONE', #44922, #120987, #628 ) ;
#88265 = ORIENTED_EDGE ( 'NONE', *, *, #94213, .T. ) ;
#88266 = CARTESIAN_POINT ( 'NONE',  ( 39.18398860626899705, 28.73617430169814568, 5.000000000000000000 ) ) ;
#88267 = VERTEX_POINT ( 'NONE', #5492 ) ;
#88269 = CIRCLE ( 'NONE', #44306, 2.500000000000000888 ) ;
#88268 = DIRECTION ( 'NONE',  ( -0.7071067811865486830, -0.7071067811865464625, -0.000000000000000000 ) ) ;
#88270 = ORIENTED_EDGE ( 'NONE', *, *, #94131, .F. ) ;
#88271 = CARTESIAN_POINT ( 'NONE',  ( 18.63425672184678916, 4.584330080086930965E-16, 0.000000000000000000 ) ) ;
#88273 = VERTEX_POINT ( 'NONE', #93948 ) ;
#88272 = CARTESIAN_POINT ( 'NONE',  ( 42.12499999999999289, -7.950000000000000178, -4.867971026610729436E-16 ) ) ;
#88274 = EDGE_CURVE ( 'NONE', #36132, #68120, #19252, .T. ) ;
#88275 = VECTOR ( 'NONE', #102369, 999.9999999999998863 ) ;
#88276 = CARTESIAN_POINT ( 'NONE',  ( 14.81601139373099585, 28.73617430169776910, 5.000000000000000000 ) ) ;
#88277 = ORIENTED_EDGE ( 'NONE', *, *, #110487, .T. ) ;
#88278 = CARTESIAN_POINT ( 'NONE',  ( 15.18398860626900237, 28.73617430169797871, 5.000000000000000000 ) ) ;
#88279 = VERTEX_POINT ( 'NONE', #6186 ) ;
#88280 = CARTESIAN_POINT ( 'NONE',  ( 19.69064382391260892, -2.759520746520534473, 4.000000000000000000 ) ) ;
#88281 = UNCERTAINTY_MEASURE_WITH_UNIT (LENGTH_MEASURE( 1.000000000000000082E-05 ), #66192, 'distance_accuracy_value', 'NONE');
#88282 = ORIENTED_EDGE ( 'NONE', *, *, #131278, .T. ) ;
#88283 = CARTESIAN_POINT ( 'NONE',  ( 5.510786437626906675, -27.52281430457051314, 5.000000000000000000 ) ) ;
#88284 = CARTESIAN_POINT ( 'NONE',  ( 113.6833603837962272, -2.130196079827426203, 7.949999999999997513 ) ) ;
#88285 = DIRECTION ( 'NONE',  ( -1.000000000000000000, -0.000000000000000000, -0.000000000000000000 ) ) ;
#88286 = AXIS2_PLACEMENT_3D ( 'NONE', #89339, #111814, #67623 ) ;
#88287 = LINE ( 'NONE', #55660, #89908 ) ;
#88288 = DIRECTION ( 'NONE',  ( -0.7071067811865486830, -0.7071067811865464625, 0.000000000000000000 ) ) ;
#88289 = CARTESIAN_POINT ( 'NONE',  ( 4.499999999999966249, 11.52377502935403264, -1.522421517564095161 ) ) ;
#88290 = PLANE ( 'NONE',  #85458 ) ;
#88292 = VECTOR ( 'NONE', #115192, 1000.000000000000000 ) ;
#88291 = CARTESIAN_POINT ( 'NONE',  ( 17.93750000000000355, -4.461849672132299105, 4.461849672132299993 ) ) ;
#88293 = CARTESIAN_POINT ( 'NONE',  ( 13.83290314143522082, -3.967499999999994476, 6.871911579029513106 ) ) ;
#88295 = AXIS2_PLACEMENT_3D ( 'NONE', #25114, #135354, #13515 ) ;
#88294 = DIRECTION ( 'NONE',  ( -0.000000000000000000, -0.3543493200069152693, 0.9351131265310292928 ) ) ;
#88296 = FACE_OUTER_BOUND ( 'NONE', #8111, .T. ) ;
#88297 = ORIENTED_EDGE ( 'NONE', *, *, #80588, .F. ) ;
#88298 = ORIENTED_EDGE ( 'NONE', *, *, #45704, .F. ) ;
#88299 = LINE ( 'NONE', #33237, #53677 ) ;
#88300 = EDGE_LOOP ( 'NONE', ( #21873, #48417, #56954, #78509 ) ) ;
#88301 = ADVANCED_FACE ( 'NONE', ( #18501 ), #9029, .T. ) ;
#88302 = EDGE_CURVE ( 'NONE', #75268, #92497, #39597, .T. ) ;
#88303 = AXIS2_PLACEMENT_3D ( 'NONE', #98460, #95598, #9262 ) ;
#88304 = LINE ( 'NONE', #56427, #68879 ) ;
#88305 = LINE ( 'NONE', #1252, #78736 ) ;
#88307 = VECTOR ( 'NONE', #9393, 1000.000000000000000 ) ;
#88306 = CARTESIAN_POINT ( 'NONE',  ( -16.17183060077635304, -2.240707523384264377, 4.000000000000000000 ) ) ;
#88308 = FACE_OUTER_BOUND ( 'NONE', #118171, .T. ) ;
#88309 = ORIENTED_EDGE ( 'NONE', *, *, #89271, .T. ) ;
#88310 = DIRECTION ( 'NONE',  ( -0.7071067811865487940, 0.7071067811865463515, -0.000000000000000000 ) ) ;
#88311 = CYLINDRICAL_SURFACE ( 'NONE', #11781, 2.500000000000000000 ) ;
#88312 = CARTESIAN_POINT ( 'NONE',  ( -26.99451991528749417, 28.92564299267956685, 4.000000000000000000 ) ) ;
#88313 = EDGE_CURVE ( 'NONE', #71584, #89949, #30865, .T. ) ;
#88314 = EDGE_CURVE ( 'NONE', #143176, #70301, #107674, .T. ) ;
#88315 = DIRECTION ( 'NONE',  ( 0.000000000000000000, 0.000000000000000000, -1.000000000000000000 ) ) ;
#88317 = ORIENTED_EDGE ( 'NONE', *, *, #22778, .T. ) ;
#88316 = FACE_OUTER_BOUND ( 'NONE', #102976, .T. ) ;
#88318 = CARTESIAN_POINT ( 'NONE',  ( -25.39999999999996305, 3.061616997868383141E-16, -2.500000000000000000 ) ) ;
#88319 = DIRECTION ( 'NONE',  ( -0.7071067811865487940, 0.7071067811865463515, -0.000000000000000000 ) ) ;
#88320 = AXIS2_PLACEMENT_3D ( 'NONE', #117478, #116067, #93623 ) ;
#88321 = SURFACE_SIDE_STYLE ('',( #561 ) ) ;
#88322 = DIRECTION ( 'NONE',  ( 0.7071067811865487940, 0.7071067811865463515, -0.000000000000000000 ) ) ;
#88323 =( BOUNDED_CURVE ( )  B_SPLINE_CURVE ( 3, ( #75555, #97252, #19723, #107446 ),
 .UNSPECIFIED., .F., .T. ) 
 B_SPLINE_CURVE_WITH_KNOTS ( ( 4, 4 ),
 ( 5.005968288816722733, 5.074607125596334534 ),
 .UNSPECIFIED. ) 
 CURVE ( )  GEOMETRIC_REPRESENTATION_ITEM ( )  RATIONAL_B_SPLINE_CURVE ( ( 1.000000000000000000, 0.9996074310407765395, 0.9996074310407765395, 1.000000000000000000 ) ) 
 REPRESENTATION_ITEM ( '' )  );
#88324 = CARTESIAN_POINT ( 'NONE',  ( -6.299744871391586898, -27.71228299555210484, 4.000000000000000000 ) ) ;
#88325 = VERTEX_POINT ( 'NONE', #129427 ) ;
#88326 = EDGE_LOOP ( 'NONE', ( #2637, #37481, #134779 ) ) ;
#88327 = ORIENTED_EDGE ( 'NONE', *, *, #88181, .F. ) ;
#88328 =( BOUNDED_CURVE ( )  B_SPLINE_CURVE ( 3, ( #122452, #76118, #66676, #98569 ),
 .UNSPECIFIED., .F., .F. ) 
 B_SPLINE_CURVE_WITH_KNOTS ( ( 4, 4 ),
 ( 2.779374508378135378, 4.199602562396796301 ),
 .UNSPECIFIED. ) 
 CURVE ( )  GEOMETRIC_REPRESENTATION_ITEM ( )  RATIONAL_B_SPLINE_CURVE ( ( 1.000000000000000000, 0.8388583629366721528, 0.8388583629366721528, 1.000000000000000000 ) ) 
 REPRESENTATION_ITEM ( '' )  );
#88329 = CARTESIAN_POINT ( 'NONE',  ( 88.95876352523143282, 0.000000000000000000, -6.110000000000001208 ) ) ;
#88330 = ORIENTED_EDGE ( 'NONE', *, *, #70071, .F. ) ;
#88331 = FACE_OUTER_BOUND ( 'NONE', #112518, .T. ) ;
#88332 = CARTESIAN_POINT ( 'NONE',  ( 85.39169371712957002, 2.130196079827421762, 7.950000000000000178 ) ) ;
#88333 = ORIENTED_EDGE ( 'NONE', *, *, #29195, .T. ) ;
#88334 = VECTOR ( 'NONE', #65081, 1000.000000000000000 ) ;
#88335 = EDGE_CURVE ( 'NONE', #84441, #83371, #124959, .T. ) ;
#88336 = CARTESIAN_POINT ( 'NONE',  ( 183.4786297241425927, -52.14999999999999147, 41.05044666116288710 ) ) ;
#88337 = CARTESIAN_POINT ( 'NONE',  ( 49.99999999999998579, 0.000000000000000000, -7.950000000000000178 ) ) ;
#88338 = VECTOR ( 'NONE', #84315, 999.9999999999998863 ) ;
#88339 = AXIS2_PLACEMENT_3D ( 'NONE', #119869, #77153, #20574 ) ;
#88340 = CARTESIAN_POINT ( 'NONE',  ( 83.18293019189810877, -1.637169565754158951, -6.109999999999998543 ) ) ;
#88341 = ORIENTED_EDGE ( 'NONE', *, *, #35720, .F. ) ;
#88342 = FACE_OUTER_BOUND ( 'NONE', #51986, .T. ) ;
#88343 = AXIS2_PLACEMENT_3D ( 'NONE', #95546, #128888, #116594 ) ;
#88344 = AXIS2_PLACEMENT_3D ( 'NONE', #46617, #1584, #56041 ) ;
#88345 = DIRECTION ( 'NONE',  ( 0.000000000000000000, 0.000000000000000000, 1.000000000000000000 ) ) ;
#88346 = AXIS2_PLACEMENT_3D ( 'NONE', #96248, #41181, #129614 ) ;
#88347 = VECTOR ( 'NONE', #35408, 999.9999999999998863 ) ;
#88348 = VECTOR ( 'NONE', #7241, 1000.000000000000000 ) ;
#88349 = ORIENTED_EDGE ( 'NONE', *, *, #7019, .T. ) ;
#88350 = ORIENTED_EDGE ( 'NONE', *, *, #119993, .T. ) ;
#88351 = ORIENTED_EDGE ( 'NONE', *, *, #23331, .F. ) ;
#88352 = DIRECTION ( 'NONE',  ( 1.000000000000000000, 0.000000000000000000, 0.000000000000000000 ) ) ;
#88353 = DIRECTION ( 'NONE',  ( -0.000000000000000000, 0.3543493200069153248, 0.9351131265310292928 ) ) ;
#88354 = DIRECTION ( 'NONE',  ( 0.7071067811865486830, -0.7071067811865464625, -0.000000000000000000 ) ) ;
#88355 = AXIS2_PLACEMENT_3D ( 'NONE', #60528, #59112, #105407 ) ;
#88356 = DIRECTION ( 'NONE',  ( -0.7071067811865487940, 0.7071067811865463515, -0.000000000000000000 ) ) ;
#88357 = LINE ( 'NONE', #121658, #104259 ) ;
#88358 = CARTESIAN_POINT ( 'NONE',  ( -27.80025329279436264, -22.22500000000000142, 2.300167135621889791 ) ) ;
#88359 = EDGE_CURVE ( 'NONE', #48675, #38058, #74361, .T. ) ;
#88360 = ORIENTED_EDGE ( 'NONE', *, *, #40272, .F. ) ;
#88361 = VERTEX_POINT ( 'NONE', #8334 ) ;
#88362 = VECTOR ( 'NONE', #11845, 1000.000000000000000 ) ;
#88363 = ADVANCED_FACE ( 'NONE', ( #72963 ), #117812, .F. ) ;
#88364 = ORIENTED_EDGE ( 'NONE', *, *, #114951, .T. ) ;
#88365 = EDGE_LOOP ( 'NONE', ( #136968, #5447, #41480, #12948 ) ) ;
#88366 = ADVANCED_FACE ( 'NONE', ( #141013 ), #72256, .F. ) ;
#88367 = EDGE_CURVE ( 'NONE', #36502, #50807, #112258, .T. ) ;
#88368 = AXIS2_PLACEMENT_3D ( 'NONE', #76057, #64460, #55031 ) ;
#88369 = VECTOR ( 'NONE', #109902, 1000.000000000000000 ) ;
#88370 = EDGE_LOOP ( 'NONE', ( #503, #22589, #91984, #30379 ) ) ;
#88371 = FACE_OUTER_BOUND ( 'NONE', #105629, .T. ) ;
#88372 = LINE ( 'NONE', #98510, #32206 ) ;
#88373 = AXIS2_PLACEMENT_3D ( 'NONE', #49379, #81281, #60243 ) ;
#88374 = DIRECTION ( 'NONE',  ( -0.3543493200069162685, -0.000000000000000000, -0.9351131265310288487 ) ) ;
#88375 = DIRECTION ( 'NONE',  ( -0.6830127018922180770, -0.6830127018922204085, -0.2588190451025213501 ) ) ;
#88376 = AXIS2_PLACEMENT_3D ( 'NONE', #139108, #106417, #95578 ) ;
#88377 = CARTESIAN_POINT ( 'NONE',  ( 118.3958333333333286, -2.130196079827369804, 7.950000000000031264 ) ) ;
#88378 = VERTEX_POINT ( 'NONE', #83831 ) ;
#88379 = CARTESIAN_POINT ( 'NONE',  ( 30.18398860626900060, 28.73617430169808173, 5.000000000000000000 ) ) ;
#88380 = EDGE_CURVE ( 'NONE', #89658, #103863, #97504, .T. ) ;
#88381 = ORIENTED_EDGE ( 'NONE', *, *, #132767, .F. ) ;
#88382 = CARTESIAN_POINT ( 'NONE',  ( 19.93303239253585346, -3.242521478231688015, -35.72961117458194735 ) ) ;
#88383 = ORIENTED_EDGE ( 'NONE', *, *, #97915, .T. ) ;
#88384 = PLANE ( 'NONE',  #39915 ) ;
#88385 = EDGE_CURVE ( 'NONE', #100921, #71118, #21231, .T. ) ;
#88386 = ORIENTED_EDGE ( 'NONE', *, *, #120509, .T. ) ;
#88387 = DIRECTION ( 'NONE',  ( 0.7071067811865487940, 0.7071067811865463515, 0.000000000000000000 ) ) ;
#88388 = ORIENTED_EDGE ( 'NONE', *, *, #91236, .F. ) ;
#88389 = ORIENTED_EDGE ( 'NONE', *, *, #128334, .T. ) ;
#88390 = AXIS2_PLACEMENT_3D ( 'NONE', #101735, #24185, #77167 ) ;
#88391 = VERTEX_POINT ( 'NONE', #127287 ) ;
#88392 = EDGE_CURVE ( 'NONE', #31545, #60397, #116426, .T. ) ;
#88393 = DIRECTION ( 'NONE',  ( 1.000000000000000000, 0.000000000000000000, 0.000000000000000000 ) ) ;
#88394 = FACE_OUTER_BOUND ( 'NONE', #134360, .T. ) ;
#88395 = CARTESIAN_POINT ( 'NONE',  ( 33.48921356237309510, -27.52281430457078670, 5.000000000000000000 ) ) ;
#88396 = DIRECTION ( 'NONE',  ( -1.000000000000000000, -1.224606353822377258E-16, -0.000000000000000000 ) ) ;
#88397 = DIRECTION ( 'NONE',  ( -0.7071067811865486830, 0.7071067811865464625, 0.000000000000000000 ) ) ;
#88399 = DIRECTION ( 'NONE',  ( 0.7071067811865487940, 0.7071067811865463515, 0.000000000000000000 ) ) ;
#88398 = VECTOR ( 'NONE', #10201, 1000.000000000000114 ) ;
#88400 = EDGE_CURVE ( 'NONE', #4583, #32218, #61380, .T. ) ;
#88401 = VECTOR ( 'NONE', #95919, 1000.000000000000000 ) ;
#88402 = DIRECTION ( 'NONE',  ( -0.7071067811865486830, -0.7071067811865464625, 0.000000000000000000 ) ) ;
#88403 = PLANE ( 'NONE',  #96820 ) ;
#88404 = DIRECTION ( 'NONE',  ( 0.7071067811865486830, -0.7071067811865464625, -0.000000000000000000 ) ) ;
#88405 = CARTESIAN_POINT ( 'NONE',  ( 0.000000000000000000, 0.000000000000000000, 5.000000000000000000 ) ) ;
#88406 = VERTEX_POINT ( 'NONE', #50462 ) ;
#88407 = EDGE_LOOP ( 'NONE', ( #137925, #69562, #124203, #98390, #66456, #133801 ) ) ;
#88409 = ORIENTED_EDGE ( 'NONE', *, *, #53866, .T. ) ;
#88408 = EDGE_CURVE ( 'NONE', #59855, #133129, #128407, .T. ) ;
#88410 = AXIS2_PLACEMENT_3D ( 'NONE', #122461, #67414, #10142 ) ;
#88411 = CARTESIAN_POINT ( 'NONE',  ( 41.99451991528749062, 28.92564299267967343, 4.000000000000000000 ) ) ;
#88412 = VERTEX_POINT ( 'NONE', #128039 ) ;
#88413 = ORIENTED_EDGE ( 'NONE', *, *, #38590, .F. ) ;
#88414 = LINE ( 'NONE', #78250, #111647 ) ;
#88415 = CARTESIAN_POINT ( 'NONE',  ( 12.70710678118645731, -9.740707523384184441, 5.000000000000000000 ) ) ;
#88416 = CARTESIAN_POINT ( 'NONE',  ( -28.49999999999979750, -1.912538124160733766, 4.000000000000000000 ) ) ;
#88417 = DIRECTION ( 'NONE',  ( 0.6830127018922181881, 0.6830127018922202975, -0.2588190451025214056 ) ) ;
#88418 = EDGE_CURVE ( 'NONE', #63455, #50077, #140318, .T. ) ;
#88419 = ORIENTED_EDGE ( 'NONE', *, *, #58124, .F. ) ;
#88420 = EDGE_CURVE ( 'NONE', #114304, #17773, #143168, .T. ) ;
#88421 = LINE ( 'NONE', #109432, #76523 ) ;
#88422 = VERTEX_POINT ( 'NONE', #58172 ) ;
#88423 = CARTESIAN_POINT ( 'NONE',  ( 13.49999999999990408, -13.91253812416061386, 4.000000000000000000 ) ) ;
#88424 = ADVANCED_FACE ( 'NONE', ( #25473 ), #126128, .T. ) ;
#88425 = CARTESIAN_POINT ( 'NONE',  ( 22.37956980810188767, 3.967499999999998916, 6.871911579029510442 ) ) ;
#88426 = VERTEX_POINT ( 'NONE', #87373 ) ;
#88427 = CARTESIAN_POINT ( 'NONE',  ( 86.82876352523145158, 0.000000000000000000, -6.109999999999999432 ) ) ;
#88428 = CARTESIAN_POINT ( 'NONE',  ( 6.094872978304351818, -9.434020220044425642, 1.153095517109193668 ) ) ;
#88429 = DIRECTION ( 'NONE',  ( 0.000000000000000000, -0.2555582702174445942, 0.9667936545734397980 ) ) ;
#88430 = ORIENTED_EDGE ( 'NONE', *, *, #81805, .F. ) ;
#88431 = CARTESIAN_POINT ( 'NONE',  ( -2.999999999999981792, 14.58746187583910903, 4.000000000000000000 ) ) ;
#88432 = VERTEX_POINT ( 'NONE', #65664 ) ;
#88433 = ORIENTED_EDGE ( 'NONE', *, *, #79015, .F. ) ;
#88434 = DIRECTION ( 'NONE',  ( -0.000000000000000000, 0.3543493200069153248, 0.9351131265310292928 ) ) ;
#88435 = DIRECTION ( 'NONE',  ( -0.3543493200069162685, -0.000000000000000000, -0.9351131265310288487 ) ) ;
#88436 = DIRECTION ( 'NONE',  ( 0.7071067811865487940, 0.7071067811865463515, -0.000000000000000000 ) ) ;
#88438 = DIRECTION ( 'NONE',  ( 0.6830127018922181881, 0.6830127018922202975, -0.2588190451025214056 ) ) ;
#88437 = VECTOR ( 'NONE', #58132, 1000.000000000000000 ) ;
#88439 = CARTESIAN_POINT ( 'NONE',  ( 42.48921356237308800, -27.52281430457085065, 5.000000000000000000 ) ) ;
#88440 = ORIENTED_EDGE ( 'NONE', *, *, #67840, .T. ) ;
#88441 = VECTOR ( 'NONE', #112812, 999.9999999999998863 ) ;
#88442 = CARTESIAN_POINT ( 'NONE',  ( 21.00000000000000000, 0.000000000000000000, 6.094999999999989981 ) ) ;
#88443 = VECTOR ( 'NONE', #45, 1000.000000000000227 ) ;
#88444 = CARTESIAN_POINT ( 'NONE',  ( -60.29974487139158867, -27.71228299555248142, 4.000000000000000000 ) ) ;
#88445 = ORIENTED_EDGE ( 'NONE', *, *, #87129, .T. ) ;
#88446 = CARTESIAN_POINT ( 'NONE',  ( -45.48921356237309510, -27.52281430457087197, 5.000000000000000000 ) ) ;
#88447 = VECTOR ( 'NONE', #106087, 1000.000000000000000 ) ;
#88448 = VECTOR ( 'NONE', #96103, 1000.000000000000000 ) ;
#88449 = PRESENTATION_LAYER_ASSIGNMENT (  '', '', ( #83915 ) ) ;
#88450 = VECTOR ( 'NONE', #25346, 1000.000000000000000 ) ;
#88451 = DIRECTION ( 'NONE',  ( -0.6830127018922180770, -0.6830127018922204085, -0.2588190451025213501 ) ) ;
#88452 = ORIENTED_EDGE ( 'NONE', *, *, #132595, .T. ) ;
#88454 = ORIENTED_EDGE ( 'NONE', *, *, #139782, .T. ) ;
#88453 = DIRECTION ( 'NONE',  ( 0.7071067811865487940, 0.7071067811865463515, 0.000000000000000000 ) ) ;
#88455 = ORIENTED_EDGE ( 'NONE', *, *, #30766, .F. ) ;
#88456 = CARTESIAN_POINT ( 'NONE',  ( 37.96659967656954393, 6.759292476615656575, 12.28218704918530868 ) ) ;
#88457 = CARTESIAN_POINT ( 'NONE',  ( 72.48921356237309510, -27.52281430457106026, 5.000000000000000000 ) ) ;
#88458 = ORIENTED_EDGE ( 'NONE', *, *, #142457, .F. ) ;
#88459 = UNCERTAINTY_MEASURE_WITH_UNIT (LENGTH_MEASURE( 1.000000000000000082E-05 ), #123409, 'distance_accuracy_value', 'NONE');
#88460 = CARTESIAN_POINT ( 'NONE',  ( -34.92500000000001137, 22.22500000000000142, 4.000000000000000000 ) ) ;
#88461 = CARTESIAN_POINT ( 'NONE',  ( 28.74845587132407587, -11.24070752338416135, 10.39518518046002704 ) ) ;
#88462 = FACE_OUTER_BOUND ( 'NONE', #18813, .T. ) ;
#88463 = LINE ( 'NONE', #132704, #14155 ) ;
#88464 = DIRECTION ( 'NONE',  ( 0.7071067811865487940, 0.7071067811865463515, -0.000000000000000000 ) ) ;
#88465 = LINE ( 'NONE', #132707, #33325 ) ;
#88466 = DIRECTION ( 'NONE',  ( 0.7071067811865487940, 0.7071067811865463515, -0.000000000000000000 ) ) ;
#88467 = CARTESIAN_POINT ( 'NONE',  ( 20.54123647476855652, 0.000000000000000000, 7.934999999999990727 ) ) ;
#88468 = CARTESIAN_POINT ( 'NONE',  ( -34.92382263987071411, 21.75929247661549226, 4.252424926123421933 ) ) ;
#88469 = CARTESIAN_POINT ( 'NONE',  ( 9.156123077392344101, -22.22500000000000142, 4.000000000000000000 ) ) ;
#88470 = LINE ( 'NONE', #67441, #41909 ) ;
#88471 = CARTESIAN_POINT ( 'NONE',  ( -23.55512991947090029, -0.7407075233842665973, 4.307968247156982677 ) ) ;
#88472 = VERTEX_POINT ( 'NONE', #66347 ) ;
#88473 = VECTOR ( 'NONE', #124555, 1000.000000000000000 ) ;
#88474 = ORIENTED_EDGE ( 'NONE', *, *, #122029, .F. ) ;
#88475 = CARTESIAN_POINT ( 'NONE',  ( 104.1041666666666714, 2.130196079827422206, 7.950000000000001954 ) ) ;
#88476 = AXIS2_PLACEMENT_3D ( 'NONE', #17701, #73551, #115567 ) ;
#88477 = ORIENTED_EDGE ( 'NONE', *, *, #64009, .F. ) ;
#88478 = VERTEX_POINT ( 'NONE', #131589 ) ;
#88479 = CIRCLE ( 'NONE', #25955, 2.500000000000000444 ) ;
#88480 = VERTEX_POINT ( 'NONE', #113198 ) ;
#88481 = CARTESIAN_POINT ( 'NONE',  ( 34.47516574401890921, -5.971932658884125722, 4.998110765256833510 ) ) ;
#88482 = CARTESIAN_POINT ( 'NONE',  ( 6.328169399223483538, 17.25929247661554200, 4.000000000000000000 ) ) ;
#88483 = VECTOR ( 'NONE', #25518, 1000.000000000000000 ) ;
#88484 = EDGE_LOOP ( 'NONE', ( #30770, #109392, #37909, #94633 ) ) ;
#88485 = CARTESIAN_POINT ( 'NONE',  ( -6.489213562373093325, -27.52281430457059841, 5.000000000000000000 ) ) ;
#88486 = PLANE ( 'NONE',  #127498 ) ;
#88487 = LINE ( 'NONE', #22466, #81115 ) ;
#88488 = PLANE ( 'NONE',  #28078 ) ;
#88489 = EDGE_CURVE ( 'NONE', #75827, #2756, #85153, .T. ) ;
#88490 = ORIENTED_EDGE ( 'NONE', *, *, #48244, .T. ) ;
#88491 = CARTESIAN_POINT ( 'NONE',  ( 7.174018035375743452, 11.05446268434087465, -28.05475473402666253 ) ) ;
#88492 = EDGE_CURVE ( 'NONE', #125073, #59468, #88813, .T. ) ;
#88493 = DIRECTION ( 'NONE',  ( -0.7071067811865486830, -0.7071067811865464625, 0.000000000000000000 ) ) ;
#88494 = CARTESIAN_POINT ( 'NONE',  ( 5.755190629914537226, 4.202752102959690472E-16, 0.000000000000000000 ) ) ;
#88496 = VECTOR ( 'NONE', #82680, 999.9999999999998863 ) ;
#88495 = CARTESIAN_POINT ( 'NONE',  ( -34.49999999999975842, 16.46425560840032176, 4.994342998332164107 ) ) ;
#88497 = CARTESIAN_POINT ( 'NONE',  ( 156.1500000000000057, -57.14999999999999147, -45.92499999999969162 ) ) ;
#88498 = LINE ( 'NONE', #53730, #89400 ) ;
#88499 = DIRECTION ( 'NONE',  ( 0.7071067811865487940, 0.7071067811865463515, 0.000000000000000000 ) ) ;
#88500 = CARTESIAN_POINT ( 'NONE',  ( -20.47599861414536448, 22.03583458319437582, 4.979811245910088502 ) ) ;
#88501 = VERTEX_POINT ( 'NONE', #43871 ) ;
#88502 = ORIENTED_EDGE ( 'NONE', *, *, #1854, .F. ) ;
#88503 = CARTESIAN_POINT ( 'NONE',  ( 121.0420968585647756, 5.291415217122923842, -3.054999999999996163 ) ) ;
#88504 = ORIENTED_EDGE ( 'NONE', *, *, #62999, .T. ) ;
#88505 = ADVANCED_FACE ( 'NONE', ( #77931 ), #13873, .T. ) ;
#88506 = AXIS2_PLACEMENT_3D ( 'NONE', #36264, #4260, #124688 ) ;
#88507 = DIRECTION ( 'NONE',  ( 0.000000000000000000, 0.000000000000000000, -1.000000000000000000 ) ) ;
#88508 = AXIS2_PLACEMENT_3D ( 'NONE', #1236, #44824, #22267 ) ;
#88509 = LINE ( 'NONE', #100089, #48027 ) ;
#88510 = EDGE_CURVE ( 'NONE', #76282, #21205, #82740, .T. ) ;
#88511 = FACE_OUTER_BOUND ( 'NONE', #63237, .T. ) ;
#88512 = CARTESIAN_POINT ( 'NONE',  ( -18.48921356237309510, -27.52281430457068367, 5.000000000000000000 ) ) ;
#88513 = CARTESIAN_POINT ( 'NONE',  ( 110.3079301918980946, -6.109999999999998543, 1.637169565754158063 ) ) ;
#88514 = ORIENTED_EDGE ( 'NONE', *, *, #1356, .T. ) ;
#88515 = EDGE_LOOP ( 'NONE', ( #27733, #68210, #87863, #36006 ) ) ;
#88516 = VECTOR ( 'NONE', #119593, 1000.000000000000000 ) ;
#88517 = PLANE ( 'NONE',  #83205 ) ;
#88518 = EDGE_CURVE ( 'NONE', #115411, #77426, #95008, .T. ) ;
#88519 = LINE ( 'NONE', #21092, #77918 ) ;
#88520 = ORIENTED_EDGE ( 'NONE', *, *, #83163, .T. ) ;
#88521 = ORIENTED_EDGE ( 'NONE', *, *, #48946, .F. ) ;
#88522 = CARTESIAN_POINT ( 'NONE',  ( 39.37543019189809712, -5.291415217122920289, -3.055000000000001492 ) ) ;
#88523 = ORIENTED_EDGE ( 'NONE', *, *, #17531, .T. ) ;
#88524 = FACE_OUTER_BOUND ( 'NONE', #117714, .T. ) ;
#88525 = DIRECTION ( 'NONE',  ( 0.000000000000000000, 0.000000000000000000, -1.000000000000000000 ) ) ;
#88526 = CARTESIAN_POINT ( 'NONE',  ( -34.92500000000001137, 4.444556126563251830, 11.73767485154040635 ) ) ;
#88527 = AXIS2_PLACEMENT_3D ( 'NONE', #10853, #65300, #42114 ) ;
#88528 = CARTESIAN_POINT ( 'NONE',  ( 26.59959685856477307, -6.109999999999997655, -1.637169565754160283 ) ) ;
#88529 = ORIENTED_EDGE ( 'NONE', *, *, #79504, .F. ) ;
#88530 = ADVANCED_FACE ( 'NONE', ( #92884 ), #136388, .F. ) ;
#88531 = DIRECTION ( 'NONE',  ( -0.3543493200069163240, 0.000000000000000000, -0.9351131265310288487 ) ) ;
#88532 = ORIENTED_EDGE ( 'NONE', *, *, #45662, .T. ) ;
#88533 = ORIENTED_EDGE ( 'NONE', *, *, #134942, .F. ) ;
#88534 = CONICAL_SURFACE ( 'NONE', #111698, 2.500000000000000444, 0.9599310885968830309 ) ;
#88535 = AXIS2_PLACEMENT_3D ( 'NONE', #12624, #142453, #99626 ) ;
#88536 = VERTEX_POINT ( 'NONE', #82056 ) ;
#88537 = VECTOR ( 'NONE', #92056, 1000.000000000000000 ) ;
#88538 = SHAPE_REPRESENTATION ( '1.1 Sliding Jaw', ( #127880 ), #35272 ) ;
#88539 = EDGE_CURVE ( 'NONE', #82607, #25494, #33532, .T. ) ;
#88541 = EDGE_CURVE ( 'NONE', #132778, #136694, #71163, .T. ) ;
#88540 = AXIS2_PLACEMENT_3D ( 'NONE', #89465, #24224, #121374 ) ;
#88542 = VECTOR ( 'NONE', #28283, 1000.000000000000000 ) ;
#88543 = LINE ( 'NONE', #67513, #123883 ) ;
#88544 = DIRECTION ( 'NONE',  ( 0.7071067811865487940, 0.7071067811865463515, -0.000000000000000000 ) ) ;
#88545 = ORIENTED_EDGE ( 'NONE', *, *, #37313, .F. ) ;
#88546 = LINE ( 'NONE', #130630, #29741 ) ;
#88547 = CIRCLE ( 'NONE', #107042, 3.378199999999994319 ) ;
#88548 = AXIS2_PLACEMENT_3D ( 'NONE', #42307, #74939, #51025 ) ;
#88549 = DIRECTION ( 'NONE',  ( -0.7071067811865487940, 0.7071067811865463515, 0.000000000000000000 ) ) ;
#88550 = EDGE_CURVE ( 'NONE', #15815, #103353, #115308, .T. ) ;
#88551 = DIRECTION ( 'NONE',  ( 1.000000000000000000, 0.000000000000000000, 0.000000000000000000 ) ) ;
#88552 = FACE_BOUND ( 'NONE', #19874, .T. ) ;
#88553 = EDGE_CURVE ( 'NONE', #83048, #59118, #92158, .T. ) ;
#88554 = ORIENTED_EDGE ( 'NONE', *, *, #27193, .T. ) ;
#88555 = CARTESIAN_POINT ( 'NONE',  ( -75.29974487139158157, -27.71228299555258445, 4.000000000000000000 ) ) ;
#88556 = DIRECTION ( 'NONE',  ( -1.000000000000000000, -0.000000000000000000, -0.000000000000000000 ) ) ;
#88557 = CARTESIAN_POINT ( 'NONE',  ( 25.39999999999999858, -5.131256043349313067, -6.052638797879072108 ) ) ;
#88558 = ADVANCED_FACE ( 'NONE', ( #28361 ), #106585, .F. ) ;
#88559 = ORIENTED_EDGE ( 'NONE', *, *, #47054, .F. ) ;
#88560 = CARTESIAN_POINT ( 'NONE',  ( 27.18398860626900060, 28.73617430169806042, 5.000000000000000000 ) ) ;
#88561 = ORIENTED_EDGE ( 'NONE', *, *, #15494, .T. ) ;
#88562 = ORIENTED_EDGE ( 'NONE', *, *, #36378, .T. ) ;
#88563 = SURFACE_SIDE_STYLE ('',( #2767 ) ) ;
#88564 = ORIENTED_EDGE ( 'NONE', *, *, #25611, .T. ) ;
#88565 = CARTESIAN_POINT ( 'NONE',  ( 46.28709685856477307, 3.054999999999997495, 5.291415217122919401 ) ) ;
#88566 = VERTEX_POINT ( 'NONE', #61032 ) ;
#88567 = EDGE_CURVE ( 'NONE', #106121, #70409, #105185, .T. ) ;
#88568 = DIRECTION ( 'NONE',  ( -0.3543493200069162685, -0.000000000000000000, -0.9351131265310288487 ) ) ;
#88569 = CARTESIAN_POINT ( 'NONE',  ( -7.499999999999945821, 6.431123077392112641, 4.000000000000000000 ) ) ;
#88570 = ORIENTED_EDGE ( 'NONE', *, *, #45424, .T. ) ;
#88571 = DIRECTION ( 'NONE',  ( 0.000000000000000000, 1.000000000000000000, 0.000000000000000000 ) ) ;
#88572 = DIRECTION ( 'NONE',  ( -0.000000000000000000, 0.000000000000000000, 1.000000000000000000 ) ) ;
#88573 = EDGE_CURVE ( 'NONE', #31464, #115452, #60291, .T. ) ;
#88574 = VECTOR ( 'NONE', #94949, 1000.000000000000227 ) ;
#88575 = LINE ( 'NONE', #22544, #82636 ) ;
#88576 = LINE ( 'NONE', #110989, #122236 ) ;
#88577 = LINE ( 'NONE', #87839, #99075 ) ;
#88578 = AXIS2_PLACEMENT_3D ( 'NONE', #46184, #90358, #14227 ) ;
#88579 = CARTESIAN_POINT ( 'NONE',  ( 0.000000000000000000, 2.375000000000000000, 1.069999999999998508 ) ) ;
#88580 = DIRECTION ( 'NONE',  ( 1.000000000000000000, 0.000000000000000000, 0.000000000000000000 ) ) ;
#88581 = ORIENTED_EDGE ( 'NONE', *, *, #8630, .F. ) ;
#88582 = ORIENTED_EDGE ( 'NONE', *, *, #84777, .F. ) ;
#88583 = ORIENTED_EDGE ( 'NONE', *, *, #118643, .T. ) ;
#88584 = VECTOR ( 'NONE', #39097, 1000.000000000000227 ) ;
#88585 = LINE ( 'NONE', #77701, #84422 ) ;
#88586 = PLANE ( 'NONE',  #9756 ) ;
#88587 = VERTEX_POINT ( 'NONE', #5127 ) ;
#88588 = ORIENTED_EDGE ( 'NONE', *, *, #88842, .T. ) ;
#88589 = DIRECTION ( 'NONE',  ( -1.000000000000000000, 0.000000000000000000, -0.000000000000000000 ) ) ;
#88590 = CARTESIAN_POINT ( 'NONE',  ( 5.999999999999957367, -21.41253812416053748, 4.000000000000000000 ) ) ;
#88591 = FACE_OUTER_BOUND ( 'NONE', #53236, .T. ) ;
#88592 = ORIENTED_EDGE ( 'NONE', *, *, #105833, .F. ) ;
#88593 = EDGE_CURVE ( 'NONE', #108717, #17336, #37077, .T. ) ;
#88594 = CARTESIAN_POINT ( 'NONE',  ( 32.20666063542130075, 21.75929247661549937, 4.998822639870702744 ) ) ;
#88595 = EDGE_CURVE ( 'NONE', #110142, #43034, #117469, .T. ) ;
#88596 = DIRECTION ( 'NONE',  ( -0.7071067811865486830, -0.7071067811865464625, 0.000000000000000000 ) ) ;
#88597 = EDGE_CURVE ( 'NONE', #134224, #112523, #15292, .T. ) ;
#88598 = CARTESIAN_POINT ( 'NONE',  ( 30.40040314143521982, -7.934999999999989839, 2.126176841940957907 ) ) ;
#88599 = FACE_OUTER_BOUND ( 'NONE', #119241, .T. ) ;
#88600 = EDGE_LOOP ( 'NONE', ( #77378, #21130, #100960 ) ) ;
#88601 = CARTESIAN_POINT ( 'NONE',  ( 113.9537635252314516, -6.109999999999999432, -3.741295971395163529E-16 ) ) ;
#88602 = LINE ( 'NONE', #10289, #7158 ) ;
#88603 = VECTOR ( 'NONE', #86738, 1000.000000000000000 ) ;
#88604 = DIRECTION ( 'NONE',  ( 0.000000000000000000, 0.000000000000000000, 1.000000000000000000 ) ) ;
#88606 = ORIENTED_EDGE ( 'NONE', *, *, #108588, .T. ) ;
#88605 = FACE_OUTER_BOUND ( 'NONE', #43423, .T. ) ;
#88608 = VECTOR ( 'NONE', #113581, 1000.000000000000227 ) ;
#88607 = DIRECTION ( 'NONE',  ( 1.000000000000000000, 0.000000000000000000, 0.000000000000000000 ) ) ;
#88609 = EDGE_LOOP ( 'NONE', ( #16770, #7733, #84749, #99984 ) ) ;
#88611 = EDGE_CURVE ( 'NONE', #81462, #18696, #18144, .T. ) ;
#88610 = DIRECTION ( 'NONE',  ( -0.000000000000000000, 1.000000000000000000, 2.921639538487157626E-15 ) ) ;
#88612 = DIRECTION ( 'NONE',  ( 0.000000000000000000, 0.000000000000000000, -1.000000000000000000 ) ) ;
#88613 = ORIENTED_EDGE ( 'NONE', *, *, #105418, .T. ) ;
#88614 = DIRECTION ( 'NONE',  ( 0.7071067811865487940, 0.7071067811865463515, -0.000000000000000000 ) ) ;
#88615 = DIRECTION ( 'NONE',  ( -0.000000000000000000, 0.3543493200069153248, 0.9351131265310292928 ) ) ;
#88616 = ORIENTED_EDGE ( 'NONE', *, *, #33062, .F. ) ;
#88617 = AXIS2_PLACEMENT_3D ( 'NONE', #53565, #100644, #76022 ) ;
#88618 = CARTESIAN_POINT ( 'NONE',  ( 8.999999999999932498, -13.39766691384882513, -10.96608748226467966 ) ) ;
#88619 = LINE ( 'NONE', #133540, #90917 ) ;
#88620 = ORIENTED_EDGE ( 'NONE', *, *, #87877, .T. ) ;
#88621 = CARTESIAN_POINT ( 'NONE',  ( -29.90332935812576309, -2.240707523384260824, 15.26439735382745511 ) ) ;
#88623 = ORIENTED_EDGE ( 'NONE', *, *, #32221, .T. ) ;
#88622 = FACE_OUTER_BOUND ( 'NONE', #97319, .T. ) ;
#88624 = ORIENTED_EDGE ( 'NONE', *, *, #93864, .F. ) ;
#88625 = VECTOR ( 'NONE', #99325, 999.9999999999998863 ) ;
#88626 = CARTESIAN_POINT ( 'NONE',  ( 14.86712903272168340, 7.883176524338217028, -28.07512293021272143 ) ) ;
#88627 = SURFACE_SIDE_STYLE ('',( #67603 ) ) ;
#88628 = ORIENTED_EDGE ( 'NONE', *, *, #40477, .F. ) ;
#88629 = CARTESIAN_POINT ( 'NONE',  ( 29.99999999999979039, -15.41253812416060143, 4.000000000000000000 ) ) ;
#88630 = LINE ( 'NONE', #89326, #49217 ) ;
#88631 = VERTEX_POINT ( 'NONE', #6541 ) ;
#88632 = ADVANCED_FACE ( 'NONE', ( #125537 ), #26218, .F. ) ;
#88633 = FACE_OUTER_BOUND ( 'NONE', #120262, .T. ) ;
#88634 = CARTESIAN_POINT ( 'NONE',  ( 48.18398860626899705, 28.73617430169820608, 5.000000000000000000 ) ) ;
#88635 = VECTOR ( 'NONE', #44416, 1000.000000000000000 ) ;
#88636 = VECTOR ( 'NONE', #49136, 1000.000000000000227 ) ;
#88637 = DIRECTION ( 'NONE',  ( 0.000000000000000000, 0.000000000000000000, -1.000000000000000000 ) ) ;
#88638 = CARTESIAN_POINT ( 'NONE',  ( 27.76626352523143737, 4.472830434245839371, -4.472830434245839371 ) ) ;
#88639 = DIRECTION ( 'NONE',  ( -1.000000000000000000, -1.224606353822377258E-16, -0.000000000000000000 ) ) ;
#88640 = AXIS2_PLACEMENT_3D ( 'NONE', #120456, #123391, #87161 ) ;
#88641 = VECTOR ( 'NONE', #49709, 999.9999999999998863 ) ;
#88642 = EDGE_LOOP ( 'NONE', ( #65964, #138158, #31534, #79 ) ) ;
#88643 = ORIENTED_EDGE ( 'NONE', *, *, #29222, .T. ) ;
#88644 = FACE_OUTER_BOUND ( 'NONE', #39520, .T. ) ;
#88645 = EDGE_LOOP ( 'NONE', ( #103062, #19529, #105781, #16382 ) ) ;
#88646 = ORIENTED_EDGE ( 'NONE', *, *, #84922, .T. ) ;
#88647 = CIRCLE ( 'NONE', #646, 2.500000000000000444 ) ;
#88648 = VECTOR ( 'NONE', #38908, 1000.000000000000000 ) ;
#88649 = DIRECTION ( 'NONE',  ( -0.7071067811865486830, -0.7071067811865464625, 0.000000000000000000 ) ) ;
#88650 = LINE ( 'NONE', #69040, #46277 ) ;
#88651 = ORIENTED_EDGE ( 'NONE', *, *, #2546, .F. ) ;
#88652 = CARTESIAN_POINT ( 'NONE',  ( 1.499999999999990896, -20.56887692260760048, 4.000000000000000000 ) ) ;
#88653 = DIRECTION ( 'NONE',  ( 0.000000000000000000, 0.000000000000000000, 1.000000000000000000 ) ) ;
#88654 = EDGE_CURVE ( 'NONE', #85221, #51427, #43508, .T. ) ;
#88655 = CARTESIAN_POINT ( 'NONE',  ( 7.499999999999956479, 0.05218569542916884352, 5.000000000000000000 ) ) ;
#88656 = CARTESIAN_POINT ( 'NONE',  ( 35.99451991528749772, 28.92564299267963079, 4.000000000000000000 ) ) ;
#88657 = CARTESIAN_POINT ( 'NONE',  ( 126.5837635252314612, -6.110000000000001208, -3.741295971395164515E-16 ) ) ;
#88658 = EDGE_CURVE ( 'NONE', #100160, #6566, #18890, .T. ) ;
#88659 = VERTEX_POINT ( 'NONE', #140661 ) ;
#88660 = DIRECTION ( 'NONE',  ( 1.000000000000000000, 0.000000000000000000, 0.000000000000000000 ) ) ;
#88661 = DIRECTION ( 'NONE',  ( -0.3543493200069162685, -0.000000000000000000, -0.9351131265310288487 ) ) ;
#88662 = LINE ( 'NONE', #56050, #112047 ) ;
#88663 = CARTESIAN_POINT ( 'NONE',  ( -36.18398860626899705, 28.73617430169812437, 5.000000000000000000 ) ) ;
#88664 = DIRECTION ( 'NONE',  ( 0.7071067811865487940, -0.7071067811865463515, 0.000000000000000000 ) ) ;
#88665 = CARTESIAN_POINT ( 'NONE',  ( 29.99999999999979750, 20.96639925780204905, 5.000000000000000000 ) ) ;
#88666 = EDGE_CURVE ( 'NONE', #64166, #131176, #21760, .T. ) ;
#88668 = EDGE_CURVE ( 'NONE', #18279, #38139, #76145, .T. ) ;
#88667 = CARTESIAN_POINT ( 'NONE',  ( 50.82919371712955581, -3.975000000000001865, 6.884901960086284411 ) ) ;
#88669 = DIRECTION ( 'NONE',  ( -0.6830127018922181881, 0.6830127018922202975, -0.2588190451025214056 ) ) ;
#88671 = LINE ( 'NONE', #13918, #115531 ) ;
#88670 = AXIS2_PLACEMENT_3D ( 'NONE', #105361, #138732, #15470 ) ;
#88672 = ORIENTED_EDGE ( 'NONE', *, *, #128443, .T. ) ;
#88673 = ORIENTED_EDGE ( 'NONE', *, *, #48969, .F. ) ;
#88674 = CARTESIAN_POINT ( 'NONE',  ( 41.10416666666666430, 2.130196079827422206, 7.950000000000001954 ) ) ;
#88675 = EDGE_CURVE ( 'NONE', #50352, #39505, #109479, .T. ) ;
#88676 = CARTESIAN_POINT ( 'NONE',  ( -5.510786437626906675, -27.52281430457051314, 5.000000000000000000 ) ) ;
#88677 = DIRECTION ( 'NONE',  ( 0.7071067811865487940, 0.7071067811865463515, 0.000000000000000000 ) ) ;
#88678 = EDGE_LOOP ( 'NONE', ( #115580, #139826, #36897, #48989 ) ) ;
#88679 = DIRECTION ( 'NONE',  ( 0.6830127018922180770, -0.6830127018922204085, -0.2588190451025213501 ) ) ;
#88680 = CARTESIAN_POINT ( 'NONE',  ( -56.99451991528749062, 28.92564299267978001, 4.000000000000000000 ) ) ;
#88681 = EDGE_CURVE ( 'NONE', #44075, #76243, #98591, .T. ) ;
#88682 = CARTESIAN_POINT ( 'NONE',  ( 40.10459685856476142, 1.637169565754164946, -6.109999999999999432 ) ) ;
#88683 = VECTOR ( 'NONE', #61875, 1000.000000000000000 ) ;
#88684 = ORIENTED_EDGE ( 'NONE', *, *, #54675, .F. ) ;
#88685 = CARTESIAN_POINT ( 'NONE',  ( 0.1600000000000007527, 2.771266204237592845, -7.457137036566489741 ) ) ;
#88686 = ORIENTED_EDGE ( 'NONE', *, *, #81991, .F. ) ;
#88687 = VERTEX_POINT ( 'NONE', #84868 ) ;
#88688 = PLANE ( 'NONE',  #79710 ) ;
#88689 = EDGE_CURVE ( 'NONE', #28531, #60511, #142822, .T. ) ;
#88690 = CARTESIAN_POINT ( 'NONE',  ( 26.12840764549667583, -2.499999999999996003, 0.000000000000000000 ) ) ;
#88691 = SURFACE_SIDE_STYLE ('',( #44489 ) ) ;
#88692 = CARTESIAN_POINT ( 'NONE',  ( -3.299744871391591339, -27.71228299555208352, 4.000000000000000000 ) ) ;
#88693 = EDGE_LOOP ( 'NONE', ( #92818, #101371, #95339, #75347 ) ) ;
#88694 = CARTESIAN_POINT ( 'NONE',  ( 65.99451991528749772, 28.92564299267984396, 4.000000000000000000 ) ) ;
#88695 = ORIENTED_EDGE ( 'NONE', *, *, #138597, .T. ) ;
#88696 = CARTESIAN_POINT ( 'NONE',  ( 78.02126352523144703, -4.472830434245838482, -4.472830434245840259 ) ) ;
#88697 = LINE ( 'NONE', #25551, #43884 ) ;
#88698 = SURFACE_STYLE_USAGE ( .BOTH. , #32157 ) ;
#88699 = SURFACE_STYLE_USAGE ( .BOTH. , #126133 ) ;
#88700 = EDGE_CURVE ( 'NONE', #18390, #61904, #131230, .T. ) ;
#88701 = CARTESIAN_POINT ( 'NONE',  ( -31.92499999999997584, -21.76999999999999247, -40.00000000000000000 ) ) ;
#88702 = CARTESIAN_POINT ( 'NONE',  ( -24.48921356237309510, -27.52281430457072631, 5.000000000000000000 ) ) ;
#88703 = AXIS2_PLACEMENT_3D ( 'NONE', #134828, #34782, #66002 ) ;
#88704 = VERTEX_POINT ( 'NONE', #85566 ) ;
#88705 =( BOUNDED_CURVE ( )  B_SPLINE_CURVE ( 3, ( #68730, #67292, #12874, #79644 ),
 .UNSPECIFIED., .F., .T. ) 
 B_SPLINE_CURVE_WITH_KNOTS ( ( 4, 4 ),
 ( 5.920967161967926273, 7.341195215986655143 ),
 .UNSPECIFIED. ) 
 CURVE ( )  GEOMETRIC_REPRESENTATION_ITEM ( )  RATIONAL_B_SPLINE_CURVE ( ( 1.000000000000000000, 0.8388583629366573868, 0.8388583629366573868, 1.000000000000000000 ) ) 
 REPRESENTATION_ITEM ( '' )  );
#88706 = CARTESIAN_POINT ( 'NONE',  ( 87.57919371712957002, 3.975000000000002753, -6.884901960086283523 ) ) ;
#88707 = CARTESIAN_POINT ( 'NONE',  ( 57.95376352523144448, -6.109999999999998543, -3.741295971395162543E-16 ) ) ;
#88708 = DIRECTION ( 'NONE',  ( 0.000000000000000000, -1.000000000000000000, 0.000000000000000000 ) ) ;
#88709 = VECTOR ( 'NONE', #58978, 999.9999999999998863 ) ;
#88710 = EDGE_CURVE ( 'NONE', #8502, #27215, #31920, .T. ) ;
#88711 = DIRECTION ( 'NONE',  ( -0.6830127018922180770, -0.6830127018922204085, -0.2588190451025213501 ) ) ;
#88712 = CARTESIAN_POINT ( 'NONE',  ( 34.49999999999976552, 7.464255608400424791, 4.994342998332163219 ) ) ;
#88713 = VERTEX_POINT ( 'NONE', #97127 ) ;
#88714 = EDGE_LOOP ( 'NONE', ( #127760, #96909, #76046, #100186 ) ) ;
#88715 = VECTOR ( 'NONE', #45716, 1000.000000000000000 ) ;
#88716 = DIRECTION ( 'NONE',  ( 0.6830127018922181881, 0.6830127018922202975, -0.2588190451025214056 ) ) ;
#88717 = ORIENTED_EDGE ( 'NONE', *, *, #91138, .F. ) ;
#88718 = EDGE_CURVE ( 'NONE', #52993, #98020, #47520, .T. ) ;
#88719 = DIRECTION ( 'NONE',  ( 1.000000000000000000, 0.000000000000000000, 0.000000000000000000 ) ) ;
#88721 = EDGE_CURVE ( 'NONE', #61026, #79521, #36077, .T. ) ;
#88720 = VERTEX_POINT ( 'NONE', #142131 ) ;
#88722 = CARTESIAN_POINT ( 'NONE',  ( -24.18398860626899705, 28.73617430169804265, 5.000000000000000000 ) ) ;
#88723 = LINE ( 'NONE', #56833, #43344 ) ;
#88724 = STYLED_ITEM ( 'NONE', ( #59204 ), #80703 ) ;
#88725 = EDGE_CURVE ( 'NONE', #6025, #16532, #76886, .T. ) ;
#88726 = DIRECTION ( 'NONE',  ( -0.6830127018922180770, -0.6830127018922204085, -0.2588190451025213501 ) ) ;
#88727 = FACE_BOUND ( 'NONE', #82988, .T. ) ;
#88728 = CARTESIAN_POINT ( 'NONE',  ( 181.1500000000000057, -3.180000000000061444, 34.92499999999998295 ) ) ;
#88729 = DIRECTION ( 'NONE',  ( -0.7071067811865486830, -0.7071067811865464625, 0.000000000000000000 ) ) ;
#88730 = CARTESIAN_POINT ( 'NONE',  ( 48.29974487139158867, -27.71228299555239971, 4.000000000000000000 ) ) ;
#88731 = AXIS2_PLACEMENT_3D ( 'NONE', #49983, #107189, #138406 ) ;
#88732 = CARTESIAN_POINT ( 'NONE',  ( 28.40832548098983423, -0.7407075233842701500, 14.76736230305387210 ) ) ;
#88734 = ORIENTED_EDGE ( 'NONE', *, *, #126878, .F. ) ;
#88733 = CARTESIAN_POINT ( 'NONE',  ( 51.70419371712956291, -6.884901960086285300, -3.975000000000000089 ) ) ;
#88735 = DIRECTION ( 'NONE',  ( -1.000000000000000000, -1.224606353822377258E-16, -0.000000000000000000 ) ) ;
#88736 = EDGE_LOOP ( 'NONE', ( #52068, #24550, #42940, #19421 ) ) ;
#88737 = ORIENTED_EDGE ( 'NONE', *, *, #29236, .T. ) ;
#88738 = CARTESIAN_POINT ( 'NONE',  ( 79.53709685856478018, -3.054999999999998828, -5.291415217122919401 ) ) ;
#88739 = VERTEX_POINT ( 'NONE', #21025 ) ;
#88740 = DIRECTION ( 'NONE',  ( -0.000000000000000000, -0.3543493200069152693, 0.9351131265310292928 ) ) ;
#88741 = EDGE_CURVE ( 'NONE', #108642, #1460, #84351, .T. ) ;
#88742 = DIRECTION ( 'NONE',  ( 0.7071067811865487940, 0.7071067811865463515, 0.000000000000000000 ) ) ;
#88743 = ORIENTED_EDGE ( 'NONE', *, *, #127966, .F. ) ;
#88744 = CARTESIAN_POINT ( 'NONE',  ( 20.66840764549667497, 9.139736423841732040E-16, 0.000000000000000000 ) ) ;
#88745 = VECTOR ( 'NONE', #138535, 999.9999999999998863 ) ;
#88746 = EDGE_CURVE ( 'NONE', #136709, #33315, #95741, .T. ) ;
#88747 = AXIS2_PLACEMENT_3D ( 'NONE', #35639, #79870, #10956 ) ;
#88748 = CARTESIAN_POINT ( 'NONE',  ( 3.469446951953614189E-15, -3.485240976185081330, -4.108735105802396426 ) ) ;
#88749 = DIRECTION ( 'NONE',  ( -0.7071067811865486830, -0.7071067811865464625, 0.000000000000000000 ) ) ;
#88750 = DIRECTION ( 'NONE',  ( 0.7071067811865486830, -0.7071067811865464625, -0.000000000000000000 ) ) ;
#88751 = CARTESIAN_POINT ( 'NONE',  ( -33.32816939922329880, -12.74070752338415602, 4.000000000000000000 ) ) ;
#88752 = LINE ( 'NONE', #20598, #117986 ) ;
#88753 = ORIENTED_EDGE ( 'NONE', *, *, #85097, .F. ) ;
#88754 = VECTOR ( 'NONE', #928, 1000.000000000000227 ) ;
#88755 = MECHANICAL_DESIGN_GEOMETRIC_PRESENTATION_REPRESENTATION (  '', ( #35479 ), #44707 ) ;
#88756 = CARTESIAN_POINT ( 'NONE',  ( 10.49999999999992362, 18.43112307739199451, 4.000000000000000000 ) ) ;
#88757 = ORIENTED_EDGE ( 'NONE', *, *, #121376, .F. ) ;
#88758 = PLANE ( 'NONE',  #40344 ) ;
#88759 = VECTOR ( 'NONE', #91427, 1000.000000000000000 ) ;
#88760 = CARTESIAN_POINT ( 'NONE',  ( 7.110173228882053387, -22.22500000000000497, 4.785647885939352086 ) ) ;
#88761 = VERTEX_POINT ( 'NONE', #139991 ) ;
#88762 = ORIENTED_EDGE ( 'NONE', *, *, #13865, .F. ) ;
#88763 = FACE_OUTER_BOUND ( 'NONE', #24376, .T. ) ;
#88764 = CARTESIAN_POINT ( 'NONE',  ( 23.99451991528749062, 28.92564299267954908, 4.000000000000000000 ) ) ;
#88765 = ORIENTED_EDGE ( 'NONE', *, *, #117526, .F. ) ;
#88766 = DIRECTION ( 'NONE',  ( -0.7071067811865486830, -0.7071067811865464625, 0.000000000000000000 ) ) ;
#88767 = ADVANCED_FACE ( 'NONE', ( #29757 ), #74002, .T. ) ;
#88768 = CARTESIAN_POINT ( 'NONE',  ( -24.18398860626899705, 28.73617430169804265, 5.000000000000000000 ) ) ;
#88769 = VECTOR ( 'NONE', #84200, 1000.000000000000000 ) ;
#88770 = CARTESIAN_POINT ( 'NONE',  ( 30.08747294953710494, -6.094999999999989981, 3.732111120401553285E-16 ) ) ;
#88771 = CARTESIAN_POINT ( 'NONE',  ( 16.10925740115140314, 1.961328573423360089, -30.40648711071796839 ) ) ;
#88772 = EDGE_LOOP ( 'NONE', ( #109660, #94961, #112334, #64476 ) ) ;
#88773 = VERTEX_POINT ( 'NONE', #63852 ) ;
#88774 = FACE_OUTER_BOUND ( 'NONE', #74312, .T. ) ;
#88775 = CARTESIAN_POINT ( 'NONE',  ( -18.18398860626898994, 28.73617430169800002, 5.000000000000000000 ) ) ;
#88777 = ORIENTED_EDGE ( 'NONE', *, *, #5824, .F. ) ;
#88776 = DIRECTION ( 'NONE',  ( -0.7071067811865487940, 0.7071067811865463515, -0.000000000000000000 ) ) ;
#88778 = VERTEX_POINT ( 'NONE', #7996 ) ;
#88779 = CARTESIAN_POINT ( 'NONE',  ( 2.999999999999999112, -1.600000000000094458, 31.92499999999998295 ) ) ;
#88780 = CARTESIAN_POINT ( 'NONE',  ( 32.99999999999977973, -19.44781430457062754, 5.000000000000000000 ) ) ;
#88781 = VECTOR ( 'NONE', #35995, 1000.000000000000000 ) ;
#88782 = DIRECTION ( 'NONE',  ( 0.000000000000000000, 1.000000000000000000, 0.000000000000000000 ) ) ;
#88783 = VERTEX_POINT ( 'NONE', #52237 ) ;
#88784 = FILL_AREA_STYLE_COLOUR ( '', #85218 ) ;
#88785 = DIRECTION ( 'NONE',  ( 0.7071067811865487940, -0.7071067811865463515, 0.000000000000000000 ) ) ;
#88786 = ORIENTED_EDGE ( 'NONE', *, *, #134937, .T. ) ;
#88787 = VECTOR ( 'NONE', #74332, 1000.000000000000227 ) ;
#88788 = CARTESIAN_POINT ( 'NONE',  ( -71.99451991528749772, 28.92564299267988304, 4.000000000000000000 ) ) ;
#88789 = CARTESIAN_POINT ( 'NONE',  ( 8.111623618947536585, 9.759292476615614831, 17.35367589129210941 ) ) ;
#88790 = CARTESIAN_POINT ( 'NONE',  ( -10.82816939922344801, 18.75929247661552779, 4.000000000000000000 ) ) ;
#88791 =( NAMED_UNIT ( * ) SI_UNIT ( $, .STERADIAN. ) SOLID_ANGLE_UNIT ( ) );
#88793 = VECTOR ( 'NONE', #1871, 999.9999999999998863 ) ;
#88792 = FACE_OUTER_BOUND ( 'NONE', #38100, .T. ) ;
#88794 = CARTESIAN_POINT ( 'NONE',  ( -14.99451991528749595, 28.92564299267948513, 4.000000000000000000 ) ) ;
#88795 = CARTESIAN_POINT ( 'NONE',  ( -12.48921356237309155, -27.52281430457064104, 5.000000000000000000 ) ) ;
#88796 = ORIENTED_EDGE ( 'NONE', *, *, #142292, .F. ) ;
#88797 = PLANE ( 'NONE',  #69814 ) ;
#88798 = EDGE_LOOP ( 'NONE', ( #105581, #7489, #12261, #91959, #39556 ) ) ;
#88799 = SURFACE_STYLE_USAGE ( .BOTH. , #307 ) ;
#88800 = CARTESIAN_POINT ( 'NONE',  ( 9.706123077391888287, 22.22500000000000142, 4.000000000000000000 ) ) ;
#88801 = VECTOR ( 'NONE', #124378, 1000.000000000000227 ) ;
#88802 = FACE_OUTER_BOUND ( 'NONE', #138252, .T. ) ;
#88803 = FACE_OUTER_BOUND ( 'NONE', #41096, .T. ) ;
#88805 = ORIENTED_EDGE ( 'NONE', *, *, #140990, .F. ) ;
#88804 = VECTOR ( 'NONE', #108342, 1000.000000000000000 ) ;
#88806 = CARTESIAN_POINT ( 'NONE',  ( 15.32816939922342847, 17.25929247661554200, 4.000000000000000000 ) ) ;
#88807 = DIRECTION ( 'NONE',  ( 0.7071067811865487940, 0.7071067811865463515, -0.000000000000000000 ) ) ;
#88808 = DIRECTION ( 'NONE',  ( -0.7071067811865486830, -0.7071067811865464625, 0.000000000000000000 ) ) ;
#88809 = ORIENTED_EDGE ( 'NONE', *, *, #98796, .F. ) ;
#88810 = DIRECTION ( 'NONE',  ( 1.000000000000000000, 0.000000000000000000, 0.000000000000000000 ) ) ;
#88811 = DIRECTION ( 'NONE',  ( 0.1737853339090460192, -0.1737853339090456029, 0.9693282805305141192 ) ) ;
#88812 = VECTOR ( 'NONE', #65876, 1000.000000000000000 ) ;
#88813 = LINE ( 'NONE', #98934, #42836 ) ;
#88814 = DIRECTION ( 'NONE',  ( 0.7071067811865486830, -0.7071067811865464625, -0.000000000000000000 ) ) ;
#88815 = CARTESIAN_POINT ( 'NONE',  ( 55.76626352523145869, 4.472830434245839371, -4.472830434245839371 ) ) ;
#88816 = DIRECTION ( 'NONE',  ( -0.7071067811865486830, -0.7071067811865464625, 0.000000000000000000 ) ) ;
#88817 = CARTESIAN_POINT ( 'NONE',  ( -51.29974487139158867, -27.71228299555242103, 4.000000000000000000 ) ) ;
#88818 = CARTESIAN_POINT ( 'NONE',  ( 32.16252705046289151, 7.949999999999998401, 1.460391307983218338E-15 ) ) ;
#88819 = LINE ( 'NONE', #86673, #48800 ) ;
#88820 = ORIENTED_EDGE ( 'NONE', *, *, #29047, .F. ) ;
#88821 = CARTESIAN_POINT ( 'NONE',  ( -4.499999999999962697, -6.839392718269134974, -8.480912228396073615 ) ) ;
#88822 = ADVANCED_FACE ( 'NONE', ( #20303 ), #96420, .T. ) ;
#88823 = EDGE_LOOP ( 'NONE', ( #9578, #115376, #138224, #39895 ) ) ;
#88824 = VECTOR ( 'NONE', #60634, 1000.000000000000227 ) ;
#88825 = DIRECTION ( 'NONE',  ( 0.7071067811865487940, 0.7071067811865463515, -0.000000000000000000 ) ) ;
#88826 = DIRECTION ( 'NONE',  ( 0.7071067811865487940, 0.7071067811865463515, -0.000000000000000000 ) ) ;
#88827 = CARTESIAN_POINT ( 'NONE',  ( -26.20710678118635428, -20.24070752338407786, 5.000000000000000000 ) ) ;
#88828 = LINE ( 'NONE', #43888, #65066 ) ;
#88829 = DIRECTION ( 'NONE',  ( 1.000000000000000000, 0.000000000000000000, 0.000000000000000000 ) ) ;
#88830 = LINE ( 'NONE', #1054, #138020 ) ;
#88831 = EDGE_CURVE ( 'NONE', #78237, #14912, #26661, .T. ) ;
#88832 = ADVANCED_FACE ( 'NONE', ( #99286 ), #134098, .F. ) ;
#88833 = ORIENTED_EDGE ( 'NONE', *, *, #121392, .T. ) ;
#88835 = ORIENTED_EDGE ( 'NONE', *, *, #63153, .F. ) ;
#88834 = AXIS2_PLACEMENT_3D ( 'NONE', #15525, #114848, #27867 ) ;
#88836 = FACE_OUTER_BOUND ( 'NONE', #17243, .T. ) ;
#88837 = PLANE ( 'NONE',  #60637 ) ;
#88838 = DIRECTION ( 'NONE',  ( 0.7071067811865487940, -0.7071067811865463515, 0.000000000000000000 ) ) ;
#88839 = CARTESIAN_POINT ( 'NONE',  ( 0.000000000000000000, -21.72500000000000142, 4.500000000000000888 ) ) ;
#88840 = EDGE_CURVE ( 'NONE', #39920, #70502, #2844, .T. ) ;
#88842 = EDGE_CURVE ( 'NONE', #32743, #111517, #90593, .T. ) ;
#88841 = CARTESIAN_POINT ( 'NONE',  ( 86.12086038379622721, -6.884901960086286188, 3.974999999999997424 ) ) ;
#88843 = LINE ( 'NONE', #135212, #85638 ) ;
#88844 = AXIS2_PLACEMENT_3D ( 'NONE', #101933, #35987, #122979 ) ;
#88845 = CARTESIAN_POINT ( 'NONE',  ( -10.49999999999992895, -19.91253812416055169, 4.000000000000000000 ) ) ;
#88847 = ADVANCED_FACE ( 'NONE', ( #121759 ), #33388, .F. ) ;
#88846 = VERTEX_POINT ( 'NONE', #23908 ) ;
#88848 = CARTESIAN_POINT ( 'NONE',  ( 73.91666666666665719, -6.884901960086287076, -3.975000000000000977 ) ) ;
#88849 = FACE_OUTER_BOUND ( 'NONE', #89260, .T. ) ;
#88850 = EDGE_CURVE ( 'NONE', #39702, #94617, #77590, .T. ) ;
#88851 = CARTESIAN_POINT ( 'NONE',  ( -34.42500000000001137, -1.458600742197974087, 5.000000000000000000 ) ) ;
#88852 = CARTESIAN_POINT ( 'NONE',  ( -22.49999999999985434, 13.56627193232213102, -10.57019076586073680 ) ) ;
#88853 = EDGE_CURVE ( 'NONE', #105060, #28681, #44990, .T. ) ;
#88854 = VERTEX_POINT ( 'NONE', #12294 ) ;
#88855 = AXIS2_PLACEMENT_3D ( 'NONE', #36134, #12912, #57188 ) ;
#88856 = DIRECTION ( 'NONE',  ( -0.7071067811865486830, -0.7071067811865464625, 0.000000000000000000 ) ) ;
#88858 = ORIENTED_EDGE ( 'NONE', *, *, #22647, .T. ) ;
#88857 = EDGE_CURVE ( 'NONE', #54435, #8757, #68170, .T. ) ;
#88859 = FACE_OUTER_BOUND ( 'NONE', #27564, .T. ) ;
#88860 = CARTESIAN_POINT ( 'NONE',  ( 69.12543019189809002, 5.291415217122919401, 3.055000000000002824 ) ) ;
#88861 = DIRECTION ( 'NONE',  ( -0.3543493200069162685, -0.000000000000000000, -0.9351131265310288487 ) ) ;
#88862 = VERTEX_POINT ( 'NONE', #124633 ) ;
#88863 = DIRECTION ( 'NONE',  ( 0.7071067811865486830, -0.7071067811865464625, -0.000000000000000000 ) ) ;
#88864 = DIRECTION ( 'NONE',  ( 0.7071067811865487940, 0.7071067811865463515, -0.000000000000000000 ) ) ;
#88865 = ADVANCED_FACE ( 'NONE', ( #23149 ), #110169, .F. ) ;
#88866 = CARTESIAN_POINT ( 'NONE',  ( 20.86500426248364803, 3.759292476615681888, 15.36553568819721072 ) ) ;
#88867 = LINE ( 'NONE', #131647, #131949 ) ;
#88869 = ORIENTED_EDGE ( 'NONE', *, *, #140053, .T. ) ;
#88868 = CARTESIAN_POINT ( 'NONE',  ( 6.792893218813416567, 0.7592924766157104211, 5.000000000000000000 ) ) ;
#88870 = CARTESIAN_POINT ( 'NONE',  ( 31.49999999999977973, 9.431123077392099319, 4.000000000000000000 ) ) ;
#88871 = CARTESIAN_POINT ( 'NONE',  ( 23.99999999999983302, -16.06887692260764666, 4.000000000000000000 ) ) ;
#88872 = CYLINDRICAL_SURFACE ( 'NONE', #30886, 0.5000000000000004441 ) ;
#88874 = EDGE_CURVE ( 'NONE', #31789, #2906, #11555, .T. ) ;
#88873 = AXIS2_PLACEMENT_3D ( 'NONE', #26669, #104936, #115773 ) ;
#88875 = LINE ( 'NONE', #31621, #2083 ) ;
#88876 = ORIENTED_EDGE ( 'NONE', *, *, #5420, .F. ) ;
#88877 = EDGE_LOOP ( 'NONE', ( #124546, #61693, #40083, #46936 ) ) ;
#88878 = CARTESIAN_POINT ( 'NONE',  ( 65.04209685856477563, 5.291415217122923842, -3.054999999999996163 ) ) ;
#88879 = AXIS2_PLACEMENT_3D ( 'NONE', #81157, #70315, #135538 ) ;
#88880 = VERTEX_POINT ( 'NONE', #143530 ) ;
#88881 = LINE ( 'NONE', #133108, #79994 ) ;
#88882 = LINE ( 'NONE', #22148, #7034 ) ;
#88883 = DIRECTION ( 'NONE',  ( 0.7071067811865487940, 0.7071067811865463515, -0.000000000000000000 ) ) ;
#88884 = LINE ( 'NONE', #57691, #91975 ) ;
#88885 = DIRECTION ( 'NONE',  ( 0.7071067811865486830, -0.7071067811865464625, -0.000000000000000000 ) ) ;
#88886 = VERTEX_POINT ( 'NONE', #1395 ) ;
#88887 = ORIENTED_EDGE ( 'NONE', *, *, #14908, .T. ) ;
#88888 = CARTESIAN_POINT ( 'NONE',  ( 39.18398860626899705, 28.73617430169814568, 5.000000000000000000 ) ) ;
#88889 = CARTESIAN_POINT ( 'NONE',  ( -17.01299345042646749, -0.9444868035190714384, -36.39086428169088094 ) ) ;
#88890 = VECTOR ( 'NONE', #117603, 1000.000000000000227 ) ;
#88891 = EDGE_CURVE ( 'NONE', #751, #97422, #68857, .T. ) ;
#88892 = ORIENTED_EDGE ( 'NONE', *, *, #51443, .T. ) ;
#88893 = AXIS2_PLACEMENT_3D ( 'NONE', #119065, #54558, #10298 ) ;
#88894 = CARTESIAN_POINT ( 'NONE',  ( 1.179999999999999272, 6.391994993740214959, 10.00000000000000000 ) ) ;
#88895 = ADVANCED_FACE ( 'NONE', ( #133390 ), #34078, .F. ) ;
#88896 = PLANE ( 'NONE',  #22500 ) ;
#88897 = LINE ( 'NONE', #133120, #134990 ) ;
#88898 = EDGE_CURVE ( 'NONE', #66948, #20082, #86905, .T. ) ;
#88899 = ORIENTED_EDGE ( 'NONE', *, *, #42760, .T. ) ;
#88900 = VECTOR ( 'NONE', #98057, 1000.000000000000000 ) ;
#88901 = VECTOR ( 'NONE', #85533, 1000.000000000000000 ) ;
#88902 = FACE_BOUND ( 'NONE', #121302, .T. ) ;
#88903 = CARTESIAN_POINT ( 'NONE',  ( 7.408407645496676963, -1.925929944387235853E-31, 2.500000000000001332 ) ) ;
#88904 = FACE_OUTER_BOUND ( 'NONE', #103313, .T. ) ;
#88905 = CARTESIAN_POINT ( 'NONE',  ( 60.50000000000000000, 0.000000000000000000, -7.950000000000000178 ) ) ;
#88907 = VECTOR ( 'NONE', #46943, 1000.000000000000000 ) ;
#88906 = LINE ( 'NONE', #78018, #36501 ) ;
#88908 = VECTOR ( 'NONE', #80381, 1000.000000000000000 ) ;
#88909 = CARTESIAN_POINT ( 'NONE',  ( -32.99451991528749062, 28.92564299267960948, 4.000000000000000000 ) ) ;
#88910 = ORIENTED_EDGE ( 'NONE', *, *, #135209, .T. ) ;
#88911 = VECTOR ( 'NONE', #85506, 999.9999999999998863 ) ;
#88912 = VERTEX_POINT ( 'NONE', #123941 ) ;
#88913 = CARTESIAN_POINT ( 'NONE',  ( 98.78709685856479439, 3.054999999999997495, 5.291415217122919401 ) ) ;
#88914 = EDGE_LOOP ( 'NONE', ( #133200, #61544, #69631, #3673 ) ) ;
#88915 = EDGE_CURVE ( 'NONE', #41910, #14576, #12997, .T. ) ;
#88916 = CARTESIAN_POINT ( 'NONE',  ( -27.48921356237309155, -27.52281430457074762, 5.000000000000000000 ) ) ;
#88917 = VERTEX_POINT ( 'NONE', #47142 ) ;
#88918 = VECTOR ( 'NONE', #54081, 1000.000000000000000 ) ;
#88919 = PLANE ( 'NONE',  #70219 ) ;
#88920 = FACE_OUTER_BOUND ( 'NONE', #16085, .T. ) ;
#88921 = VECTOR ( 'NONE', #43101, 1000.000000000000000 ) ;
#88922 = DIRECTION ( 'NONE',  ( 1.000000000000000000, 1.224606353822377258E-16, 0.000000000000000000 ) ) ;
#88923 = VERTEX_POINT ( 'NONE', #35529 ) ;
#88924 = PLANE ( 'NONE',  #85412 ) ;
#88925 = PLANE ( 'NONE',  #100528 ) ;
#88926 = EDGE_CURVE ( 'NONE', #31980, #94995, #79761, .T. ) ;
#88927 = DIRECTION ( 'NONE',  ( 0.000000000000000000, 1.000000000000000000, 0.000000000000000000 ) ) ;
#88928 = DIRECTION ( 'NONE',  ( -0.000000000000000000, -0.3543493200069152693, 0.9351131265310292928 ) ) ;
#88929 = DIRECTION ( 'NONE',  ( 0.7071067811865487940, -0.7071067811865463515, 0.000000000000000000 ) ) ;
#88930 = CARTESIAN_POINT ( 'NONE',  ( 2.962472949537105826, -7.464222240803106570E-16, -6.094999999999989981 ) ) ;
#88931 = VECTOR ( 'NONE', #140468, 1000.000000000000000 ) ;
#88932 = CARTESIAN_POINT ( 'NONE',  ( -7.499999999999944045, 1.466399257802248446, 5.000000000000000000 ) ) ;
#88933 = ORIENTED_EDGE ( 'NONE', *, *, #86571, .F. ) ;
#88934 = CARTESIAN_POINT ( 'NONE',  ( -8.292893218813398803, 14.25929247661557575, 5.000000000000000000 ) ) ;
#88935 = FACE_OUTER_BOUND ( 'NONE', #126028, .T. ) ;
#88936 = ORIENTED_EDGE ( 'NONE', *, *, #43640, .F. ) ;
#88937 = ORIENTED_EDGE ( 'NONE', *, *, #64578, .F. ) ;
#88938 = ORIENTED_EDGE ( 'NONE', *, *, #104721, .T. ) ;
#88939 = CARTESIAN_POINT ( 'NONE',  ( 58.18793019189810423, 6.110000000000002984, -1.637169565754156730 ) ) ;
#88940 = ORIENTED_EDGE ( 'NONE', *, *, #11537, .T. ) ;
#88941 = PLANE ( 'NONE',  #90543 ) ;
#88942 = AXIS2_PLACEMENT_3D ( 'NONE', #44949, #8129, #121015 ) ;
#88943 = CARTESIAN_POINT ( 'NONE',  ( 89.83376352523143282, 6.110000000000001208, 1.122388791418549305E-15 ) ) ;
#88944 = FACE_OUTER_BOUND ( 'NONE', #19208, .T. ) ;
#88945 = B_SPLINE_CURVE_WITH_KNOTS ( 'NONE', 3,
 ( #64756, #111838, #99491, #32864 ),
 .UNSPECIFIED., .F., .F.,
 ( 4, 4 ),
 ( 0.008853860144884172223, 0.009403245473020183098 ),
 .UNSPECIFIED. ) ;
#88946 = ORIENTED_EDGE ( 'NONE', *, *, #33298, .T. ) ;
#88947 = CARTESIAN_POINT ( 'NONE',  ( -34.42500000000001137, -22.22500000000000142, 5.000000000000000000 ) ) ;
#88948 = DIRECTION ( 'NONE',  ( -0.7071067811865486830, -0.7071067811865464625, 0.000000000000000000 ) ) ;
#88949 = ORIENTED_EDGE ( 'NONE', *, *, #86027, .F. ) ;
#88951 = EDGE_CURVE ( 'NONE', #132937, #104393, #91321, .T. ) ;
#88950 = VECTOR ( 'NONE', #50226, 1000.000000000000000 ) ;
#88952 = CARTESIAN_POINT ( 'NONE',  ( 12.79289321881337216, 12.75929247661559174, 5.000000000000000000 ) ) ;
#88953 = DIRECTION ( 'NONE',  ( 0.6830127018922181881, 0.6830127018922202975, -0.2588190451025214056 ) ) ;
#88954 = EDGE_LOOP ( 'NONE', ( #100198, #115776, #75324, #122789 ) ) ;
#88955 = ADVANCED_FACE ( 'NONE', ( #91997 ), #49246, .F. ) ;
#88956 = DIRECTION ( 'NONE',  ( 0.6830127018922180770, -0.6830127018922204085, -0.2588190451025213501 ) ) ;
#88957 = VERTEX_POINT ( 'NONE', #113758 ) ;
#88958 = ORIENTED_EDGE ( 'NONE', *, *, #96512, .T. ) ;
#88959 = ORIENTED_EDGE ( 'NONE', *, *, #106308, .F. ) ;
#88960 = CARTESIAN_POINT ( 'NONE',  ( 119.4954301918981230, 5.291415217122916737, 3.055000000000001936 ) ) ;
#88961 = CARTESIAN_POINT ( 'NONE',  ( 78.48921356237309510, -27.52281430457109934, 5.000000000000000000 ) ) ;
#88962 = DIRECTION ( 'NONE',  ( -1.000000000000000000, -1.224606353822377258E-16, -0.000000000000000000 ) ) ;
#88963 = EDGE_CURVE ( 'NONE', #114079, #47703, #52121, .T. ) ;
#88964 = ORIENTED_EDGE ( 'NONE', *, *, #57735, .T. ) ;
#88965 = CARTESIAN_POINT ( 'NONE',  ( 20.48334561358940675, 22.22500000000000142, 4.500000000000000888 ) ) ;
#88966 = VERTEX_POINT ( 'NONE', #83277 ) ;
#88967 = VECTOR ( 'NONE', #67160, 999.9999999999998863 ) ;
#88968 = VECTOR ( 'NONE', #53904, 1000.000000000000000 ) ;
#88969 = CARTESIAN_POINT ( 'NONE',  ( 9.020403141435219041, 7.934999999999989839, -2.126176841940961904 ) ) ;
#88970 = CARTESIAN_POINT ( 'NONE',  ( 19.41972383043609440, 4.584330080086930965E-16, 0.000000000000000000 ) ) ;
#88971 = DIRECTION ( 'NONE',  ( -0.7071067811865486830, 0.7071067811865464625, 0.000000000000000000 ) ) ;
#88972 = DIRECTION ( 'NONE',  ( -0.7071067811865487940, 0.7071067811865463515, -0.000000000000000000 ) ) ;
#88973 = ORIENTED_EDGE ( 'NONE', *, *, #40258, .T. ) ;
#88974 = CIRCLE ( 'NONE', #38368, 2.500000000000000444 ) ;
#88975 = ORIENTED_EDGE ( 'NONE', *, *, #62281, .T. ) ;
#88976 = ORIENTED_EDGE ( 'NONE', *, *, #141747, .F. ) ;
#88977 = LINE ( 'NONE', #44032, #101925 ) ;
#88978 = FACE_OUTER_BOUND ( 'NONE', #39765, .T. ) ;
#88979 = CARTESIAN_POINT ( 'NONE',  ( 36.48921356237310221, -27.52281430457080802, 5.000000000000000000 ) ) ;
#88980 = LINE ( 'NONE', #21567, #87618 ) ;
#88981 = LINE ( 'NONE', #112157, #101606 ) ;
#88982 = VECTOR ( 'NONE', #33370, 1000.000000000000000 ) ;
#88983 = CARTESIAN_POINT ( 'NONE',  ( 1.499999999999994449, 9.052185695429081136, 5.000000000000000000 ) ) ;
#88984 = CARTESIAN_POINT ( 'NONE',  ( -9.489213562373095101, -27.52281430457062328, 5.000000000000000000 ) ) ;
#88985 = DIRECTION ( 'NONE',  ( -1.000000000000000000, 7.120242111146219159E-15, 0.000000000000000000 ) ) ;
#88986 = ORIENTED_EDGE ( 'NONE', *, *, #44980, .T. ) ;
#88987 = CARTESIAN_POINT ( 'NONE',  ( -23.99999999999983302, 7.931123077392102871, 4.000000000000000000 ) ) ;
#88988 = VERTEX_POINT ( 'NONE', #81148 ) ;
#88989 = CARTESIAN_POINT ( 'NONE',  ( 19.75016440660220951, -1.782848796972203331, -32.42302261545219011 ) ) ;
#88990 = EDGE_LOOP ( 'NONE', ( #132891, #143178, #68897, #10415 ) ) ;
#88991 =( BOUNDED_CURVE ( )  B_SPLINE_CURVE ( 3, ( #124809, #58902, #122121, #70484 ),
 .UNSPECIFIED., .F., .F. ) 
 B_SPLINE_CURVE_WITH_KNOTS ( ( 4, 4 ),
 ( 2.276824562219553395E-15, 1.570796326794894338 ),
 .UNSPECIFIED. ) 
 CURVE ( )  GEOMETRIC_REPRESENTATION_ITEM ( )  RATIONAL_B_SPLINE_CURVE ( ( 1.000000000000000000, 0.8047378541243661587, 0.8047378541243661587, 1.000000000000000000 ) ) 
 REPRESENTATION_ITEM ( '' )  );
#88992 = DIRECTION ( 'NONE',  ( 0.7071067811865486830, -0.7071067811865464625, -0.000000000000000000 ) ) ;
#88994 = ORIENTED_EDGE ( 'NONE', *, *, #107205, .T. ) ;
#88993 = CYLINDRICAL_SURFACE ( 'NONE', #20940, 7.950000000000000178 ) ;
#88995 = VECTOR ( 'NONE', #14234, 1000.000000000000000 ) ;
#88996 = LINE ( 'NONE', #57090, #4619 ) ;
#88997 = CARTESIAN_POINT ( 'NONE',  ( 26.24139925780185578, 21.72500000000000142, 5.000000000000000000 ) ) ;
#88998 = ADVANCED_FACE ( 'NONE', ( #70995 ), #61556, .F. ) ;
#88999 = ORIENTED_EDGE ( 'NONE', *, *, #43027, .F. ) ;
#89000 = PLANE ( 'NONE',  #85535 ) ;
#89001 = ORIENTED_EDGE ( 'NONE', *, *, #18502, .F. ) ;
#89002 = CARTESIAN_POINT ( 'NONE',  ( 0.1161069444170876597, 0.000000000000000000, 0.000000000000000000 ) ) ;
#89003 = EDGE_LOOP ( 'NONE', ( #52566, #37880, #80274, #83147 ) ) ;
#89004 = AXIS2_PLACEMENT_3D ( 'NONE', #41313, #46924, #48286 ) ;
#89005 = CARTESIAN_POINT ( 'NONE',  ( -8.345055162546129779, 5.259292476615662792, 12.77922209995892011 ) ) ;
#89007 = EDGE_CURVE ( 'NONE', #43696, #116862, #102897, .T. ) ;
#89006 = CARTESIAN_POINT ( 'NONE',  ( 110.9125270504628986, -7.949999999999998401, -4.867971026610728450E-16 ) ) ;
#89009 = VECTOR ( 'NONE', #19045, 1000.000000000000000 ) ;
#89008 = CYLINDRICAL_SURFACE ( 'NONE', #16071, 0.5000000000000004441 ) ;
#89010 = VECTOR ( 'NONE', #85369, 1000.000000000000227 ) ;
#89011 = DIRECTION ( 'NONE',  ( -0.7071067811865486830, -0.7071067811865464625, 0.000000000000000000 ) ) ;
#89012 = EDGE_CURVE ( 'NONE', #8228, #109090, #58729, .T. ) ;
#89013 = CARTESIAN_POINT ( 'NONE',  ( 2.999999999999975131, 9.631307414974328296, -9.079085613539536581 ) ) ;
#89014 = LINE ( 'NONE', #112877, #42618 ) ;
#89015 = EDGE_CURVE ( 'NONE', #47310, #89141, #3532, .T. ) ;
#89016 = LINE ( 'NONE', #24442, #122514 ) ;
#89017 = CARTESIAN_POINT ( 'NONE',  ( 16.91666666666666785, 5.278424836066147208, 3.047499999999990550 ) ) ;
#89018 = CARTESIAN_POINT ( 'NONE',  ( -2.510786437626908008, -27.52281430457053446, 5.000000000000000000 ) ) ;
#89019 = CARTESIAN_POINT ( 'NONE',  ( 0.000000000000000000, -0.5999999999999994227, -3.054668707061620747 ) ) ;
#89021 = EDGE_CURVE ( 'NONE', #88053, #77065, #116612, .T. ) ;
#89020 = FACE_OUTER_BOUND ( 'NONE', #25217, .T. ) ;
#89022 = VERTEX_POINT ( 'NONE', #49948 ) ;
#89023 = ORIENTED_EDGE ( 'NONE', *, *, #106279, .F. ) ;
#89024 = CARTESIAN_POINT ( 'NONE',  ( 22.82816939922337696, 12.75929247661558996, 4.000000000000000000 ) ) ;
#89025 = ORIENTED_EDGE ( 'NONE', *, *, #106209, .T. ) ;
#89026 = EDGE_CURVE ( 'NONE', #91989, #70462, #60855, .T. ) ;
#89027 = CARTESIAN_POINT ( 'NONE',  ( 103.6879301918981042, 6.110000000000002984, -1.637169565754156730 ) ) ;
#89028 = CARTESIAN_POINT ( 'NONE',  ( -3.328169399223507519, -12.74070752338415602, 4.000000000000000000 ) ) ;
#89029 = LINE ( 'NONE', #135393, #16187 ) ;
#89030 = LINE ( 'NONE', #58580, #40038 ) ;
#89031 = LINE ( 'NONE', #67265, #135861 ) ;
#89032 = ORIENTED_EDGE ( 'NONE', *, *, #24236, .F. ) ;
#89033 = DIRECTION ( 'NONE',  ( 1.000000000000000000, 1.084202172485504681E-16, 0.000000000000000000 ) ) ;
#89034 = CYLINDRICAL_SURFACE ( 'NONE', #106676, 0.5000000000000004441 ) ;
#89035 = EDGE_CURVE ( 'NONE', #98425, #34748, #127487, .T. ) ;
#89036 = DIRECTION ( 'NONE',  ( 0.000000000000000000, 0.000000000000000000, -1.000000000000000000 ) ) ;
#89037 = ADVANCED_FACE ( 'NONE', ( #104281 ), #136937, .F. ) ;
#89038 = LINE ( 'NONE', #54973, #67054 ) ;
#89039 = CARTESIAN_POINT ( 'NONE',  ( -54.48921356237310221, -27.52281430457093236, 5.000000000000000000 ) ) ;
#89041 = ORIENTED_EDGE ( 'NONE', *, *, #131390, .F. ) ;
#89040 = CARTESIAN_POINT ( 'NONE',  ( -4.499999999999972466, 19.39370406404966829, 1.459788787078212025 ) ) ;
#89042 = DIRECTION ( 'NONE',  ( -1.000000000000000000, -1.224606353822377258E-16, -0.000000000000000000 ) ) ;
#89043 = DIRECTION ( 'NONE',  ( 0.7071067811865486830, -0.7071067811865464625, -0.000000000000000000 ) ) ;
#89044 = LINE ( 'NONE', #78884, #68829 ) ;
#89045 = EDGE_CURVE ( 'NONE', #10796, #133726, #93439, .T. ) ;
#89046 = CARTESIAN_POINT ( 'NONE',  ( 24.48921356237309510, -27.52281430457072631, 5.000000000000000000 ) ) ;
#89047 = ORIENTED_EDGE ( 'NONE', *, *, #49381, .F. ) ;
#89048 = VERTEX_POINT ( 'NONE', #103573 ) ;
#89049 = VERTEX_POINT ( 'NONE', #5683 ) ;
#89050 = CARTESIAN_POINT ( 'NONE',  ( 94.06293019189809002, 1.637169565754157174, 6.110000000000002984 ) ) ;
#89051 = ORIENTED_EDGE ( 'NONE', *, *, #88963, .F. ) ;
#89052 = LINE ( 'NONE', #35401, #78758 ) ;
#89053 = DIRECTION ( 'NONE',  ( -0.000000000000000000, -0.3543493200069152693, 0.9351131265310292928 ) ) ;
#89054 = DIRECTION ( 'NONE',  ( 1.000000000000000000, 0.000000000000000000, 0.000000000000000000 ) ) ;
#89055 = ORIENTED_EDGE ( 'NONE', *, *, #53978, .F. ) ;
#89056 = LINE ( 'NONE', #122348, #118480 ) ;
#89058 = AXIS2_PLACEMENT_3D ( 'NONE', #34719, #123165, #25249 ) ;
#89057 = CARTESIAN_POINT ( 'NONE',  ( -32.29289321881321939, 11.25929247661559884, 5.000000000000000000 ) ) ;
#89059 = CARTESIAN_POINT ( 'NONE',  ( 82.16209685856479439, -5.291415217122919401, 3.054999999999997939 ) ) ;
#89060 = VERTEX_POINT ( 'NONE', #94129 ) ;
#89061 = LINE ( 'NONE', #45575, #74407 ) ;
#89062 = EDGE_CURVE ( 'NONE', #11322, #13287, #136216, .T. ) ;
#89063 = CARTESIAN_POINT ( 'NONE',  ( 34.49999999999975842, 12.05432934483081908, 4.994342998332162331 ) ) ;
#89064 = ORIENTED_EDGE ( 'NONE', *, *, #61082, .T. ) ;
#89065 = ORIENTED_EDGE ( 'NONE', *, *, #55260, .F. ) ;
#89066 = EDGE_LOOP ( 'NONE', ( #135853, #58714, #57937, #5105 ) ) ;
#89067 = LINE ( 'NONE', #133287, #51483 ) ;
#89068 = DIRECTION ( 'NONE',  ( 1.000000000000000000, -0.000000000000000000, 0.000000000000000000 ) ) ;
#89069 = CIRCLE ( 'NONE', #139689, 2.500000000000000444 ) ;
#89070 = LINE ( 'NONE', #67315, #103525 ) ;
#89071 = EDGE_CURVE ( 'NONE', #107544, #99130, #39798, .T. ) ;
#89072 = CARTESIAN_POINT ( 'NONE',  ( 6.639999999999993463, -34.64999999999999858, -40.00000000000000000 ) ) ;
#89073 = DIRECTION ( 'NONE',  ( 0.7071067811865486830, -0.7071067811865464625, -0.000000000000000000 ) ) ;
#89074 = AXIS2_PLACEMENT_3D ( 'NONE', #52966, #9446, #42851 ) ;
#89075 = EDGE_LOOP ( 'NONE', ( #123518, #15395, #11419, #124505 ) ) ;
#89076 = VERTEX_POINT ( 'NONE', #94831 ) ;
#89077 = AXIS2_PLACEMENT_3D ( 'NONE', #88663, #111837, #44459 ) ;
#89078 = CYLINDRICAL_SURFACE ( 'NONE', #124365, 0.5000000000000004441 ) ;
#89080 = VERTEX_POINT ( 'NONE', #125358 ) ;
#89079 = EDGE_CURVE ( 'NONE', #115930, #103304, #27438, .T. ) ;
#89081 = ORIENTED_EDGE ( 'NONE', *, *, #8426, .F. ) ;
#89082 = CARTESIAN_POINT ( 'NONE',  ( -35.93988928955958073, -9.740707523384177335, 10.89222023123389427 ) ) ;
#89083 = EDGE_LOOP ( 'NONE', ( #2747, #6244, #143210, #21295 ) ) ;
#89084 = VECTOR ( 'NONE', #7638, 1000.000000000000227 ) ;
#89085 = DIRECTION ( 'NONE',  ( 0.000000000000000000, 1.000000000000000000, 6.123233995736750012E-17 ) ) ;
#89086 = DIRECTION ( 'NONE',  ( -0.7071067811865487940, 0.7071067811865463515, -0.000000000000000000 ) ) ;
#89087 = EDGE_CURVE ( 'NONE', #110076, #121606, #70308, .T. ) ;
#89088 = DIRECTION ( 'NONE',  ( -0.7071067811865486830, -0.7071067811865464625, -0.000000000000000000 ) ) ;
#89089 = DIRECTION ( 'NONE',  ( 0.000000000000000000, -1.000000000000000000, 0.000000000000000000 ) ) ;
#89090 = CARTESIAN_POINT ( 'NONE',  ( 34.92499999999998295, -11.14387692260747365, 4.000000000000000000 ) ) ;
#89091 = EDGE_LOOP ( 'NONE', ( #47364, #101929, #131856, #78856 ) ) ;
#89092 = ORIENTED_EDGE ( 'NONE', *, *, #42105, .F. ) ;
#89094 = EDGE_CURVE ( 'NONE', #6909, #69387, #48502, .T. ) ;
#89093 = LINE ( 'NONE', #47066, #122168 ) ;
#89095 = ORIENTED_EDGE ( 'NONE', *, *, #135003, .T. ) ;
#89096 = FACE_OUTER_BOUND ( 'NONE', #91868, .T. ) ;
#89097 = ORIENTED_EDGE ( 'NONE', *, *, #120810, .F. ) ;
#89098 = CARTESIAN_POINT ( 'NONE',  ( 36.48921356237310221, -27.52281430457080802, 5.000000000000000000 ) ) ;
#89099 = ORIENTED_EDGE ( 'NONE', *, *, #19685, .T. ) ;
#89100 = ORIENTED_EDGE ( 'NONE', *, *, #12093, .F. ) ;
#89101 = ORIENTED_EDGE ( 'NONE', *, *, #110101, .F. ) ;
#89102 = VECTOR ( 'NONE', #84903, 1000.000000000000000 ) ;
#89103 = LINE ( 'NONE', #133324, #106756 ) ;
#89104 = STYLED_ITEM ( 'NONE', ( #124580 ), #107309 ) ;
#89105 = CYLINDRICAL_SURFACE ( 'NONE', #92291, 2.500000000000000444 ) ;
#89106 = DIRECTION ( 'NONE',  ( -0.000000000000000000, 0.3543493200069153248, 0.9351131265310292928 ) ) ;
#89107 = CARTESIAN_POINT ( 'NONE',  ( 119.7295968585647756, -6.110000000000000320, -1.637169565754161393 ) ) ;
#89108 = CARTESIAN_POINT ( 'NONE',  ( 0.000000000000000000, 0.000000000000000000, 5.000000000000000000 ) ) ;
#89109 = AXIS2_PLACEMENT_3D ( 'NONE', #6998, #40415, #94047 ) ;
#89110 = CARTESIAN_POINT ( 'NONE',  ( -15.18398860626900237, 28.73617430169797871, 5.000000000000000000 ) ) ;
#89111 = DIRECTION ( 'NONE',  ( 0.7071067811865486830, -0.7071067811865464625, -0.000000000000000000 ) ) ;
#89112 = LINE ( 'NONE', #10787, #2953 ) ;
#89113 = EDGE_CURVE ( 'NONE', #37814, #26730, #99100, .T. ) ;
#89114 = DIRECTION ( 'NONE',  ( 0.7071067811865486830, -0.7071067811865464625, -0.000000000000000000 ) ) ;
#89115 = ORIENTED_EDGE ( 'NONE', *, *, #22351, .F. ) ;
#89116 = EDGE_CURVE ( 'NONE', #45124, #100098, #108548, .T. ) ;
#89117 = CARTESIAN_POINT ( 'NONE',  ( 19.88840764549667384, 9.139736423841732040E-16, 0.000000000000000000 ) ) ;
#89118 = CARTESIAN_POINT ( 'NONE',  ( 45.18398860626900415, 28.73617430169818832, 5.000000000000000000 ) ) ;
#89119 = ORIENTED_EDGE ( 'NONE', *, *, #56631, .T. ) ;
#89120 = ORIENTED_EDGE ( 'NONE', *, *, #92910, .T. ) ;
#89121 = VERTEX_POINT ( 'NONE', #118744 ) ;
#89122 = DIRECTION ( 'NONE',  ( -0.000000000000000000, -0.3543493200069152693, 0.9351131265310292928 ) ) ;
#89123 = EDGE_LOOP ( 'NONE', ( #95988, #123335, #101556, #7542, #41050, #74999 ) ) ;
#89124 = VERTEX_POINT ( 'NONE', #96250 ) ;
#89125 = DIRECTION ( 'NONE',  ( -0.3543493200069162685, -0.000000000000000000, -0.9351131265310288487 ) ) ;
#89126 = CARTESIAN_POINT ( 'NONE',  ( 14.77497294953710494, 4.461849672132300881, 4.461849672132299105 ) ) ;
#89127 = DIRECTION ( 'NONE',  ( -0.6830127018922181881, 0.6830127018922202975, -0.2588190451025214056 ) ) ;
#89128 = EDGE_CURVE ( 'NONE', #83224, #89438, #99988, .T. ) ;
#89129 = DIRECTION ( 'NONE',  ( -0.7071067811865486830, 0.7071067811865464625, 0.000000000000000000 ) ) ;
#89130 = VERTEX_POINT ( 'NONE', #98433 ) ;
#89131 = DIRECTION ( 'NONE',  ( -0.7071067811865486830, 0.7071067811865464625, 0.000000000000000000 ) ) ;
#89132 = ORIENTED_EDGE ( 'NONE', *, *, #88741, .T. ) ;
#89133 = LINE ( 'NONE', #136184, #118623 ) ;
#89134 = CARTESIAN_POINT ( 'NONE',  ( 23.69206980810188057, -7.934999999999991616, -2.126176841940955242 ) ) ;
#89135 = ORIENTED_EDGE ( 'NONE', *, *, #136972, .F. ) ;
#89136 = CARTESIAN_POINT ( 'NONE',  ( 84.93293019189812298, 1.637169565754156730, 6.110000000000001208 ) ) ;
#89137 = CARTESIAN_POINT ( 'NONE',  ( 6.856969496093653582, -9.116755745626452523, 2.682239519146091045 ) ) ;
#89138 = CARTESIAN_POINT ( 'NONE',  ( -34.45011844616455221, -5.997695858405977631, 5.000000000000000888 ) ) ;
#89139 = VERTEX_POINT ( 'NONE', #7832 ) ;
#89140 = EDGE_LOOP ( 'NONE', ( #118680, #33123, #128419, #24977 ) ) ;
#89141 = VERTEX_POINT ( 'NONE', #128907 ) ;
#89142 = CARTESIAN_POINT ( 'NONE',  ( -8.999999999999937828, 8.587461875839158765, 4.000000000000000000 ) ) ;
#89143 = LINE ( 'NONE', #77567, #11613 ) ;
#89144 = CARTESIAN_POINT ( 'NONE',  ( -31.17183060077625711, -11.24070752338416490, 4.000000000000000000 ) ) ;
#89145 = DIRECTION ( 'NONE',  ( 0.7071067811865487940, 0.7071067811865463515, 0.000000000000000000 ) ) ;
#89146 = EDGE_CURVE ( 'NONE', #52088, #76199, #41923, .T. ) ;
#89147 = VERTEX_POINT ( 'NONE', #141965 ) ;
#89148 = CARTESIAN_POINT ( 'NONE',  ( -23.99999999999981881, -16.44781430457065952, 5.000000000000000000 ) ) ;
#89149 = PLANE ( 'NONE',  #74644 ) ;
#89150 = ORIENTED_EDGE ( 'NONE', *, *, #83262, .F. ) ;
#89151 = DIRECTION ( 'NONE',  ( 0.7071067811865487940, 0.7071067811865463515, 0.000000000000000000 ) ) ;
#89152 = FACE_OUTER_BOUND ( 'NONE', #5678, .T. ) ;
#89153 = EDGE_LOOP ( 'NONE', ( #50656, #72748, #56357, #13847 ) ) ;
#89155 = EDGE_LOOP ( 'NONE', ( #51361, #134707, #134053, #64133, #78083 ) ) ;
#89154 = PLANE ( 'NONE',  #55640 ) ;
#89156 = ORIENTED_EDGE ( 'NONE', *, *, #68123, .T. ) ;
#89157 = CARTESIAN_POINT ( 'NONE',  ( -6.722814304570563948, -21.72499999999999432, 5.000000000000000000 ) ) ;
#89158 = LINE ( 'NONE', #78286, #20554 ) ;
#89159 = ORIENTED_EDGE ( 'NONE', *, *, #14908, .F. ) ;
#89160 = LINE ( 'NONE', #4944, #44375 ) ;
#89161 =( BOUNDED_CURVE ( )  B_SPLINE_CURVE ( 2, ( #142278, #140134, #108158, #29202, #54556, #107478, #119063, #18296, #8141, #73443, #85012, #8823, #42964 ),
 .UNSPECIFIED., .F., .T. ) 
 B_SPLINE_CURVE_WITH_KNOTS ( ( 3, 2, 2, 2, 2, 2, 3 ),
 ( 0.5000000000000000000, 0.5027777777777777679, 0.5055555555555555358, 0.5083333333333333037, 0.5111111111111110716, 0.5138888888888888395, 0.5166666666666667185 ),
 .UNSPECIFIED. ) 
 CURVE ( )  GEOMETRIC_REPRESENTATION_ITEM ( )  RATIONAL_B_SPLINE_CURVE ( ( 1.000000000000000000, 0.9659258262890683122, 1.000000000000000000, 0.9659258262890683122, 1.000000000000000000, 0.9659258262890683122, 1.000000000000000000, 0.9659258262890683122, 1.000000000000000000, 0.9659258262890683122, 1.000000000000000000, 0.9659258262890683122, 1.000000000000000000 ) ) 
 REPRESENTATION_ITEM ( '' )  );
#89162 = CARTESIAN_POINT ( 'NONE',  ( -15.29974487139158867, -27.71228299555216879, 4.000000000000000000 ) ) ;
#89163 = AXIS2_PLACEMENT_3D ( 'NONE', #68031, #12856, #55690 ) ;
#89164 = EDGE_CURVE ( 'NONE', #63415, #96788, #109304, .T. ) ;
#89165 = FACE_OUTER_BOUND ( 'NONE', #97773, .T. ) ;
#89166 = FACE_OUTER_BOUND ( 'NONE', #49511, .T. ) ;
#89167 = ADVANCED_FACE ( 'NONE', ( #141207 ), #85393, .F. ) ;
#89168 = CARTESIAN_POINT ( 'NONE',  ( 16.82816939922341248, 12.75929247661558819, 4.000000000000000000 ) ) ;
#89169 = DIRECTION ( 'NONE',  ( -0.000000000000000000, 0.3543493200069153248, 0.9351131265310292928 ) ) ;
#89170 = DIRECTION ( 'NONE',  ( 0.6830127018922180770, -0.6830127018922204085, -0.2588190451025213501 ) ) ;
#89171 = ADVANCED_FACE ( 'NONE', ( #30317 ), #74556, .F. ) ;
#89172 = LINE ( 'NONE', #31227, #92289 ) ;
#89173 = CARTESIAN_POINT ( 'NONE',  ( 19.22873647476855652, 5.808823158059031044, -5.808823158059038150 ) ) ;
#89174 = LINE ( 'NONE', #86325, #25904 ) ;
#89175 = FACE_OUTER_BOUND ( 'NONE', #8700, .T. ) ;
#89176 = CARTESIAN_POINT ( 'NONE',  ( -8.241399257801971245, 21.72500000000000142, 5.000000000000000000 ) ) ;
#89178 = ADVANCED_FACE ( 'NONE', ( #7094 ), #67996, .T. ) ;
#89177 = CARTESIAN_POINT ( 'NONE',  ( -7.140000000000002345, -35.56014942880460694, -11.72188031596274982 ) ) ;
#89180 = EDGE_CURVE ( 'NONE', #86644, #55203, #33904, .T. ) ;
#89179 = ORIENTED_EDGE ( 'NONE', *, *, #179, .T. ) ;
#89181 = ORIENTED_EDGE ( 'NONE', *, *, #19732, .T. ) ;
#89182 = CARTESIAN_POINT ( 'NONE',  ( 98.56250000000000000, -5.819803920172572198, -5.819803920172573086 ) ) ;
#89183 = ORIENTED_EDGE ( 'NONE', *, *, #1984, .T. ) ;
#89184 = VECTOR ( 'NONE', #94308, 1000.000000000000000 ) ;
#89185 = EDGE_LOOP ( 'NONE', ( #70750, #2220, #58549, #143068 ) ) ;
#89186 = ORIENTED_EDGE ( 'NONE', *, *, #83746, .F. ) ;
#89187 = CARTESIAN_POINT ( 'NONE',  ( -17.51078643762690845, -27.52281430457043143, 5.000000000000000000 ) ) ;
#89188 = FACE_OUTER_BOUND ( 'NONE', #44216, .T. ) ;
#89189 = ORIENTED_EDGE ( 'NONE', *, *, #97849, .T. ) ;
#89190 = CARTESIAN_POINT ( 'NONE',  ( -30.88837638105223249, 9.759292476615614831, 17.35367589129219823 ) ) ;
#89191 = DIRECTION ( 'NONE',  ( 0.7071067811865487940, -0.7071067811865463515, 0.000000000000000000 ) ) ;
#89192 = EDGE_CURVE ( 'NONE', #90802, #61417, #123050, .T. ) ;
#89193 = CARTESIAN_POINT ( 'NONE',  ( -0.4892135623730947680, -27.52281430457055578, 5.000000000000000000 ) ) ;
#89194 = PLANE ( 'NONE',  #74349 ) ;
#89195 = ORIENTED_EDGE ( 'NONE', *, *, #69919, .F. ) ;
#89196 = EDGE_CURVE ( 'NONE', #69443, #124524, #2666, .T. ) ;
#89197 = CARTESIAN_POINT ( 'NONE',  ( 20.22995720542193254, 21.73644205237998506, 5.000000000000000888 ) ) ;
#89198 = CARTESIAN_POINT ( 'NONE',  ( 8.968407645496675684, 9.139736423841732040E-16, 0.000000000000000000 ) ) ;
#89199 = DIRECTION ( 'NONE',  ( 0.7071067811865486830, -0.7071067811865464625, -0.000000000000000000 ) ) ;
#89200 = CARTESIAN_POINT ( 'NONE',  ( 27.00000000000001421, 3.441786896390103934, 7.166352137582786774 ) ) ;
#89201 = DIRECTION ( 'NONE',  ( 0.6830127018922181881, 0.6830127018922202975, -0.2588190451025214056 ) ) ;
#89202 = CARTESIAN_POINT ( 'NONE',  ( -12.69999999999998153, 0.000000000000000000, 2.500000000000000444 ) ) ;
#89203 = CARTESIAN_POINT ( 'NONE',  ( 85.68336038379622721, -2.130196079827426203, 7.949999999999996625 ) ) ;
#89204 = EDGE_CURVE ( 'NONE', #41627, #42504, #44062, .T. ) ;
#89205 = VECTOR ( 'NONE', #56617, 1000.000000000000000 ) ;
#89206 = CARTESIAN_POINT ( 'NONE',  ( -12.69999999999998153, 0.3999999999999995226, 2.467792535850613866 ) ) ;
#89207 = VECTOR ( 'NONE', #6150, 1000.000000000000000 ) ;
#89208 = ORIENTED_EDGE ( 'NONE', *, *, #16701, .T. ) ;
#89209 = ORIENTED_EDGE ( 'NONE', *, *, #70983, .T. ) ;
#89210 = VECTOR ( 'NONE', #117599, 1000.000000000000000 ) ;
#89211 = CARTESIAN_POINT ( 'NONE',  ( 123.2295968585647756, -6.110000000000000320, -1.637169565754161393 ) ) ;
#89212 = ORIENTED_EDGE ( 'NONE', *, *, #111853, .F. ) ;
#89213 = VECTOR ( 'NONE', #58076, 1000.000000000000000 ) ;
#89214 = FACE_OUTER_BOUND ( 'NONE', #121874, .T. ) ;
#89215 = EDGE_CURVE ( 'NONE', #133767, #23195, #114774, .T. ) ;
#89216 = PLANE ( 'NONE',  #17853 ) ;
#89217 = DIRECTION ( 'NONE',  ( 0.7071067811865487940, 0.7071067811865463515, -0.000000000000000000 ) ) ;
#89218 = CARTESIAN_POINT ( 'NONE',  ( 118.4745968585647802, 1.637169565754164058, -6.109999999999996767 ) ) ;
#89219 = ORIENTED_EDGE ( 'NONE', *, *, #1558, .T. ) ;
#89220 = ORIENTED_EDGE ( 'NONE', *, *, #78354, .F. ) ;
#89221 = EDGE_CURVE ( 'NONE', #46307, #27599, #21592, .T. ) ;
#89222 = LINE ( 'NONE', #133444, #32303 ) ;
#89223 = PLANE ( 'NONE',  #17653 ) ;
#89224 = EDGE_LOOP ( 'NONE', ( #119817, #76427, #81838, #12604 ) ) ;
#89225 = VERTEX_POINT ( 'NONE', #68682 ) ;
#89226 = CARTESIAN_POINT ( 'NONE',  ( 35.87543019189811133, -5.291415217122920289, -3.055000000000001492 ) ) ;
#89227 = ORIENTED_EDGE ( 'NONE', *, *, #128931, .F. ) ;
#89228 = DIRECTION ( 'NONE',  ( 1.000000000000000000, 1.224606353822377258E-16, 0.000000000000000000 ) ) ;
#89229 = CARTESIAN_POINT ( 'NONE',  ( -23.99999999999982236, 11.58746187583912324, 4.000000000000000000 ) ) ;
#89230 = CARTESIAN_POINT ( 'NONE',  ( 26.99999999999980815, 16.93112307739200872, 4.000000000000000000 ) ) ;
#89231 = EDGE_CURVE ( 'NONE', #17414, #16132, #119056, .T. ) ;
#89232 = CARTESIAN_POINT ( 'NONE',  ( 34.18293019189809456, -1.637169565754158951, -6.109999999999998543 ) ) ;
#89233 = ORIENTED_EDGE ( 'NONE', *, *, #30767, .T. ) ;
#89234 = PLANE ( 'NONE',  #98788 ) ;
#89235 = ORIENTED_EDGE ( 'NONE', *, *, #3323, .F. ) ;
#89236 = ORIENTED_EDGE ( 'NONE', *, *, #85735, .F. ) ;
#89237 = EDGE_LOOP ( 'NONE', ( #138382, #63057, #123626, #102210 ) ) ;
#89238 = CARTESIAN_POINT ( 'NONE',  ( -3.489213562373097322, -27.52281430457057709, 5.000000000000000000 ) ) ;
#89239 = CARTESIAN_POINT ( 'NONE',  ( -66.18398860626901126, 28.73617430169833753, 5.000000000000000000 ) ) ;
#89240 = ORIENTED_EDGE ( 'NONE', *, *, #45338, .F. ) ;
#89241 = DIRECTION ( 'NONE',  ( 1.000000000000000000, 0.000000000000000000, 0.000000000000000000 ) ) ;
#89242 = EDGE_CURVE ( 'NONE', #15478, #3113, #35349, .T. ) ;
#89243 = CARTESIAN_POINT ( 'NONE',  ( -34.92500000000001137, 22.22500000000000142, 4.000000000000000000 ) ) ;
#89244 =( LENGTH_UNIT ( ) NAMED_UNIT ( * ) SI_UNIT ( .MILLI., .METRE. ) );
#89245 = DIRECTION ( 'NONE',  ( -0.6830127018922180770, -0.6830127018922204085, -0.2588190451025213501 ) ) ;
#89246 = FACE_BOUND ( 'NONE', #122087, .T. ) ;
#89247 = ORIENTED_EDGE ( 'NONE', *, *, #51762, .F. ) ;
#89248 = CARTESIAN_POINT ( 'NONE',  ( 9.524999999999998579, -4.870000000000013429, -40.00000000000000000 ) ) ;
#89250 = EDGE_CURVE ( 'NONE', #133772, #30172, #521, .T. ) ;
#89249 = DIRECTION ( 'NONE',  ( -0.2399999999999972433, 3.469446951953571048E-17, -0.9707728879609286432 ) ) ;
#89251 = CARTESIAN_POINT ( 'NONE',  ( 18.32840764549667512, 9.139736423841732040E-16, 0.000000000000000000 ) ) ;
#89252 = PLANE ( 'NONE',  #71712 ) ;
#89253 = VERTEX_POINT ( 'NONE', #65852 ) ;
#89254 = LINE ( 'NONE', #88560, #15655 ) ;
#89255 = ORIENTED_EDGE ( 'NONE', *, *, #121229, .F. ) ;
#89256 = ORIENTED_EDGE ( 'NONE', *, *, #3817, .F. ) ;
#89257 = VERTEX_POINT ( 'NONE', #1230 ) ;
#89258 = CIRCLE ( 'NONE', #79991, 2.055000000000001048 ) ;
#89259 = CARTESIAN_POINT ( 'NONE',  ( 43.37043019189810877, -3.055000000000001492, 5.291415217122917625 ) ) ;
#89260 = EDGE_LOOP ( 'NONE', ( #92878, #38821, #106419, #54871 ) ) ;
#89261 = DIRECTION ( 'NONE',  ( 0.7071067811865487940, 0.7071067811865463515, 0.000000000000000000 ) ) ;
#89262 = VECTOR ( 'NONE', #20729, 1000.000000000000000 ) ;
#89263 = DIRECTION ( 'NONE',  ( -0.7071067811865486830, 0.7071067811865464625, 0.000000000000000000 ) ) ;
#89264 = CARTESIAN_POINT ( 'NONE',  ( 57.18398860626899705, 28.73617430169827358, 5.000000000000000000 ) ) ;
#89265 = ORIENTED_EDGE ( 'NONE', *, *, #136983, .T. ) ;
#89266 = DIRECTION ( 'NONE',  ( -0.6830127018922180770, -0.6830127018922204085, -0.2588190451025213501 ) ) ;
#89267 =( BOUNDED_CURVE ( )  B_SPLINE_CURVE ( 3, ( #117689, #130778, #41588, #30745 ),
 .UNSPECIFIED., .F., .T. ) 
 B_SPLINE_CURVE_WITH_KNOTS ( ( 4, 4 ),
 ( 1.901594255663624056, 1.933014472006547635 ),
 .UNSPECIFIED. ) 
 CURVE ( )  GEOMETRIC_REPRESENTATION_ITEM ( )  RATIONAL_B_SPLINE_CURVE ( ( 1.000000000000000000, 0.9999177325257868620, 0.9999177325257868620, 1.000000000000000000 ) ) 
 REPRESENTATION_ITEM ( '' )  );
#89268 = DIRECTION ( 'NONE',  ( 1.000000000000000000, 0.000000000000000000, 0.000000000000000000 ) ) ;
#89269 = VECTOR ( 'NONE', #89693, 1000.000000000000227 ) ;
#89270 = DIRECTION ( 'NONE',  ( -0.6830127018922180770, -0.6830127018922204085, -0.2588190451025213501 ) ) ;
#89271 = EDGE_CURVE ( 'NONE', #92661, #98173, #79593, .T. ) ;
#89272 = FACE_OUTER_BOUND ( 'NONE', #69629, .T. ) ;
#89273 = DIRECTION ( 'NONE',  ( -0.000000000000000000, 1.000000000000000000, -0.000000000000000000 ) ) ;
#89274 = ORIENTED_EDGE ( 'NONE', *, *, #28449, .F. ) ;
#89275 = EDGE_LOOP ( 'NONE', ( #35806, #60425, #43318, #36887 ) ) ;
#89276 = ORIENTED_EDGE ( 'NONE', *, *, #82459, .F. ) ;
#89277 = ORIENTED_EDGE ( 'NONE', *, *, #43215, .T. ) ;
#89278 = LINE ( 'NONE', #45799, #68202 ) ;
#89279 = LINE ( 'NONE', #142941, #123214 ) ;
#89280 = ORIENTED_EDGE ( 'NONE', *, *, #39622, .F. ) ;
#89281 = ORIENTED_EDGE ( 'NONE', *, *, #58443, .F. ) ;
#89282 =( NAMED_UNIT ( * ) SI_UNIT ( $, .STERADIAN. ) SOLID_ANGLE_UNIT ( ) );
#89283 = EDGE_CURVE ( 'NONE', #97187, #121745, #123776, .T. ) ;
#89284 = EDGE_CURVE ( 'NONE', #52318, #106536, #120881, .T. ) ;
#89285 = CARTESIAN_POINT ( 'NONE',  ( -5.292893218813417455, 17.25929247661554200, 5.000000000000000000 ) ) ;
#89286 = ORIENTED_EDGE ( 'NONE', *, *, #37132, .F. ) ;
#89287 = CARTESIAN_POINT ( 'NONE',  ( 20.36747333860806819, 3.821174125832445049E-16, 0.000000000000000000 ) ) ;
#89288 = VECTOR ( 'NONE', #98307, 999.9999999999998863 ) ;
#89289 = DIRECTION ( 'NONE',  ( -0.000000000000000000, -0.3543493200069152138, 0.9351131265310292928 ) ) ;
#89290 = CARTESIAN_POINT ( 'NONE',  ( 32.00456980810188412, 6.871911579029510442, -3.967499999999998916 ) ) ;
#89291 = VECTOR ( 'NONE', #86356, 999.9999999999998863 ) ;
#89292 = DIRECTION ( 'NONE',  ( -0.7071067811865486830, -0.7071067811865464625, 0.000000000000000000 ) ) ;
#89293 = ORIENTED_EDGE ( 'NONE', *, *, #12891, .F. ) ;
#89294 = CARTESIAN_POINT ( 'NONE',  ( 114.3912635252314232, -4.472830434245839371, -4.472830434245839371 ) ) ;
#89296 = ADVANCED_FACE ( 'NONE', ( #77431 ), #63834, .T. ) ;
#89295 = VECTOR ( 'NONE', #49395, 1000.000000000000000 ) ;
#89297 = CARTESIAN_POINT ( 'NONE',  ( 34.92499999999998295, 6.006123077391907650, 4.000000000000000000 ) ) ;
#89298 = CARTESIAN_POINT ( 'NONE',  ( -34.42500000000001137, -7.458600742197909916, 5.000000000000000000 ) ) ;
#89299 = DIRECTION ( 'NONE',  ( 0.000000000000000000, 0.000000000000000000, -1.000000000000000000 ) ) ;
#89301 = VERTEX_POINT ( 'NONE', #11376 ) ;
#89300 = CARTESIAN_POINT ( 'NONE',  ( -17.99999999999987566, 16.55218569542899587, 5.000000000000000000 ) ) ;
#89302 = DIRECTION ( 'NONE',  ( -0.7071067811865487940, 0.7071067811865463515, 0.000000000000000000 ) ) ;
#89303 = ORIENTED_EDGE ( 'NONE', *, *, #52650, .T. ) ;
#89304 = VECTOR ( 'NONE', #49782, 1000.000000000000000 ) ;
#89305 = CARTESIAN_POINT ( 'NONE',  ( -24.18398860626899705, 28.73617430169804265, 5.000000000000000000 ) ) ;
#89306 = CARTESIAN_POINT ( 'NONE',  ( 122.6835989386367771, -43.14999999999999147, -34.92499999999998295 ) ) ;
#89307 = CARTESIAN_POINT ( 'NONE',  ( 120.0000000000000000, 0.000000000000000000, -7.950000000000000178 ) ) ;
#89308 = EDGE_CURVE ( 'NONE', #125463, #126916, #46226, .T. ) ;
#89309 = ORIENTED_EDGE ( 'NONE', *, *, #35952, .T. ) ;
#89310 = LINE ( 'NONE', #58882, #57519 ) ;
#89311 = DIRECTION ( 'NONE',  ( -0.000000000000000000, 0.000000000000000000, 1.000000000000000000 ) ) ;
#89312 = LINE ( 'NONE', #133537, #2690 ) ;
#89313 = ORIENTED_EDGE ( 'NONE', *, *, #47739, .F. ) ;
#89314 = CARTESIAN_POINT ( 'NONE',  ( -30.32816939922331301, -6.740707523384216415, 4.000000000000000000 ) ) ;
#89315 = EDGE_LOOP ( 'NONE', ( #122948, #136625, #132576, #62727 ) ) ;
#89316 = CARTESIAN_POINT ( 'NONE',  ( -36.48921356237310221, -27.52281430457080802, 5.000000000000000000 ) ) ;
#89318 = VERTEX_POINT ( 'NONE', #99112 ) ;
#89317 = FACE_OUTER_BOUND ( 'NONE', #121418, .T. ) ;
#89319 = ORIENTED_EDGE ( 'NONE', *, *, #12683, .T. ) ;
#89320 = CARTESIAN_POINT ( 'NONE',  ( 12.14969952407321507, 10.07123342099957064, -26.87533215267990983 ) ) ;
#89321 = LINE ( 'NONE', #23327, #32064 ) ;
#89322 = VERTEX_POINT ( 'NONE', #12827 ) ;
#89323 = LINE ( 'NONE', #49236, #6568 ) ;
#89324 = ADVANCED_FACE ( 'NONE', ( #122298 ), #143356, .F. ) ;
#89325 = DIRECTION ( 'NONE',  ( 1.000000000000000000, 3.115803279706882722E-16, 0.000000000000000000 ) ) ;
#89326 = CARTESIAN_POINT ( 'NONE',  ( 60.48921356237309510, -27.52281430457097500, 5.000000000000000000 ) ) ;
#89327 = VERTEX_POINT ( 'NONE', #100587 ) ;
#89328 = EDGE_CURVE ( 'NONE', #10041, #30236, #45513, .T. ) ;
#89329 = CARTESIAN_POINT ( 'NONE',  ( -4.099200028784281358, 22.22500000000000142, 16.68104793800802810 ) ) ;
#89330 = CARTESIAN_POINT ( 'NONE',  ( 12.48921356237309155, -27.52281430457064104, 5.000000000000000000 ) ) ;
#89331 = CARTESIAN_POINT ( 'NONE',  ( 27.18398860626900060, 28.73617430169806042, 5.000000000000000000 ) ) ;
#89332 = CARTESIAN_POINT ( 'NONE',  ( 126.0872339960914275, -6.972148538754269431, 2.385612954137347419 ) ) ;
#89333 = CARTESIAN_POINT ( 'NONE',  ( 30.53709685856477307, -3.054999999999999272, -5.291415217122919401 ) ) ;
#89334 = LINE ( 'NONE', #99465, #92796 ) ;
#89335 = EDGE_CURVE ( 'NONE', #23231, #139660, #3372, .T. ) ;
#89336 = EDGE_CURVE ( 'NONE', #48400, #14811, #138204, .T. ) ;
#89337 = ORIENTED_EDGE ( 'NONE', *, *, #65602, .T. ) ;
#89338 = ORIENTED_EDGE ( 'NONE', *, *, #49382, .T. ) ;
#89339 = CARTESIAN_POINT ( 'NONE',  ( 153.4000000000000057, 25.96999999999993847, 34.92499999999998295 ) ) ;
#89340 = ORIENTED_EDGE ( 'NONE', *, *, #86582, .F. ) ;
#89341 = ORIENTED_EDGE ( 'NONE', *, *, #91168, .F. ) ;
#89342 = CARTESIAN_POINT ( 'NONE',  ( 1.292751919595855004, -3.287470007381915860, -5.962884502238249951 ) ) ;
#89343 = DIRECTION ( 'NONE',  ( 0.3543493200069162685, -0.000000000000000000, -0.9351131265310288487 ) ) ;
#89344 = VERTEX_POINT ( 'NONE', #48337 ) ;
#89345 = CARTESIAN_POINT ( 'NONE',  ( -5.510786437626906675, -27.52281430457051314, 5.000000000000000000 ) ) ;
#89346 = CYLINDRICAL_SURFACE ( 'NONE', #62891, 2.500000000000000000 ) ;
#89347 = DIRECTION ( 'NONE',  ( -0.7071067811865486830, -0.7071067811865464625, 0.000000000000000000 ) ) ;
#89348 = EDGE_CURVE ( 'NONE', #133793, #116472, #92527, .T. ) ;
#89349 = CARTESIAN_POINT ( 'NONE',  ( -31.82816939922330945, 12.75929247661558641, 4.000000000000000000 ) ) ;
#89350 = CARTESIAN_POINT ( 'NONE',  ( 126.0004301918981042, -3.055000000000002380, 5.291415217122920289 ) ) ;
#89351 = ORIENTED_EDGE ( 'NONE', *, *, #130205, .T. ) ;
#89352 = EDGE_CURVE ( 'NONE', #107639, #66777, #47666, .T. ) ;
#89353 = DIRECTION ( 'NONE',  ( 0.7071067811865487940, 0.7071067811865463515, 0.000000000000000000 ) ) ;
#89354 = PRESENTATION_STYLE_ASSIGNMENT (( #100935 ) ) ;
#89355 = CARTESIAN_POINT ( 'NONE',  ( -23.29289321881329045, -3.740707523384244837, 5.000000000000000000 ) ) ;
#89356 = CARTESIAN_POINT ( 'NONE',  ( 0.5043781857168800897, 7.083145261826254035, -2.736640815332766596 ) ) ;
#89357 = LINE ( 'NONE', #108938, #24182 ) ;
#89358 = CARTESIAN_POINT ( 'NONE',  ( 5.999999999999958256, 7.552185695429089130, 5.000000000000000000 ) ) ;
#89359 = PLANE ( 'NONE',  #43421 ) ;
#89360 = CARTESIAN_POINT ( 'NONE',  ( 45.43336038379622011, 2.130196079827431532, -7.949999999999997513 ) ) ;
#89361 = AXIS2_PLACEMENT_3D ( 'NONE', #103627, #28242, #127546 ) ;
#89362 = CARTESIAN_POINT ( 'NONE',  ( 28.49999999999981171, 3.073033219394654569, -6.593910359670904775 ) ) ;
#89363 = DIRECTION ( 'NONE',  ( 0.7071067811865487940, 0.7071067811865463515, 0.000000000000000000 ) ) ;
#89364 = ORIENTED_EDGE ( 'NONE', *, *, #70184, .T. ) ;
#89365 = VERTEX_POINT ( 'NONE', #25135 ) ;
#89366 = CARTESIAN_POINT ( 'NONE',  ( 42.56249999999998579, -5.819803920172572198, -5.819803920172573086 ) ) ;
#89367 = EDGE_CURVE ( 'NONE', #104733, #89868, #75035, .T. ) ;
#89368 = VECTOR ( 'NONE', #19500, 1000.000000000000227 ) ;
#89369 = PLANE ( 'NONE',  #99417 ) ;
#89370 = FACE_OUTER_BOUND ( 'NONE', #130193, .T. ) ;
#89371 = ORIENTED_EDGE ( 'NONE', *, *, #62878, .T. ) ;
#89372 = EDGE_CURVE ( 'NONE', #93963, #70973, #136053, .T. ) ;
#89373 = FACE_OUTER_BOUND ( 'NONE', #36422, .T. ) ;
#89374 =( BOUNDED_SURFACE ( )  B_SPLINE_SURFACE ( 3, 2, ( 
 ( #88889, #1802, #23604 ),
 ( #34488, #22855, #56286 ),
 ( #135253, #78705, #91711 ),
 ( #33794, #100465, #122925 ),
 ( #402, #78005, #122184 ),
 ( #46102, #68568, #67121 ),
 ( #90277, #134530, #35229 ),
 ( #24322, #112754, #57696 ),
 ( #124348, #2537, #46846 ),
 ( #91033, #35942, #80160 ),
 ( #113451, #58434, #102613 ),
 ( #3263, #47555, #61287 ) ),
 .UNSPECIFIED., .F., .F., .F. ) 
 B_SPLINE_SURFACE_WITH_KNOTS ( ( 4, 2, 2, 2, 2, 4 ),
 ( 3, 3 ),
 ( 0.000000000000000000, 0.0009975800291739328821, 0.001995160058347865764, 0.002493950072934832205, 0.002992740087521798646, 0.003990320116695731528 ),
 ( 0.000000000000000000, 1.000000000000000000 ),
 .UNSPECIFIED. ) 
 GEOMETRIC_REPRESENTATION_ITEM ( )  RATIONAL_B_SPLINE_SURFACE ( (
 ( 1.000000000000000000, 0.7825691453495835503, 1.000000000000000000),
 ( 1.000000000000000000, 0.7825473240981194456, 1.000000000000000000),
 ( 1.000000000000000000, 0.7821547027292599097, 1.000000000000000000),
 ( 1.000000000000000000, 0.7799370077755589659, 1.000000000000000000),
 ( 1.000000000000000000, 0.7781753367904327146, 1.000000000000000000),
 ( 1.000000000000000000, 0.7735157641301041442, 1.000000000000000000),
 ( 1.000000000000000000, 0.7716557628207030284, 1.000000000000000000),
 ( 1.000000000000000000, 0.7671421219664820157, 1.000000000000000000),
 ( 1.000000000000000000, 0.7644786082298313801, 1.000000000000000000),
 ( 1.000000000000000000, 0.7550095275972034115, 1.000000000000000000),
 ( 1.000000000000000000, 0.7469941267412624208, 1.000000000000000000),
 ( 1.000000000000000000, 0.7366656399173064917, 1.000000000000000000) ) ) 
 REPRESENTATION_ITEM ( '' )  SURFACE ( )  );
#89375 = CARTESIAN_POINT ( 'NONE',  ( -10.49999999999992539, -12.66682484999667579, -0.6294897503864175237 ) ) ;
#89376 = CARTESIAN_POINT ( 'NONE',  ( 36.31293019189809002, -1.637169565754159617, -6.110000000000001208 ) ) ;
#89378 = ORIENTED_EDGE ( 'NONE', *, *, #126686, .T. ) ;
#89377 = VECTOR ( 'NONE', #102561, 1000.000000000000227 ) ;
#89379 = EDGE_LOOP ( 'NONE', ( #70441, #36795, #137536, #87107 ) ) ;
#89380 = ORIENTED_EDGE ( 'NONE', *, *, #2751, .T. ) ;
#89381 = ADVANCED_FACE ( 'NONE', ( #125183 ), #135372, .F. ) ;
#89382 = CARTESIAN_POINT ( 'NONE',  ( 0.000000000000000000, 0.000000000000000000, 7.950000000000000178 ) ) ;
#89383 = LINE ( 'NONE', #92217, #61594 ) ;
#89384 = DIRECTION ( 'NONE',  ( -0.6830127018922180770, 0.6830127018922202975, -0.2588190451025213501 ) ) ;
#89385 = ORIENTED_EDGE ( 'NONE', *, *, #91957, .T. ) ;
#89386 = LINE ( 'NONE', #57497, #97436 ) ;
#89387 = ORIENTED_EDGE ( 'NONE', *, *, #140379, .T. ) ;
#89388 = CARTESIAN_POINT ( 'NONE',  ( 19.41972383043609440, -2.500000000000000000, 3.061616997868383634E-16 ) ) ;
#89389 = DIRECTION ( 'NONE',  ( -0.6830127018922181881, 0.6830127018922202975, -0.2588190451025214056 ) ) ;
#89390 = CARTESIAN_POINT ( 'NONE',  ( -34.47516574401891631, -20.97193265888396496, 4.998110765256836174 ) ) ;
#89391 = ADVANCED_FACE ( 'NONE', ( #16388 ), #93970, .F. ) ;
#89392 = CARTESIAN_POINT ( 'NONE',  ( 27.18398860626900060, 28.73617430169806042, 5.000000000000000000 ) ) ;
#89393 = DIRECTION ( 'NONE',  ( 0.7071067811865487940, -0.7071067811865463515, 0.000000000000000000 ) ) ;
#89394 = VECTOR ( 'NONE', #31449, 1000.000000000000000 ) ;
#89395 = EDGE_CURVE ( 'NONE', #139596, #137134, #38891, .T. ) ;
#89396 = VECTOR ( 'NONE', #113427, 1000.000000000000000 ) ;
#89397 = VERTEX_POINT ( 'NONE', #102726 ) ;
#89398 = CARTESIAN_POINT ( 'NONE',  ( 10.94186803553636977, 0.000000000000000000, 2.500000000000000444 ) ) ;
#89399 = CARTESIAN_POINT ( 'NONE',  ( 53.72459685856478018, -1.637169565754160949, 6.109999999999997655 ) ) ;
#89400 = VECTOR ( 'NONE', #97167, 999.9999999999998863 ) ;
#89401 = CARTESIAN_POINT ( 'NONE',  ( 8.031592354503320763, 9.902892378096218942E-16, 0.000000000000000000 ) ) ;
#89402 = CARTESIAN_POINT ( 'NONE',  ( 13.49999999999991473, -2.947814304570798960, 5.000000000000000000 ) ) ;
#89403 = DIRECTION ( 'NONE',  ( -0.000000000000000000, 0.000000000000000000, 1.000000000000000000 ) ) ;
#89404 = ORIENTED_EDGE ( 'NONE', *, *, #85374, .F. ) ;
#89405 = TOROIDAL_SURFACE ( 'NONE', #80127, 6.000000000000000000, 3.000000000000000000 ) ;
#89406 = CYLINDRICAL_SURFACE ( 'NONE', #51653, 0.5000000000000004441 ) ;
#89408 = EDGE_CURVE ( 'NONE', #26300, #15282, #70827, .T. ) ;
#89407 = SHAPE_REPRESENTATION_RELATIONSHIP ( 'NONE' , 'NONE' ,  #40289, #18911 ) ;
#89409 = EDGE_LOOP ( 'NONE', ( #95684, #47267, #15411, #94594 ) ) ;
#89410 = CARTESIAN_POINT ( 'NONE',  ( -14.51078643762690490, -27.52281430457045275, 5.000000000000000000 ) ) ;
#89411 = ORIENTED_EDGE ( 'NONE', *, *, #121883, .T. ) ;
#89412 = CARTESIAN_POINT ( 'NONE',  ( -2.207106781186520372, -17.24070752338410628, 5.000000000000000000 ) ) ;
#89413 = LINE ( 'NONE', #217, #119672 ) ;
#89414 = CARTESIAN_POINT ( 'NONE',  ( 33.65494483745361265, 5.259292476615669010, 12.77922209995901603 ) ) ;
#89415 = FACE_BOUND ( 'NONE', #55646, .T. ) ;
#89416 = PLANE ( 'NONE',  #68900 ) ;
#89417 = DIRECTION ( 'NONE',  ( 0.000000000000000000, 0.000000000000000000, 1.000000000000000000 ) ) ;
#89418 = DIRECTION ( 'NONE',  ( -0.7071067811865486830, -0.7071067811865464625, -0.000000000000000000 ) ) ;
#89420 = ORIENTED_EDGE ( 'NONE', *, *, #83646, .F. ) ;
#89419 = CARTESIAN_POINT ( 'NONE',  ( -24.29974487139158867, -27.71228299555223273, 4.000000000000000000 ) ) ;
#89421 = DIRECTION ( 'NONE',  ( -0.6830127018922180770, -0.6830127018922204085, -0.2588190451025213501 ) ) ;
#89422 = ORIENTED_EDGE ( 'NONE', *, *, #69846, .F. ) ;
#89423 = ORIENTED_EDGE ( 'NONE', *, *, #124796, .F. ) ;
#89424 = CARTESIAN_POINT ( 'NONE',  ( 71.51626352523145158, -4.472830434245838482, 4.472830434245838482 ) ) ;
#89425 = ORIENTED_EDGE ( 'NONE', *, *, #27016, .T. ) ;
#89426 = FACE_OUTER_BOUND ( 'NONE', #85076, .T. ) ;
#89427 = EDGE_CURVE ( 'NONE', #102663, #2265, #137498, .T. ) ;
#89428 = ORIENTED_EDGE ( 'NONE', *, *, #107825, .T. ) ;
#89429 = FACE_OUTER_BOUND ( 'NONE', #20289, .T. ) ;
#89430 = VECTOR ( 'NONE', #104872, 1000.000000000000000 ) ;
#89431 = LINE ( 'NONE', #91580, #42652 ) ;
#89432 = CARTESIAN_POINT ( 'NONE',  ( 3.618384906019942004, -2.240707523384257716, 13.37739548510238485 ) ) ;
#89433 = FACE_OUTER_BOUND ( 'NONE', #84951, .T. ) ;
#89434 = DIRECTION ( 'NONE',  ( -0.000000000000000000, 0.000000000000000000, 1.000000000000000000 ) ) ;
#89435 = DIRECTION ( 'NONE',  ( -0.6830127018922180770, -0.6830127018922204085, -0.2588190451025213501 ) ) ;
#89436 = CARTESIAN_POINT ( 'NONE',  ( -21.79289321881330821, -17.24070752338410628, 5.000000000000000000 ) ) ;
#89437 = CARTESIAN_POINT ( 'NONE',  ( 7.600000000000009415, 0.000000000000000000, 0.000000000000000000 ) ) ;
#89438 = VERTEX_POINT ( 'NONE', #83112 ) ;
#89439 = VECTOR ( 'NONE', #49618, 1000.000000000000000 ) ;
#89440 = EDGE_LOOP ( 'NONE', ( #66862, #9907, #26, #82356 ) ) ;
#89441 = CARTESIAN_POINT ( 'NONE',  ( 27.29974487139158512, -27.71228299555225405, 4.000000000000000000 ) ) ;
#89442 = VERTEX_POINT ( 'NONE', #103403 ) ;
#89443 = ORIENTED_EDGE ( 'NONE', *, *, #46847, .F. ) ;
#89444 = ORIENTED_EDGE ( 'NONE', *, *, #29895, .F. ) ;
#89445 = EDGE_CURVE ( 'NONE', #106219, #21922, #60689, .T. ) ;
#89446 = EDGE_CURVE ( 'NONE', #37203, #69267, #88974, .T. ) ;
#89447 = CARTESIAN_POINT ( 'NONE',  ( 28.87543019189810067, -5.291415217122920289, -3.055000000000001492 ) ) ;
#89448 = ORIENTED_EDGE ( 'NONE', *, *, #79983, .T. ) ;
#89449 = CARTESIAN_POINT ( 'NONE',  ( 44.75000000000000000, -9.735942053221458872E-16, 7.950000000000000178 ) ) ;
#89450 = ADVANCED_FACE ( 'NONE', ( #4051 ), #114972, .F. ) ;
#89451 = STYLED_ITEM ( 'NONE', ( #112094 ), #106085 ) ;
#89452 = FILL_AREA_STYLE_COLOUR ( '', #56290 ) ;
#89453 = CARTESIAN_POINT ( 'NONE',  ( 32.56663961620377989, 1.633150327867695095, 6.094999999999988205 ) ) ;
#89454 = CARTESIAN_POINT ( 'NONE',  ( 14.64989824621740233, 4.671147552932954916, -29.50326184817846098 ) ) ;
#89455 = ORIENTED_EDGE ( 'NONE', *, *, #8996, .F. ) ;
#89456 = VECTOR ( 'NONE', #143254, 1000.000000000000000 ) ;
#89457 = EDGE_CURVE ( 'NONE', #30341, #27902, #36054, .T. ) ;
#89458 = FACE_OUTER_BOUND ( 'NONE', #20624, .T. ) ;
#89459 = PLANE ( 'NONE',  #55750 ) ;
#89460 = DIRECTION ( 'NONE',  ( -0.7071067811865486830, -0.7071067811865464625, -0.000000000000000000 ) ) ;
#89462 = ORIENTED_EDGE ( 'NONE', *, *, #119579, .F. ) ;
#89461 = CARTESIAN_POINT ( 'NONE',  ( -29.99451991528749417, 28.92564299267958816, 4.000000000000000000 ) ) ;
#89463 = ORIENTED_EDGE ( 'NONE', *, *, #105710, .T. ) ;
#89464 = DIRECTION ( 'NONE',  ( 0.7071067811865487940, 0.7071067811865463515, 0.000000000000000000 ) ) ;
#89465 = CARTESIAN_POINT ( 'NONE',  ( 0.000000000000000000, 21.72500000000000142, 4.500000000000000888 ) ) ;
#89466 = CARTESIAN_POINT ( 'NONE',  ( 0.000000000000000000, 0.000000000000000000, 5.000000000000000000 ) ) ;
#89467 = EDGE_CURVE ( 'NONE', #137446, #100841, #124467, .T. ) ;
#89468 = ORIENTED_EDGE ( 'NONE', *, *, #140510, .F. ) ;
#89469 = CARTESIAN_POINT ( 'NONE',  ( -14.99999999999989342, -18.41253812416056945, 4.000000000000000000 ) ) ;
#89470 = DIRECTION ( 'NONE',  ( -0.6830127018922180770, -0.6830127018922204085, -0.2588190451025213501 ) ) ;
#89471 = VERTEX_POINT ( 'NONE', #115686 ) ;
#89472 = VECTOR ( 'NONE', #56315, 1000.000000000000000 ) ;
#89473 = SURFACE_STYLE_FILL_AREA ( #133709 ) ;
#89474 = DIRECTION ( 'NONE',  ( -0.7071067811865486830, -0.7071067811865464625, 0.000000000000000000 ) ) ;
#89475 = EDGE_CURVE ( 'NONE', #133992, #62201, #5517, .T. ) ;
#89476 = CARTESIAN_POINT ( 'NONE',  ( 14.29387692260793763, 22.22500000000000142, 4.000000000000000000 ) ) ;
#89477 = CARTESIAN_POINT ( 'NONE',  ( 3.087196949643289834, 3.821174125832445049E-16, 0.000000000000000000 ) ) ;
#89478 = CARTESIAN_POINT ( 'NONE',  ( 0.000000000000000000, 0.000000000000000000, 5.000000000000000000 ) ) ;
#89479 = CARTESIAN_POINT ( 'NONE',  ( 42.29974487139158157, -27.71228299555235708, 4.000000000000000000 ) ) ;
#89480 = AXIS2_PLACEMENT_3D ( 'NONE', #125785, #26460, #138076 ) ;
#89481 = LINE ( 'NONE', #17610, #52983 ) ;
#89482 = ORIENTED_EDGE ( 'NONE', *, *, #82385, .T. ) ;
#89483 = ORIENTED_EDGE ( 'NONE', *, *, #2950, .T. ) ;
#89484 = EDGE_CURVE ( 'NONE', #111064, #82851, #113952, .T. ) ;
#89485 = DIRECTION ( 'NONE',  ( 1.000000000000000000, 3.115803279706882722E-16, -0.000000000000000000 ) ) ;
#89486 = CIRCLE ( 'NONE', #66431, 2.500000000000000888 ) ;
#89487 = AXIS2_PLACEMENT_3D ( 'NONE', #3771, #103809, #46668 ) ;
#89488 =( NAMED_UNIT ( * ) SI_UNIT ( $, .STERADIAN. ) SOLID_ANGLE_UNIT ( ) );
#89489 = PLANE ( 'NONE',  #76059 ) ;
#89490 = VECTOR ( 'NONE', #32715, 1000.000000000000000 ) ;
#89491 = VERTEX_POINT ( 'NONE', #39630 ) ;
#89492 = LINE ( 'NONE', #123592, #110955 ) ;
#89493 = PLANE ( 'NONE',  #99702 ) ;
#89494 = DIRECTION ( 'NONE',  ( 0.000000000000000000, -1.000000000000000000, 0.000000000000000000 ) ) ;
#89495 = ORIENTED_EDGE ( 'NONE', *, *, #136290, .T. ) ;
#89496 = EDGE_CURVE ( 'NONE', #106121, #26065, #138929, .T. ) ;
#89497 = SURFACE_STYLE_USAGE ( .BOTH. , #124981 ) ;
#89498 = CARTESIAN_POINT ( 'NONE',  ( 29.99999999999980105, 2.587461875839216496, 4.000000000000000000 ) ) ;
#89499 = UNCERTAINTY_MEASURE_WITH_UNIT (LENGTH_MEASURE( 1.000000000000000082E-05 ), #92601, 'distance_accuracy_value', 'NONE');
#89500 = LINE ( 'NONE', #122848, #104782 ) ;
#89501 = AXIS2_PLACEMENT_3D ( 'NONE', #74568, #107860, #38361 ) ;
#89502 = CARTESIAN_POINT ( 'NONE',  ( 18.29974487139159223, -27.71228299555219010, 4.000000000000000000 ) ) ;
#89503 = CARTESIAN_POINT ( 'NONE',  ( 54.16209685856478018, -5.291415217122919401, 3.054999999999998384 ) ) ;
#89504 = LINE ( 'NONE', #68502, #65002 ) ;
#89505 = EDGE_CURVE ( 'NONE', #66379, #142228, #9060, .T. ) ;
#89506 = EDGE_CURVE ( 'NONE', #20442, #67467, #52610, .T. ) ;
#89507 = LINE ( 'NONE', #88817, #101715 ) ;
#89508 = CYLINDRICAL_SURFACE ( 'NONE', #139098, 5.999999999999998224 ) ;
#89509 = CARTESIAN_POINT ( 'NONE',  ( -23.39513766812465079, 21.75929247661549937, 21.32995629748191746 ) ) ;
#89510 = ORIENTED_EDGE ( 'NONE', *, *, #143533, .T. ) ;
#89511 = DIRECTION ( 'NONE',  ( 0.000000000000000000, 1.000000000000000000, 0.000000000000000000 ) ) ;
#89512 = ORIENTED_EDGE ( 'NONE', *, *, #53213, .F. ) ;
#89513 = LINE ( 'NONE', #92342, #107925 ) ;
#89514 = EDGE_CURVE ( 'NONE', #105535, #14052, #73665, .T. ) ;
#89515 = CARTESIAN_POINT ( 'NONE',  ( -11.99999999999991296, -13.97847968911261418, -0.1324546996127068943 ) ) ;
#89516 = DIRECTION ( 'NONE',  ( -0.7071067811865486830, 0.7071067811865464625, 0.000000000000000000 ) ) ;
#89517 = CARTESIAN_POINT ( 'NONE',  ( 3.250000000000000000, 0.000000000000000000, 0.000000000000000000 ) ) ;
#89518 = EDGE_CURVE ( 'NONE', #42670, #90134, #140342, .T. ) ;
#89519 = DIRECTION ( 'NONE',  ( 0.7071067811865486830, -0.7071067811865464625, -0.000000000000000000 ) ) ;
#89520 = CARTESIAN_POINT ( 'NONE',  ( -5.510786437626906675, -27.52281430457051314, 5.000000000000000000 ) ) ;
#89521 = EDGE_LOOP ( 'NONE', ( #125991, #129374, #68469, #75939 ) ) ;
#89522 = VERTEX_POINT ( 'NONE', #63535 ) ;
#89523 = CARTESIAN_POINT ( 'NONE',  ( -25.49999999999982592, -4.796895815301041033, -3.611700055028741918 ) ) ;
#89524 = FACE_OUTER_BOUND ( 'NONE', #59720, .T. ) ;
#89525 = UNCERTAINTY_MEASURE_WITH_UNIT (LENGTH_MEASURE( 1.000000000000000082E-05 ), #61011, 'distance_accuracy_value', 'NONE');
#89526 = DIRECTION ( 'NONE',  ( 0.000000000000000000, 0.000000000000000000, 1.000000000000000000 ) ) ;
#89527 = CARTESIAN_POINT ( 'NONE',  ( -0.7070132642930445632, -21.74070752338405654, 4.999753212805222446 ) ) ;
#89528 = CARTESIAN_POINT ( 'NONE',  ( 78.82919371712957002, -3.975000000000001865, 6.884901960086284411 ) ) ;
#89529 = CARTESIAN_POINT ( 'NONE',  ( -34.49999999999975842, -10.53574439159939757, 4.994342998332166772 ) ) ;
#89530 = DIRECTION ( 'NONE',  ( 1.000000000000000000, 0.000000000000000000, 0.000000000000000000 ) ) ;
#89531 = EDGE_LOOP ( 'NONE', ( #136594, #30217, #22512, #98392, #90777, #77587 ) ) ;
#89532 = CARTESIAN_POINT ( 'NONE',  ( 78.14583333333332860, 2.130196079827431976, -7.949999999999999289 ) ) ;
#89533 = EDGE_CURVE ( 'NONE', #13228, #49400, #62808, .T. ) ;
#89534 = CARTESIAN_POINT ( 'NONE',  ( 66.18398860626901126, 28.73617430169833753, 5.000000000000000000 ) ) ;
#89535 = DIRECTION ( 'NONE',  ( 0.7071067811865487940, 0.7071067811865463515, 0.000000000000000000 ) ) ;
#89536 = CARTESIAN_POINT ( 'NONE',  ( 24.18398860626899705, 28.73617430169804265, 5.000000000000000000 ) ) ;
#89537 = ORIENTED_EDGE ( 'NONE', *, *, #18195, .F. ) ;
#89538 = EDGE_CURVE ( 'NONE', #88631, #117097, #108381, .T. ) ;
#89539 = CARTESIAN_POINT ( 'NONE',  ( -1.171830600776462061, 9.759292476615621936, 4.000000000000000000 ) ) ;
#89540 = CARTESIAN_POINT ( 'NONE',  ( -18.00548008471250583, 28.92564299267925776, 4.000000000000000000 ) ) ;
#89541 = CARTESIAN_POINT ( 'NONE',  ( 64.75043019189810423, 3.055000000000002824, -5.291415217122919401 ) ) ;
#89542 = VECTOR ( 'NONE', #142318, 1000.000000000000000 ) ;
#89543 = ORIENTED_EDGE ( 'NONE', *, *, #89467, .F. ) ;
#89544 = ORIENTED_EDGE ( 'NONE', *, *, #36190, .F. ) ;
#89545 = DIRECTION ( 'NONE',  ( -0.7071067811865486830, -0.7071067811865464625, 0.000000000000000000 ) ) ;
#89546 = CYLINDRICAL_SURFACE ( 'NONE', #77713, 0.5000000000000004441 ) ;
#89547 = CARTESIAN_POINT ( 'NONE',  ( 4.969723521325230209, -2.055000000000000160, 2.789133085058097101E-16 ) ) ;
#89548 = AXIS2_PLACEMENT_3D ( 'NONE', #110785, #42011, #87638 ) ;
#89549 = CARTESIAN_POINT ( 'NONE',  ( -14.99999999999990230, -4.068876922607767455, 4.000000000000000000 ) ) ;
#89550 = LINE ( 'NONE', #78683, #58190 ) ;
#89552 = ORIENTED_EDGE ( 'NONE', *, *, #71048, .T. ) ;
#89551 = DIRECTION ( 'NONE',  ( -0.000000000000000000, 0.3543493200069153248, 0.9351131265310292928 ) ) ;
#89553 = CARTESIAN_POINT ( 'NONE',  ( -47.99451991528749062, 28.92564299267971251, 4.000000000000000000 ) ) ;
#89554 = DIRECTION ( 'NONE',  ( 0.000000000000000000, -1.000000000000000000, 0.000000000000000000 ) ) ;
#89555 = LINE ( 'NONE', #114163, #132824 ) ;
#89556 = LINE ( 'NONE', #10550, #76233 ) ;
#89557 = EDGE_LOOP ( 'NONE', ( #6872, #34287, #76984, #70126 ) ) ;
#89558 =( GEOMETRIC_REPRESENTATION_CONTEXT ( 3 ) GLOBAL_UNCERTAINTY_ASSIGNED_CONTEXT ( ( #33050 ) ) GLOBAL_UNIT_ASSIGNED_CONTEXT ( ( #33490, #121166, #35637 ) ) REPRESENTATION_CONTEXT ( 'NONE', 'WORKASPACE' ) );
#89559 = ADVANCED_FACE ( 'NONE', ( #74393 ), #106987, .T. ) ;
#89560 = VERTEX_POINT ( 'NONE', #85233 ) ;
#89561 = CARTESIAN_POINT ( 'NONE',  ( 54.54209685856477563, 5.291415217122923842, -3.054999999999996163 ) ) ;
#89562 = ORIENTED_EDGE ( 'NONE', *, *, #80076, .T. ) ;
#89563 = VECTOR ( 'NONE', #141670, 1000.000000000000227 ) ;
#89564 = DIRECTION ( 'NONE',  ( 0.000000000000000000, 0.000000000000000000, 1.000000000000000000 ) ) ;
#89565 = FACE_OUTER_BOUND ( 'NONE', #86372, .T. ) ;
#89566 = CARTESIAN_POINT ( 'NONE',  ( 4.969723521325230209, 4.202752102959690472E-16, 0.000000000000000000 ) ) ;
#89567 = STYLED_ITEM ( 'NONE', ( #22631 ), #3731 ) ;
#89568 = CARTESIAN_POINT ( 'NONE',  ( -25.39999999999996305, 0.000000000000000000, 0.000000000000000000 ) ) ;
#89569 = DIRECTION ( 'NONE',  ( 0.7071067811865486830, -0.7071067811865464625, -0.000000000000000000 ) ) ;
#89570 = ORIENTED_EDGE ( 'NONE', *, *, #46870, .T. ) ;
#89571 = VERTEX_POINT ( 'NONE', #31590 ) ;
#89572 = LINE ( 'NONE', #133802, #111674 ) ;
#89573 = ORIENTED_EDGE ( 'NONE', *, *, #112693, .T. ) ;
#89574 = DIRECTION ( 'NONE',  ( -0.3543493200069162685, -0.000000000000000000, -0.9351131265310288487 ) ) ;
#89575 = CARTESIAN_POINT ( 'NONE',  ( -9.707106781186466193, -18.74070752338409207, 5.000000000000000000 ) ) ;
#89576 = CARTESIAN_POINT ( 'NONE',  ( 34.92499999999998295, 22.22500000000000142, 4.500000000000000888 ) ) ;
#89577 = VERTEX_POINT ( 'NONE', #18526 ) ;
#89578 = VECTOR ( 'NONE', #92597, 1000.000000000000000 ) ;
#89579 = FACE_BOUND ( 'NONE', #73521, .T. ) ;
#89580 = DIRECTION ( 'NONE',  ( 0.000000000000000000, -5.559056632600921604E-15, 1.000000000000000000 ) ) ;
#89581 = LINE ( 'NONE', #90292, #90611 ) ;
#89582 = DIRECTION ( 'NONE',  ( 0.7071067811865487940, 0.7071067811865463515, 0.000000000000000000 ) ) ;
#89583 = DIRECTION ( 'NONE',  ( -0.000000000000000000, 1.000000000000000000, -0.000000000000000000 ) ) ;
#89584 = VECTOR ( 'NONE', #48217, 1000.000000000000227 ) ;
#89585 = VECTOR ( 'NONE', #122549, 1000.000000000000000 ) ;
#89586 = CARTESIAN_POINT ( 'NONE',  ( 2.139447441471317379, 4.584330080086930965E-16, 0.000000000000000000 ) ) ;
#89587 = DIRECTION ( 'NONE',  ( 1.000000000000000000, 2.039446610170337541E-32, -1.224646799147353207E-16 ) ) ;
#89588 = ORIENTED_EDGE ( 'NONE', *, *, #25642, .T. ) ;
#89589 = CIRCLE ( 'NONE', #117302, 2.500000000000000888 ) ;
#89590 = VERTEX_POINT ( 'NONE', #106250 ) ;
#89591 = CARTESIAN_POINT ( 'NONE',  ( 107.0995968585648086, -6.109999999999997655, -1.637169565754160283 ) ) ;
#89592 = ORIENTED_EDGE ( 'NONE', *, *, #56191, .T. ) ;
#89593 = DIRECTION ( 'NONE',  ( 0.7071067811865487940, 0.7071067811865463515, -0.000000000000000000 ) ) ;
#89594 = VERTEX_POINT ( 'NONE', #95402 ) ;
#89595 = VECTOR ( 'NONE', #96991, 1000.000000000000227 ) ;
#89596 = CONICAL_SURFACE ( 'NONE', #84952, 2.055000000000001048, 0.9599310885968758145 ) ;
#89597 = DIRECTION ( 'NONE',  ( -0.6830127018922181881, 0.6830127018922202975, -0.2588190451025214056 ) ) ;
#89598 = CARTESIAN_POINT ( 'NONE',  ( 4.566639616203773677, 1.633150327867685103, 6.094999999999992646 ) ) ;
#89599 = FACE_OUTER_BOUND ( 'NONE', #29339, .T. ) ;
#89600 = EDGE_CURVE ( 'NONE', #29556, #14737, #75126, .T. ) ;
#89601 = EDGE_LOOP ( 'NONE', ( #121129, #95324, #82431, #105170 ) ) ;
#89602 = CARTESIAN_POINT ( 'NONE',  ( 34.42499999999998295, -18.02281430457042433, 5.000000000000000000 ) ) ;
#89603 = DIRECTION ( 'NONE',  ( 0.7071067811865487940, 0.7071067811865463515, -0.000000000000000000 ) ) ;
#89604 = DIRECTION ( 'NONE',  ( -0.000000000000000000, 0.000000000000000000, 1.000000000000000000 ) ) ;
#89605 = CARTESIAN_POINT ( 'NONE',  ( 25.39999999999999858, -43.14999999999999147, 40.92499999999998295 ) ) ;
#89606 = FACE_OUTER_BOUND ( 'NONE', #36917, .T. ) ;
#89607 = CARTESIAN_POINT ( 'NONE',  ( -0.09843580608236146556, 11.25929247661560240, 10.79108189686406938 ) ) ;
#89608 = LINE ( 'NONE', #125093, #7396 ) ;
#89609 = EDGE_LOOP ( 'NONE', ( #116751, #11645, #56469 ) ) ;
#89610 = CARTESIAN_POINT ( 'NONE',  ( 86.75000000000000000, -9.735942053221458872E-16, 7.950000000000000178 ) ) ;
#89611 = FACE_OUTER_BOUND ( 'NONE', #95819, .T. ) ;
#89612 = EDGE_CURVE ( 'NONE', #874, #31525, #51205, .T. ) ;
#89613 = ORIENTED_EDGE ( 'NONE', *, *, #129563, .T. ) ;
#89614 = VERTEX_POINT ( 'NONE', #129456 ) ;
#89615 = EDGE_CURVE ( 'NONE', #87976, #3063, #119979, .T. ) ;
#89616 = ADVANCED_FACE ( 'NONE', ( #30141 ), #41748, .F. ) ;
#89617 = EDGE_LOOP ( 'NONE', ( #142546, #7588, #130296, #21296 ) ) ;
#89618 = CARTESIAN_POINT ( 'NONE',  ( 51.91709685856476852, 3.054999999999998828, 5.291415217122922066 ) ) ;
#89619 = AXIS2_PLACEMENT_3D ( 'NONE', #123363, #68288, #34195 ) ;
#89620 = ORIENTED_EDGE ( 'NONE', *, *, #117723, .T. ) ;
#89621 = EDGE_CURVE ( 'NONE', #16679, #128612, #109133, .T. ) ;
#89622 = EDGE_CURVE ( 'NONE', #61284, #23063, #50487, .T. ) ;
#89623 = CARTESIAN_POINT ( 'NONE',  ( -34.49999999999975131, -16.53574439159933718, 4.994342998332169437 ) ) ;
#89624 = CONICAL_SURFACE ( 'NONE', #17781, 2.500000000000000888, 0.9599310885968822538 ) ;
#89625 = CARTESIAN_POINT ( 'NONE',  ( 8.504139616203772789, -3.047499999999994547, 5.278424836066145431 ) ) ;
#89626 = CARTESIAN_POINT ( 'NONE',  ( 90.12543019189811844, 5.291415217122919401, 3.055000000000002824 ) ) ;
#89627 = CARTESIAN_POINT ( 'NONE',  ( 14.99999999999990585, -3.033600742197708477, 5.000000000000000000 ) ) ;
#89628 = VERTEX_POINT ( 'NONE', #6923 ) ;
#89629 = EDGE_CURVE ( 'NONE', #137290, #131245, #29425, .T. ) ;
#89630 = VERTEX_POINT ( 'NONE', #90234 ) ;
#89631 = CARTESIAN_POINT ( 'NONE',  ( -2.999999999999975131, 13.93112307739204603, 4.000000000000000000 ) ) ;
#89632 =( GEOMETRIC_REPRESENTATION_CONTEXT ( 3 ) GLOBAL_UNCERTAINTY_ASSIGNED_CONTEXT ( ( #63850 ) ) GLOBAL_UNIT_ASSIGNED_CONTEXT ( ( #46762, #45311, #135170 ) ) REPRESENTATION_CONTEXT ( 'NONE', 'WORKASPACE' ) );
#89633 = CARTESIAN_POINT ( 'NONE',  ( -12.20000000000000284, -25.47159979880235881, 14.98806839329795260 ) ) ;
#89634 = ORIENTED_EDGE ( 'NONE', *, *, #86511, .F. ) ;
#89635 = CARTESIAN_POINT ( 'NONE',  ( 10.94186803553636977, 3.821174125832445049E-16, 0.000000000000000000 ) ) ;
#89636 = LINE ( 'NONE', #25802, #78459 ) ;
#89637 = DIRECTION ( 'NONE',  ( -0.000000000000000000, -0.3543493200069152693, 0.9351131265310292928 ) ) ;
#89638 = EDGE_CURVE ( 'NONE', #11133, #3647, #32309, .T. ) ;
#89639 = VERTEX_POINT ( 'NONE', #79422 ) ;
#89640 = FACE_OUTER_BOUND ( 'NONE', #138367, .T. ) ;
#89641 = ORIENTED_EDGE ( 'NONE', *, *, #12976, .T. ) ;
#89642 = EDGE_LOOP ( 'NONE', ( #6160, #58650 ) ) ;
#89643 = ORIENTED_EDGE ( 'NONE', *, *, #29268, .F. ) ;
#89645 = VECTOR ( 'NONE', #118017, 1000.000000000000227 ) ;
#89644 = CARTESIAN_POINT ( 'NONE',  ( -69.29974487139159578, -27.71228299555254537, 4.000000000000000000 ) ) ;
#89646 = DIRECTION ( 'NONE',  ( 0.7071067811865487940, 0.7071067811865463515, -0.000000000000000000 ) ) ;
#89647 = CIRCLE ( 'NONE', #55007, 1.000000000000000888 ) ;
#89648 = LINE ( 'NONE', #57060, #4641 ) ;
#89649 = CARTESIAN_POINT ( 'NONE',  ( -45.18398860626900415, 28.73617430169818832, 5.000000000000000000 ) ) ;
#89650 = EDGE_LOOP ( 'NONE', ( #85118, #100704, #95207, #6050 ) ) ;
#89651 = ADVANCED_FACE ( 'NONE', ( #22110 ), #12665, .T. ) ;
#89652 = CARTESIAN_POINT ( 'NONE',  ( 10.36246187583895306, 22.22500000000000142, 4.000000000000000000 ) ) ;
#89653 = CARTESIAN_POINT ( 'NONE',  ( 12.66623647476855297, 7.934999999999990727, -1.457635852685135314E-15 ) ) ;
#89654 = DIRECTION ( 'NONE',  ( 1.000000000000000000, 0.000000000000000000, -0.000000000000000000 ) ) ;
#89655 = CARTESIAN_POINT ( 'NONE',  ( -23.36654548503486950, 7.297668562427137573, 4.000000000000000000 ) ) ;
#89656 = COLOUR_RGB ( '', 0.66274510, 0.83137255, 0.94901961) ;
#89657 = DIRECTION ( 'NONE',  ( 1.000000000000000000, 0.000000000000000000, 0.000000000000000000 ) ) ;
#89658 = VERTEX_POINT ( 'NONE', #46054 ) ;
#89659 = ORIENTED_EDGE ( 'NONE', *, *, #14030, .F. ) ;
#89661 = VERTEX_POINT ( 'NONE', #99675 ) ;
#89660 = EDGE_CURVE ( 'NONE', #26438, #52182, #123619, .T. ) ;
#89662 = CARTESIAN_POINT ( 'NONE',  ( 19.39583333333333570, 1.633150327867706864, -6.094999999999981100 ) ) ;
#89663 = DIRECTION ( 'NONE',  ( -0.7071067811865486830, 0.7071067811865464625, 0.000000000000000000 ) ) ;
#89664 = UNCERTAINTY_MEASURE_WITH_UNIT (LENGTH_MEASURE( 1.000000000000000082E-05 ), #57436, 'distance_accuracy_value', 'NONE');
#89665 = DIRECTION ( 'NONE',  ( -0.7071067811865486830, -0.7071067811865464625, 0.000000000000000000 ) ) ;
#89666 = LINE ( 'NONE', #132507, #50571 ) ;
#89667 = CARTESIAN_POINT ( 'NONE',  ( 8.377306452199936970, 8.650827907999497413, -3.927822742214815754 ) ) ;
#89668 = EDGE_CURVE ( 'NONE', #117033, #45436, #55492, .T. ) ;
#89669 = CARTESIAN_POINT ( 'NONE',  ( 9.328169399223467551, 8.259292476615627265, 4.000000000000000000 ) ) ;
#89670 = CARTESIAN_POINT ( 'NONE',  ( 2.671830600776447628, -18.74070752338408852, 4.000000000000000000 ) ) ;
#89671 = DIRECTION ( 'NONE',  ( -0.7071067811865486830, 0.7071067811865464625, 0.000000000000000000 ) ) ;
#89672 = DIRECTION ( 'NONE',  ( 0.000000000000000000, -1.000000000000000000, 0.000000000000000000 ) ) ;
#89673 = EDGE_CURVE ( 'NONE', #72349, #91883, #19610, .T. ) ;
#89674 = VERTEX_POINT ( 'NONE', #43897 ) ;
#89675 = FACE_OUTER_BOUND ( 'NONE', #67557, .T. ) ;
#89676 = ORIENTED_EDGE ( 'NONE', *, *, #110091, .T. ) ;
#89677 = CARTESIAN_POINT ( 'NONE',  ( 17.49081203853565825, -2.909728817766679132, -34.30943779066389254 ) ) ;
#89678 = ORIENTED_EDGE ( 'NONE', *, *, #27897, .T. ) ;
#89679 = EDGE_CURVE ( 'NONE', #86675, #75683, #11951, .T. ) ;
#89680 = DIRECTION ( 'NONE',  ( -0.000000000000000000, -0.000000000000000000, 1.000000000000000000 ) ) ;
#89682 = VERTEX_POINT ( 'NONE', #131619 ) ;
#89681 = FACE_OUTER_BOUND ( 'NONE', #33629, .T. ) ;
#89683 = STYLED_ITEM ( 'NONE', ( #87465 ), #112081 ) ;
#89684 = LINE ( 'NONE', #123768, #101960 ) ;
#89685 = CARTESIAN_POINT ( 'NONE',  ( 69.25000000000000000, -9.735942053221458872E-16, 7.950000000000000178 ) ) ;
#89686 = ORIENTED_EDGE ( 'NONE', *, *, #57901, .F. ) ;
#89687 = VERTEX_POINT ( 'NONE', #68520 ) ;
#89688 = CARTESIAN_POINT ( 'NONE',  ( 151.4000000000000057, -17.48000000000005016, -33.92499999999998295 ) ) ;
#89689 = VERTEX_POINT ( 'NONE', #1754 ) ;
#89690 = ADVANCED_FACE ( 'NONE', ( #98276 ), #45349, .F. ) ;
#89691 = VECTOR ( 'NONE', #104387, 999.9999999999998863 ) ;
#89692 = AXIS2_PLACEMENT_3D ( 'NONE', #84095, #117370, #18044 ) ;
#89693 = DIRECTION ( 'NONE',  ( -0.3543493200069163240, -0.000000000000000000, -0.9351131265310288487 ) ) ;
#89694 = CARTESIAN_POINT ( 'NONE',  ( 102.7458603837962272, 3.974999999999996980, 6.884901960086287964 ) ) ;
#89695 = FILL_AREA_STYLE_COLOUR ( '', #101790 ) ;
#89696 = VERTEX_POINT ( 'NONE', #121434 ) ;
#89697 = EDGE_CURVE ( 'NONE', #3281, #51730, #33748, .T. ) ;
#89698 = FACE_OUTER_BOUND ( 'NONE', #44080, .T. ) ;
#89699 = PLANE ( 'NONE',  #31121 ) ;
#89700 = PLANE ( 'NONE',  #57774 ) ;
#89701 = CARTESIAN_POINT ( 'NONE',  ( 10.93750000000000178, -4.461849672132299105, 4.461849672132299993 ) ) ;
#89702 = CARTESIAN_POINT ( 'NONE',  ( 14.74000000000000021, 9.521314400968980422E-16, 0.000000000000000000 ) ) ;
#89703 = CONICAL_SURFACE ( 'NONE', #45759, 2.500000000000000888, 0.9599310885968822538 ) ;
#89704 = FACE_OUTER_BOUND ( 'NONE', #134602, .T. ) ;
#89705 = CARTESIAN_POINT ( 'NONE',  ( 2.999999999999981792, -10.44781430457072169, 5.000000000000000000 ) ) ;
#89706 = ORIENTED_EDGE ( 'NONE', *, *, #15205, .T. ) ;
#89707 = ORIENTED_EDGE ( 'NONE', *, *, #15855, .F. ) ;
#89708 = CARTESIAN_POINT ( 'NONE',  ( 1.889826771117872006, -22.22500000000000497, 4.785647885939354751 ) ) ;
#89709 = EDGE_LOOP ( 'NONE', ( #69278, #27539, #139635, #78940 ) ) ;
#89710 = CARTESIAN_POINT ( 'NONE',  ( 92.60459685856478984, 1.637169565754164946, -6.109999999999999432 ) ) ;
#89711 = CARTESIAN_POINT ( 'NONE',  ( -45.18398860626900415, 28.73617430169818832, 5.000000000000000000 ) ) ;
#89712 = CARTESIAN_POINT ( 'NONE',  ( -14.99451991528749595, 28.92564299267948513, 4.000000000000000000 ) ) ;
#89713 = DIRECTION ( 'NONE',  ( -1.000000000000000000, -0.000000000000000000, -0.000000000000000000 ) ) ;
#89714 = CYLINDRICAL_SURFACE ( 'NONE', #108087, 2.500000000000000000 ) ;
#89715 = VERTEX_POINT ( 'NONE', #76538 ) ;
#89716 = LINE ( 'NONE', #123079, #114594 ) ;
#89717 = CARTESIAN_POINT ( 'NONE',  ( 0.5685132242927012358, -0.4000000000000004108, 2.467792535850613866 ) ) ;
#89718 = CARTESIAN_POINT ( 'NONE',  ( -27.48921356237309155, -27.52281430457074762, 5.000000000000000000 ) ) ;
#89719 = EDGE_CURVE ( 'NONE', #53420, #40404, #34437, .T. ) ;
#89720 = DIRECTION ( 'NONE',  ( 0.6830127018922181881, 0.6830127018922202975, -0.2588190451025214056 ) ) ;
#89721 = CARTESIAN_POINT ( 'NONE',  ( -16.49999999999987210, -17.94781430457065241, 5.000000000000000000 ) ) ;
#89723 = ORIENTED_EDGE ( 'NONE', *, *, #92394, .T. ) ;
#89722 = DIRECTION ( 'NONE',  ( 0.000000000000000000, 1.000000000000000000, 0.000000000000000000 ) ) ;
#89724 = FACE_OUTER_BOUND ( 'NONE', #76309, .T. ) ;
#89725 = VECTOR ( 'NONE', #38104, 999.9999999999998863 ) ;
#89726 = CARTESIAN_POINT ( 'NONE',  ( 34.92499999999998295, -1.298069433179003695, 4.500000000000000888 ) ) ;
#89727 = CARTESIAN_POINT ( 'NONE',  ( -12.48921356237309155, -27.52281430457064104, 5.000000000000000000 ) ) ;
#89728 = DIRECTION ( 'NONE',  ( 0.6830127018922180770, -0.6830127018922204085, -0.2588190451025213501 ) ) ;
#89729 = CARTESIAN_POINT ( 'NONE',  ( 26.99999999999981526, -21.41253812416053748, 4.000000000000000000 ) ) ;
#89730 = ORIENTED_EDGE ( 'NONE', *, *, #44364, .F. ) ;
#89731 = ADVANCED_FACE ( 'NONE', ( #120713 ), #122869, .T. ) ;
#89732 = ORIENTED_EDGE ( 'NONE', *, *, #29576, .T. ) ;
#89733 = EDGE_LOOP ( 'NONE', ( #17752, #29476, #108162, #63963 ) ) ;
#89734 = CARTESIAN_POINT ( 'NONE',  ( 96.68793019189811844, 6.110000000000002984, -1.637169565754156730 ) ) ;
#89735 = VECTOR ( 'NONE', #143508, 999.9999999999998863 ) ;
#89736 = ORIENTED_EDGE ( 'NONE', *, *, #113061, .T. ) ;
#89737 = LINE ( 'NONE', #123820, #69460 ) ;
#89738 = DIRECTION ( 'NONE',  ( 0.7071067811865486830, -0.7071067811865464625, -0.000000000000000000 ) ) ;
#89739 = LINE ( 'NONE', #133961, #59631 ) ;
#89740 = CARTESIAN_POINT ( 'NONE',  ( 51.48921356237309510, -27.52281430457091460, 5.000000000000000000 ) ) ;
#89741 = ORIENTED_EDGE ( 'NONE', *, *, #97132, .T. ) ;
#89742 = CARTESIAN_POINT ( 'NONE',  ( 103.9583333333333286, 3.974999999999997424, 6.884901960086288852 ) ) ;
#89743 = DIRECTION ( 'NONE',  ( -0.3543493200069162685, -0.000000000000000000, -0.9351131265310288487 ) ) ;
#89744 = DIRECTION ( 'NONE',  ( -1.000000000000000000, -0.000000000000000000, -0.000000000000000000 ) ) ;
#89745 = CARTESIAN_POINT ( 'NONE',  ( 84.64126352523145158, 4.472830434245836706, 4.472830434245840259 ) ) ;
#89746 = EDGE_CURVE ( 'NONE', #46825, #14025, #67823, .T. ) ;
#89747 = VERTEX_POINT ( 'NONE', #77952 ) ;
#89748 = LINE ( 'NONE', #42706, #129962 ) ;
#89749 = CARTESIAN_POINT ( 'NONE',  ( -11.81601139373100651, 28.73617430169779041, 5.000000000000000000 ) ) ;
#89750 = ORIENTED_EDGE ( 'NONE', *, *, #123938, .F. ) ;
#89751 = EDGE_LOOP ( 'NONE', ( #95885, #57758, #124698, #7017 ) ) ;
#89752 = DIRECTION ( 'NONE',  ( 0.7071067811865487940, 0.7071067811865463515, 0.000000000000000000 ) ) ;
#89753 = EDGE_CURVE ( 'NONE', #83353, #106932, #9819, .T. ) ;
#89754 = DIRECTION ( 'NONE',  ( 0.6830127018922180770, -0.6830127018922204085, -0.2588190451025213501 ) ) ;
#89755 = CARTESIAN_POINT ( 'NONE',  ( -9.156123077392344101, -22.22500000000000142, 4.000000000000000000 ) ) ;
#89756 = CARTESIAN_POINT ( 'NONE',  ( 184.1500000000000057, -30.18000000000009564, -12.70000000000045404 ) ) ;
#89757 = LINE ( 'NONE', #101350, #109889 ) ;
#89758 = ORIENTED_EDGE ( 'NONE', *, *, #69315, .T. ) ;
#89759 = ORIENTED_EDGE ( 'NONE', *, *, #12893, .F. ) ;
#89760 = CARTESIAN_POINT ( 'NONE',  ( 12.70710678118645909, -6.740707523384214639, 5.000000000000000000 ) ) ;
#89761 = ORIENTED_EDGE ( 'NONE', *, *, #112910, .F. ) ;
#89762 = EDGE_LOOP ( 'NONE', ( #131247, #39571, #34758, #85170, #91961 ) ) ;
#89763 = FACE_OUTER_BOUND ( 'NONE', #63973, .T. ) ;
#89764 = ORIENTED_EDGE ( 'NONE', *, *, #51908, .T. ) ;
#89765 = CARTESIAN_POINT ( 'NONE',  ( 8.700255128608413102, -27.71228299555199825, 4.000000000000000000 ) ) ;
#89766 = DIRECTION ( 'NONE',  ( 0.7071067811865487940, 0.7071067811865463515, 0.000000000000000000 ) ) ;
#89767 = DIRECTION ( 'NONE',  ( 0.3543493200069162685, -0.000000000000000000, -0.9351131265310288487 ) ) ;
#89768 = CARTESIAN_POINT ( 'NONE',  ( 24.87009481391959298, 1.845822036158552892, 4.338987337627242091 ) ) ;
#89769 = EDGE_CURVE ( 'NONE', #89870, #81077, #132360, .T. ) ;
#89770 = VECTOR ( 'NONE', #67185, 1000.000000000000000 ) ;
#89771 = CARTESIAN_POINT ( 'NONE',  ( 26.40000000000000568, -16.48000000000005016, -34.92499999999998295 ) ) ;
#89772 = ORIENTED_EDGE ( 'NONE', *, *, #141435, .F. ) ;
#89773 = CIRCLE ( 'NONE', #34323, 2.500000000000000444 ) ;
#89774 = ORIENTED_EDGE ( 'NONE', *, *, #107961, .F. ) ;
#89775 = DIRECTION ( 'NONE',  ( -0.7071067811865486830, -0.7071067811865464625, 0.000000000000000000 ) ) ;
#89776 = ORIENTED_EDGE ( 'NONE', *, *, #118180, .T. ) ;
#89777 = PLANE ( 'NONE',  #2825 ) ;
#89779 = ORIENTED_EDGE ( 'NONE', *, *, #95939, .T. ) ;
#89778 = EDGE_CURVE ( 'NONE', #68985, #62041, #30568, .T. ) ;
#89780 = DIRECTION ( 'NONE',  ( -0.000000000000000000, -0.3543493200069152693, 0.9351131265310292928 ) ) ;
#89781 = VERTEX_POINT ( 'NONE', #22801 ) ;
#89782 = ORIENTED_EDGE ( 'NONE', *, *, #106642, .T. ) ;
#89783 = VECTOR ( 'NONE', #78574, 1000.000000000000000 ) ;
#89784 = VERTEX_POINT ( 'NONE', #10517 ) ;
#89785 = VECTOR ( 'NONE', #96519, 1000.000000000000114 ) ;
#89786 = EDGE_CURVE ( 'NONE', #123983, #117224, #95979, .T. ) ;
#89787 = ADVANCED_FACE ( 'NONE', ( #137330 ), #69967, .F. ) ;
#89788 = PLANE ( 'NONE',  #62826 ) ;
#89789 = LINE ( 'NONE', #23076, #36735 ) ;
#89791 = EDGE_CURVE ( 'NONE', #121119, #73381, #63633, .T. ) ;
#89790 = DIRECTION ( 'NONE',  ( -0.7071067811865486830, -0.7071067811865464625, 0.000000000000000000 ) ) ;
#89792 = CARTESIAN_POINT ( 'NONE',  ( 121.4795968585647614, 6.109999999999999432, 1.637169565754164280 ) ) ;
#89793 = CARTESIAN_POINT ( 'NONE',  ( -42.48921356237308800, -27.52281430457085065, 5.000000000000000000 ) ) ;
#89794 = EDGE_CURVE ( 'NONE', #95118, #55534, #127139, .T. ) ;
#89795 = DIRECTION ( 'NONE',  ( 0.7071067811865487940, -0.7071067811865463515, 0.000000000000000000 ) ) ;
#89796 = EDGE_CURVE ( 'NONE', #47233, #1370, #115515, .T. ) ;
#89797 = LINE ( 'NONE', #32589, #60971 ) ;
#89798 = CARTESIAN_POINT ( 'NONE',  ( -56.99451991528749062, 28.92564299267978001, 4.000000000000000000 ) ) ;
#89799 = EDGE_CURVE ( 'NONE', #41140, #85990, #27835, .T. ) ;
#89800 = VERTEX_POINT ( 'NONE', #112704 ) ;
#89801 = CARTESIAN_POINT ( 'NONE',  ( -27.48921356237309155, -27.52281430457074762, 5.000000000000000000 ) ) ;
#89802 = FACE_OUTER_BOUND ( 'NONE', #5832, .T. ) ;
#89803 = CARTESIAN_POINT ( 'NONE',  ( -36.18398860626899705, 28.73617430169812437, 5.000000000000000000 ) ) ;
#89804 = VERTEX_POINT ( 'NONE', #103244 ) ;
#89805 = VERTEX_POINT ( 'NONE', #3893 ) ;
#89806 = DIRECTION ( 'NONE',  ( 0.7071067811865487940, 0.7071067811865463515, 0.000000000000000000 ) ) ;
#89807 = ORIENTED_EDGE ( 'NONE', *, *, #54693, .T. ) ;
#89808 = ORIENTED_EDGE ( 'NONE', *, *, #125748, .T. ) ;
#89809 = FACE_OUTER_BOUND ( 'NONE', #129661, .T. ) ;
#89810 = CARTESIAN_POINT ( 'NONE',  ( 108.2875270504628986, 0.000000000000000000, -7.949999999999998401 ) ) ;
#89811 = EDGE_CURVE ( 'NONE', #5696, #114242, #46799, .T. ) ;
#89812 = LINE ( 'NONE', #134056, #65787 ) ;
#89813 = DIRECTION ( 'NONE',  ( -0.7071067811865487940, 0.7071067811865463515, 0.000000000000000000 ) ) ;
#89814 = VERTEX_POINT ( 'NONE', #4587 ) ;
#89815 = STYLED_ITEM ( 'NONE', ( #58838 ), #5117 ) ;
#89816 = DIRECTION ( 'NONE',  ( 0.7071067811865487940, 0.7071067811865463515, 0.000000000000000000 ) ) ;
#89817 = ORIENTED_EDGE ( 'NONE', *, *, #107627, .T. ) ;
#89818 = ADVANCED_FACE ( 'NONE', ( #125744 ), #38024, .T. ) ;
#89819 = LINE ( 'NONE', #102861, #44581 ) ;
#89820 = CARTESIAN_POINT ( 'NONE',  ( 22.96290314143522338, -3.967499999999994476, 6.871911579029513106 ) ) ;
#89821 = ORIENTED_EDGE ( 'NONE', *, *, #80129, .F. ) ;
#89822 = CARTESIAN_POINT ( 'NONE',  ( 84.49543019189812298, 5.291415217122917625, 3.055000000000002380 ) ) ;
#89823 = DIRECTION ( 'NONE',  ( -0.7071067811865486830, -0.7071067811865463515, 0.000000000000000000 ) ) ;
#89824 = FACE_OUTER_BOUND ( 'NONE', #120252, .T. ) ;
#89825 = ORIENTED_EDGE ( 'NONE', *, *, #82185, .F. ) ;
#89826 = ORIENTED_EDGE ( 'NONE', *, *, #70549, .T. ) ;
#89827 = ORIENTED_EDGE ( 'NONE', *, *, #62059, .T. ) ;
#89828 = DIRECTION ( 'NONE',  ( -0.6830127018922180770, -0.6830127018922204085, -0.2588190451025213501 ) ) ;
#89829 = DIRECTION ( 'NONE',  ( 0.000000000000000000, -1.000000000000000000, 0.000000000000000000 ) ) ;
#89830 = LINE ( 'NONE', #65266, #82101 ) ;
#89831 = LINE ( 'NONE', #123212, #63550 ) ;
#89832 = VERTEX_POINT ( 'NONE', #92358 ) ;
#89833 = AXIS2_PLACEMENT_3D ( 'NONE', #34412, #110514, #133042 ) ;
#89834 = CARTESIAN_POINT ( 'NONE',  ( -13.11345250541376473, 3.796869306786347487, 4.054893674211258237 ) ) ;
#89835 = CARTESIAN_POINT ( 'NONE',  ( -36.48921356237310221, -27.52281430457080802, 5.000000000000000000 ) ) ;
#89836 = CARTESIAN_POINT ( 'NONE',  ( 23.29298673570678346, -21.74070752338406720, 4.999753212805222446 ) ) ;
#89837 = ADVANCED_FACE ( 'NONE', ( #136586 ), #81541, .F. ) ;
#89838 = VERTEX_POINT ( 'NONE', #104678 ) ;
#89839 = PLANE ( 'NONE',  #109073 ) ;
#89840 = DIRECTION ( 'NONE',  ( 0.000000000000000000, 0.000000000000000000, 1.000000000000000000 ) ) ;
#89841 = ORIENTED_EDGE ( 'NONE', *, *, #62687, .F. ) ;
#89842 = ADVANCED_FACE ( 'NONE', ( #114811 ), #5346, .F. ) ;
#89844 = EDGE_LOOP ( 'NONE', ( #11301, #60683, #59075, #78455 ) ) ;
#89843 = DIRECTION ( 'NONE',  ( -0.7071067811865487940, 0.7071067811865463515, 0.000000000000000000 ) ) ;
#89845 = VERTEX_POINT ( 'NONE', #113406 ) ;
#89846 = DIRECTION ( 'NONE',  ( 0.3543493200069162685, -0.000000000000000000, -0.9351131265310288487 ) ) ;
#89847 = PLANE ( 'NONE',  #29868 ) ;
#89848 = ORIENTED_EDGE ( 'NONE', *, *, #6680, .T. ) ;
#89849 =( NAMED_UNIT ( * ) SI_UNIT ( $, .STERADIAN. ) SOLID_ANGLE_UNIT ( ) );
#89850 = UNCERTAINTY_MEASURE_WITH_UNIT (LENGTH_MEASURE( 1.000000000000000082E-05 ), #3278, 'distance_accuracy_value', 'NONE');
#89851 = EDGE_CURVE ( 'NONE', #89661, #84730, #47504, .T. ) ;
#89852 = DIRECTION ( 'NONE',  ( 0.6830127018922180770, -0.6830127018922204085, -0.2588190451025213501 ) ) ;
#89853 = CARTESIAN_POINT ( 'NONE',  ( -29.67183060077625711, 20.25929247661551003, 4.000000000000000000 ) ) ;
#89854 = DIRECTION ( 'NONE',  ( 0.7071067811865487940, 0.7071067811865463515, 0.000000000000000000 ) ) ;
#89855 = VECTOR ( 'NONE', #20595, 1000.000000000000000 ) ;
#89856 = CARTESIAN_POINT ( 'NONE',  ( 48.20419371712955581, -6.884901960086285300, -3.975000000000000089 ) ) ;
#89857 = DIRECTION ( 'NONE',  ( 0.7071067811865487940, -0.7071067811865463515, 0.000000000000000000 ) ) ;
#89858 = ADVANCED_FACE ( 'NONE', ( #48894 ), #49631, .F. ) ;
#89859 = FACE_OUTER_BOUND ( 'NONE', #78246, .T. ) ;
#89860 = DIRECTION ( 'NONE',  ( 0.7071067811865486830, -0.7071067811865464625, -0.000000000000000000 ) ) ;
#89861 = DIRECTION ( 'NONE',  ( 0.000000000000000000, -5.559056632600921604E-15, 1.000000000000000000 ) ) ;
#89862 = CARTESIAN_POINT ( 'NONE',  ( 18.79123647476855652, -9.717572351234235426E-16, -7.934999999999990727 ) ) ;
#89863 = CARTESIAN_POINT ( 'NONE',  ( 2.895403141435219485, 2.126176841940962348, 7.934999999999988951 ) ) ;
#89864 = DIRECTION ( 'NONE',  ( 0.6830127018922181881, 0.6830127018922202975, -0.2588190451025214056 ) ) ;
#89865 = CARTESIAN_POINT ( 'NONE',  ( 109.5000000000000000, 0.000000000000000000, -7.950000000000000178 ) ) ;
#89866 = DIRECTION ( 'NONE',  ( -0.6830127018922180770, -0.6830127018922204085, -0.2588190451025213501 ) ) ;
#89867 = ORIENTED_EDGE ( 'NONE', *, *, #88926, .F. ) ;
#89868 = VERTEX_POINT ( 'NONE', #36567 ) ;
#89869 = CARTESIAN_POINT ( 'NONE',  ( 104.6875000000000000, -5.819803920172573086, 5.819803920172572198 ) ) ;
#89870 = VERTEX_POINT ( 'NONE', #135208 ) ;
#89871 = ORIENTED_EDGE ( 'NONE', *, *, #134555, .T. ) ;
#89872 = EDGE_CURVE ( 'NONE', #36166, #15951, #138034, .T. ) ;
#89873 = VERTEX_POINT ( 'NONE', #80814 ) ;
#89874 = CARTESIAN_POINT ( 'NONE',  ( 12.18398860626900060, 28.73617430169795739, 5.000000000000000000 ) ) ;
#89875 = CARTESIAN_POINT ( 'NONE',  ( 17.30673006690389926, -3.740707523384244837, 12.88036043432863664 ) ) ;
#89876 = CARTESIAN_POINT ( 'NONE',  ( -18.72281430457046270, -21.72500000000000142, 5.000000000000000000 ) ) ;
#89877 = VERTEX_POINT ( 'NONE', #80113 ) ;
#89878 = AXIS2_PLACEMENT_3D ( 'NONE', #7056, #85361, #140463 ) ;
#89879 = LINE ( 'NONE', #134863, #76489 ) ;
#89880 = CARTESIAN_POINT ( 'NONE',  ( -6.524001385854439228, 22.03583458319438293, 4.979811245910091166 ) ) ;
#89881 = VECTOR ( 'NONE', #36626, 1000.000000000000000 ) ;
#89882 = DIRECTION ( 'NONE',  ( 0.7071067811865486830, -0.7071067811865464625, -0.000000000000000000 ) ) ;
#89883 = DIRECTION ( 'NONE',  ( -0.000000000000000000, -0.3543493200069152693, 0.9351131265310292928 ) ) ;
#89884 = EDGE_CURVE ( 'NONE', #68280, #15118, #47412, .T. ) ;
#89885 = ORIENTED_EDGE ( 'NONE', *, *, #16717, .T. ) ;
#89886 = EDGE_CURVE ( 'NONE', #31340, #8931, #124296, .T. ) ;
#89887 = PLANE ( 'NONE',  #78864 ) ;
#89888 = LINE ( 'NONE', #97354, #72491 ) ;
#89889 = PLANE ( 'NONE',  #130678 ) ;
#89891 = CARTESIAN_POINT ( 'NONE',  ( 4.911592354503321545, 9.902892378096218942E-16, 0.000000000000000000 ) ) ;
#89890 = AXIS2_PLACEMENT_3D ( 'NONE', #71618, #16483, #60779 ) ;
#89892 = LINE ( 'NONE', #36940, #12219 ) ;
#89893 = CARTESIAN_POINT ( 'NONE',  ( 29.18753812416031934, -22.22500000000000497, 4.000000000000000000 ) ) ;
#89894 = VECTOR ( 'NONE', #129715, 1000.000000000000000 ) ;
#89895 = FACE_OUTER_BOUND ( 'NONE', #111730, .T. ) ;
#89896 = CARTESIAN_POINT ( 'NONE',  ( 8.994519915287490619, 28.92564299267944250, 4.000000000000000000 ) ) ;
#89897 = ADVANCED_FACE ( 'NONE', ( #106805 ), #84391, .F. ) ;
#89898 = ORIENTED_EDGE ( 'NONE', *, *, #143283, .F. ) ;
#89899 = ORIENTED_EDGE ( 'NONE', *, *, #82063, .F. ) ;
#89900 = CARTESIAN_POINT ( 'NONE',  ( 124.9795968585647756, 6.109999999999999432, 1.637169565754164280 ) ) ;
#89901 = ORIENTED_EDGE ( 'NONE', *, *, #101575, .F. ) ;
#89902 = CARTESIAN_POINT ( 'NONE',  ( 100.3124999999999858, 5.819803920172571310, 5.819803920172576639 ) ) ;
#89903 = AXIS2_PLACEMENT_3D ( 'NONE', #61203, #28535, #93062 ) ;
#89904 = DIRECTION ( 'NONE',  ( 1.248002500702738701E-15, 1.000000000000000000, -0.000000000000000000 ) ) ;
#89905 = CARTESIAN_POINT ( 'NONE',  ( 60.29974487139158867, -27.71228299555248142, 4.000000000000000000 ) ) ;
#89907 = EDGE_CURVE ( 'NONE', #116519, #29125, #19099, .T. ) ;
#89906 = CARTESIAN_POINT ( 'NONE',  ( -13.49999999999990763, 13.46639925780212366, 5.000000000000000000 ) ) ;
#89908 = VECTOR ( 'NONE', #130367, 999.9999999999998863 ) ;
#89909 = CARTESIAN_POINT ( 'NONE',  ( 118.6204301918981230, 3.055000000000001936, -5.291415217122916737 ) ) ;
#89910 = EDGE_CURVE ( 'NONE', #86031, #60612, #42310, .T. ) ;
#89911 = EDGE_LOOP ( 'NONE', ( #13655, #40954, #90126 ) ) ;
#89912 = EDGE_LOOP ( 'NONE', ( #121679, #127910, #133856, #68786 ) ) ;
#89913 = CARTESIAN_POINT ( 'NONE',  ( -30.48921356237309510, -27.52281430457076894, 5.000000000000000000 ) ) ;
#89914 = AXIS2_PLACEMENT_3D ( 'NONE', #133331, #2041, #55057 ) ;
#89915 = ORIENTED_EDGE ( 'NONE', *, *, #5485, .T. ) ;
#89916 = VERTEX_POINT ( 'NONE', #29256 ) ;
#89917 = CARTESIAN_POINT ( 'NONE',  ( 35.00043019189810423, -3.055000000000002380, 5.291415217122920289 ) ) ;
#89918 = ORIENTED_EDGE ( 'NONE', *, *, #94572, .T. ) ;
#89919 = DIRECTION ( 'NONE',  ( 0.000000000000000000, 0.000000000000000000, 1.000000000000000000 ) ) ;
#89920 = EDGE_CURVE ( 'NONE', #51650, #138101, #74207, .T. ) ;
#89921 = CARTESIAN_POINT ( 'NONE',  ( 3.858736474768553304, 5.808823158059031044, -5.808823158059037262 ) ) ;
#89922 = CARTESIAN_POINT ( 'NONE',  ( 29.95376352523145158, -6.109999999999998543, -3.741295971395162543E-16 ) ) ;
#89923 = ORIENTED_EDGE ( 'NONE', *, *, #3985, .T. ) ;
#89924 = CARTESIAN_POINT ( 'NONE',  ( 0.000000000000000000, 9.735942053221458872E-16, -7.950000000000000178 ) ) ;
#89925 = ORIENTED_EDGE ( 'NONE', *, *, #35869, .F. ) ;
#89926 = VERTEX_POINT ( 'NONE', #41556 ) ;
#89927 = VECTOR ( 'NONE', #10784, 1000.000000000000000 ) ;
#89928 = ORIENTED_EDGE ( 'NONE', *, *, #75387, .F. ) ;
#89929 = VECTOR ( 'NONE', #77758, 999.9999999999998863 ) ;
#89930 = SURFACE_SIDE_STYLE ('',( #102275 ) ) ;
#89931 = CARTESIAN_POINT ( 'NONE',  ( -30.48921356237309510, -27.52281430457076894, 5.000000000000000000 ) ) ;
#89932 = ORIENTED_EDGE ( 'NONE', *, *, #96324, .F. ) ;
#89933 = CARTESIAN_POINT ( 'NONE',  ( 17.64297733114876365, -22.22500000000000142, -14.91997170495656277 ) ) ;
#89934 = DIRECTION ( 'NONE',  ( 0.5735764363510453823, -0.8191520442889923537, 1.003171929053525486E-16 ) ) ;
#89935 = DIRECTION ( 'NONE',  ( 0.6830127018922181881, 0.6830127018922202975, -0.2588190451025214056 ) ) ;
#89936 = CARTESIAN_POINT ( 'NONE',  ( -0.7071067811865372477, -12.74070752338415424, 5.000000000000000000 ) ) ;
#89937 = FACE_BOUND ( 'NONE', #41268, .T. ) ;
#89938 = EDGE_LOOP ( 'NONE', ( #54305, #15204, #133348, #78198 ) ) ;
#89939 = CARTESIAN_POINT ( 'NONE',  ( -12.32816939922344268, -6.740707523384212863, 4.000000000000000000 ) ) ;
#89940 = CARTESIAN_POINT ( 'NONE',  ( 57.18398860626899705, 28.73617430169827358, 5.000000000000000000 ) ) ;
#89941 = CARTESIAN_POINT ( 'NONE',  ( 27.48921356237309155, -27.52281430457074762, 5.000000000000000000 ) ) ;
#89942 = ORIENTED_EDGE ( 'NONE', *, *, #74001, .F. ) ;
#89943 = DIRECTION ( 'NONE',  ( 0.6830127018922181881, 0.6830127018922202975, -0.2588190451025214056 ) ) ;
#89944 = ORIENTED_EDGE ( 'NONE', *, *, #106316, .T. ) ;
#89945 = EDGE_LOOP ( 'NONE', ( #21933, #17788, #138413, #120644 ) ) ;
#89946 = VERTEX_POINT ( 'NONE', #86520 ) ;
#89947 = EDGE_CURVE ( 'NONE', #97043, #61191, #73499, .T. ) ;
#89948 = CARTESIAN_POINT ( 'NONE',  ( 44.39126352523143737, -4.472830434245838482, -4.472830434245838482 ) ) ;
#89949 = VERTEX_POINT ( 'NONE', #119122 ) ;
#89950 = PLANE ( 'NONE',  #106530 ) ;
#89951 = EDGE_CURVE ( 'NONE', #32782, #17436, #128770, .T. ) ;
#89952 = ADVANCED_FACE ( 'NONE', ( #117663 ), #94504, .F. ) ;
#89953 = DIRECTION ( 'NONE',  ( -0.7071067811865487940, 0.7071067811865463515, 0.000000000000000000 ) ) ;
#89954 = ORIENTED_EDGE ( 'NONE', *, *, #140727, .T. ) ;
#89955 = EDGE_CURVE ( 'NONE', #49015, #1952, #130746, .T. ) ;
#89956 = LINE ( 'NONE', #66802, #53826 ) ;
#89957 = DIRECTION ( 'NONE',  ( 0.3543493200069162685, -0.000000000000000000, -0.9351131265310288487 ) ) ;
#89958 = ADVANCED_FACE ( 'NONE', ( #139498 ), #62625, .T. ) ;
#89959 = DIRECTION ( 'NONE',  ( -0.7071067811865486830, -0.7071067811865464625, 0.000000000000000000 ) ) ;
#89960 =( LENGTH_UNIT ( ) NAMED_UNIT ( * ) SI_UNIT ( .MILLI., .METRE. ) );
#89961 = CARTESIAN_POINT ( 'NONE',  ( 15.96626304157554266, 4.202752102959690472E-16, 0.000000000000000000 ) ) ;
#89962 = EDGE_CURVE ( 'NONE', #24150, #127065, #102940, .T. ) ;
#89963 = EDGE_LOOP ( 'NONE', ( #11724, #763, #66064, #30162 ) ) ;
#89964 = VERTEX_POINT ( 'NONE', #7494 ) ;
#89965 = ORIENTED_EDGE ( 'NONE', *, *, #13916, .T. ) ;
#89966 = EDGE_LOOP ( 'NONE', ( #3988, #129160, #36235, #131424 ) ) ;
#89967 = CARTESIAN_POINT ( 'NONE',  ( -66.29974487139159578, -27.71228299555252406, 4.000000000000000000 ) ) ;
#89968 = VECTOR ( 'NONE', #36816, 1000.000000000000000 ) ;
#89969 = VECTOR ( 'NONE', #42621, 1000.000000000000000 ) ;
#89970 = ORIENTED_EDGE ( 'NONE', *, *, #21019, .T. ) ;
#89971 = VECTOR ( 'NONE', #128990, 1000.000000000000000 ) ;
#89973 = EDGE_LOOP ( 'NONE', ( #106093, #134855, #59841, #51229 ) ) ;
#89972 = AXIS2_PLACEMENT_3D ( 'NONE', #22167, #43956, #52670 ) ;
#89974 = FILL_AREA_STYLE_COLOUR ( '', #118458 ) ;
#89975 = ADVANCED_FACE ( 'NONE', ( #19803 ), #108211, .F. ) ;
#89976 = ADVANCED_FACE ( 'NONE', ( #107532 ), #140179, .F. ) ;
#89977 = FACE_OUTER_BOUND ( 'NONE', #114747, .T. ) ;
#89978 = VERTEX_POINT ( 'NONE', #129275 ) ;
#89979 = CARTESIAN_POINT ( 'NONE',  ( -9.656710001662071718, 3.759292476615678336, 13.27625715073263457 ) ) ;
#89980 = AXIS2_PLACEMENT_3D ( 'NONE', #82685, #49369, #40611 ) ;
#89981 = VECTOR ( 'NONE', #26396, 1000.000000000000000 ) ;
#89982 = EDGE_CURVE ( 'NONE', #31545, #36043, #85779, .T. ) ;
#89983 = CARTESIAN_POINT ( 'NONE',  ( -0.1839886062690032631, 28.73617430169787568, 5.000000000000000000 ) ) ;
#89984 = CARTESIAN_POINT ( 'NONE',  ( 26.75456980810189123, -6.871911579029512218, 3.967499999999996252 ) ) ;
#89985 = DIRECTION ( 'NONE',  ( -0.6830127018922181881, 0.6830127018922202975, -0.2588190451025214056 ) ) ;
#89986 = VERTEX_POINT ( 'NONE', #64044 ) ;
#89987 = CARTESIAN_POINT ( 'NONE',  ( 107.2454301918981088, -5.291415217122919401, -3.055000000000000604 ) ) ;
#89988 = CARTESIAN_POINT ( 'NONE',  ( 19.05000000000000071, 3.174999999999997158, 5.000000000000000000 ) ) ;
#89989 = LINE ( 'NONE', #113898, #23302 ) ;
#89990 = DIRECTION ( 'NONE',  ( -1.000000000000000000, -0.000000000000000000, -0.000000000000000000 ) ) ;
#89991 = ADVANCED_FACE ( 'NONE', ( #28569 ), #72828, .F. ) ;
#89993 = ORIENTED_EDGE ( 'NONE', *, *, #98511, .T. ) ;
#89992 = DIRECTION ( 'NONE',  ( 0.7071067811865487940, 0.7071067811865463515, -0.000000000000000000 ) ) ;
#89994 = AXIS2_PLACEMENT_3D ( 'NONE', #86312, #120307, #10150 ) ;
#89995 = DIRECTION ( 'NONE',  ( 0.000000000000000000, -1.000000000000000000, 0.000000000000000000 ) ) ;
#89997 = ORIENTED_EDGE ( 'NONE', *, *, #101087, .T. ) ;
#89996 = AXIS2_PLACEMENT_3D ( 'NONE', #17662, #59270, #107543 ) ;
#89998 = LINE ( 'NONE', #100190, #77526 ) ;
#89999 = DIRECTION ( 'NONE',  ( 0.7071067811865487940, -0.7071067811865463515, 0.000000000000000000 ) ) ;
#90000 = LINE ( 'NONE', #13141, #118973 ) ;
#90001 = ORIENTED_EDGE ( 'NONE', *, *, #33554, .T. ) ;
#90002 = CARTESIAN_POINT ( 'NONE',  ( -17.29289321881332953, -3.740707523384248390, 5.000000000000000000 ) ) ;
#90003 = CARTESIAN_POINT ( 'NONE',  ( -53.99451991528749062, 28.92564299267975869, 4.000000000000000000 ) ) ;
#90004 = DIRECTION ( 'NONE',  ( -0.7071067811865486830, 0.7071067811865464625, 0.000000000000000000 ) ) ;
#90005 = EDGE_CURVE ( 'NONE', #133772, #63910, #77086, .T. ) ;
#90006 = VERTEX_POINT ( 'NONE', #31416 ) ;
#90007 = VECTOR ( 'NONE', #16014, 1000.000000000000227 ) ;
#90008 = AXIS2_PLACEMENT_3D ( 'NONE', #69801, #70529, #115360 ) ;
#90010 = VECTOR ( 'NONE', #109293, 999.9999999999998863 ) ;
#90009 = LINE ( 'NONE', #24763, #132638 ) ;
#90011 = ORIENTED_EDGE ( 'NONE', *, *, #34479, .F. ) ;
#90012 = VECTOR ( 'NONE', #6191, 1000.000000000000000 ) ;
#90013 = DIRECTION ( 'NONE',  ( 1.000000000000000000, 1.224606353822377258E-16, 0.000000000000000000 ) ) ;
#90015 = ORIENTED_EDGE ( 'NONE', *, *, #27226, .F. ) ;
#90014 = PLANE ( 'NONE',  #25499 ) ;
#90016 = ORIENTED_EDGE ( 'NONE', *, *, #116405, .F. ) ;
#90017 = LINE ( 'NONE', #134263, #65838 ) ;
#90018 = PRESENTATION_LAYER_ASSIGNMENT (  '', '', ( #140934 ) ) ;
#90019 = LINE ( 'NONE', #135000, #34343 ) ;
#90020 = ORIENTED_EDGE ( 'NONE', *, *, #100296, .T. ) ;
#90021 = VECTOR ( 'NONE', #81990, 1000.000000000000227 ) ;
#90022 = DIRECTION ( 'NONE',  ( 0.7071067811865487940, 0.7071067811865463515, 0.000000000000000000 ) ) ;
#90023 = SURFACE_STYLE_FILL_AREA ( #67607 ) ;
#90024 = DIRECTION ( 'NONE',  ( -0.7071067811865486830, -0.7071067811865464625, -0.000000000000000000 ) ) ;
#90025 = ORIENTED_EDGE ( 'NONE', *, *, #56926, .F. ) ;
#90026 = CARTESIAN_POINT ( 'NONE',  ( 60.29974487139158867, -27.71228299555248142, 4.000000000000000000 ) ) ;
#90027 = ADVANCED_FACE ( 'NONE', ( #67644 ), #76349, .F. ) ;
#90028 = PLANE ( 'NONE',  #32837 ) ;
#90029 = DIRECTION ( 'NONE',  ( -0.7071067811865486830, -0.7071067811865464625, 0.000000000000000000 ) ) ;
#90030 = VECTOR ( 'NONE', #101060, 1000.000000000000000 ) ;
#90031 = DIRECTION ( 'NONE',  ( 0.2399999999999954947, 0.000000000000000000, -0.9707728879609288652 ) ) ;
#90032 = FACE_OUTER_BOUND ( 'NONE', #13218, .T. ) ;
#90033 = LINE ( 'NONE', #34248, #25749 ) ;
#90034 = EDGE_LOOP ( 'NONE', ( #140452, #46242, #99740, #49859, #107690, #14429 ) ) ;
#90035 = ORIENTED_EDGE ( 'NONE', *, *, #37186, .F. ) ;
#90036 = ORIENTED_EDGE ( 'NONE', *, *, #79020, .F. ) ;
#90037 = DIRECTION ( 'NONE',  ( -0.7071067811865486830, -0.7071067811865464625, 0.000000000000000000 ) ) ;
#90038 = ORIENTED_EDGE ( 'NONE', *, *, #110189, .T. ) ;
#90039 = ORIENTED_EDGE ( 'NONE', *, *, #74001, .T. ) ;
#90040 = EDGE_CURVE ( 'NONE', #21343, #141074, #65501, .T. ) ;
#90041 = ORIENTED_EDGE ( 'NONE', *, *, #29130, .F. ) ;
#90042 = CARTESIAN_POINT ( 'NONE',  ( 1.529293640529030496, -1.216522783188787482, -6.459157641439147390 ) ) ;
#90043 = ORIENTED_EDGE ( 'NONE', *, *, #119601, .F. ) ;
#90044 = DIRECTION ( 'NONE',  ( -0.6830127018922180770, -0.6830127018922204085, -0.2588190451025213501 ) ) ;
#90045 = CARTESIAN_POINT ( 'NONE',  ( 25.39999999999999858, 7.568741776763671325, 1.931219224265529055 ) ) ;
#90046 = FACE_OUTER_BOUND ( 'NONE', #7198, .T. ) ;
#90047 = DIRECTION ( 'NONE',  ( 0.3543493200069163240, 0.000000000000000000, -0.9351131265310288487 ) ) ;
#90048 = CARTESIAN_POINT ( 'NONE',  ( 125.7087635252314470, -7.482591942790329030E-16, 6.110000000000001208 ) ) ;
#90049 = EDGE_CURVE ( 'NONE', #29880, #137064, #12497, .T. ) ;
#90050 = ORIENTED_EDGE ( 'NONE', *, *, #83842, .F. ) ;
#90051 = ADVANCED_FACE ( 'NONE', ( #78490 ), #121261, .T. ) ;
#90052 = DIRECTION ( 'NONE',  ( -0.6830127018922181881, 0.6830127018922202975, -0.2588190451025214056 ) ) ;
#90053 = CARTESIAN_POINT ( 'NONE',  ( -7.110173228882056051, -22.22500000000000497, 4.785647885939354751 ) ) ;
#90054 = CARTESIAN_POINT ( 'NONE',  ( -11.99451991528749417, 28.92564299267946382, 4.000000000000000000 ) ) ;
#90055 = LINE ( 'NONE', #113234, #64148 ) ;
#90056 = DIRECTION ( 'NONE',  ( 0.000000000000000000, 0.000000000000000000, 1.000000000000000000 ) ) ;
#90057 = CARTESIAN_POINT ( 'NONE',  ( -42.29974487139158157, -27.71228299555235708, 4.000000000000000000 ) ) ;
#90058 = CARTESIAN_POINT ( 'NONE',  ( 27.18398860626900060, 28.73617430169806042, 5.000000000000000000 ) ) ;
#90059 = CARTESIAN_POINT ( 'NONE',  ( 45.28752705046289151, 0.000000000000000000, -7.949999999999998401 ) ) ;
#90060 = LINE ( 'NONE', #89362, #132486 ) ;
#90061 = CARTESIAN_POINT ( 'NONE',  ( 27.32816939922333432, -9.740707523384191546, 4.000000000000000000 ) ) ;
#90062 = VERTEX_POINT ( 'NONE', #109679 ) ;
#90063 = ORIENTED_EDGE ( 'NONE', *, *, #80980, .T. ) ;
#90064 = CARTESIAN_POINT ( 'NONE',  ( 46.93749999999999289, 5.819803920172573974, -5.819803920172572198 ) ) ;
#90065 = LINE ( 'NONE', #69065, #143423 ) ;
#90066 = ADVANCED_FACE ( 'NONE', ( #11042 ), #133589, .F. ) ;
#90067 = CARTESIAN_POINT ( 'NONE',  ( 2.139447441471317379, 4.584330080086930965E-16, 0.000000000000000000 ) ) ;
#90068 = VERTEX_POINT ( 'NONE', #119811 ) ;
#90069 = LINE ( 'NONE', #911, #61790 ) ;
#90070 = PLANE ( 'NONE',  #100123 ) ;
#90071 = AXIS2_PLACEMENT_3D ( 'NONE', #97107, #41330, #86991 ) ;
#90072 = CARTESIAN_POINT ( 'NONE',  ( 36.89626352523143993, 4.472830434245840259, -4.472830434245839371 ) ) ;
#90073 = EDGE_CURVE ( 'NONE', #135680, #66418, #110366, .T. ) ;
#90074 = VERTEX_POINT ( 'NONE', #87218 ) ;
#90075 =( LENGTH_UNIT ( ) NAMED_UNIT ( * ) SI_UNIT ( .MILLI., .METRE. ) );
#90077 = ORIENTED_EDGE ( 'NONE', *, *, #43880, .T. ) ;
#90076 = VECTOR ( 'NONE', #45054, 999.9999999999998863 ) ;
#90078 = CARTESIAN_POINT ( 'NONE',  ( 31.92500000000002203, -21.76999999999999247, -39.50000000000000000 ) ) ;
#90079 = VECTOR ( 'NONE', #977, 1000.000000000000000 ) ;
#90080 = VECTOR ( 'NONE', #133727, 1000.000000000000227 ) ;
#90081 = AXIS2_PLACEMENT_3D ( 'NONE', #140901, #61274, #60539 ) ;
#90082 = LINE ( 'NONE', #12523, #75435 ) ;
#90083 =( NAMED_UNIT ( * ) SI_UNIT ( $, .STERADIAN. ) SOLID_ANGLE_UNIT ( ) );
#90084 = MECHANICAL_DESIGN_GEOMETRIC_PRESENTATION_REPRESENTATION (  '', ( #9009 ), #57632 ) ;
#90085 = DIRECTION ( 'NONE',  ( 0.000000000000000000, -1.000000000000000000, 0.000000000000000000 ) ) ;
#90087 = ADVANCED_FACE ( 'NONE', ( #20501 ), #66195, .F. ) ;
#90086 = ORIENTED_EDGE ( 'NONE', *, *, #89427, .F. ) ;
#90088 = LINE ( 'NONE', #99522, #104371 ) ;
#90089 = ORIENTED_EDGE ( 'NONE', *, *, #22878, .T. ) ;
#90090 = CARTESIAN_POINT ( 'NONE',  ( 39.89169371712955581, 2.130196079827421762, 7.950000000000000178 ) ) ;
#90091 = EDGE_CURVE ( 'NONE', #75313, #97144, #112249, .T. ) ;
#90092 = DIRECTION ( 'NONE',  ( -0.6830127018922181881, 0.6830127018922202975, -0.2588190451025214056 ) ) ;
#90093 = FILL_AREA_STYLE_COLOUR ( '', #140403 ) ;
#90094 = ADVANCED_FACE ( 'NONE', ( #98784 ), #111078, .F. ) ;
#90095 = PLANE ( 'NONE',  #49195 ) ;
#90096 = CARTESIAN_POINT ( 'NONE',  ( 36.08314806772909833, 21.75929247661549937, 7.311836541448132998 ) ) ;
#90097 = DIRECTION ( 'NONE',  ( 0.7071067811865486830, -0.7071067811865464625, -0.000000000000000000 ) ) ;
#90098 = AXIS2_PLACEMENT_3D ( 'NONE', #136389, #37078, #34239 ) ;
#90099 = ORIENTED_EDGE ( 'NONE', *, *, #62067, .T. ) ;
#90100 = CARTESIAN_POINT ( 'NONE',  ( 27.32816939922333432, -12.74070752338415247, 4.000000000000000000 ) ) ;
#90101 = CARTESIAN_POINT ( 'NONE',  ( 59.41209685856478728, 5.291415217122921177, -3.054999999999994831 ) ) ;
#90102 = CARTESIAN_POINT ( 'NONE',  ( 2.994519915287485734, 28.92564299267940342, 4.000000000000000000 ) ) ;
#90103 = CARTESIAN_POINT ( 'NONE',  ( -24.48921356237309510, -27.52281430457072631, 5.000000000000000000 ) ) ;
#90105 = ORIENTED_EDGE ( 'NONE', *, *, #10585, .F. ) ;
#90104 = CARTESIAN_POINT ( 'NONE',  ( -6.499999999999999112, 0.000000000000000000, 10.00000000000000000 ) ) ;
#90106 = ORIENTED_EDGE ( 'NONE', *, *, #61850, .F. ) ;
#90107 = VECTOR ( 'NONE', #119434, 1000.000000000000000 ) ;
#90108 = VECTOR ( 'NONE', #64892, 1000.000000000000227 ) ;
#90109 = DIRECTION ( 'NONE',  ( -0.000000000000000000, 0.3543493200069153248, 0.9351131265310292928 ) ) ;
#90110 = VERTEX_POINT ( 'NONE', #11769 ) ;
#90111 = ADVANCED_FACE ( 'NONE', ( #32863 ), #55316, .T. ) ;
#90112 = VECTOR ( 'NONE', #116822, 999.9999999999998863 ) ;
#90113 = CARTESIAN_POINT ( 'NONE',  ( 32.75030053044775968, 22.27000000000001023, -14.49242101875391064 ) ) ;
#90114 = ORIENTED_EDGE ( 'NONE', *, *, #122223, .F. ) ;
#90115 = CARTESIAN_POINT ( 'NONE',  ( 0.000000000000000000, 0.000000000000000000, 5.000000000000000000 ) ) ;
#90116 = CARTESIAN_POINT ( 'NONE',  ( -57.18398860626899705, 28.73617430169827358, 5.000000000000000000 ) ) ;
#90117 = VECTOR ( 'NONE', #117861, 1000.000000000000000 ) ;
#90118 = CIRCLE ( 'NONE', #87755, 2.500000000000000444 ) ;
#90120 = VECTOR ( 'NONE', #20305, 1000.000000000000000 ) ;
#90119 = DIRECTION ( 'NONE',  ( 0.7071067811865487940, -0.7071067811865463515, 0.000000000000000000 ) ) ;
#90121 = FACE_BOUND ( 'NONE', #73795, .T. ) ;
#90122 = CARTESIAN_POINT ( 'NONE',  ( -14.19331503651554272, 6.646281381260698673, 4.665372575888455664 ) ) ;
#90123 = DIRECTION ( 'NONE',  ( 0.7071067811865487940, 0.7071067811865463515, -0.000000000000000000 ) ) ;
#90124 = DIRECTION ( 'NONE',  ( -0.000000000000000000, 0.000000000000000000, 1.000000000000000000 ) ) ;
#90126 = ORIENTED_EDGE ( 'NONE', *, *, #112601, .T. ) ;
#90125 = DIRECTION ( 'NONE',  ( 0.7071067811865486830, -0.7071067811865464625, -0.000000000000000000 ) ) ;
#90127 = AXIS2_PLACEMENT_3D ( 'NONE', #98287, #75823, #106995 ) ;
#90128 = PRESENTATION_LAYER_ASSIGNMENT (  '', '', ( #134140 ) ) ;
#90129 = CARTESIAN_POINT ( 'NONE',  ( 0.4892135623730947680, -27.52281430457055578, 5.000000000000000000 ) ) ;
#90130 = ORIENTED_EDGE ( 'NONE', *, *, #55115, .F. ) ;
#90132 = VERTEX_POINT ( 'NONE', #45181 ) ;
#90131 = ADVANCED_FACE ( 'NONE', ( #121960 ), #162, .F. ) ;
#90133 = CARTESIAN_POINT ( 'NONE',  ( 74.87043019189812298, -3.055000000000001492, 5.291415217122917625 ) ) ;
#90134 = VERTEX_POINT ( 'NONE', #33581 ) ;
#90135 = DIRECTION ( 'NONE',  ( 0.7071067811865487940, 0.7071067811865463515, -0.000000000000000000 ) ) ;
#90136 = DIRECTION ( 'NONE',  ( -0.7071067811865487940, 0.7071067811865463515, 0.000000000000000000 ) ) ;
#90137 = EDGE_CURVE ( 'NONE', #79543, #2861, #89357, .T. ) ;
#90138 = VERTEX_POINT ( 'NONE', #53906 ) ;
#90139 = FACE_OUTER_BOUND ( 'NONE', #130802, .T. ) ;
#90140 = AXIS2_PLACEMENT_3D ( 'NONE', #134993, #12452, #121915 ) ;
#90141 = ADVANCED_FACE ( 'NONE', ( #98099 ), #131444, .F. ) ;
#90142 = EDGE_CURVE ( 'NONE', #57153, #11328, #15328, .T. ) ;
#90143 = LINE ( 'NONE', #3126, #91196 ) ;
#90144 = DIRECTION ( 'NONE',  ( 1.000000000000000000, 0.000000000000000000, 0.000000000000000000 ) ) ;
#90145 = DIRECTION ( 'NONE',  ( 1.000000000000000000, 0.000000000000000000, 0.000000000000000000 ) ) ;
#90147 =( LENGTH_UNIT ( ) NAMED_UNIT ( * ) SI_UNIT ( .MILLI., .METRE. ) );
#90146 = DIRECTION ( 'NONE',  ( -0.7071067811865486830, 0.7071067811865464625, 0.000000000000000000 ) ) ;
#90148 = DIRECTION ( 'NONE',  ( -1.000000000000000000, -1.224606353822377258E-16, -0.000000000000000000 ) ) ;
#90149 = CARTESIAN_POINT ( 'NONE',  ( 12.29974487139158512, -27.71228299555214747, 4.000000000000000000 ) ) ;
#90150 = EDGE_LOOP ( 'NONE', ( #55000, #97282, #67421, #32694 ) ) ;
#90151 = VERTEX_POINT ( 'NONE', #16035 ) ;
#90152 = DIRECTION ( 'NONE',  ( -0.000000000000000000, 0.000000000000000000, 1.000000000000000000 ) ) ;
#90153 = ORIENTED_EDGE ( 'NONE', *, *, #4009, .T. ) ;
#90154 = ORIENTED_EDGE ( 'NONE', *, *, #14812, .F. ) ;
#90155 = EDGE_LOOP ( 'NONE', ( #93004, #113501, #53012, #131778 ) ) ;
#90156 = EDGE_CURVE ( 'NONE', #120604, #111726, #113235, .T. ) ;
#90157 = ADVANCED_FACE ( 'NONE', ( #136420 ), #58212, .F. ) ;
#90158 = CARTESIAN_POINT ( 'NONE',  ( 30.62543019189810423, 5.291415217122919401, 3.055000000000002824 ) ) ;
#90159 = ORIENTED_EDGE ( 'NONE', *, *, #122059, .T. ) ;
#90160 = CARTESIAN_POINT ( 'NONE',  ( 16.17183060077635659, -14.24070752338414003, 4.000000000000000000 ) ) ;
#90161 = ADVANCED_FACE ( 'NONE', ( #79956 ), #5166, .F. ) ;
#90162 = DIRECTION ( 'NONE',  ( -0.7071067811865486830, -0.7071067811865464625, 0.000000000000000000 ) ) ;
#90163 = CARTESIAN_POINT ( 'NONE',  ( 2.546236474768552860, -7.934999999999990727, 4.858786175617117713E-16 ) ) ;
#90164 = LINE ( 'NONE', #67003, #30991 ) ;
#90165 = ORIENTED_EDGE ( 'NONE', *, *, #38511, .F. ) ;
#90166 = DIRECTION ( 'NONE',  ( -0.000000000000000000, 0.3543493200069153248, 0.9351131265310292928 ) ) ;
#90167 = FACE_OUTER_BOUND ( 'NONE', #136724, .T. ) ;
#90168 = CARTESIAN_POINT ( 'NONE',  ( 16.49999999999988987, 15.05218569542901186, 5.000000000000000000 ) ) ;
#90169 = EDGE_CURVE ( 'NONE', #140659, #111351, #112536, .T. ) ;
#90171 = ORIENTED_EDGE ( 'NONE', *, *, #113116, .T. ) ;
#90170 = DIRECTION ( 'NONE',  ( -0.7071067811865486830, -0.7071067811865464625, -0.000000000000000000 ) ) ;
#90172 = VERTEX_POINT ( 'NONE', #92192 ) ;
#90173 = PRESENTATION_STYLE_ASSIGNMENT (( #67763 ) ) ;
#90174 = CARTESIAN_POINT ( 'NONE',  ( 24.98911971346034022, -22.02621442084247505, 4.990779571109222879 ) ) ;
#90175 = CARTESIAN_POINT ( 'NONE',  ( 0.000000000000000000, 0.000000000000000000, 5.000000000000000000 ) ) ;
#90176 = EDGE_LOOP ( 'NONE', ( #79442, #130379, #84659, #36128 ) ) ;
#90177 = CARTESIAN_POINT ( 'NONE',  ( 8.671830600776413434, -21.74070752338406365, 4.000000000000000000 ) ) ;
#90178 = LINE ( 'NONE', #136531, #50222 ) ;
#90179 = CARTESIAN_POINT ( 'NONE',  ( 34.92499999999998295, 0.006123077391964604210, 4.000000000000000000 ) ) ;
#90180 =( LENGTH_UNIT ( ) NAMED_UNIT ( * ) SI_UNIT ( .MILLI., .METRE. ) );
#90181 = CARTESIAN_POINT ( 'NONE',  ( -5.206660635421487271, 21.75929247661549937, 4.998822639870708073 ) ) ;
#90182 = EDGE_CURVE ( 'NONE', #45676, #11432, #26253, .T. ) ;
#90183 = VECTOR ( 'NONE', #63292, 1000.000000000000000 ) ;
#90184 = VECTOR ( 'NONE', #139630, 1000.000000000000000 ) ;
#90185 = VECTOR ( 'NONE', #51434, 1000.000000000000000 ) ;
#90186 = DIRECTION ( 'NONE',  ( -0.000000000000000000, -0.3543493200069152693, 0.9351131265310292928 ) ) ;
#90187 = DIRECTION ( 'NONE',  ( -0.7071067811865486830, 0.7071067811865464625, 0.000000000000000000 ) ) ;
#90188 = LINE ( 'NONE', #110492, #79259 ) ;
#90189 = AXIS2_PLACEMENT_3D ( 'NONE', #70226, #115769, #135451 ) ;
#90190 = CARTESIAN_POINT ( 'NONE',  ( -13.49999999999990763, -2.947814304570798960, 5.000000000000000000 ) ) ;
#90191 = DIRECTION ( 'NONE',  ( -0.7071067811865487940, 0.7071067811865463515, -0.000000000000000000 ) ) ;
#90192 = ORIENTED_EDGE ( 'NONE', *, *, #3389, .T. ) ;
#90193 = EDGE_CURVE ( 'NONE', #69532, #49090, #24806, .T. ) ;
#90194 = VERTEX_POINT ( 'NONE', #35004 ) ;
#90195 = EDGE_CURVE ( 'NONE', #54251, #42897, #57471, .T. ) ;
#90196 = DIRECTION ( 'NONE',  ( 0.6830127018922181881, 0.6830127018922202975, -0.2588190451025214056 ) ) ;
#90197 = DIRECTION ( 'NONE',  ( -1.000000000000000000, -1.224606353822377258E-16, -0.000000000000000000 ) ) ;
#90198 = ADVANCED_FACE ( 'NONE', ( #101653 ), #2310, .F. ) ;
#90199 = CARTESIAN_POINT ( 'NONE',  ( 0.000000000000000000, 21.72500000000000142, 4.500000000000000888 ) ) ;
#90200 = LINE ( 'NONE', #133724, #122286 ) ;
#90201 = EDGE_LOOP ( 'NONE', ( #118268, #79728, #22118, #4383 ) ) ;
#90202 = AXIS2_PLACEMENT_3D ( 'NONE', #32815, #74900, #31369 ) ;
#90203 = DIRECTION ( 'NONE',  ( 0.000000000000000000, 0.000000000000000000, 1.000000000000000000 ) ) ;
#90204 = CARTESIAN_POINT ( 'NONE',  ( 5.999999999999956479, -19.22509904557635707, 1.855685503482192189 ) ) ;
#90205 = FACE_OUTER_BOUND ( 'NONE', #122437, .T. ) ;
#90206 = VERTEX_POINT ( 'NONE', #3050 ) ;
#90207 = CARTESIAN_POINT ( 'NONE',  ( 2.999999999999999112, -7.600000000000055600, -28.92499999999998650 ) ) ;
#90208 = DIRECTION ( 'NONE',  ( 0.7071067811865487940, 0.7071067811865463515, 0.000000000000000000 ) ) ;
#90209 = AXIS2_PLACEMENT_3D ( 'NONE', #32671, #20325, #21781 ) ;
#90210 = AXIS2_PLACEMENT_3D ( 'NONE', #132056, #55202, #111721 ) ;
#90211 = CARTESIAN_POINT ( 'NONE',  ( -0.2997448713915885632, -27.71228299555206220, 4.000000000000000000 ) ) ;
#90212 = CARTESIAN_POINT ( 'NONE',  ( 52.26626352523145158, 4.472830434245839371, -4.472830434245839371 ) ) ;
#90213 =( BOUNDED_CURVE ( )  B_SPLINE_CURVE ( 3, ( #85402, #94144, #8526, #138381 ),
 .UNSPECIFIED., .F., .T. ) 
 B_SPLINE_CURVE_WITH_KNOTS ( ( 4, 4 ),
 ( 1.208578181583236821, 1.359146454359470901 ),
 .UNSPECIFIED. ) 
 CURVE ( )  GEOMETRIC_REPRESENTATION_ITEM ( )  RATIONAL_B_SPLINE_CURVE ( ( 1.000000000000000000, 0.9981116584018945304, 0.9981116584018945304, 1.000000000000000000 ) ) 
 REPRESENTATION_ITEM ( '' )  );
#90214 = LINE ( 'NONE', #57617, #83527 ) ;
#90215 = LINE ( 'NONE', #134456, #23259 ) ;
#90216 = CARTESIAN_POINT ( 'NONE',  ( 25.82816939922335209, 12.75929247661558819, 4.000000000000000000 ) ) ;
#90217 = VERTEX_POINT ( 'NONE', #124127 ) ;
#90218 = DIRECTION ( 'NONE',  ( 0.7071067811865487940, 0.7071067811865463515, 0.000000000000000000 ) ) ;
#90219 = VERTEX_POINT ( 'NONE', #46628 ) ;
#90220 = DIRECTION ( 'NONE',  ( -0.5735764363510501562, 0.8191520442889890230, 1.003171929053521419E-16 ) ) ;
#90221 = VECTOR ( 'NONE', #9484, 1000.000000000000227 ) ;
#90222 = AXIS2_PLACEMENT_3D ( 'NONE', #73326, #116805, #37849 ) ;
#90223 = AXIS2_PLACEMENT_3D ( 'NONE', #24438, #125186, #46968 ) ;
#90224 = CARTESIAN_POINT ( 'NONE',  ( -57.29974487139158157, -27.71228299555246011, 4.000000000000000000 ) ) ;
#90225 = LINE ( 'NONE', #111247, #44270 ) ;
#90226 = CARTESIAN_POINT ( 'NONE',  ( 19.74845587132413272, -11.24070752338416135, 10.39518518046004658 ) ) ;
#90227 = LINE ( 'NONE', #101823, #104317 ) ;
#90228 = VECTOR ( 'NONE', #59394, 999.9999999999998863 ) ;
#90229 = ORIENTED_EDGE ( 'NONE', *, *, #63335, .F. ) ;
#90230 = EDGE_LOOP ( 'NONE', ( #107063, #43152, #76370, #17313 ) ) ;
#90231 = DIRECTION ( 'NONE',  ( -0.7071067811865486830, -0.7071067811865464625, 0.000000000000000000 ) ) ;
#90232 =( LENGTH_UNIT ( ) NAMED_UNIT ( * ) SI_UNIT ( .MILLI., .METRE. ) );
#90233 = AXIS2_PLACEMENT_3D ( 'NONE', #127898, #70678, #59784 ) ;
#90234 = CARTESIAN_POINT ( 'NONE',  ( -15.79289321881334551, 12.75929247661558641, 5.000000000000000000 ) ) ;
#90235 = LINE ( 'NONE', #68522, #122151 ) ;
#90236 = CARTESIAN_POINT ( 'NONE',  ( 75.76669371712954160, -7.949999999999999289, 2.130196079827424427 ) ) ;
#90237 = DIRECTION ( 'NONE',  ( 0.6830127018922180770, -0.6830127018922204085, -0.2588190451025213501 ) ) ;
#90238 = DIRECTION ( 'NONE',  ( 0.6830127018922181881, 0.6830127018922202975, -0.2588190451025214056 ) ) ;
#90239 = ORIENTED_EDGE ( 'NONE', *, *, #36800, .F. ) ;
#90240 = CARTESIAN_POINT ( 'NONE',  ( 74.93750000000000000, 5.819803920172573974, -5.819803920172572198 ) ) ;
#90241 = FACE_OUTER_BOUND ( 'NONE', #104193, .T. ) ;
#90242 = MANIFOLD_SOLID_BREP ( 'Fillet5', #113437 ) ;
#90243 = LINE ( 'NONE', #35907, #60151 ) ;
#90244 = DIRECTION ( 'NONE',  ( -1.000000000000000000, -0.000000000000000000, -0.000000000000000000 ) ) ;
#90245 = AXIS2_PLACEMENT_3D ( 'NONE', #90971, #27827, #15486 ) ;
#90246 = ORIENTED_EDGE ( 'NONE', *, *, #2802, .T. ) ;
#90247 = PLANE ( 'NONE',  #35270 ) ;
#90248 = DIRECTION ( 'NONE',  ( -1.000000000000000000, -1.224606353822377258E-16, -0.000000000000000000 ) ) ;
#90249 = CARTESIAN_POINT ( 'NONE',  ( 67.81293019189807580, -1.637169565754159617, -6.110000000000001208 ) ) ;
#90250 = ORIENTED_EDGE ( 'NONE', *, *, #17937, .T. ) ;
#90251 = VERTEX_POINT ( 'NONE', #137157 ) ;
#90252 = AXIS2_PLACEMENT_3D ( 'NONE', #87147, #6678, #84323 ) ;
#90253 = CARTESIAN_POINT ( 'NONE',  ( 4.969723521325230209, 4.202752102959690472E-16, 0.000000000000000000 ) ) ;
#90254 = CARTESIAN_POINT ( 'NONE',  ( -31.49999999999978684, 3.073033219394599058, -6.593910359671041554 ) ) ;
#90255 = LINE ( 'NONE', #79447, #53258 ) ;
#90256 = EDGE_CURVE ( 'NONE', #142977, #42748, #135043, .T. ) ;
#90258 = ORIENTED_EDGE ( 'NONE', *, *, #74694, .F. ) ;
#90257 = CARTESIAN_POINT ( 'NONE',  ( -25.39999999999996305, 0.000000000000000000, 0.000000000000000000 ) ) ;
#90259 = EDGE_CURVE ( 'NONE', #135515, #135619, #142370, .T. ) ;
#90260 = CARTESIAN_POINT ( 'NONE',  ( 59.99451991528749772, 28.92564299267980132, 4.000000000000000000 ) ) ;
#90261 = DIRECTION ( 'NONE',  ( -0.7071067811865486830, -0.7071067811865464625, 0.000000000000000000 ) ) ;
#90262 = LINE ( 'NONE', #78688, #95736 ) ;
#90263 =( LENGTH_UNIT ( ) NAMED_UNIT ( * ) SI_UNIT ( .MILLI., .METRE. ) );
#90264 = ORIENTED_EDGE ( 'NONE', *, *, #53526, .T. ) ;
#90265 = ORIENTED_EDGE ( 'NONE', *, *, #106962, .T. ) ;
#90266 = CARTESIAN_POINT ( 'NONE',  ( 54.25043019189811133, 3.055000000000002824, -5.291415217122919401 ) ) ;
#90267 = ORIENTED_EDGE ( 'NONE', *, *, #34099, .T. ) ;
#90268 = EDGE_CURVE ( 'NONE', #24066, #116804, #50855, .T. ) ;
#90269 = PLANE ( 'NONE',  #38353 ) ;
#90270 = DIRECTION ( 'NONE',  ( 0.7071067811865486830, -0.7071067811865464625, -0.000000000000000000 ) ) ;
#90271 = LINE ( 'NONE', #2530, #84975 ) ;
#90272 = DIRECTION ( 'NONE',  ( -0.7071067811865486830, -0.7071067811865464625, 0.000000000000000000 ) ) ;
#90273 = LINE ( 'NONE', #79466, #15449 ) ;
#90274 = ORIENTED_EDGE ( 'NONE', *, *, #71290, .F. ) ;
#90275 = ORIENTED_EDGE ( 'NONE', *, *, #31078, .F. ) ;
#90276 = DIRECTION ( 'NONE',  ( -0.3543493200069162685, -0.000000000000000000, -0.9351131265310288487 ) ) ;
#90277 = CARTESIAN_POINT ( 'NONE',  ( -16.82844983938008454, -0.2153006699122482492, -34.28771444467989937 ) ) ;
#90278 = EDGE_CURVE ( 'NONE', #53667, #132228, #137880, .T. ) ;
#90280 = ORIENTED_EDGE ( 'NONE', *, *, #114142, .T. ) ;
#90279 = VECTOR ( 'NONE', #7617, 999.9999999999998863 ) ;
#90281 = LINE ( 'NONE', #114864, #7397 ) ;
#90282 = DIRECTION ( 'NONE',  ( 0.6830127018922180770, -0.6830127018922204085, -0.2588190451025213501 ) ) ;
#90283 = CARTESIAN_POINT ( 'NONE',  ( 13.49999999999990052, 22.22500000000000142, 4.362957392718788796 ) ) ;
#90285 = EDGE_CURVE ( 'NONE', #142977, #67716, #84227, .T. ) ;
#90284 = VECTOR ( 'NONE', #84828, 999.9999999999998863 ) ;
#90286 = VECTOR ( 'NONE', #10835, 1000.000000000000227 ) ;
#90288 = EDGE_CURVE ( 'NONE', #55364, #76579, #110028, .T. ) ;
#90287 = VECTOR ( 'NONE', #105854, 999.9999999999998863 ) ;
#90289 = ORIENTED_EDGE ( 'NONE', *, *, #89769, .T. ) ;
#90290 = FACE_BOUND ( 'NONE', #126399, .T. ) ;
#90291 = LINE ( 'NONE', #134545, #114980 ) ;
#90292 = CARTESIAN_POINT ( 'NONE',  ( 36.29974487139159578, -27.71228299555231445, 4.000000000000000000 ) ) ;
#90293 = CARTESIAN_POINT ( 'NONE',  ( 37.85002705046288440, -5.819803920172573086, -5.819803920172573086 ) ) ;
#90294 = VECTOR ( 'NONE', #46802, 1000.000000000000000 ) ;
#90295 = LINE ( 'NONE', #3951, #87426 ) ;
#90296 = DIRECTION ( 'NONE',  ( -0.7071067811865487940, 0.7071067811865463515, -0.000000000000000000 ) ) ;
#90297 = DIRECTION ( 'NONE',  ( -1.224646799147353207E-16, 1.665334536937735304E-16, -1.000000000000000000 ) ) ;
#90298 = ORIENTED_EDGE ( 'NONE', *, *, #98675, .T. ) ;
#90299 = ORIENTED_EDGE ( 'NONE', *, *, #68959, .T. ) ;
#90300 = CARTESIAN_POINT ( 'NONE',  ( 103.8912635252314516, -4.472830434245838482, -4.472830434245838482 ) ) ;
#90301 = EDGE_LOOP ( 'NONE', ( #43084, #7849, #23966, #69601, #136504 ) ) ;
#90302 = DIRECTION ( 'NONE',  ( -0.3543493200069162685, -0.000000000000000000, -0.9351131265310288487 ) ) ;
#90303 = ORIENTED_EDGE ( 'NONE', *, *, #141389, .T. ) ;
#90304 = ADVANCED_FACE ( 'NONE', ( #120914 ), #128424, .F. ) ;
#90305 = VECTOR ( 'NONE', #86118, 1000.000000000000227 ) ;
#90306 = VECTOR ( 'NONE', #55679, 1000.000000000000000 ) ;
#90307 = DIRECTION ( 'NONE',  ( -0.7071067811865487940, 0.7071067811865463515, 0.000000000000000000 ) ) ;
#90308 = CARTESIAN_POINT ( 'NONE',  ( 12.48921356237309155, -27.52281430457064104, 5.000000000000000000 ) ) ;
#90309 = EDGE_CURVE ( 'NONE', #116082, #135321, #97742, .T. ) ;
#90310 = EDGE_CURVE ( 'NONE', #90465, #37645, #16792, .T. ) ;
#90311 = AXIS2_PLACEMENT_3D ( 'NONE', #117007, #127166, #6067 ) ;
#90312 = LINE ( 'NONE', #25046, #91081 ) ;
#90313 = ORIENTED_EDGE ( 'NONE', *, *, #4816, .T. ) ;
#90314 = DIRECTION ( 'NONE',  ( 0.3543493200069162685, -0.000000000000000000, -0.9351131265310288487 ) ) ;
#90315 = CARTESIAN_POINT ( 'NONE',  ( -54.48921356237310221, -27.52281430457093236, 5.000000000000000000 ) ) ;
#90316 = PLANE ( 'NONE',  #133455 ) ;
#90317 = DIRECTION ( 'NONE',  ( 0.7071067811865487940, 0.7071067811865463515, 0.000000000000000000 ) ) ;
#90318 = CARTESIAN_POINT ( 'NONE',  ( 68.37499999999998579, 7.950000000000000178, 1.460391307983218535E-15 ) ) ;
#90319 = AXIS2_PLACEMENT_3D ( 'NONE', #43894, #88107, #132357 ) ;
#90320 = LINE ( 'NONE', #80198, #139401 ) ;
#90321 = ORIENTED_EDGE ( 'NONE', *, *, #29127, .T. ) ;
#90323 = ADVANCED_FACE ( 'NONE', ( #39276 ), #18180, .T. ) ;
#90322 = AXIS2_PLACEMENT_3D ( 'NONE', #28724, #83835, #127292 ) ;
#90324 = LINE ( 'NONE', #1152, #63534 ) ;
#90325 = DIRECTION ( 'NONE',  ( -0.5735764363510499342, -0.8191520442889891340, 0.000000000000000000 ) ) ;
#90326 = ORIENTED_EDGE ( 'NONE', *, *, #91183, .T. ) ;
#90327 = ORIENTED_EDGE ( 'NONE', *, *, #54560, .F. ) ;
#90328 = EDGE_CURVE ( 'NONE', #35419, #27726, #47514, .T. ) ;
#90329 = COLOUR_RGB ( '', 0.09019608, 0.27058824, 0.51372549) ;
#90331 = EDGE_LOOP ( 'NONE', ( #111199, #27361, #58921, #91858 ) ) ;
#90330 = EDGE_CURVE ( 'NONE', #37842, #2427, #108572, .T. ) ;
#90332 = CARTESIAN_POINT ( 'NONE',  ( 50.45876352523143282, 0.000000000000000000, -6.110000000000001208 ) ) ;
#90333 = ORIENTED_EDGE ( 'NONE', *, *, #132277, .F. ) ;
#90334 = DIRECTION ( 'NONE',  ( -0.000000000000000000, -0.3543493200069152693, 0.9351131265310292928 ) ) ;
#90335 = VECTOR ( 'NONE', #142395, 1000.000000000000000 ) ;
#90336 = CARTESIAN_POINT ( 'NONE',  ( 6.316639616203774565, -1.633150327867691987, -6.094999999999989093 ) ) ;
#90337 = CARTESIAN_POINT ( 'NONE',  ( 88.22959685856474721, -6.110000000000000320, -1.637169565754161393 ) ) ;
#90338 = DIRECTION ( 'NONE',  ( 0.000000000000000000, 0.000000000000000000, -1.000000000000000000 ) ) ;
#90339 = EDGE_CURVE ( 'NONE', #74056, #115521, #105226, .T. ) ;
#90340 = VERTEX_POINT ( 'NONE', #141986 ) ;
#90341 = DIRECTION ( 'NONE',  ( -0.000000000000000000, -1.000000000000000000, -0.000000000000000000 ) ) ;
#90342 = ORIENTED_EDGE ( 'NONE', *, *, #68787, .T. ) ;
#90343 = CARTESIAN_POINT ( 'NONE',  ( 19.49999999999985789, -16.53360074219757436, 5.000000000000000000 ) ) ;
#90344 = VECTOR ( 'NONE', #74028, 1000.000000000000227 ) ;
#90345 = EDGE_CURVE ( 'NONE', #92829, #108854, #9254, .T. ) ;
#90346 = DIRECTION ( 'NONE',  ( 0.7071067811865486830, -0.7071067811865464625, -0.000000000000000000 ) ) ;
#90347 = ORIENTED_EDGE ( 'NONE', *, *, #8204, .F. ) ;
#90348 = CARTESIAN_POINT ( 'NONE',  ( -21.22572773465412865, 22.22500000000000142, -0.1911663670286917194 ) ) ;
#90349 = DIRECTION ( 'NONE',  ( -0.3543493200069162685, -0.000000000000000000, -0.9351131265310288487 ) ) ;
#90350 = LINE ( 'NONE', #112125, #56745 ) ;
#90351 = VERTEX_POINT ( 'NONE', #53531 ) ;
#90352 = LINE ( 'NONE', #123727, #8704 ) ;
#90353 = ORIENTED_EDGE ( 'NONE', *, *, #83805, .T. ) ;
#90354 = ORIENTED_EDGE ( 'NONE', *, *, #83521, .T. ) ;
#90355 = ORIENTED_EDGE ( 'NONE', *, *, #110445, .T. ) ;
#90356 = DIRECTION ( 'NONE',  ( -0.7071067811865486830, 0.7071067811865464625, 0.000000000000000000 ) ) ;
#90357 = CIRCLE ( 'NONE', #62644, 4.749999999999997335 ) ;
#90358 = DIRECTION ( 'NONE',  ( -1.000000000000000000, -0.000000000000000000, -0.000000000000000000 ) ) ;
#90359 = CARTESIAN_POINT ( 'NONE',  ( -33.18398860626899705, 28.73617430169810305, 5.000000000000000000 ) ) ;
#90360 = DIRECTION ( 'NONE',  ( -0.7071067811865486830, -0.7071067811865464625, 0.000000000000000000 ) ) ;
#90361 = PLANE ( 'NONE',  #90582 ) ;
#90362 = VERTEX_POINT ( 'NONE', #138583 ) ;
#90363 = VECTOR ( 'NONE', #42483, 1000.000000000000227 ) ;
#90364 = DIRECTION ( 'NONE',  ( -1.000000000000000000, -0.000000000000000000, -0.000000000000000000 ) ) ;
#90365 = EDGE_CURVE ( 'NONE', #31098, #35930, #105914, .T. ) ;
#90366 = ADVANCED_FACE ( 'NONE', ( #17497, #83499 ), #94347, .T. ) ;
#90367 = CARTESIAN_POINT ( 'NONE',  ( 24.18706980810188867, -2.126176841940956130, 7.934999999999991616 ) ) ;
#90368 = CARTESIAN_POINT ( 'NONE',  ( -21.18398860626899349, 28.73617430169802134, 5.000000000000000000 ) ) ;
#90369 = DIRECTION ( 'NONE',  ( -0.000000000000000000, 0.000000000000000000, 1.000000000000000000 ) ) ;
#90370 =( BOUNDED_CURVE ( )  B_SPLINE_CURVE ( 3, ( #18795, #30408, #137757, #29667 ),
 .UNSPECIFIED., .F., .T. ) 
 B_SPLINE_CURVE_WITH_KNOTS ( ( 4, 4 ),
 ( 1.864375635226932282, 1.933014472006565176 ),
 .UNSPECIFIED. ) 
 CURVE ( )  GEOMETRIC_REPRESENTATION_ITEM ( )  RATIONAL_B_SPLINE_CURVE ( ( 1.000000000000000000, 0.9996074310407762065, 0.9996074310407762065, 1.000000000000000000 ) ) 
 REPRESENTATION_ITEM ( '' )  );
#90372 = EDGE_CURVE ( 'NONE', #110816, #119393, #89716, .T. ) ;
#90371 = CARTESIAN_POINT ( 'NONE',  ( 19.17183060077633172, -17.24070752338411339, 4.000000000000000000 ) ) ;
#90373 = ORIENTED_EDGE ( 'NONE', *, *, #16436, .F. ) ;
#90374 = ORIENTED_EDGE ( 'NONE', *, *, #53543, .T. ) ;
#90375 = VERTEX_POINT ( 'NONE', #66550 ) ;
#90376 = LINE ( 'NONE', #2638, #99632 ) ;
#90377 = DIRECTION ( 'NONE',  ( 0.7071067811865486830, -0.7071067811865464625, -0.000000000000000000 ) ) ;
#90378 = DIRECTION ( 'NONE',  ( 1.000000000000000000, -0.000000000000000000, -0.000000000000000000 ) ) ;
#90380 = EDGE_CURVE ( 'NONE', #92320, #127894, #57838, .T. ) ;
#90379 = VECTOR ( 'NONE', #27260, 1000.000000000000000 ) ;
#90381 = PLANE ( 'NONE',  #73707 ) ;
#90382 = CARTESIAN_POINT ( 'NONE',  ( -25.49999999999982236, 1.030536316426491128, -5.498701923753738896 ) ) ;
#90383 = VECTOR ( 'NONE', #33311, 1000.000000000000227 ) ;
#90384 = VECTOR ( 'NONE', #28615, 1000.000000000000227 ) ;
#90385 = LINE ( 'NONE', #3353, #29883 ) ;
#90386 = LINE ( 'NONE', #12811, #45653 ) ;
#90387 = LINE ( 'NONE', #125159, #333 ) ;
#90388 = CARTESIAN_POINT ( 'NONE',  ( 13.49999999999990585, -10.53360074219763121, 5.000000000000000000 ) ) ;
#90389 = DIRECTION ( 'NONE',  ( -0.000000000000000000, 0.000000000000000000, 1.000000000000000000 ) ) ;
#90390 = ORIENTED_EDGE ( 'NONE', *, *, #78922, .T. ) ;
#90391 = VECTOR ( 'NONE', #126038, 1000.000000000000227 ) ;
#90392 = VECTOR ( 'NONE', #125172, 999.9999999999998863 ) ;
#90393 = VECTOR ( 'NONE', #81859, 999.9999999999998863 ) ;
#90394 = PRESENTATION_LAYER_ASSIGNMENT (  '', '', ( #4984 ) ) ;
#90395 = ORIENTED_EDGE ( 'NONE', *, *, #93138, .T. ) ;
#90396 = STYLED_ITEM ( 'NONE', ( #25253 ), #114939 ) ;
#90397 = CARTESIAN_POINT ( 'NONE',  ( 5.292893218813418343, -3.740707523384243505, 5.000000000000000000 ) ) ;
#90399 = VERTEX_POINT ( 'NONE', #68023 ) ;
#90398 = CARTESIAN_POINT ( 'NONE',  ( -34.49999999999975842, 15.05432934483078533, 4.994342998332167660 ) ) ;
#90400 = LINE ( 'NONE', #134647, #91207 ) ;
#90401 = VERTEX_POINT ( 'NONE', #133251 ) ;
#90402 = CARTESIAN_POINT ( 'NONE',  ( 152.4000000000000057, -17.48000000000005016, 34.92499999999998295 ) ) ;
#90403 = ORIENTED_EDGE ( 'NONE', *, *, #51989, .T. ) ;
#90404 = FACE_OUTER_BOUND ( 'NONE', #98794, .T. ) ;
#90405 = AXIS2_PLACEMENT_3D ( 'NONE', #103600, #126785, #51401 ) ;
#90406 = ORIENTED_EDGE ( 'NONE', *, *, #8217, .T. ) ;
#90407 =( BOUNDED_CURVE ( )  B_SPLINE_CURVE ( 3, ( #42789, #76853, #121028, #31889 ),
 .UNSPECIFIED., .F., .F. ) 
 B_SPLINE_CURVE_WITH_KNOTS ( ( 4, 4 ),
 ( 5.143245962375958769, 6.645403452391247079 ),
 .UNSPECIFIED. ) 
 CURVE ( )  GEOMETRIC_REPRESENTATION_ITEM ( )  RATIONAL_B_SPLINE_CURVE ( ( 1.000000000000000000, 0.8206354192515226131, 0.8206354192515226131, 1.000000000000000000 ) ) 
 REPRESENTATION_ITEM ( '' )  );
#90408 = CARTESIAN_POINT ( 'NONE',  ( -59.99451991528749772, 28.92564299267980132, 4.000000000000000000 ) ) ;
#90409 = CARTESIAN_POINT ( 'NONE',  ( 99.53752705046289861, -9.735942053221456900E-16, 7.949999999999998401 ) ) ;
#90410 = DIRECTION ( 'NONE',  ( 0.7071067811865487940, -0.7071067811865463515, 0.000000000000000000 ) ) ;
#90411 = PLANE ( 'NONE',  #90223 ) ;
#90412 = ORIENTED_EDGE ( 'NONE', *, *, #127140, .T. ) ;
#90413 = SURFACE_STYLE_USAGE ( .BOTH. , #77435 ) ;
#90414 = LINE ( 'NONE', #24441, #72762 ) ;
#90415 = EDGE_CURVE ( 'NONE', #74158, #141302, #77453, .T. ) ;
#90416 = PLANE ( 'NONE',  #25242 ) ;
#90417 = CARTESIAN_POINT ( 'NONE',  ( 9.770833333333335702, 6.094999999999991758, 1.633150327867687102 ) ) ;
#90419 = AXIS2_PLACEMENT_3D ( 'NONE', #50630, #17959, #5668 ) ;
#90418 = LINE ( 'NONE', #134666, #109299 ) ;
#90420 = CARTESIAN_POINT ( 'NONE',  ( -12.69999999999998153, 0.000000000000000000, 0.000000000000000000 ) ) ;
#90421 = LINE ( 'NONE', #79606, #29269 ) ;
#90422 = VERTEX_POINT ( 'NONE', #22997 ) ;
#90423 = AXIS2_PLACEMENT_3D ( 'NONE', #61102, #126297, #103799 ) ;
#90424 = CARTESIAN_POINT ( 'NONE',  ( 8.816011393731004731, 28.73617430169781173, 5.000000000000000000 ) ) ;
#90425 = ORIENTED_EDGE ( 'NONE', *, *, #88874, .F. ) ;
#90426 = AXIS2_PLACEMENT_3D ( 'NONE', #34899, #24708, #112444 ) ;
#90427 = CARTESIAN_POINT ( 'NONE',  ( 97.70876352523144703, -7.482591942790329030E-16, 6.110000000000001208 ) ) ;
#90428 = VECTOR ( 'NONE', #5878, 1000.000000000000000 ) ;
#90429 = CARTESIAN_POINT ( 'NONE',  ( 29.67183060077626422, -21.74070752338406010, 4.000000000000000000 ) ) ;
#90430 = CARTESIAN_POINT ( 'NONE',  ( -34.75611968250420603, -7.294349301475856251, 4.955485411084898040 ) ) ;
#90431 = CARTESIAN_POINT ( 'NONE',  ( 122.6835989386367913, -43.15000000000001990, -34.92499999999998295 ) ) ;
#90432 = VERTEX_POINT ( 'NONE', #54970 ) ;
#90433 = VECTOR ( 'NONE', #54065, 1000.000000000000000 ) ;
#90434 = CARTESIAN_POINT ( 'NONE',  ( 0.000000000000000000, 0.000000000000000000, 5.000000000000000000 ) ) ;
#90435 = CARTESIAN_POINT ( 'NONE',  ( -34.75611968250420603, -13.29434930147579941, 4.955485411084898040 ) ) ;
#90436 = EDGE_CURVE ( 'NONE', #32991, #69078, #122320, .T. ) ;
#90437 = DIRECTION ( 'NONE',  ( 0.6830127018922181881, 0.6830127018922202975, -0.2588190451025214056 ) ) ;
#90438 = ORIENTED_EDGE ( 'NONE', *, *, #113604, .T. ) ;
#90439 = CARTESIAN_POINT ( 'NONE',  ( 24.79593897580385331, 4.791522900035168675, 4.000000000000000000 ) ) ;
#90440 = ADVANCED_FACE ( 'NONE', ( #112204 ), #12850, .F. ) ;
#90441 = ADVANCED_FACE ( 'NONE', ( #1945 ), #132556, .F. ) ;
#90442 = VECTOR ( 'NONE', #143164, 1000.000000000000000 ) ;
#90443 = DIRECTION ( 'NONE',  ( 1.000000000000000000, 0.000000000000000000, 0.000000000000000000 ) ) ;
#90445 = ORIENTED_EDGE ( 'NONE', *, *, #45655, .T. ) ;
#90444 = LINE ( 'NONE', #80309, #40537 ) ;
#90446 = DIRECTION ( 'NONE',  ( -1.000000000000000000, 0.000000000000000000, 0.000000000000000000 ) ) ;
#90447 = CARTESIAN_POINT ( 'NONE',  ( 101.4333603837962414, 2.130196079827431532, -7.949999999999996625 ) ) ;
#90448 = CARTESIAN_POINT ( 'NONE',  ( 0.000000000000000000, 0.000000000000000000, 0.000000000000000000 ) ) ;
#90449 = LINE ( 'NONE', #562, #57244 ) ;
#90450 = LINE ( 'NONE', #137533, #128017 ) ;
#90451 = ADVANCED_FACE ( 'NONE', ( #46253 ), #1256, .T. ) ;
#90453 = VERTEX_POINT ( 'NONE', #33929 ) ;
#90452 = EDGE_CURVE ( 'NONE', #129956, #85957, #550, .T. ) ;
#90454 = ORIENTED_EDGE ( 'NONE', *, *, #50202, .F. ) ;
#90455 = ORIENTED_EDGE ( 'NONE', *, *, #63621, .F. ) ;
#90456 = CARTESIAN_POINT ( 'NONE',  ( 84.43793019189811844, -6.110000000000001208, 1.637169565754158951 ) ) ;
#90457 = COLOUR_RGB ( '', 0.66274510, 0.83137255, 0.94901961) ;
#90458 = ORIENTED_EDGE ( 'NONE', *, *, #33006, .T. ) ;
#90459 = EDGE_CURVE ( 'NONE', #39260, #41530, #123802, .T. ) ;
#90460 = DIRECTION ( 'NONE',  ( -0.7071067811865486830, -0.7071067811865464625, 0.000000000000000000 ) ) ;
#90461 = LINE ( 'NONE', #55707, #13246 ) ;
#90462 = VECTOR ( 'NONE', #75463, 1000.000000000000227 ) ;
#90463 = FACE_OUTER_BOUND ( 'NONE', #63625, .T. ) ;
#90464 = FACE_OUTER_BOUND ( 'NONE', #108074, .T. ) ;
#90465 = VERTEX_POINT ( 'NONE', #68704 ) ;
#90466 = DIRECTION ( 'NONE',  ( 1.055184596092948005E-16, -1.000000000000000000, 0.000000000000000000 ) ) ;
#90467 = CARTESIAN_POINT ( 'NONE',  ( -11.99451991528749417, 28.92564299267946382, 4.000000000000000000 ) ) ;
#90468 = ADVANCED_FACE ( 'NONE', ( #99137 ), #110722, .F. ) ;
#90469 = CYLINDRICAL_SURFACE ( 'NONE', #90507, 2.500000000000000444 ) ;
#90470 = CARTESIAN_POINT ( 'NONE',  ( 83.91209685856479439, 5.291415217122921177, -3.054999999999994831 ) ) ;
#90471 = VERTEX_POINT ( 'NONE', #55685 ) ;
#90472 = CARTESIAN_POINT ( 'NONE',  ( 2.999999999999999112, -7.600000000000055600, -34.92499999999998295 ) ) ;
#90473 = ADVANCED_FACE ( 'NONE', ( #115727 ), #27318, .F. ) ;
#90474 = CARTESIAN_POINT ( 'NONE',  ( 2.292893218813448986, -12.74070752338415247, 5.000000000000000000 ) ) ;
#90475 = VECTOR ( 'NONE', #30099, 1000.000000000000000 ) ;
#90476 = EDGE_CURVE ( 'NONE', #79668, #99063, #5563, .T. ) ;
#90477 = ORIENTED_EDGE ( 'NONE', *, *, #142448, .T. ) ;
#90478 = EDGE_LOOP ( 'NONE', ( #61488, #61966, #133378, #110950 ) ) ;
#90479 = CARTESIAN_POINT ( 'NONE',  ( -4.499999999999976019, -8.568876922607730151, 4.000000000000000000 ) ) ;
#90480 = CYLINDRICAL_SURFACE ( 'NONE', #24670, 6.094999999999989093 ) ;
#90481 = CARTESIAN_POINT ( 'NONE',  ( 19.49999999999986500, -4.533600742197692490, 5.000000000000000000 ) ) ;
#90482 = EDGE_CURVE ( 'NONE', #123934, #86133, #70182, .T. ) ;
#90483 = AXIS2_PLACEMENT_3D ( 'NONE', #27649, #60321, #103765 ) ;
#90484 = VECTOR ( 'NONE', #73278, 1000.000000000000000 ) ;
#90485 = FACE_OUTER_BOUND ( 'NONE', #90728, .T. ) ;
#90486 = DIRECTION ( 'NONE',  ( 1.000000000000000000, 0.000000000000000000, 0.000000000000000000 ) ) ;
#90487 = DIRECTION ( 'NONE',  ( 0.6830127018922181881, 0.6830127018922202975, -0.2588190451025214056 ) ) ;
#90488 = ORIENTED_EDGE ( 'NONE', *, *, #70403, .F. ) ;
#90489 = VERTEX_POINT ( 'NONE', #28057 ) ;
#90490 = CARTESIAN_POINT ( 'NONE',  ( 0.000000000000000000, 0.000000000000000000, 5.000000000000000000 ) ) ;
#90491 = ORIENTED_EDGE ( 'NONE', *, *, #73206, .F. ) ;
#90492 = ORIENTED_EDGE ( 'NONE', *, *, #55455, .F. ) ;
#90493 = ADVANCED_FACE ( 'NONE', ( #115021 ), #70868, .F. ) ;
#90494 = AXIS2_PLACEMENT_3D ( 'NONE', #60297, #49430, #1738 ) ;
#90496 = EDGE_CURVE ( 'NONE', #128364, #25807, #137541, .T. ) ;
#90495 = VECTOR ( 'NONE', #101922, 1000.000000000000227 ) ;
#90497 = VECTOR ( 'NONE', #93329, 999.9999999999998863 ) ;
#90498 = LINE ( 'NONE', #14357, #93748 ) ;
#90499 = EDGE_LOOP ( 'NONE', ( #76812, #79240, #29748, #130210 ) ) ;
#90500 = PLANE ( 'NONE',  #106096 ) ;
#90501 = CARTESIAN_POINT ( 'NONE',  ( -17.90332935812583770, -2.240707523384257716, 15.26439735382748353 ) ) ;
#90502 = ADVANCED_FACE ( 'NONE', ( #128101 ), #15016, .T. ) ;
#90503 = DIRECTION ( 'NONE',  ( 0.7071067811865486830, -0.7071067811865464625, -0.000000000000000000 ) ) ;
#90504 = VECTOR ( 'NONE', #7436, 1000.000000000000000 ) ;
#90505 = CIRCLE ( 'NONE', #72012, 2.500000000000000888 ) ;
#90506 = VECTOR ( 'NONE', #114623, 1000.000000000000000 ) ;
#90507 = AXIS2_PLACEMENT_3D ( 'NONE', #134715, #89744, #78175 ) ;
#90508 = LINE ( 'NONE', #104934, #35192 ) ;
#90509 = ORIENTED_EDGE ( 'NONE', *, *, #116309, .F. ) ;
#90510 = ADVANCED_FACE ( 'NONE', ( #60725 ), #83895, .F. ) ;
#90511 = VECTOR ( 'NONE', #120638, 1000.000000000000000 ) ;
#90512 = DIRECTION ( 'NONE',  ( 0.000000000000000000, 0.000000000000000000, -1.000000000000000000 ) ) ;
#90513 = ORIENTED_EDGE ( 'NONE', *, *, #3443, .T. ) ;
#90514 = DIRECTION ( 'NONE',  ( 0.7071067811865487940, 0.7071067811865463515, 0.000000000000000000 ) ) ;
#90515 = ORIENTED_EDGE ( 'NONE', *, *, #80792, .F. ) ;
#90516 = CARTESIAN_POINT ( 'NONE',  ( 116.1625270504628986, 7.949999999999998401, 1.460391307983218338E-15 ) ) ;
#90517 = ORIENTED_EDGE ( 'NONE', *, *, #97128, .F. ) ;
#90518 = LINE ( 'NONE', #93362, #34332 ) ;
#90519 = EDGE_LOOP ( 'NONE', ( #96912, #94736, #42808, #35078 ) ) ;
#90520 = ORIENTED_EDGE ( 'NONE', *, *, #84339, .F. ) ;
#90521 = CIRCLE ( 'NONE', #85843, 9.119999999999999218 ) ;
#90522 = VERTEX_POINT ( 'NONE', #4091 ) ;
#90523 = CARTESIAN_POINT ( 'NONE',  ( 21.77612515620402078, -2.500000000000000000, 3.061616997868383634E-16 ) ) ;
#90524 = DIRECTION ( 'NONE',  ( 1.369518533665900312E-16, -1.000000000000000000, 0.000000000000000000 ) ) ;
#90525 = CARTESIAN_POINT ( 'NONE',  ( 33.48921356237309510, -27.52281430457078670, 5.000000000000000000 ) ) ;
#90526 = CARTESIAN_POINT ( 'NONE',  ( 121.3337635252314328, 6.110000000000001208, 1.122388791418549305E-15 ) ) ;
#90527 = PLANE ( 'NONE',  #19586 ) ;
#90529 = EDGE_CURVE ( 'NONE', #68141, #66768, #62123, .T. ) ;
#90528 = AXIS2_PLACEMENT_3D ( 'NONE', #140744, #141479, #142213 ) ;
#90530 = FACE_OUTER_BOUND ( 'NONE', #47852, .T. ) ;
#90532 = LINE ( 'NONE', #91937, #134675 ) ;
#90531 = DIRECTION ( 'NONE',  ( 0.5735764363510448272, -0.8191520442889927978, 1.003171929053526103E-16 ) ) ;
#90533 = AXIS2_PLACEMENT_3D ( 'NONE', #120864, #109287, #85380 ) ;
#90534 = ADVANCED_FACE ( 'NONE', ( #17181 ), #136810, .F. ) ;
#90535 = DIRECTION ( 'NONE',  ( -0.5735764363510501562, 0.8191520442889890230, 1.003171929053521419E-16 ) ) ;
#90536 = VECTOR ( 'NONE', #8939, 1000.000000000000000 ) ;
#90537 = DIRECTION ( 'NONE',  ( -0.000000000000000000, -0.3543493200069152693, 0.9351131265310292928 ) ) ;
#90538 = ORIENTED_EDGE ( 'NONE', *, *, #70201, .F. ) ;
#90539 = VECTOR ( 'NONE', #19131, 1000.000000000000000 ) ;
#90540 = DIRECTION ( 'NONE',  ( -1.000000000000000000, -1.224606353822377258E-16, -0.000000000000000000 ) ) ;
#90541 = CARTESIAN_POINT ( 'NONE',  ( -9.299744871391588674, -27.71228299555212971, 4.000000000000000000 ) ) ;
#90542 = EDGE_LOOP ( 'NONE', ( #16845, #60869, #73091, #64934 ) ) ;
#90543 = AXIS2_PLACEMENT_3D ( 'NONE', #141896, #109234, #9160 ) ;
#90544 = ORIENTED_EDGE ( 'NONE', *, *, #21206, .T. ) ;
#90545 = CARTESIAN_POINT ( 'NONE',  ( 15.70701326429294475, -21.74070752338405654, 4.999753212805220670 ) ) ;
#90546 = ORIENTED_EDGE ( 'NONE', *, *, #123884, .T. ) ;
#90547 = VECTOR ( 'NONE', #135703, 999.9999999999998863 ) ;
#90548 = LINE ( 'NONE', #23860, #109250 ) ;
#90549 = PLANE ( 'NONE',  #13125 ) ;
#90550 = VECTOR ( 'NONE', #134270, 999.9999999999998863 ) ;
#90551 = CARTESIAN_POINT ( 'NONE',  ( -33.48921356237309510, -27.52281430457078670, 5.000000000000000000 ) ) ;
#90552 = CARTESIAN_POINT ( 'NONE',  ( -32.24139925780183091, 21.72499999999999432, 5.000000000000000000 ) ) ;
#90553 = ADVANCED_FACE ( 'NONE', ( #116489 ), #29033, .T. ) ;
#90554 = ORIENTED_EDGE ( 'NONE', *, *, #17488, .F. ) ;
#90555 = LINE ( 'NONE', #136182, #46434 ) ;
#90556 = ORIENTED_EDGE ( 'NONE', *, *, #29664, .F. ) ;
#90557 = DIRECTION ( 'NONE',  ( -0.7071067811865486830, -0.7071067811865464625, -0.000000000000000000 ) ) ;
#90558 = EDGE_CURVE ( 'NONE', #126051, #121499, #61443, .T. ) ;
#90559 = VECTOR ( 'NONE', #122664, 999.9999999999998863 ) ;
#90560 = CARTESIAN_POINT ( 'NONE',  ( 32.29623647476855552, 7.934999999999990727, -1.457635852685135314E-15 ) ) ;
#90561 = VERTEX_POINT ( 'NONE', #107734 ) ;
#90562 = CARTESIAN_POINT ( 'NONE',  ( 80.12043019189810877, 3.055000000000002380, -5.291415217122917625 ) ) ;
#90563 = CARTESIAN_POINT ( 'NONE',  ( 60.48921356237309510, -27.52281430457097500, 5.000000000000000000 ) ) ;
#90564 = CARTESIAN_POINT ( 'NONE',  ( 98.51669371712957002, 7.950000000000000178, -2.130196079827421318 ) ) ;
#90565 = ORIENTED_EDGE ( 'NONE', *, *, #99126, .F. ) ;
#90566 = ORIENTED_EDGE ( 'NONE', *, *, #293, .F. ) ;
#90567 = VECTOR ( 'NONE', #138954, 1000.000000000000000 ) ;
#90568 = ORIENTED_EDGE ( 'NONE', *, *, #126365, .F. ) ;
#90569 = DIRECTION ( 'NONE',  ( -0.7071067811865487940, 0.7071067811865463515, 0.000000000000000000 ) ) ;
#90570 = DIRECTION ( 'NONE',  ( -0.000000000000000000, -0.3543493200069152693, 0.9351131265310292928 ) ) ;
#90571 = FACE_OUTER_BOUND ( 'NONE', #40000, .T. ) ;
#90572 = AXIS2_PLACEMENT_3D ( 'NONE', #36038, #138731, #117637 ) ;
#90573 = FACE_OUTER_BOUND ( 'NONE', #86574, .T. ) ;
#90574 = B_SPLINE_CURVE_WITH_KNOTS ( 'NONE', 3,
 ( #132677, #33368, #121736, #22415, #66677, #11533, #55812, #100015, #123390, #57410 ),
 .UNSPECIFIED., .F., .F.,
 ( 4, 2, 2, 2, 4 ),
 ( 0.000000000000000000, 0.0009358269096809158352, 0.001871653819361831670, 0.002807480729042747397, 0.003743307638723663341 ),
 .UNSPECIFIED. ) ;
#90575 = ORIENTED_EDGE ( 'NONE', *, *, #71820, .F. ) ;
#90576 = CARTESIAN_POINT ( 'NONE',  ( 80.28752705046289861, 0.000000000000000000, -7.949999999999998401 ) ) ;
#90577 = ADVANCED_FACE ( 'NONE', ( #42529 ), #86732, .T. ) ;
#90578 = CARTESIAN_POINT ( 'NONE',  ( 7.140000000000044089, -1.036479131253094653E-14, -40.00000000000000000 ) ) ;
#90580 = VECTOR ( 'NONE', #110036, 1000.000000000000000 ) ;
#90579 = PLANE ( 'NONE',  #100094 ) ;
#90581 = ORIENTED_EDGE ( 'NONE', *, *, #116649, .F. ) ;
#90582 = AXIS2_PLACEMENT_3D ( 'NONE', #81668, #38147, #69349 ) ;
#90583 = CARTESIAN_POINT ( 'NONE',  ( 12.35051985313232237, 3.061616997868383634E-16, -2.500000000000000444 ) ) ;
#90584 = ORIENTED_EDGE ( 'NONE', *, *, #54373, .F. ) ;
#90585 = VERTEX_POINT ( 'NONE', #84589 ) ;
#90586 = ORIENTED_EDGE ( 'NONE', *, *, #33248, .F. ) ;
#90587 = EDGE_CURVE ( 'NONE', #118712, #126622, #52648, .T. ) ;
#90588 = FACE_OUTER_BOUND ( 'NONE', #107968, .T. ) ;
#90589 = FACE_OUTER_BOUND ( 'NONE', #1246, .T. ) ;
#90591 = VERTEX_POINT ( 'NONE', #74432 ) ;
#90590 = CIRCLE ( 'NONE', #116009, 5.968999999999998529 ) ;
#90592 = ORIENTED_EDGE ( 'NONE', *, *, #94086, .T. ) ;
#90593 = LINE ( 'NONE', #122475, #66024 ) ;
#90594 = LINE ( 'NONE', #34789, #41611 ) ;
#90595 = CARTESIAN_POINT ( 'NONE',  ( 8.111591955682463606, 2.055000000000001048, 0.000000000000000000 ) ) ;
#90596 = LINE ( 'NONE', #47837, #32072 ) ;
#90597 = DIRECTION ( 'NONE',  ( -0.6830127018922180770, -0.6830127018922204085, -0.2588190451025213501 ) ) ;
#90598 = DIRECTION ( 'NONE',  ( 0.000000000000000000, 0.000000000000000000, -1.000000000000000000 ) ) ;
#90599 = DIRECTION ( 'NONE',  ( -0.7071067811865486830, -0.7071067811865464625, -0.000000000000000000 ) ) ;
#90600 = LINE ( 'NONE', #135539, #120104 ) ;
#90601 = CARTESIAN_POINT ( 'NONE',  ( 21.12456980810188867, -6.871911579029512218, 3.967499999999996252 ) ) ;
#90602 = CYLINDRICAL_SURFACE ( 'NONE', #18969, 2.500000000000000000 ) ;
#90603 = CARTESIAN_POINT ( 'NONE',  ( 151.4000000000000057, -16.48000000000005016, 33.92499999999998295 ) ) ;
#90604 = VECTOR ( 'NONE', #73272, 999.9999999999998863 ) ;
#90605 = DIRECTION ( 'NONE',  ( 0.7071067811865487940, 0.7071067811865463515, 0.000000000000000000 ) ) ;
#90606 = DIRECTION ( 'NONE',  ( 0.7071067811865487940, 0.7071067811865463515, 0.000000000000000000 ) ) ;
#90607 = ORIENTED_EDGE ( 'NONE', *, *, #73150, .F. ) ;
#90608 = ORIENTED_EDGE ( 'NONE', *, *, #77390, .T. ) ;
#90609 = CIRCLE ( 'NONE', #2608, 3.500000000000000444 ) ;
#90610 = CARTESIAN_POINT ( 'NONE',  ( 95.79166666666665719, 3.975000000000003642, -6.884901960086285300 ) ) ;
#90611 = VECTOR ( 'NONE', #101889, 1000.000000000000000 ) ;
#90612 = EDGE_LOOP ( 'NONE', ( #125062, #113107, #77680, #130566 ) ) ;
#90613 = ORIENTED_EDGE ( 'NONE', *, *, #107117, .F. ) ;
#90614 = ORIENTED_EDGE ( 'NONE', *, *, #110621, .T. ) ;
#90615 = EDGE_CURVE ( 'NONE', #96207, #80484, #32343, .T. ) ;
#90616 = LINE ( 'NONE', #123963, #13254 ) ;
#90617 = DIRECTION ( 'NONE',  ( 0.6830127018922180770, -0.6830127018922204085, -0.2588190451025213501 ) ) ;
#90618 = VECTOR ( 'NONE', #42803, 999.9999999999998863 ) ;
#90619 = AXIS2_PLACEMENT_3D ( 'NONE', #100929, #78481, #44450 ) ;
#90620 = AXIS2_PLACEMENT_3D ( 'NONE', #128901, #87556, #85390 ) ;
#90621 = AXIS2_PLACEMENT_3D ( 'NONE', #60908, #115914, #62300 ) ;
#90622 = CARTESIAN_POINT ( 'NONE',  ( 14.55557268365555679, 9.434219313260308937, -1.151903651517597549 ) ) ;
#90623 = ORIENTED_EDGE ( 'NONE', *, *, #38939, .T. ) ;
#90624 = DIRECTION ( 'NONE',  ( -0.7071067811865486830, -0.7071067811865464625, 0.000000000000000000 ) ) ;
#90625 = AXIS2_PLACEMENT_3D ( 'NONE', #59548, #70449, #56716 ) ;
#90626 = PLANE ( 'NONE',  #95100 ) ;
#90627 = DIRECTION ( 'NONE',  ( -0.7071067811865486830, -0.7071067811865464625, -0.000000000000000000 ) ) ;
#90628 = CARTESIAN_POINT ( 'NONE',  ( -7.499999999999944045, -19.53360074219753884, 5.000000000000000000 ) ) ;
#90629 = EDGE_CURVE ( 'NONE', #93458, #84994, #62845, .T. ) ;
#90630 = EDGE_CURVE ( 'NONE', #18836, #42793, #120758, .T. ) ;
#90631 = LINE ( 'NONE', #47173, #48845 ) ;
#90632 = DIRECTION ( 'NONE',  ( -0.7071067811865486830, -0.7071067811865464625, 0.000000000000000000 ) ) ;
#90633 = CARTESIAN_POINT ( 'NONE',  ( 25.39999999999999858, -14.29000000000013593, 12.69999999999954632 ) ) ;
#90634 = VECTOR ( 'NONE', #142354, 1000.000000000000114 ) ;
#90635 = FACE_OUTER_BOUND ( 'NONE', #66436, .T. ) ;
#90636 = LINE ( 'NONE', #123974, #66130 ) ;
#90637 = DIRECTION ( 'NONE',  ( -1.000000000000000000, -1.224606353822377258E-16, -0.000000000000000000 ) ) ;
#90638 = CARTESIAN_POINT ( 'NONE',  ( 45.18398860626900415, 28.73617430169818832, 5.000000000000000000 ) ) ;
#90639 = CARTESIAN_POINT ( 'NONE',  ( 26.99451991528749417, 28.92564299267956685, 4.000000000000000000 ) ) ;
#90640 = CARTESIAN_POINT ( 'NONE',  ( -20.48334561358941386, 22.22500000000000142, 4.500000000000000888 ) ) ;
#90641 = EDGE_CURVE ( 'NONE', #33213, #91632, #29465, .T. ) ;
#90642 = EDGE_CURVE ( 'NONE', #31547, #94901, #63575, .T. ) ;
#90643 = ORIENTED_EDGE ( 'NONE', *, *, #5022, .F. ) ;
#90644 = EDGE_LOOP ( 'NONE', ( #10454, #29985, #131296, #80375 ) ) ;
#90645 = CARTESIAN_POINT ( 'NONE',  ( 108.5004301918981184, -3.055000000000002380, 5.291415217122920289 ) ) ;
#90646 = ADVANCED_FACE ( 'NONE', ( #96834 ), #54818, .F. ) ;
#90647 = VERTEX_POINT ( 'NONE', #128786 ) ;
#90648 = VECTOR ( 'NONE', #128656, 1000.000000000000227 ) ;
#90649 = EDGE_CURVE ( 'NONE', #33187, #92519, #142540, .T. ) ;
#90650 = CARTESIAN_POINT ( 'NONE',  ( 99.87499999999998579, 7.950000000000000178, 1.460391307983218535E-15 ) ) ;
#90651 = EDGE_CURVE ( 'NONE', #68408, #100403, #31629, .T. ) ;
#90652 = DIRECTION ( 'NONE',  ( 0.3543493200069163240, 0.000000000000000000, -0.9351131265310288487 ) ) ;
#90653 = CARTESIAN_POINT ( 'NONE',  ( -0.7071067811865329178, -15.74070752338412760, 5.000000000000000000 ) ) ;
#90654 = CARTESIAN_POINT ( 'NONE',  ( 0.000000000000000000, -35.14999999999999147, -40.00000000000000000 ) ) ;
#90655 =( GEOMETRIC_REPRESENTATION_CONTEXT ( 3 ) GLOBAL_UNCERTAINTY_ASSIGNED_CONTEXT ( ( #11209 ) ) GLOBAL_UNIT_ASSIGNED_CONTEXT ( ( #69662, #113118, #113841 ) ) REPRESENTATION_CONTEXT ( 'NONE', 'WORKASPACE' ) );
#90656 = ADVANCED_FACE ( 'NONE', ( #76581 ), #75852, .F. ) ;
#90657 = VECTOR ( 'NONE', #76765, 1000.000000000000000 ) ;
#90658 = CARTESIAN_POINT ( 'NONE',  ( 109.5787635252314516, -7.482591942790325086E-16, 6.109999999999998543 ) ) ;
#90659 = ORIENTED_EDGE ( 'NONE', *, *, #54320, .F. ) ;
#90660 = STYLED_ITEM ( 'NONE', ( #818 ), #84973 ) ;
#90661 = ORIENTED_EDGE ( 'NONE', *, *, #41495, .T. ) ;
#90662 = CARTESIAN_POINT ( 'NONE',  ( 1.827855086967997478, 2.055000000000001048, 0.000000000000000000 ) ) ;
#90663 = VECTOR ( 'NONE', #68008, 1000.000000000000000 ) ;
#90664 = DIRECTION ( 'NONE',  ( 0.7071067811865486830, -0.7071067811865464625, -0.000000000000000000 ) ) ;
#90665 = ADVANCED_FACE ( 'NONE', ( #7706 ), #120016, .F. ) ;
#90666 = ORIENTED_EDGE ( 'NONE', *, *, #23051, .F. ) ;
#90667 = ORIENTED_EDGE ( 'NONE', *, *, #50354, .T. ) ;
#90668 = EDGE_LOOP ( 'NONE', ( #103152, #71930, #21132, #126526, #47871 ) ) ;
#90669 = COLOUR_RGB ( '', 0.40784314, 0.44705882, 0.49803922) ;
#90670 = FACE_OUTER_BOUND ( 'NONE', #128007, .T. ) ;
#90671 = CARTESIAN_POINT ( 'NONE',  ( 2.254569808101886341, -6.871911579029512218, 3.967499999999996252 ) ) ;
#90672 = EDGE_CURVE ( 'NONE', #89139, #47131, #21464, .T. ) ;
#90673 = CARTESIAN_POINT ( 'NONE',  ( 32.72459685856478728, -1.637169565754160949, 6.109999999999997655 ) ) ;
#90674 = VERTEX_POINT ( 'NONE', #65728 ) ;
#90675 = ORIENTED_EDGE ( 'NONE', *, *, #89035, .F. ) ;
#90676 = CARTESIAN_POINT ( 'NONE',  ( -20.81601139373100295, 28.73617430169773002, 5.000000000000000000 ) ) ;
#90677 = VERTEX_POINT ( 'NONE', #18566 ) ;
#90678 = ORIENTED_EDGE ( 'NONE', *, *, #49602, .F. ) ;
#90679 = VECTOR ( 'NONE', #99340, 1000.000000000000000 ) ;
#90680 = ORIENTED_EDGE ( 'NONE', *, *, #4316, .F. ) ;
#90681 = VECTOR ( 'NONE', #59582, 1000.000000000000227 ) ;
#90682 = DIRECTION ( 'NONE',  ( -0.7071067811865487940, 0.7071067811865463515, -0.000000000000000000 ) ) ;
#90683 = EDGE_CURVE ( 'NONE', #25059, #45102, #9098, .T. ) ;
#90684 = CARTESIAN_POINT ( 'NONE',  ( -20.20710678118641113, 18.75929247661552779, 5.000000000000000000 ) ) ;
#90685 = CARTESIAN_POINT ( 'NONE',  ( 25.65999999999999659, 2.055000000000001492, 2.516649172247811554E-16 ) ) ;
#90686 = ORIENTED_EDGE ( 'NONE', *, *, #90328, .F. ) ;
#90687 = DIRECTION ( 'NONE',  ( 0.3543493200069162685, -0.000000000000000000, -0.9351131265310288487 ) ) ;
#90688 = EDGE_CURVE ( 'NONE', #104746, #117017, #96140, .T. ) ;
#90689 = AXIS2_PLACEMENT_3D ( 'NONE', #91466, #16741, #105175 ) ;
#90690 = CARTESIAN_POINT ( 'NONE',  ( 33.29974487139158867, -27.71228299555229313, 4.000000000000000000 ) ) ;
#90691 = EDGE_CURVE ( 'NONE', #67860, #9144, #97577, .T. ) ;
#90692 = FACE_BOUND ( 'NONE', #36137, .T. ) ;
#90693 = ORIENTED_EDGE ( 'NONE', *, *, #71162, .T. ) ;
#90694 = CARTESIAN_POINT ( 'NONE',  ( 11.99999999999992895, -0.4125381241607481431, 4.000000000000000000 ) ) ;
#90695 = CARTESIAN_POINT ( 'NONE',  ( 19.10813147593277250, 2.055000000000001048, 2.516649172247811554E-16 ) ) ;
#90696 = CARTESIAN_POINT ( 'NONE',  ( -21.47512612785032715, 14.25929247661557753, 9.797011795316587168 ) ) ;
#90697 = VERTEX_POINT ( 'NONE', #129489 ) ;
#90698 = DIRECTION ( 'NONE',  ( 1.000000000000000000, 0.000000000000000000, 0.000000000000000000 ) ) ;
#90699 = ORIENTED_EDGE ( 'NONE', *, *, #90812, .T. ) ;
#90700 = ORIENTED_EDGE ( 'NONE', *, *, #19434, .T. ) ;
#90701 = VECTOR ( 'NONE', #110879, 999.9999999999998863 ) ;
#90702 = ORIENTED_EDGE ( 'NONE', *, *, #13092, .F. ) ;
#90703 = CARTESIAN_POINT ( 'NONE',  ( 48.76626352523144448, 4.472830434245838482, -4.472830434245837594 ) ) ;
#90704 = ORIENTED_EDGE ( 'NONE', *, *, #11344, .F. ) ;
#90705 = DIRECTION ( 'NONE',  ( -1.000000000000000000, -1.224606353822377258E-16, -0.000000000000000000 ) ) ;
#90706 = CARTESIAN_POINT ( 'NONE',  ( 29.99999999999999645, 2.375000000000000000, 0.000000000000000000 ) ) ;
#90707 = EDGE_CURVE ( 'NONE', #10935, #126541, #124339, .T. ) ;
#90708 = ORIENTED_EDGE ( 'NONE', *, *, #38123, .F. ) ;
#90709 = PRESENTATION_STYLE_ASSIGNMENT (( #126860 ) ) ;
#90710 = FACE_OUTER_BOUND ( 'NONE', #30531, .T. ) ;
#90711 = VECTOR ( 'NONE', #129418, 999.9999999999998863 ) ;
#90712 = COLOUR_RGB ( '', 0.40784314, 0.44705882, 0.49803922) ;
#90713 = VECTOR ( 'NONE', #106356, 1000.000000000000114 ) ;
#90714 = AXIS2_PLACEMENT_3D ( 'NONE', #79311, #24167, #113294 ) ;
#90715 = SURFACE_SIDE_STYLE ('',( #46529 ) ) ;
#90716 = CARTESIAN_POINT ( 'NONE',  ( 2.613322195557305605, 4.202752102959690472E-16, 0.000000000000000000 ) ) ;
#90718 = EDGE_CURVE ( 'NONE', #1660, #125050, #23593, .T. ) ;
#90717 = CARTESIAN_POINT ( 'NONE',  ( 27.79333936457828358, 21.75929247661549226, 4.998822639870708073 ) ) ;
#90719 = CARTESIAN_POINT ( 'NONE',  ( -17.29289321881334018, -15.74070752338413470, 5.000000000000000000 ) ) ;
#90720 = VERTEX_POINT ( 'NONE', #68558 ) ;
#90721 = ORIENTED_EDGE ( 'NONE', *, *, #137632, .F. ) ;
#90722 = AXIS2_PLACEMENT_3D ( 'NONE', #17277, #85377, #141946 ) ;
#90723 = AXIS2_PLACEMENT_3D ( 'NONE', #25882, #57826, #91170 ) ;
#90724 = ORIENTED_EDGE ( 'NONE', *, *, #30900, .T. ) ;
#90725 = STYLED_ITEM ( 'NONE', ( #83855 ), #65678 ) ;
#90726 = EDGE_LOOP ( 'NONE', ( #90192, #70545, #129223, #8544, #138823 ) ) ;
#90727 = CARTESIAN_POINT ( 'NONE',  ( -12.29974487139158512, -27.71228299555214747, 4.000000000000000000 ) ) ;
#90728 = EDGE_LOOP ( 'NONE', ( #24312, #83548, #27089, #90860, #5059 ) ) ;
#90729 = VECTOR ( 'NONE', #96394, 1000.000000000000000 ) ;
#90730 = ORIENTED_EDGE ( 'NONE', *, *, #5989, .T. ) ;
#90731 = CARTESIAN_POINT ( 'NONE',  ( 166.8575281714868481, 26.96999999999994202, -31.92499999999998295 ) ) ;
#90732 = ADVANCED_FACE ( 'NONE', ( #46835 ), #25006, .F. ) ;
#90733 = PLANE ( 'NONE',  #136537 ) ;
#90734 = ORIENTED_EDGE ( 'NONE', *, *, #39901, .F. ) ;
#90735 = VECTOR ( 'NONE', #128452, 999.9999999999998863 ) ;
#90736 = DIRECTION ( 'NONE',  ( 0.000000000000000000, -1.000000000000000000, 0.000000000000000000 ) ) ;
#90737 = CARTESIAN_POINT ( 'NONE',  ( 39.29974487139159578, -27.71228299555233576, 4.000000000000000000 ) ) ;
#90738 = EDGE_CURVE ( 'NONE', #103631, #76159, #35990, .T. ) ;
#90739 = CARTESIAN_POINT ( 'NONE',  ( 26.31706980810189123, -2.126176841940956130, 7.934999999999991616 ) ) ;
#90740 = DIRECTION ( 'NONE',  ( 0.7071067811865487940, 0.7071067811865463515, 0.000000000000000000 ) ) ;
#90741 = ORIENTED_EDGE ( 'NONE', *, *, #77749, .T. ) ;
#90743 = CARTESIAN_POINT ( 'NONE',  ( -30.29974487139158867, -27.71228299555227537, 4.000000000000000000 ) ) ;
#90742 = CARTESIAN_POINT ( 'NONE',  ( 111.1829301918981230, -1.637169565754159173, -6.109999999999999432 ) ) ;
#90744 = LINE ( 'NONE', #12433, #74382 ) ;
#90745 = CARTESIAN_POINT ( 'NONE',  ( -15.33010218547255832, 17.25929247661554555, 19.83885114516074921 ) ) ;
#90746 = ORIENTED_EDGE ( 'NONE', *, *, #109343, .F. ) ;
#90747 = PLANE ( 'NONE',  #102855 ) ;
#90749 = ORIENTED_EDGE ( 'NONE', *, *, #116017, .F. ) ;
#90748 = DIRECTION ( 'NONE',  ( 0.7071067811865486830, -0.7071067811865464625, -0.000000000000000000 ) ) ;
#90750 = CARTESIAN_POINT ( 'NONE',  ( 31.49999999999977973, -10.91253812416064228, 4.000000000000000000 ) ) ;
#90751 = ORIENTED_EDGE ( 'NONE', *, *, #101070, .F. ) ;
#90752 = LINE ( 'NONE', #44404, #84643 ) ;
#90753 = LINE ( 'NONE', #134983, #114076 ) ;
#90754 = CARTESIAN_POINT ( 'NONE',  ( 120.4374999999999858, 5.819803920172574863, -5.819803920172573086 ) ) ;
#90756 = EDGE_CURVE ( 'NONE', #138480, #118870, #79461, .T. ) ;
#90755 = ORIENTED_EDGE ( 'NONE', *, *, #77483, .F. ) ;
#90757 = CIRCLE ( 'NONE', #132475, 1.000000000000000888 ) ;
#90758 = PLANE ( 'NONE',  #94517 ) ;
#90759 = CIRCLE ( 'NONE', #28236, 3.000000000000002665 ) ;
#90760 = EDGE_CURVE ( 'NONE', #30354, #103699, #112745, .T. ) ;
#90761 = CARTESIAN_POINT ( 'NONE',  ( 0.000000000000000000, -8.616843969807042924, 0.000000000000000000 ) ) ;
#90762 = FACE_OUTER_BOUND ( 'NONE', #140917, .T. ) ;
#90763 = ORIENTED_EDGE ( 'NONE', *, *, #89283, .T. ) ;
#90764 = VECTOR ( 'NONE', #56785, 1000.000000000000000 ) ;
#90765 = CARTESIAN_POINT ( 'NONE',  ( 53.99451991528749062, 28.92564299267975869, 4.000000000000000000 ) ) ;
#90766 = EDGE_LOOP ( 'NONE', ( #140878, #125427, #94192 ) ) ;
#90767 = PLANE ( 'NONE',  #90140 ) ;
#90769 = ORIENTED_EDGE ( 'NONE', *, *, #34001, .F. ) ;
#90768 = DIRECTION ( 'NONE',  ( -0.7071067811865486830, -0.7071067811865464625, 0.000000000000000000 ) ) ;
#90770 = EDGE_CURVE ( 'NONE', #39702, #35602, #13406, .T. ) ;
#90771 = EDGE_LOOP ( 'NONE', ( #53354, #829, #124281, #64339 ) ) ;
#90772 = DIRECTION ( 'NONE',  ( -1.000000000000000000, 0.000000000000000000, -0.000000000000000000 ) ) ;
#90773 = LINE ( 'NONE', #92152, #113172 ) ;
#90774 = VECTOR ( 'NONE', #67724, 1000.000000000000000 ) ;
#90775 = VERTEX_POINT ( 'NONE', #43934 ) ;
#90776 = LINE ( 'NONE', #24773, #101692 ) ;
#90777 = ORIENTED_EDGE ( 'NONE', *, *, #141001, .F. ) ;
#90778 = CARTESIAN_POINT ( 'NONE',  ( 23.29289321881329400, 14.25929247661557753, 5.000000000000000000 ) ) ;
#90779 = LINE ( 'NONE', #80613, #132411 ) ;
#90780 = VECTOR ( 'NONE', #91879, 1000.000000000000000 ) ;
#90781 = CARTESIAN_POINT ( 'NONE',  ( 63.48921356237309510, -27.52281430457099631, 5.000000000000000000 ) ) ;
#90782 = DIRECTION ( 'NONE',  ( 0.7071067811865486830, -0.7071067811865464625, -0.000000000000000000 ) ) ;
#90783 = AXIS2_PLACEMENT_3D ( 'NONE', #23156, #110875, #100047 ) ;
#90784 = LINE ( 'NONE', #113937, #46073 ) ;
#90785 = DIRECTION ( 'NONE',  ( -0.7071067811865486830, -0.7071067811865464625, 0.000000000000000000 ) ) ;
#90786 = VERTEX_POINT ( 'NONE', #111302 ) ;
#90787 = EDGE_LOOP ( 'NONE', ( #120619, #132920, #8097, #17621 ) ) ;
#90788 = ORIENTED_EDGE ( 'NONE', *, *, #39218, .F. ) ;
#90789 = CARTESIAN_POINT ( 'NONE',  ( 121.8958333333333144, -2.130196079827427091, 7.949999999999999289 ) ) ;
#90790 = ORIENTED_EDGE ( 'NONE', *, *, #96809, .T. ) ;
#90791 = VERTEX_POINT ( 'NONE', #80152 ) ;
#90792 = ORIENTED_EDGE ( 'NONE', *, *, #117004, .F. ) ;
#90793 = AXIS2_PLACEMENT_3D ( 'NONE', #10995, #34950, #90004 ) ;
#90794 = LINE ( 'NONE', #13893, #82623 ) ;
#90795 = DIRECTION ( 'NONE',  ( 1.000000000000000000, 0.000000000000000000, 0.000000000000000000 ) ) ;
#90796 = ORIENTED_EDGE ( 'NONE', *, *, #65268, .T. ) ;
#90797 = CARTESIAN_POINT ( 'NONE',  ( 34.92499999999998295, -21.72500000000000142, 5.000000000000000000 ) ) ;
#90798 = CARTESIAN_POINT ( 'NONE',  ( 131.5423521607622490, -49.05583548141700589, 39.86617647058822911 ) ) ;
#90799 = FACE_OUTER_BOUND ( 'NONE', #45234, .T. ) ;
#90800 = CARTESIAN_POINT ( 'NONE',  ( 8.999999999999937828, 13.93112307739204425, 4.000000000000000000 ) ) ;
#90801 = CARTESIAN_POINT ( 'NONE',  ( 124.1045968585647756, 1.637169565754164946, -6.109999999999999432 ) ) ;
#90802 = VERTEX_POINT ( 'NONE', #2528 ) ;
#90803 = PLANE ( 'NONE',  #113595 ) ;
#90804 = CARTESIAN_POINT ( 'NONE',  ( 104.7875270504628986, 0.000000000000000000, -7.949999999999998401 ) ) ;
#90806 = CONICAL_SURFACE ( 'NONE', #28288, 2.055000000000001048, 0.9599310885968758145 ) ;
#90805 = DIRECTION ( 'NONE',  ( 0.6830127018922180770, -0.6830127018922204085, -0.2588190451025213501 ) ) ;
#90807 = CARTESIAN_POINT ( 'NONE',  ( 0.9430526776243700615, 5.848452262106093258, 4.137244182379782309 ) ) ;
#90808 = DIRECTION ( 'NONE',  ( 0.7071067811865487940, 0.7071067811865463515, 0.000000000000000000 ) ) ;
#90809 = CARTESIAN_POINT ( 'NONE',  ( 2.816011393730999401, 28.73617430169785436, 5.000000000000000000 ) ) ;
#90810 = CARTESIAN_POINT ( 'NONE',  ( 51.41252705046289861, -7.949999999999998401, -4.867971026610728450E-16 ) ) ;
#90811 = LINE ( 'NONE', #21955, #374 ) ;
#90812 = EDGE_CURVE ( 'NONE', #68516, #44903, #57688, .T. ) ;
#90813 = DIRECTION ( 'NONE',  ( 1.000000000000000000, 0.000000000000000000, 0.000000000000000000 ) ) ;
#90814 = ORIENTED_EDGE ( 'NONE', *, *, #81494, .F. ) ;
#90815 = ORIENTED_EDGE ( 'NONE', *, *, #60258, .F. ) ;
#90816 = CARTESIAN_POINT ( 'NONE',  ( 48.68749999999998579, -5.819803920172573086, 5.819803920172572198 ) ) ;
#90817 = EDGE_CURVE ( 'NONE', #64329, #137485, #22845, .T. ) ;
#90818 = ORIENTED_EDGE ( 'NONE', *, *, #79584, .F. ) ;
#90819 = CARTESIAN_POINT ( 'NONE',  ( -34.47516574401891631, -10.50948238788427425, 4.998110765256835286 ) ) ;
#90820 = ADVANCED_FACE ( 'NONE', ( #100456 ), #59185, .T. ) ;
#90821 = VERTEX_POINT ( 'NONE', #12706 ) ;
#90822 = AXIS2_PLACEMENT_3D ( 'NONE', #87894, #21209, #111042 ) ;
#90823 = VECTOR ( 'NONE', #64895, 999.9999999999998863 ) ;
#90824 = VECTOR ( 'NONE', #125428, 1000.000000000000000 ) ;
#90825 = EDGE_CURVE ( 'NONE', #102617, #105152, #14132, .T. ) ;
#90826 = LINE ( 'NONE', #37874, #112771 ) ;
#90827 = PLANE ( 'NONE',  #120908 ) ;
#90828 = VECTOR ( 'NONE', #65625, 1000.000000000000000 ) ;
#90829 = VECTOR ( 'NONE', #26138, 1000.000000000000000 ) ;
#90830 = CARTESIAN_POINT ( 'NONE',  ( 42.43793019189809712, -6.110000000000001208, 1.637169565754158951 ) ) ;
#90832 = EDGE_CURVE ( 'NONE', #29747, #61512, #67113, .T. ) ;
#90831 = ORIENTED_EDGE ( 'NONE', *, *, #44900, .F. ) ;
#90833 = CARTESIAN_POINT ( 'NONE',  ( 1.146007053337370074, 0.3999999999999995781, 2.166563668000046849 ) ) ;
#90834 = ORIENTED_EDGE ( 'NONE', *, *, #52177, .T. ) ;
#90835 = AXIS2_PLACEMENT_3D ( 'NONE', #64229, #110552, #77969 ) ;
#90836 = CONICAL_SURFACE ( 'NONE', #46890, 2.055000000000001048, 0.9599310885968758145 ) ;
#90837 = MECHANICAL_DESIGN_GEOMETRIC_PRESENTATION_REPRESENTATION (  '', ( #137067 ), #44486 ) ;
#90838 = LINE ( 'NONE', #135067, #135353 ) ;
#90839 = CARTESIAN_POINT ( 'NONE',  ( 3.183988606268992161, 28.73617430169789699, 5.000000000000000000 ) ) ;
#90840 = DIRECTION ( 'NONE',  ( -0.7071067811865486830, -0.7071067811865464625, -0.000000000000000000 ) ) ;
#90841 = ADVANCED_FACE ( 'NONE', ( #99721 ), #58424, .F. ) ;
#90842 = CARTESIAN_POINT ( 'NONE',  ( 8.111591955682463606, 4.202752102959690472E-16, 0.000000000000000000 ) ) ;
#90843 = ORIENTED_EDGE ( 'NONE', *, *, #121642, .T. ) ;
#90844 = EDGE_CURVE ( 'NONE', #99639, #50968, #82344, .T. ) ;
#90845 = LINE ( 'NONE', #79984, #142 ) ;
#90846 = VERTEX_POINT ( 'NONE', #122915 ) ;
#90847 = CARTESIAN_POINT ( 'NONE',  ( 34.42499999999998295, 22.22500000000000142, 5.000000000000000000 ) ) ;
#90848 = DIRECTION ( 'NONE',  ( -0.000000000000000000, -0.3543493200069152693, 0.9351131265310292928 ) ) ;
#90849 = DIRECTION ( 'NONE',  ( -0.6830127018922181881, 0.6830127018922202975, -0.2588190451025214056 ) ) ;
#90850 = DIRECTION ( 'NONE',  ( -0.7071067811865486830, -0.7071067811865464625, -0.000000000000000000 ) ) ;
#90851 = EDGE_CURVE ( 'NONE', #9933, #99443, #33092, .T. ) ;
#90852 = CARTESIAN_POINT ( 'NONE',  ( 31.28752705046289151, 0.000000000000000000, -7.949999999999998401 ) ) ;
#90853 = CARTESIAN_POINT ( 'NONE',  ( 58.68293019189811588, -1.637169565754158951, -6.109999999999998543 ) ) ;
#90854 = CARTESIAN_POINT ( 'NONE',  ( 17.99999999999987921, 20.96639925780205260, 5.000000000000000000 ) ) ;
#90855 = DIRECTION ( 'NONE',  ( -0.7071067811865486830, -0.7071067811865464625, 0.000000000000000000 ) ) ;
#90857 = EDGE_LOOP ( 'NONE', ( #111506, #114865, #45654, #52556 ) ) ;
#90856 = CARTESIAN_POINT ( 'NONE',  ( -31.49999999999977973, 19.46639925780206326, 5.000000000000000000 ) ) ;
#90858 = ORIENTED_EDGE ( 'NONE', *, *, #15785, .T. ) ;
#90859 = CARTESIAN_POINT ( 'NONE',  ( 1.592112687295236251, -0.3999999999999997446, -2.358007167714499364 ) ) ;
#90860 = ORIENTED_EDGE ( 'NONE', *, *, #124051, .T. ) ;
#90861 = VECTOR ( 'NONE', #60226, 1000.000000000000114 ) ;
#90862 = PLANE ( 'NONE',  #65080 ) ;
#90863 = VERTEX_POINT ( 'NONE', #77305 ) ;
#90864 = AXIS2_PLACEMENT_3D ( 'NONE', #73779, #117954, #52032 ) ;
#90865 = DIRECTION ( 'NONE',  ( -0.000000000000000000, 0.000000000000000000, 1.000000000000000000 ) ) ;
#90866 = EDGE_CURVE ( 'NONE', #123433, #98806, #88881, .T. ) ;
#90867 = LINE ( 'NONE', #47393, #8474 ) ;
#90868 = PRESENTATION_LAYER_ASSIGNMENT (  '', '', ( #65415 ) ) ;
#90869 = CARTESIAN_POINT ( 'NONE',  ( -19.05000000000000071, 3.174999999999997158, 1.444000000000000394 ) ) ;
#90870 = FACE_BOUND ( 'NONE', #116393, .T. ) ;
#90871 = CARTESIAN_POINT ( 'NONE',  ( 0.4892135623730947680, -27.52281430457055578, 5.000000000000000000 ) ) ;
#90872 = FACE_OUTER_BOUND ( 'NONE', #68917, .T. ) ;
#90873 = LINE ( 'NONE', #45241, #45685 ) ;
#90874 = CYLINDRICAL_SURFACE ( 'NONE', #96584, 4.749999999999997335 ) ;
#90876 = ORIENTED_EDGE ( 'NONE', *, *, #107812, .T. ) ;
#90875 = CARTESIAN_POINT ( 'NONE',  ( 75.48921356237309510, -27.52281430457107803, 5.000000000000000000 ) ) ;
#90877 = ORIENTED_EDGE ( 'NONE', *, *, #87175, .F. ) ;
#90878 = LINE ( 'NONE', #48790, #141250 ) ;
#90880 = ADVANCED_FACE ( 'NONE', ( #1793 ), #90269, .F. ) ;
#90879 =( BOUNDED_SURFACE ( )  B_SPLINE_SURFACE ( 1, 2, ( 
 ( #111055, #98766, #32104, #56032, #120493, #143004, #132875, #43693, #132150, #121241, #21931, #11024, #33565, #121940, #45163, #126255, #92902, #26931, #3711, #35716, #38534, #46605, #79938, #16021, #92173, #48697, #101633, #125555, #26232, #24786, #58912, #71180, #124109, #60307, #102382, #90789, #114642, #15310, #113216, #81347, #103753, #69035, #48004, #13886, #14635, #3031, #4397, #104485, #103077, #47323, #58189, #91495, #27637, #36392, #49444, #82757, #135708, #115326, #136402, #5146, #137136, #37839, #71902, #82073, #70496, #93630, #137861, #69768, #80622, #126944, #116075, #37092, #124822, #25491, #59593, #113943, #16771, #2284, #135021, #130552, #51565, #83473, #141407, #127694, #84210, #94327, #128405, #105206, #7297, #31237, #105892, #96436, #42122, #107347, #41371, #6557, #116796, #52946, #75453, #28380, #72637, #50838, #119624, #63174, #140680, #61051, #86333, #117485, #19625, #17480, #29771, #50130, #5865, #139301, #140006, #138562, #30521, #85583, #62441, #106600, #8015, #39258, #61733, #52255, #74754, #129814, #118935, #95759, #18159, #29083, #95026, #39993, #73317, #63871, #108031, #40682, #84887, #129096, #74019, #8695, #118198, #18907, #97148, #1416, #45700, #111643, #21042, #133407, #134117, #65310, #43524, #120326, #97912, #89869, #76902, #77606, #55126, #88475, #11573, #121075, #34096, #66022, #78305, #9426, #99303, #121777, #122492, #23167, #108743, #55854, #22455, #100763, #10859, #131980, #100059, #34804, #56598, #109495, #143547, #66711, #21775, #44262, #79048, #110887, #132718, #67447, #32665, #12313, #20319, #33408, #710, #64562, #45006, #53709, #142150, #89182, #110188, #42834, #87034, #131249, #31937, #76162, #10170, #54433, #98609, #142840, #87745, #2114, #115164, #58010, #46427, #92722, #136958, #70326, #90610, #113776, #102205, #47159, #4225, #124650, #58744, #69592, #59435, #24620, #37667, #15836, #4965, #91340, #134852, #13718, #113045, #81169, #25327, #60133, #104299, #23927, #14466, #136232, #112358, #38365, #35548, #92016, #123958, #36920, #57291, #48520, #81906, #125376, #102913, #3554, #126097, #49267, #26762, #68875, #80459, #71012, #47851, #13016, #93456, #68186, #137691, #123253, #2859, #135549, #36233, #103592, #26063, #114474, #15152, #101463, #79778, #106421, #54097, #50657, #87410, #65696, #17988, #73839, #98283, #128928, #71718, #10524, #7109, #139114, #142508, #131626, #18715, #29601, #117317, #82579, #39070, #118013, #43195, #109859, #105034, #76544, #17311, #5699, #32315, #120722, #64948, #49965, #73153, #61572, #6382, #109139, #84040, #62265, #28914, #9825, #127506, #21432, #54786, #98964, #94850, #94148, #116629, #72459, #40515, #128236, #143203, #126772, #27456, #51389, #95583, #115882, #16583, #138384, #139844, #83297, #84717, #60873, #28202, #105722, #39818, #89532, #133763, #101838, #35904, #13374, #133073, #1072, #46805, #112020, #33060, #68528, #132366, #113412, #124304, #33756, #56245, #11958, #123627, #100425, #46062, #55499, #67830, #90240, #24971, #69228, #135216, #44654, #57650, #14096, #88848, #67082, #359, #121441, #58392, #45357, #101114, #78667, #12672, #35184, #34443, #2490, #122876, #90988, #77271, #23562, #1761, #80121, #102575, #22119, #79430, #134484, #43904, #56942, #24281, #112713, #88117, #66374, #77961, #110545, #11219, #99683, #122144, #22808, #111266, #116281, #27843, #4594, #48902, #5354, #116986, #91672, #93816, #16976, #72108, #138042, #137337, #59781, #114820, #114137, #72836, #125752, #38729, #6052, #26427, #69973, #14822, #81547, #48177, #37300, #82950, #16217, #61246, #127146, #105392, #93106, #80821, #83688, #135896, #125013, #50324, #38032, #94511, #3221, #27122, #71365, #59094, #103946, #138764, #25695, #39460, #3901, #36573, #60507, #104686, #103253, #126430, #49637, #92364, #82255, #136595, #115522, #70675, #127896, #28578, #17657, #15501, #61930, #47512, #32129, #40872, #53915, #43021, #106812, #75647, #52440, #9636, #97352, #42318, #76358, #141615, #130016, #86528, #108946, #74214, #73507, #20508, #53148, #96628, #140186, #29972, #30726, #117671, #87229, #74952, #131453, #120527, #140866, #128590, #21251, #29265, #129282, #139505, #118406, #6753, #41565, #106081, #7501, #130754, #51036, #8881, #31425, #51760, #18356, #98108, #95233, #62632, #95950, #85077, #40189, #108219, #119819, #84397, #19107, #63372, #64765, #107539, #119129, #8198, #142338, #85788, #19811, #64052, #121971, #123461, #68371, #1605, #12508, #100250, #65512, #21959, #100947, #35014, #90816, #87935, #57479, #172, #132178, #79255, #24119, #56789, #32873, #56061, #44467, #132907, #90064, #66906, #905, #11778, #45890, #110378, #112547, #101662, #135053, #33589, #77095, #99499, #55325, #23381, #111087, #2319, #46638, #109690, #45189, #78498, #54613, #124136, #121272, #34277, #66204, #122696, #143034, #134314, #13206, #67652, #89366, #133601, #35747, #79965, #10358, #11051, #22642, #98795, #111846, #43719, #88674, #77790, #94355, #105238, #14665, #37122, #136428, #104516, #81378, #26957, #36421, #125585, #80651, #69798, #58944, #5174, #37868, #49473, #16044, #93663, #70526, #102412, #5890, #113243, #3060, #82791, #15338, #115356, #24820, #48729, #92931, #91521, #26262, #137887, #47355, #126974, #25522, #13921, #82102, #126280, #124847, #4420, #71209, #135736, #114668, #113973, #59625, #103103, #60335, #27665, #103781, #3740, #48030, #92200, #138593, #137166, #116101, #50159, #38560, #71932, #16800, #61079, #39285, #83508, #58221, #69063, #129846, #64592, #118229, #95786, #63894, #9456, #20346, #29108, #107374, #30548, #40709, #18938, #53736, #74782, #8043, #97173, #140033, #130582, #108766, #63203, #118961, #141439, #19653, #116826, #97937, #52278, #84913, #42149, #31265, #108057, #8724, #96464, #127724, #84237, #52978, #86360, #142175, #6588, #119649, #62464, #50865, #75478, #42864, #28404, #95061, #140708, #106635, #51590 ),
 ( #17506, #72668, #139331, #41401, #128435, #85608, #61761, #105925, #40021, #73347, #29805, #74044, #117515, #18189, #7327, #129127, #44291, #89900, #11598, #76191, #111672, #31964, #13041, #23954, #76927, #99332, #55154, #23194, #17026, #89211, #79078, #21071, #101492, #134145, #112387, #34835, #87773, #56625, #57317, #132004, #110211, #43551, #65339, #2144, #88503, #734, #121801, #55884, #78332, #132740, #100791, #33433, #1442, #120351, #22479, #45030, #66741, #77633, #67479, #32696, #45727, #123281, #87060, #10885, #109520, #121101, #21800, #133431, #110915, #68211, #131275, #10195, #100083, #34119, #54459, #98635, #142864, #122525, #66048, #12338, #123982, #115185, #104325, #4253, #92037, #136261, #4992, #38390, #15866, #135577, #3580, #49294, #114501, #35575, #71037, #134879, #115907, #126798, #36256, #58771, #14490, #126119, #102938, #48550, #82605, #24644, #60898, #93481, #71749, #137716, #47184, #60159, #16615, #91366, #69619, #2888, #68899, #105062, #47873, #103614, #81196, #15179, #37693, #36947, #27484, #125404, #46454, #79806, #26092, #92746, #90645, #113077, #13747, #81933, #136987, #58037, #70351, #59456, #26791, #102237, #80485, #124679, #25357, #113804, #62293, #40540, #75312, #96292, #29625, #118786, #117340, #8553, #130405, #84742, #140535, #19480, #52111, #138414, #119480, #73868, #106452, #63727, #52799, #85431, #41226, #128955, #5723, #105746, #129659, #107886, #31093, #28228, #141249, #84064, #72487, #96998, #41962, #30357, #116650, #139865, #128261, #73179, #74601, #7133, #94878, #83325, #139140, #20170, #28937, #86177, #64413, #6406, #49990, #95609, #94172, #39100, #127531, #17337, #61595, #118041, #50688, #39844, #18012, #51415, #18746, #63021, #107197, #7872, #32515, #132570, #120182, #89734, #77468, #45560, #34655, #99153, #131109, #133957, #31793, #131824, #142003, #76750, #9272, #54987, #78889, #10029, #567, #123096, #11422, #89050, #54292, #20893, #100627, #23776, #76008, #65159, #98471, #108589, #110738, #44861, #53548, #97757, #21633, #67286, #109348, #121632, #42694, #86894, #43386, #44107, #142695, #78164, #133267, #110045, #10719, #55703, #87599, #120931, #99899, #122340, #33950, #23016, #143400, #65887, #88329, #33265, #22302, #66571, #111485, #12166, #56452, #1275, #36094, #123818, #112915, #102045, #4089, #81022, #92567, #59291, #136807, #113619, #1961, #4810, #12867, #46272, #125947, #58599, #15014, #68042, #91870, #136092, #134700, #25181, #37519, #90456, #26623, #68725, #57151, #125224, #25911, #79640, #47708, #70179, #35396, #14312, #24476, #124507, #13575, #114342, #70865, #69435, #36772, #103448, #102770, #3414, #137538, #48372, #81754, #115018, #80322, #15695, #49113, #59978, #104146, #93305, #38223, #101325, #82442, #126625, #112220, #57858, #2714, #47011, #91200, #135415, #27315, #127355, #62843, #140374, #52645, #49833, #19314, #105582, #94003, #41066, #85264, #117867, #138244, #17854, #6243, #94704, #51958, #28779, #106282, #117173, #107024, #72319, #129487, #63571, #96832, #138968, #38927, #61440, #17178, #128783, #73024, #107732, #8392, #71567, #62121, #40382, #16427, #85997, #83149, #139701, #28054, #84586, #104891, #96138, #30180, #29462, #6958, #51245, #74428, #141076, #118615, #116485, #128098, #41787, #95438, #60722, #115725, #5559, #50521, #39667, #83893, #73697, #18563, #7703, #98314, #132399, #122173, #64254, #1103, #133103, #11988, #77992, #130955, #99718, #100452, #31626, #9855, #86728, #108417, #56275, #43225, #43932, #21461, #54814, #121469, #87442, #390, #32341, #44685, #119319, #65725, #88153, #88878, #33784, #75157, #22145, #33090, #67111, #120755, #142538, #66404, #45384, #22842, #75850, #141827, #109888, #77301, #9096, #76578, #97575, #131657, #120014, #110575, #111299, #10553, #20726, #53363, #64984, #130235, #109172, #30923, #20006, #54124, #42525, #98998, #143234, #11256, #55526, #61780, #82816, #113441, #27689, #94371, #57685, #56971, #5908, #38581, #80150, #123653, #13403, #14129, #101144, #72690, #58421, #28428, #17523, #124335, #112046, #116847, #12700, #112742, #122912, #101864, #133792, #35931, #105945, #134516, #126997, #6605, #137907, #71955, #35217, #1791, #83533, #89561, #46092, #90266, #79459, #34477, #93681, #116126, #78694, #23591, #2524, #50183, #24309, #104540, #67861, #68555, #46832, #25004, #91021, #61104, #16828, #135242, #69259, #105258, #5205, #49496, #138618, #39310, #127744, #42168, #41422, #107395, #18963, #18211, #120371, #29824, #86382, #53757, #73368, #62484, #63229, #106662, #95806, #84934, #130608, #63911, #75496, #31286, #119667, #96484, #128455, #131295, #139355, #29126, #108790, #85631, #141463, #50890, #74809, #118986, #117534, #8061, #20366, #7351, #9480, #51614, #40044, #108076, #8744, #64611, #19672, #97959, #52297, #142194, #31979, #129869, #42886, #87081, #97198, #84257, #21094, #52999, #140726, #76206, #65358, #109539, #95085, #30571, #140052, #40730, #129147, #74066, #118253, #87788, #111689, #10907, #132024, #34136, #78349, #100099, #32718, #33449, #110225, #55174, #133449, #88522, #77650, #132760, #45047, #121121, #122543, #12356, #100807, #99348, #76947, #66065, #17, #11618, #121819, #56642, #1459, #10214, #22494, #55901, #142884, #54474, #21818, #753, #44310, #89226, #66761, #23218, #67498, #45744, #110934, #89917, #98655, #43569, #109284, #85376, #96938, #142633, #64357, #128887, #20832, #84684, #65829, #76689, #129592, #8495, #107830, #75947, #52746, #141945, #131764, #73807, #10655, #43326, #21571, #87537, #140477, #9962, #109990, #41166, #19418, #96234, #117977, #54922, #141185, #53486, #31032, #108529, #131045, #41901, #54232, #86114, #98416, #29569, #75258, #97691, #32448, #120860, #18682, #31729, #42635, #139807, #130342, #119418, #120121, #40486, #62957, #30297, #20112, #86833, #9204, #65093, #107134, #7811, #52059, #74540, #118724, #63671, #16453, #126656 ) ),
 .UNSPECIFIED., .F., .F., .F. ) 
 B_SPLINE_SURFACE_WITH_KNOTS ( ( 2, 2 ),
 ( 3, 2, 2, 2, 2, 2, 2, 2, 2, 2, 2, 2, 2, 2, 2, 2, 2, 2, 2, 2, 2, 2, 2, 2, 2, 2, 2, 2, 2, 2, 2, 2, 2, 2, 2, 2, 2, 2, 2, 2, 2, 2, 2, 2, 2, 2, 2, 2, 2, 2, 2, 2, 2, 2, 2, 2, 2, 2, 2, 2, 2, 2, 2, 2, 2, 2, 2, 2, 2, 2, 2, 2, 2, 2, 2, 2, 2, 2, 2, 2, 2, 2, 2, 2, 2, 2, 2, 2, 2, 2, 2, 2, 2, 2, 2, 2, 2, 2, 2, 2, 2, 2, 2, 2, 2, 2, 2, 2, 2, 2, 2, 2, 2, 2, 2, 2, 2, 2, 2, 2, 2, 2, 2, 2, 2, 2, 2, 2, 2, 2, 2, 2, 2, 2, 2, 2, 2, 2, 2, 2, 2, 2, 2, 2, 2, 2, 2, 2, 2, 2, 2, 2, 2, 2, 2, 2, 2, 2, 2, 2, 2, 2, 2, 2, 2, 2, 2, 2, 2, 2, 2, 2, 2, 2, 2, 2, 2, 2, 2, 2, 2, 2, 2, 2, 2, 2, 2, 2, 2, 2, 2, 2, 2, 2, 2, 2, 2, 2, 2, 2, 2, 2, 2, 2, 2, 2, 2, 2, 2, 2, 2, 2, 2, 2, 2, 2, 2, 2, 2, 2, 2, 2, 2, 2, 2, 2, 2, 2, 2, 2, 2, 2, 2, 2, 2, 2, 2, 2, 2, 2, 2, 2, 2, 2, 2, 2, 2, 2, 2, 2, 2, 2, 2, 2, 2, 2, 2, 2, 2, 2, 2, 2, 2, 2, 2, 2, 2, 2, 2, 2, 2, 2, 2, 2, 2, 2, 2, 2, 2, 2, 2, 2, 2, 2, 2, 2, 2, 2, 2, 2, 2, 2, 2, 2, 2, 2, 2, 2, 2, 2, 2, 2, 2, 2, 2, 2, 2, 2, 2, 2, 2, 2, 2, 2, 2, 2, 2, 2, 2, 2, 2, 2, 2, 2, 2, 2, 2, 2, 2, 2, 2, 2, 2, 2, 2, 2, 2, 2, 2, 2, 2, 2, 2, 2, 2, 2, 2, 2, 2, 2, 2, 3 ),
 ( 0.000000000000000000, 1.000000000000000000 ),
 ( 0.000000000000000000, 0.002777777777777777884, 0.005555555555555555768, 0.008333333333333333218, 0.01111111111111111154, 0.01388888888888888812, 0.01666666666666666644, 0.01944444444444444475, 0.02222222222222222307, 0.02500000000000000139, 0.02777777777777777624, 0.03055555555555555455, 0.03333333333333333287, 0.03611111111111110772, 0.03888888888888888951, 0.04166666666666666435, 0.04444444444444444614, 0.04722222222222222099, 0.05000000000000000278, 0.05277777777777777762, 0.05555555555555555247, 0.05833333333333333426, 0.06111111111111110911, 0.06388888888888888395, 0.06666666666666666574, 0.06944444444444444753, 0.07222222222222221544, 0.07499999999999999722, 0.07777777777777777901, 0.08055555555555556080, 0.08333333333333332871, 0.08611111111111111049, 0.08888888888888889228, 0.09166666666666666019, 0.09444444444444444198, 0.09722222222222222376, 0.1000000000000000056, 0.1027777777777777735, 0.1055555555555555552, 0.1083333333333333370, 0.1111111111111111049, 0.1138888888888888867, 0.1166666666666666685, 0.1194444444444444503, 0.1222222222222222182, 0.1250000000000000000, 0.1277777777777777679, 0.1305555555555555636, 0.1333333333333333315, 0.1361111111111110994, 0.1388888888888888951, 0.1416666666666666630, 0.1444444444444444309, 0.1472222222222222265, 0.1499999999999999944, 0.1527777777777777901, 0.1555555555555555580, 0.1583333333333333259, 0.1611111111111111216, 0.1638888888888888895, 0.1666666666666666574, 0.1694444444444444531, 0.1722222222222222210, 0.1749999999999999889, 0.1777777777777777846, 0.1805555555555555525, 0.1833333333333333204, 0.1861111111111111160, 0.1888888888888888840, 0.1916666666666666796, 0.1944444444444444475, 0.1972222222222222154, 0.2000000000000000111, 0.2027777777777777790, 0.2055555555555555469, 0.2083333333333333426, 0.2111111111111111105, 0.2138888888888888784, 0.2166666666666666741, 0.2194444444444444420, 0.2222222222222222099, 0.2250000000000000056, 0.2277777777777777735, 0.2305555555555555691, 0.2333333333333333370, 0.2361111111111111049, 0.2388888888888889006, 0.2416666666666666685, 0.2444444444444444364, 0.2472222222222222321, 0.2500000000000000000, 0.2527777777777777679, 0.2555555555555555358, 0.2583333333333333592, 0.2611111111111111271, 0.2638888888888888951, 0.2666666666666666630, 0.2694444444444444309, 0.2722222222222221988, 0.2750000000000000222, 0.2777777777777777901, 0.2805555555555555580, 0.2833333333333333259, 0.2861111111111110938, 0.2888888888888888618, 0.2916666666666666852, 0.2944444444444444531, 0.2972222222222222210, 0.2999999999999999889, 0.3027777777777777568, 0.3055555555555555802, 0.3083333333333333481, 0.3111111111111111160, 0.3138888888888888840, 0.3166666666666666519, 0.3194444444444444198, 0.3222222222222222432, 0.3250000000000000111, 0.3277777777777777790, 0.3305555555555555469, 0.3333333333333333148, 0.3361111111111111382, 0.3388888888888889062, 0.3416666666666666741, 0.3444444444444444420, 0.3472222222222222099, 0.3499999999999999778, 0.3527777777777778012, 0.3555555555555555691, 0.3583333333333333370, 0.3611111111111111049, 0.3638888888888888729, 0.3666666666666666408, 0.3694444444444444642, 0.3722222222222222321, 0.3750000000000000000, 0.3777777777777777679, 0.3805555555555555358, 0.3833333333333333592, 0.3861111111111111271, 0.3888888888888888951, 0.3916666666666666630, 0.3944444444444444309, 0.3972222222222221988, 0.4000000000000000222, 0.4027777777777777901, 0.4055555555555555580, 0.4083333333333333259, 0.4111111111111110938, 0.4138888888888888618, 0.4166666666666666852, 0.4194444444444444531, 0.4222222222222222210, 0.4249999999999999889, 0.4277777777777777568, 0.4305555555555555802, 0.4333333333333333481, 0.4361111111111111160, 0.4388888888888888840, 0.4416666666666666519, 0.4444444444444444198, 0.4472222222222222432, 0.4500000000000000111, 0.4527777777777777790, 0.4555555555555555469, 0.4583333333333333148, 0.4611111111111111382, 0.4638888888888889062, 0.4666666666666666741, 0.4694444444444444420, 0.4722222222222222099, 0.4749999999999999778, 0.4777777777777778012, 0.4805555555555555691, 0.4833333333333333370, 0.4861111111111111049, 0.4888888888888888729, 0.4916666666666666408, 0.4944444444444444642, 0.4972222222222222321, 0.5000000000000000000, 0.5027777777777777679, 0.5055555555555555358, 0.5083333333333333037, 0.5111111111111110716, 0.5138888888888888395, 0.5166666666666667185, 0.5194444444444444864, 0.5222222222222222543, 0.5250000000000000222, 0.5277777777777777901, 0.5305555555555555580, 0.5333333333333333259, 0.5361111111111110938, 0.5388888888888888618, 0.5416666666666666297, 0.5444444444444443976, 0.5472222222222222765, 0.5500000000000000444, 0.5527777777777778123, 0.5555555555555555802, 0.5583333333333333481, 0.5611111111111111160, 0.5638888888888888840, 0.5666666666666666519, 0.5694444444444444198, 0.5722222222222221877, 0.5749999999999999556, 0.5777777777777777235, 0.5805555555555556024, 0.5833333333333333703, 0.5861111111111111382, 0.5888888888888889062, 0.5916666666666666741, 0.5944444444444444420, 0.5972222222222222099, 0.5999999999999999778, 0.6027777777777777457, 0.6055555555555555136, 0.6083333333333332815, 0.6111111111111111605, 0.6138888888888889284, 0.6166666666666666963, 0.6194444444444444642, 0.6222222222222222321, 0.6250000000000000000, 0.6277777777777777679, 0.6305555555555555358, 0.6333333333333333037, 0.6361111111111110716, 0.6388888888888888395, 0.6416666666666667185, 0.6444444444444444864, 0.6472222222222222543, 0.6500000000000000222, 0.6527777777777777901, 0.6555555555555555580, 0.6583333333333333259, 0.6611111111111110938, 0.6638888888888888618, 0.6666666666666666297, 0.6694444444444443976, 0.6722222222222222765, 0.6750000000000000444, 0.6777777777777778123, 0.6805555555555555802, 0.6833333333333333481, 0.6861111111111111160, 0.6888888888888888840, 0.6916666666666666519, 0.6944444444444444198, 0.6972222222222221877, 0.6999999999999999556, 0.7027777777777777235, 0.7055555555555556024, 0.7083333333333333703, 0.7111111111111111382, 0.7138888888888889062, 0.7166666666666666741, 0.7194444444444444420, 0.7222222222222222099, 0.7249999999999999778, 0.7277777777777777457, 0.7305555555555555136, 0.7333333333333332815, 0.7361111111111111605, 0.7388888888888889284, 0.7416666666666666963, 0.7444444444444444642, 0.7472222222222222321, 0.7500000000000000000, 0.7527777777777777679, 0.7555555555555555358, 0.7583333333333333037, 0.7611111111111110716, 0.7638888888888888395, 0.7666666666666667185, 0.7694444444444444864, 0.7722222222222222543, 0.7750000000000000222, 0.7777777777777777901, 0.7805555555555555580, 0.7833333333333333259, 0.7861111111111110938, 0.7888888888888888618, 0.7916666666666666297, 0.7944444444444443976, 0.7972222222222222765, 0.8000000000000000444, 0.8027777777777778123, 0.8055555555555555802, 0.8083333333333333481, 0.8111111111111111160, 0.8138888888888888840, 0.8166666666666666519, 0.8194444444444444198, 0.8222222222222221877, 0.8249999999999999556, 0.8277777777777777235, 0.8305555555555556024, 0.8333333333333333703, 0.8361111111111111382, 0.8388888888888889062, 0.8416666666666666741, 0.8444444444444444420, 0.8472222222222222099, 0.8499999999999999778, 0.8527777777777777457, 0.8555555555555555136, 0.8583333333333332815, 0.8611111111111111605, 0.8638888888888889284, 0.8666666666666666963, 0.8694444444444444642, 0.8722222222222222321, 0.8750000000000000000, 0.8777777777777777679, 0.8805555555555555358, 0.8833333333333333037, 0.8861111111111110716, 0.8888888888888888395, 0.8916666666666667185, 0.8944444444444444864, 0.8972222222222222543, 0.9000000000000000222, 0.9027777777777777901, 0.9055555555555555580, 0.9083333333333333259, 0.9111111111111110938, 0.9138888888888888618, 0.9166666666666666297, 0.9194444444444443976, 0.9222222222222222765, 0.9250000000000000444, 0.9277777777777778123, 0.9305555555555555802, 0.9333333333333333481, 0.9361111111111111160, 0.9388888888888888840, 0.9416666666666666519, 0.9444444444444444198, 0.9472222222222221877, 0.9499999999999999556, 0.9527777777777777235, 0.9555555555555556024, 0.9583333333333333703, 0.9611111111111111382, 0.9638888888888889062, 0.9666666666666666741, 0.9694444444444444420, 0.9722222222222222099, 0.9749999999999999778 ),
 .UNSPECIFIED. ) 
 GEOMETRIC_REPRESENTATION_ITEM ( )  RATIONAL_B_SPLINE_SURFACE ( (
 ( 1.000000000000000000, 0.9659258262890683122, 1.000000000000000000, 0.9659258262890683122, 1.000000000000000000, 0.9659258262890683122, 1.000000000000000000, 0.9659258262890683122, 1.000000000000000000, 0.9659258262890683122, 1.000000000000000000, 0.9659258262890683122, 1.000000000000000000, 0.9659258262890683122, 1.000000000000000000, 0.9659258262890683122, 1.000000000000000000, 0.9659258262890683122, 1.000000000000000000, 0.9659258262890683122, 1.000000000000000000, 0.9659258262890683122, 1.000000000000000000, 0.9659258262890683122, 1.000000000000000000, 0.9659258262890683122, 1.000000000000000000, 0.9659258262890683122, 1.000000000000000000, 0.9659258262890683122, 1.000000000000000000, 0.9659258262890683122, 1.000000000000000000, 0.9659258262890683122, 1.000000000000000000, 0.9659258262890683122, 1.000000000000000000, 0.9659258262890683122, 1.000000000000000000, 0.9659258262890683122, 1.000000000000000000, 0.9659258262890683122, 1.000000000000000000, 0.9659258262890683122, 1.000000000000000000, 0.9659258262890683122, 1.000000000000000000, 0.9659258262890683122, 1.000000000000000000, 0.9659258262890683122, 1.000000000000000000, 0.9659258262890683122, 1.000000000000000000, 0.9659258262890683122, 1.000000000000000000, 0.9659258262890683122, 1.000000000000000000, 0.9659258262890683122, 1.000000000000000000, 0.9659258262890683122, 1.000000000000000000, 0.9659258262890683122, 1.000000000000000000, 0.9659258262890683122, 1.000000000000000000, 0.9659258262890683122, 1.000000000000000000, 0.9659258262890683122, 1.000000000000000000, 0.9659258262890683122, 1.000000000000000000, 0.9659258262890683122, 1.000000000000000000, 0.9659258262890683122, 1.000000000000000000, 0.9659258262890683122, 1.000000000000000000, 0.9659258262890683122, 1.000000000000000000, 0.9659258262890683122, 1.000000000000000000, 0.9659258262890683122, 1.000000000000000000, 0.9659258262890683122, 1.000000000000000000, 0.9659258262890683122, 1.000000000000000000, 0.9659258262890683122, 1.000000000000000000, 0.9659258262890683122, 1.000000000000000000, 0.9659258262890683122, 1.000000000000000000, 0.9659258262890683122, 1.000000000000000000, 0.9659258262890683122, 1.000000000000000000, 0.9659258262890683122, 1.000000000000000000, 0.9659258262890683122, 1.000000000000000000, 0.9659258262890683122, 1.000000000000000000, 0.9659258262890683122, 1.000000000000000000, 0.9659258262890683122, 1.000000000000000000, 0.9659258262890683122, 1.000000000000000000, 0.9659258262890683122, 1.000000000000000000, 0.9659258262890683122, 1.000000000000000000, 0.9659258262890683122, 1.000000000000000000, 0.9659258262890683122, 1.000000000000000000, 0.9659258262890683122, 1.000000000000000000, 0.9659258262890683122, 1.000000000000000000, 0.9659258262890683122, 1.000000000000000000, 0.9659258262890683122, 1.000000000000000000, 0.9659258262890683122, 1.000000000000000000, 0.9659258262890683122, 1.000000000000000000, 0.9659258262890683122, 1.000000000000000000, 0.9659258262890683122, 1.000000000000000000, 0.9659258262890683122, 1.000000000000000000, 0.9659258262890683122, 1.000000000000000000, 0.9659258262890683122, 1.000000000000000000, 0.9659258262890683122, 1.000000000000000000, 0.9659258262890683122, 1.000000000000000000, 0.9659258262890683122, 1.000000000000000000, 0.9659258262890683122, 1.000000000000000000, 0.9659258262890683122, 1.000000000000000000, 0.9659258262890683122, 1.000000000000000000, 0.9659258262890683122, 1.000000000000000000, 0.9659258262890683122, 1.000000000000000000, 0.9659258262890683122, 1.000000000000000000, 0.9659258262890683122, 1.000000000000000000, 0.9659258262890683122, 1.000000000000000000, 0.9659258262890683122, 1.000000000000000000, 0.9659258262890683122, 1.000000000000000000, 0.9659258262890683122, 1.000000000000000000, 0.9659258262890683122, 1.000000000000000000, 0.9659258262890683122, 1.000000000000000000, 0.9659258262890683122, 1.000000000000000000, 0.9659258262890683122, 1.000000000000000000, 0.9659258262890683122, 1.000000000000000000, 0.9659258262890683122, 1.000000000000000000, 0.9659258262890683122, 1.000000000000000000, 0.9659258262890683122, 1.000000000000000000, 0.9659258262890683122, 1.000000000000000000, 0.9659258262890683122, 1.000000000000000000, 0.9659258262890683122, 1.000000000000000000, 0.9659258262890683122, 1.000000000000000000, 0.9659258262890683122, 1.000000000000000000, 0.9659258262890683122, 1.000000000000000000, 0.9659258262890683122, 1.000000000000000000, 0.9659258262890683122, 1.000000000000000000, 0.9659258262890683122, 1.000000000000000000, 0.9659258262890683122, 1.000000000000000000, 0.9659258262890683122, 1.000000000000000000, 0.9659258262890683122, 1.000000000000000000, 0.9659258262890683122, 1.000000000000000000, 0.9659258262890683122, 1.000000000000000000, 0.9659258262890683122, 1.000000000000000000, 0.9659258262890683122, 1.000000000000000000, 0.9659258262890683122, 1.000000000000000000, 0.9659258262890683122, 1.000000000000000000, 0.9659258262890683122, 1.000000000000000000, 0.9659258262890683122, 1.000000000000000000, 0.9659258262890683122, 1.000000000000000000, 0.9659258262890683122, 1.000000000000000000, 0.9659258262890683122, 1.000000000000000000, 0.9659258262890683122, 1.000000000000000000, 0.9659258262890683122, 1.000000000000000000, 0.9659258262890683122, 1.000000000000000000, 0.9659258262890683122, 1.000000000000000000, 0.9659258262890683122, 1.000000000000000000, 0.9659258262890683122, 1.000000000000000000, 0.9659258262890683122, 1.000000000000000000, 0.9659258262890683122, 1.000000000000000000, 0.9659258262890683122, 1.000000000000000000, 0.9659258262890683122, 1.000000000000000000, 0.9659258262890683122, 1.000000000000000000, 0.9659258262890683122, 1.000000000000000000, 0.9659258262890683122, 1.000000000000000000, 0.9659258262890683122, 1.000000000000000000, 0.9659258262890683122, 1.000000000000000000, 0.9659258262890683122, 1.000000000000000000, 0.9659258262890683122, 1.000000000000000000, 0.9659258262890683122, 1.000000000000000000, 0.9659258262890683122, 1.000000000000000000, 0.9659258262890683122, 1.000000000000000000, 0.9659258262890683122, 1.000000000000000000, 0.9659258262890683122, 1.000000000000000000, 0.9659258262890683122, 1.000000000000000000, 0.9659258262890683122, 1.000000000000000000, 0.9659258262890683122, 1.000000000000000000, 0.9659258262890683122, 1.000000000000000000, 0.9659258262890683122, 1.000000000000000000, 0.9659258262890683122, 1.000000000000000000, 0.9659258262890683122, 1.000000000000000000, 0.9659258262890683122, 1.000000000000000000, 0.9659258262890683122, 1.000000000000000000, 0.9659258262890683122, 1.000000000000000000, 0.9659258262890683122, 1.000000000000000000, 0.9659258262890683122, 1.000000000000000000, 0.9659258262890683122, 1.000000000000000000, 0.9659258262890683122, 1.000000000000000000, 0.9659258262890683122, 1.000000000000000000, 0.9659258262890683122, 1.000000000000000000, 0.9659258262890683122, 1.000000000000000000, 0.9659258262890683122, 1.000000000000000000, 0.9659258262890683122, 1.000000000000000000, 0.9659258262890683122, 1.000000000000000000, 0.9659258262890683122, 1.000000000000000000, 0.9659258262890683122, 1.000000000000000000, 0.9659258262890683122, 1.000000000000000000, 0.9659258262890683122, 1.000000000000000000, 0.9659258262890683122, 1.000000000000000000, 0.9659258262890683122, 1.000000000000000000, 0.9659258262890683122, 1.000000000000000000, 0.9659258262890683122, 1.000000000000000000, 0.9659258262890683122, 1.000000000000000000, 0.9659258262890683122, 1.000000000000000000, 0.9659258262890683122, 1.000000000000000000, 0.9659258262890683122, 1.000000000000000000, 0.9659258262890683122, 1.000000000000000000, 0.9659258262890683122, 1.000000000000000000, 0.9659258262890683122, 1.000000000000000000, 0.9659258262890683122, 1.000000000000000000, 0.9659258262890683122, 1.000000000000000000, 0.9659258262890683122, 1.000000000000000000, 0.9659258262890683122, 1.000000000000000000, 0.9659258262890683122, 1.000000000000000000, 0.9659258262890683122, 1.000000000000000000, 0.9659258262890683122, 1.000000000000000000, 0.9659258262890683122, 1.000000000000000000, 0.9659258262890683122, 1.000000000000000000, 0.9659258262890683122, 1.000000000000000000, 0.9659258262890683122, 1.000000000000000000, 0.9659258262890683122, 1.000000000000000000, 0.9659258262890683122, 1.000000000000000000, 0.9659258262890683122, 1.000000000000000000, 0.9659258262890683122, 1.000000000000000000, 0.9659258262890683122, 1.000000000000000000, 0.9659258262890683122, 1.000000000000000000, 0.9659258262890683122, 1.000000000000000000, 0.9659258262890683122, 1.000000000000000000, 0.9659258262890683122, 1.000000000000000000, 0.9659258262890683122, 1.000000000000000000, 0.9659258262890683122, 1.000000000000000000, 0.9659258262890683122, 1.000000000000000000, 0.9659258262890683122, 1.000000000000000000, 0.9659258262890683122, 1.000000000000000000, 0.9659258262890683122, 1.000000000000000000, 0.9659258262890683122, 1.000000000000000000, 0.9659258262890683122, 1.000000000000000000, 0.9659258262890683122, 1.000000000000000000, 0.9659258262890683122, 1.000000000000000000, 0.9659258262890683122, 1.000000000000000000, 0.9659258262890683122, 1.000000000000000000, 0.9659258262890683122, 1.000000000000000000, 0.9659258262890683122, 1.000000000000000000, 0.9659258262890683122, 1.000000000000000000, 0.9659258262890683122, 1.000000000000000000, 0.9659258262890683122, 1.000000000000000000, 0.9659258262890683122, 1.000000000000000000, 0.9659258262890683122, 1.000000000000000000, 0.9659258262890683122, 1.000000000000000000, 0.9659258262890683122, 1.000000000000000000, 0.9659258262890683122, 1.000000000000000000, 0.9659258262890683122, 1.000000000000000000, 0.9659258262890683122, 1.000000000000000000, 0.9659258262890683122, 1.000000000000000000, 0.9659258262890683122, 1.000000000000000000, 0.9659258262890683122, 1.000000000000000000, 0.9659258262890683122, 1.000000000000000000, 0.9659258262890683122, 1.000000000000000000, 0.9659258262890683122, 1.000000000000000000, 0.9659258262890683122, 1.000000000000000000, 0.9659258262890683122, 1.000000000000000000, 0.9659258262890683122, 1.000000000000000000, 0.9659258262890683122, 1.000000000000000000, 0.9659258262890683122, 1.000000000000000000, 0.9659258262890683122, 1.000000000000000000, 0.9659258262890683122, 1.000000000000000000, 0.9659258262890683122, 1.000000000000000000, 0.9659258262890683122, 1.000000000000000000, 0.9659258262890683122, 1.000000000000000000, 0.9659258262890683122, 1.000000000000000000, 0.9659258262890683122, 1.000000000000000000, 0.9659258262890683122, 1.000000000000000000, 0.9659258262890683122, 1.000000000000000000, 0.9659258262890683122, 1.000000000000000000, 0.9659258262890683122, 1.000000000000000000, 0.9659258262890683122, 1.000000000000000000, 0.9659258262890683122, 1.000000000000000000, 0.9659258262890683122, 1.000000000000000000, 0.9659258262890683122, 1.000000000000000000, 0.9659258262890683122, 1.000000000000000000, 0.9659258262890683122, 1.000000000000000000, 0.9659258262890683122, 1.000000000000000000, 0.9659258262890683122, 1.000000000000000000, 0.9659258262890683122, 1.000000000000000000, 0.9659258262890683122, 1.000000000000000000, 0.9659258262890683122, 1.000000000000000000, 0.9659258262890683122, 1.000000000000000000, 0.9659258262890683122, 1.000000000000000000, 0.9659258262890683122, 1.000000000000000000, 0.9659258262890683122, 1.000000000000000000, 0.9659258262890683122, 1.000000000000000000, 0.9659258262890683122, 1.000000000000000000, 0.9659258262890683122, 1.000000000000000000, 0.9659258262890683122, 1.000000000000000000, 0.9659258262890683122, 1.000000000000000000, 0.9659258262890683122, 1.000000000000000000, 0.9659258262890683122, 1.000000000000000000, 0.9659258262890683122, 1.000000000000000000, 0.9659258262890683122, 1.000000000000000000, 0.9659258262890683122, 1.000000000000000000, 0.9659258262890683122, 1.000000000000000000, 0.9659258262890683122, 1.000000000000000000, 0.9659258262890683122, 1.000000000000000000, 0.9659258262890683122, 1.000000000000000000, 0.9659258262890683122, 1.000000000000000000, 0.9659258262890683122, 1.000000000000000000, 0.9659258262890683122, 1.000000000000000000, 0.9659258262890683122, 1.000000000000000000, 0.9659258262890683122, 1.000000000000000000, 0.9659258262890683122, 1.000000000000000000, 0.9659258262890683122, 1.000000000000000000, 0.9659258262890683122, 1.000000000000000000, 0.9659258262890683122, 1.000000000000000000, 0.9659258262890683122, 1.000000000000000000, 0.9659258262890683122, 1.000000000000000000, 0.9659258262890683122, 1.000000000000000000, 0.9659258262890683122, 1.000000000000000000, 0.9659258262890683122, 1.000000000000000000, 0.9659258262890683122, 1.000000000000000000, 0.9659258262890683122, 1.000000000000000000, 0.9659258262890683122, 1.000000000000000000, 0.9659258262890683122, 1.000000000000000000, 0.9659258262890683122, 1.000000000000000000, 0.9659258262890683122, 1.000000000000000000, 0.9659258262890683122, 1.000000000000000000, 0.9659258262890683122, 1.000000000000000000, 0.9659258262890683122, 1.000000000000000000, 0.9659258262890683122, 1.000000000000000000, 0.9659258262890683122, 1.000000000000000000, 0.9659258262890683122, 1.000000000000000000, 0.9659258262890683122, 1.000000000000000000, 0.9659258262890683122, 1.000000000000000000, 0.9659258262890683122, 1.000000000000000000, 0.9659258262890683122, 1.000000000000000000, 0.9659258262890683122, 1.000000000000000000, 0.9659258262890683122, 1.000000000000000000, 0.9659258262890683122, 1.000000000000000000, 0.9659258262890683122, 1.000000000000000000, 0.9659258262890683122, 1.000000000000000000, 0.9659258262890683122, 1.000000000000000000, 0.9659258262890683122, 1.000000000000000000, 0.9659258262890683122, 1.000000000000000000, 0.9659258262890683122, 1.000000000000000000, 0.9659258262890683122, 1.000000000000000000, 0.9659258262890683122, 1.000000000000000000, 0.9659258262890683122, 1.000000000000000000, 0.9659258262890683122, 1.000000000000000000, 0.9659258262890683122, 1.000000000000000000, 0.9659258262890683122, 1.000000000000000000, 0.9659258262890683122, 1.000000000000000000, 0.9659258262890683122, 1.000000000000000000, 0.9659258262890683122, 1.000000000000000000, 0.9659258262890683122, 1.000000000000000000, 0.9659258262890683122, 1.000000000000000000, 0.9659258262890683122, 1.000000000000000000, 0.9659258262890683122, 1.000000000000000000, 0.9659258262890683122, 1.000000000000000000, 0.9659258262890683122, 1.000000000000000000, 0.9659258262890683122, 1.000000000000000000, 0.9659258262890683122, 1.000000000000000000, 0.9659258262890683122, 1.000000000000000000, 0.9659258262890683122, 1.000000000000000000, 0.9659258262890683122, 1.000000000000000000, 0.9659258262890683122, 1.000000000000000000, 0.9659258262890683122, 1.000000000000000000, 0.9659258262890683122, 1.000000000000000000, 0.9659258262890683122, 1.000000000000000000, 0.9659258262890683122, 1.000000000000000000, 0.9659258262890683122, 1.000000000000000000, 0.9659258262890683122, 1.000000000000000000, 0.9659258262890683122, 1.000000000000000000, 0.9659258262890683122, 1.000000000000000000, 0.9659258262890683122, 1.000000000000000000, 0.9659258262890683122, 1.000000000000000000, 0.9659258262890683122, 1.000000000000000000, 0.9659258262890683122, 1.000000000000000000, 0.9659258262890683122, 1.000000000000000000, 0.9659258262890683122, 1.000000000000000000, 0.9659258262890683122, 1.000000000000000000, 0.9659258262890683122, 1.000000000000000000, 0.9659258262890683122, 1.000000000000000000, 0.9659258262890683122, 1.000000000000000000, 0.9659258262890683122, 1.000000000000000000, 0.9659258262890683122, 1.000000000000000000, 0.9659258262890683122, 1.000000000000000000, 0.9659258262890683122, 1.000000000000000000, 0.9659258262890683122, 1.000000000000000000, 0.9659258262890683122, 1.000000000000000000, 0.9659258262890683122, 1.000000000000000000),
 ( 1.000000000000000000, 0.9659258262890683122, 1.000000000000000000, 0.9659258262890683122, 1.000000000000000000, 0.9659258262890683122, 1.000000000000000000, 0.9659258262890683122, 1.000000000000000000, 0.9659258262890683122, 1.000000000000000000, 0.9659258262890683122, 1.000000000000000000, 0.9659258262890683122, 1.000000000000000000, 0.9659258262890683122, 1.000000000000000000, 0.9659258262890683122, 1.000000000000000000, 0.9659258262890683122, 1.000000000000000000, 0.9659258262890683122, 1.000000000000000000, 0.9659258262890683122, 1.000000000000000000, 0.9659258262890683122, 1.000000000000000000, 0.9659258262890683122, 1.000000000000000000, 0.9659258262890683122, 1.000000000000000000, 0.9659258262890683122, 1.000000000000000000, 0.9659258262890683122, 1.000000000000000000, 0.9659258262890683122, 1.000000000000000000, 0.9659258262890683122, 1.000000000000000000, 0.9659258262890683122, 1.000000000000000000, 0.9659258262890683122, 1.000000000000000000, 0.9659258262890683122, 1.000000000000000000, 0.9659258262890683122, 1.000000000000000000, 0.9659258262890683122, 1.000000000000000000, 0.9659258262890683122, 1.000000000000000000, 0.9659258262890683122, 1.000000000000000000, 0.9659258262890683122, 1.000000000000000000, 0.9659258262890683122, 1.000000000000000000, 0.9659258262890683122, 1.000000000000000000, 0.9659258262890683122, 1.000000000000000000, 0.9659258262890683122, 1.000000000000000000, 0.9659258262890683122, 1.000000000000000000, 0.9659258262890683122, 1.000000000000000000, 0.9659258262890683122, 1.000000000000000000, 0.9659258262890683122, 1.000000000000000000, 0.9659258262890683122, 1.000000000000000000, 0.9659258262890683122, 1.000000000000000000, 0.9659258262890683122, 1.000000000000000000, 0.9659258262890683122, 1.000000000000000000, 0.9659258262890683122, 1.000000000000000000, 0.9659258262890683122, 1.000000000000000000, 0.9659258262890683122, 1.000000000000000000, 0.9659258262890683122, 1.000000000000000000, 0.9659258262890683122, 1.000000000000000000, 0.9659258262890683122, 1.000000000000000000, 0.9659258262890683122, 1.000000000000000000, 0.9659258262890683122, 1.000000000000000000, 0.9659258262890683122, 1.000000000000000000, 0.9659258262890683122, 1.000000000000000000, 0.9659258262890683122, 1.000000000000000000, 0.9659258262890683122, 1.000000000000000000, 0.9659258262890683122, 1.000000000000000000, 0.9659258262890683122, 1.000000000000000000, 0.9659258262890683122, 1.000000000000000000, 0.9659258262890683122, 1.000000000000000000, 0.9659258262890683122, 1.000000000000000000, 0.9659258262890683122, 1.000000000000000000, 0.9659258262890683122, 1.000000000000000000, 0.9659258262890683122, 1.000000000000000000, 0.9659258262890683122, 1.000000000000000000, 0.9659258262890683122, 1.000000000000000000, 0.9659258262890683122, 1.000000000000000000, 0.9659258262890683122, 1.000000000000000000, 0.9659258262890683122, 1.000000000000000000, 0.9659258262890683122, 1.000000000000000000, 0.9659258262890683122, 1.000000000000000000, 0.9659258262890683122, 1.000000000000000000, 0.9659258262890683122, 1.000000000000000000, 0.9659258262890683122, 1.000000000000000000, 0.9659258262890683122, 1.000000000000000000, 0.9659258262890683122, 1.000000000000000000, 0.9659258262890683122, 1.000000000000000000, 0.9659258262890683122, 1.000000000000000000, 0.9659258262890683122, 1.000000000000000000, 0.9659258262890683122, 1.000000000000000000, 0.9659258262890683122, 1.000000000000000000, 0.9659258262890683122, 1.000000000000000000, 0.9659258262890683122, 1.000000000000000000, 0.9659258262890683122, 1.000000000000000000, 0.9659258262890683122, 1.000000000000000000, 0.9659258262890683122, 1.000000000000000000, 0.9659258262890683122, 1.000000000000000000, 0.9659258262890683122, 1.000000000000000000, 0.9659258262890683122, 1.000000000000000000, 0.9659258262890683122, 1.000000000000000000, 0.9659258262890683122, 1.000000000000000000, 0.9659258262890683122, 1.000000000000000000, 0.9659258262890683122, 1.000000000000000000, 0.9659258262890683122, 1.000000000000000000, 0.9659258262890683122, 1.000000000000000000, 0.9659258262890683122, 1.000000000000000000, 0.9659258262890683122, 1.000000000000000000, 0.9659258262890683122, 1.000000000000000000, 0.9659258262890683122, 1.000000000000000000, 0.9659258262890683122, 1.000000000000000000, 0.9659258262890683122, 1.000000000000000000, 0.9659258262890683122, 1.000000000000000000, 0.9659258262890683122, 1.000000000000000000, 0.9659258262890683122, 1.000000000000000000, 0.9659258262890683122, 1.000000000000000000, 0.9659258262890683122, 1.000000000000000000, 0.9659258262890683122, 1.000000000000000000, 0.9659258262890683122, 1.000000000000000000, 0.9659258262890683122, 1.000000000000000000, 0.9659258262890683122, 1.000000000000000000, 0.9659258262890683122, 1.000000000000000000, 0.9659258262890683122, 1.000000000000000000, 0.9659258262890683122, 1.000000000000000000, 0.9659258262890683122, 1.000000000000000000, 0.9659258262890683122, 1.000000000000000000, 0.9659258262890683122, 1.000000000000000000, 0.9659258262890683122, 1.000000000000000000, 0.9659258262890683122, 1.000000000000000000, 0.9659258262890683122, 1.000000000000000000, 0.9659258262890683122, 1.000000000000000000, 0.9659258262890683122, 1.000000000000000000, 0.9659258262890683122, 1.000000000000000000, 0.9659258262890683122, 1.000000000000000000, 0.9659258262890683122, 1.000000000000000000, 0.9659258262890683122, 1.000000000000000000, 0.9659258262890683122, 1.000000000000000000, 0.9659258262890683122, 1.000000000000000000, 0.9659258262890683122, 1.000000000000000000, 0.9659258262890683122, 1.000000000000000000, 0.9659258262890683122, 1.000000000000000000, 0.9659258262890683122, 1.000000000000000000, 0.9659258262890683122, 1.000000000000000000, 0.9659258262890683122, 1.000000000000000000, 0.9659258262890683122, 1.000000000000000000, 0.9659258262890683122, 1.000000000000000000, 0.9659258262890683122, 1.000000000000000000, 0.9659258262890683122, 1.000000000000000000, 0.9659258262890683122, 1.000000000000000000, 0.9659258262890683122, 1.000000000000000000, 0.9659258262890683122, 1.000000000000000000, 0.9659258262890683122, 1.000000000000000000, 0.9659258262890683122, 1.000000000000000000, 0.9659258262890683122, 1.000000000000000000, 0.9659258262890683122, 1.000000000000000000, 0.9659258262890683122, 1.000000000000000000, 0.9659258262890683122, 1.000000000000000000, 0.9659258262890683122, 1.000000000000000000, 0.9659258262890683122, 1.000000000000000000, 0.9659258262890683122, 1.000000000000000000, 0.9659258262890683122, 1.000000000000000000, 0.9659258262890683122, 1.000000000000000000, 0.9659258262890683122, 1.000000000000000000, 0.9659258262890683122, 1.000000000000000000, 0.9659258262890683122, 1.000000000000000000, 0.9659258262890683122, 1.000000000000000000, 0.9659258262890683122, 1.000000000000000000, 0.9659258262890683122, 1.000000000000000000, 0.9659258262890683122, 1.000000000000000000, 0.9659258262890683122, 1.000000000000000000, 0.9659258262890683122, 1.000000000000000000, 0.9659258262890683122, 1.000000000000000000, 0.9659258262890683122, 1.000000000000000000, 0.9659258262890683122, 1.000000000000000000, 0.9659258262890683122, 1.000000000000000000, 0.9659258262890683122, 1.000000000000000000, 0.9659258262890683122, 1.000000000000000000, 0.9659258262890683122, 1.000000000000000000, 0.9659258262890683122, 1.000000000000000000, 0.9659258262890683122, 1.000000000000000000, 0.9659258262890683122, 1.000000000000000000, 0.9659258262890683122, 1.000000000000000000, 0.9659258262890683122, 1.000000000000000000, 0.9659258262890683122, 1.000000000000000000, 0.9659258262890683122, 1.000000000000000000, 0.9659258262890683122, 1.000000000000000000, 0.9659258262890683122, 1.000000000000000000, 0.9659258262890683122, 1.000000000000000000, 0.9659258262890683122, 1.000000000000000000, 0.9659258262890683122, 1.000000000000000000, 0.9659258262890683122, 1.000000000000000000, 0.9659258262890683122, 1.000000000000000000, 0.9659258262890683122, 1.000000000000000000, 0.9659258262890683122, 1.000000000000000000, 0.9659258262890683122, 1.000000000000000000, 0.9659258262890683122, 1.000000000000000000, 0.9659258262890683122, 1.000000000000000000, 0.9659258262890683122, 1.000000000000000000, 0.9659258262890683122, 1.000000000000000000, 0.9659258262890683122, 1.000000000000000000, 0.9659258262890683122, 1.000000000000000000, 0.9659258262890683122, 1.000000000000000000, 0.9659258262890683122, 1.000000000000000000, 0.9659258262890683122, 1.000000000000000000, 0.9659258262890683122, 1.000000000000000000, 0.9659258262890683122, 1.000000000000000000, 0.9659258262890683122, 1.000000000000000000, 0.9659258262890683122, 1.000000000000000000, 0.9659258262890683122, 1.000000000000000000, 0.9659258262890683122, 1.000000000000000000, 0.9659258262890683122, 1.000000000000000000, 0.9659258262890683122, 1.000000000000000000, 0.9659258262890683122, 1.000000000000000000, 0.9659258262890683122, 1.000000000000000000, 0.9659258262890683122, 1.000000000000000000, 0.9659258262890683122, 1.000000000000000000, 0.9659258262890683122, 1.000000000000000000, 0.9659258262890683122, 1.000000000000000000, 0.9659258262890683122, 1.000000000000000000, 0.9659258262890683122, 1.000000000000000000, 0.9659258262890683122, 1.000000000000000000, 0.9659258262890683122, 1.000000000000000000, 0.9659258262890683122, 1.000000000000000000, 0.9659258262890683122, 1.000000000000000000, 0.9659258262890683122, 1.000000000000000000, 0.9659258262890683122, 1.000000000000000000, 0.9659258262890683122, 1.000000000000000000, 0.9659258262890683122, 1.000000000000000000, 0.9659258262890683122, 1.000000000000000000, 0.9659258262890683122, 1.000000000000000000, 0.9659258262890683122, 1.000000000000000000, 0.9659258262890683122, 1.000000000000000000, 0.9659258262890683122, 1.000000000000000000, 0.9659258262890683122, 1.000000000000000000, 0.9659258262890683122, 1.000000000000000000, 0.9659258262890683122, 1.000000000000000000, 0.9659258262890683122, 1.000000000000000000, 0.9659258262890683122, 1.000000000000000000, 0.9659258262890683122, 1.000000000000000000, 0.9659258262890683122, 1.000000000000000000, 0.9659258262890683122, 1.000000000000000000, 0.9659258262890683122, 1.000000000000000000, 0.9659258262890683122, 1.000000000000000000, 0.9659258262890683122, 1.000000000000000000, 0.9659258262890683122, 1.000000000000000000, 0.9659258262890683122, 1.000000000000000000, 0.9659258262890683122, 1.000000000000000000, 0.9659258262890683122, 1.000000000000000000, 0.9659258262890683122, 1.000000000000000000, 0.9659258262890683122, 1.000000000000000000, 0.9659258262890683122, 1.000000000000000000, 0.9659258262890683122, 1.000000000000000000, 0.9659258262890683122, 1.000000000000000000, 0.9659258262890683122, 1.000000000000000000, 0.9659258262890683122, 1.000000000000000000, 0.9659258262890683122, 1.000000000000000000, 0.9659258262890683122, 1.000000000000000000, 0.9659258262890683122, 1.000000000000000000, 0.9659258262890683122, 1.000000000000000000, 0.9659258262890683122, 1.000000000000000000, 0.9659258262890683122, 1.000000000000000000, 0.9659258262890683122, 1.000000000000000000, 0.9659258262890683122, 1.000000000000000000, 0.9659258262890683122, 1.000000000000000000, 0.9659258262890683122, 1.000000000000000000, 0.9659258262890683122, 1.000000000000000000, 0.9659258262890683122, 1.000000000000000000, 0.9659258262890683122, 1.000000000000000000, 0.9659258262890683122, 1.000000000000000000, 0.9659258262890683122, 1.000000000000000000, 0.9659258262890683122, 1.000000000000000000, 0.9659258262890683122, 1.000000000000000000, 0.9659258262890683122, 1.000000000000000000, 0.9659258262890683122, 1.000000000000000000, 0.9659258262890683122, 1.000000000000000000, 0.9659258262890683122, 1.000000000000000000, 0.9659258262890683122, 1.000000000000000000, 0.9659258262890683122, 1.000000000000000000, 0.9659258262890683122, 1.000000000000000000, 0.9659258262890683122, 1.000000000000000000, 0.9659258262890683122, 1.000000000000000000, 0.9659258262890683122, 1.000000000000000000, 0.9659258262890683122, 1.000000000000000000, 0.9659258262890683122, 1.000000000000000000, 0.9659258262890683122, 1.000000000000000000, 0.9659258262890683122, 1.000000000000000000, 0.9659258262890683122, 1.000000000000000000, 0.9659258262890683122, 1.000000000000000000, 0.9659258262890683122, 1.000000000000000000, 0.9659258262890683122, 1.000000000000000000, 0.9659258262890683122, 1.000000000000000000, 0.9659258262890683122, 1.000000000000000000, 0.9659258262890683122, 1.000000000000000000, 0.9659258262890683122, 1.000000000000000000, 0.9659258262890683122, 1.000000000000000000, 0.9659258262890683122, 1.000000000000000000, 0.9659258262890683122, 1.000000000000000000, 0.9659258262890683122, 1.000000000000000000, 0.9659258262890683122, 1.000000000000000000, 0.9659258262890683122, 1.000000000000000000, 0.9659258262890683122, 1.000000000000000000, 0.9659258262890683122, 1.000000000000000000, 0.9659258262890683122, 1.000000000000000000, 0.9659258262890683122, 1.000000000000000000, 0.9659258262890683122, 1.000000000000000000, 0.9659258262890683122, 1.000000000000000000, 0.9659258262890683122, 1.000000000000000000, 0.9659258262890683122, 1.000000000000000000, 0.9659258262890683122, 1.000000000000000000, 0.9659258262890683122, 1.000000000000000000, 0.9659258262890683122, 1.000000000000000000, 0.9659258262890683122, 1.000000000000000000, 0.9659258262890683122, 1.000000000000000000, 0.9659258262890683122, 1.000000000000000000, 0.9659258262890683122, 1.000000000000000000, 0.9659258262890683122, 1.000000000000000000, 0.9659258262890683122, 1.000000000000000000, 0.9659258262890683122, 1.000000000000000000, 0.9659258262890683122, 1.000000000000000000, 0.9659258262890683122, 1.000000000000000000, 0.9659258262890683122, 1.000000000000000000, 0.9659258262890683122, 1.000000000000000000, 0.9659258262890683122, 1.000000000000000000, 0.9659258262890683122, 1.000000000000000000, 0.9659258262890683122, 1.000000000000000000, 0.9659258262890683122, 1.000000000000000000, 0.9659258262890683122, 1.000000000000000000, 0.9659258262890683122, 1.000000000000000000, 0.9659258262890683122, 1.000000000000000000, 0.9659258262890683122, 1.000000000000000000, 0.9659258262890683122, 1.000000000000000000, 0.9659258262890683122, 1.000000000000000000, 0.9659258262890683122, 1.000000000000000000, 0.9659258262890683122, 1.000000000000000000, 0.9659258262890683122, 1.000000000000000000, 0.9659258262890683122, 1.000000000000000000, 0.9659258262890683122, 1.000000000000000000, 0.9659258262890683122, 1.000000000000000000, 0.9659258262890683122, 1.000000000000000000, 0.9659258262890683122, 1.000000000000000000, 0.9659258262890683122, 1.000000000000000000, 0.9659258262890683122, 1.000000000000000000, 0.9659258262890683122, 1.000000000000000000, 0.9659258262890683122, 1.000000000000000000, 0.9659258262890683122, 1.000000000000000000, 0.9659258262890683122, 1.000000000000000000, 0.9659258262890683122, 1.000000000000000000, 0.9659258262890683122, 1.000000000000000000, 0.9659258262890683122, 1.000000000000000000, 0.9659258262890683122, 1.000000000000000000, 0.9659258262890683122, 1.000000000000000000, 0.9659258262890683122, 1.000000000000000000, 0.9659258262890683122, 1.000000000000000000, 0.9659258262890683122, 1.000000000000000000, 0.9659258262890683122, 1.000000000000000000, 0.9659258262890683122, 1.000000000000000000, 0.9659258262890683122, 1.000000000000000000, 0.9659258262890683122, 1.000000000000000000, 0.9659258262890683122, 1.000000000000000000, 0.9659258262890683122, 1.000000000000000000, 0.9659258262890683122, 1.000000000000000000, 0.9659258262890683122, 1.000000000000000000, 0.9659258262890683122, 1.000000000000000000, 0.9659258262890683122, 1.000000000000000000, 0.9659258262890683122, 1.000000000000000000, 0.9659258262890683122, 1.000000000000000000, 0.9659258262890683122, 1.000000000000000000) ) ) 
 REPRESENTATION_ITEM ( '' )  SURFACE ( )  );
#90881 = ORIENTED_EDGE ( 'NONE', *, *, #126807, .F. ) ;
#90882 = ORIENTED_EDGE ( 'NONE', *, *, #44385, .T. ) ;
#90883 = CARTESIAN_POINT ( 'NONE',  ( 72.53709685856478018, -3.054999999999998828, -5.291415217122919401 ) ) ;
#90884 = EDGE_LOOP ( 'NONE', ( #13758, #104164, #136099, #7546, #97663, #127248, #135390 ) ) ;
#90885 = FACE_OUTER_BOUND ( 'NONE', #28129, .T. ) ;
#90886 = ADVANCED_FACE ( 'NONE', ( #39488 ), #37339, .T. ) ;
#90887 = VECTOR ( 'NONE', #133115, 1000.000000000000000 ) ;
#90888 = EDGE_LOOP ( 'NONE', ( #115880, #22640, #49873, #138383 ) ) ;
#90889 = CARTESIAN_POINT ( 'NONE',  ( 0.000000000000000000, -11.35517001088072142, -1.126524801160109890 ) ) ;
#90890 = VECTOR ( 'NONE', #73670, 1000.000000000000000 ) ;
#90891 = CARTESIAN_POINT ( 'NONE',  ( 122.6250000000000000, -7.950000000000000178, -4.867971026610729436E-16 ) ) ;
#90892 = CARTESIAN_POINT ( 'NONE',  ( 3.758600742197928835, 21.72499999999999432, 5.000000000000000000 ) ) ;
#90893 = EDGE_CURVE ( 'NONE', #57216, #76385, #59130, .T. ) ;
#90894 = FILL_AREA_STYLE_COLOUR ( '', #41227 ) ;
#90895 = DIRECTION ( 'NONE',  ( -1.000000000000000000, -0.000000000000000000, -0.000000000000000000 ) ) ;
#90896 = PLANE ( 'NONE',  #109416 ) ;
#90897 = CARTESIAN_POINT ( 'NONE',  ( 6.160000000000001030, 2.055000000000001492, 2.516649172247811554E-16 ) ) ;
#90898 = ORIENTED_EDGE ( 'NONE', *, *, #71779, .T. ) ;
#90899 = ORIENTED_EDGE ( 'NONE', *, *, #107815, .T. ) ;
#90900 = LINE ( 'NONE', #32963, #86693 ) ;
#90901 = CARTESIAN_POINT ( 'NONE',  ( 20.27718569542926730, -21.72500000000000853, 5.000000000000000000 ) ) ;
#90902 = EDGE_LOOP ( 'NONE', ( #68235, #1699, #129259, #51144 ) ) ;
#90903 = VERTEX_POINT ( 'NONE', #26456 ) ;
#90904 = ORIENTED_EDGE ( 'NONE', *, *, #36182, .T. ) ;
#90905 = EDGE_CURVE ( 'NONE', #137076, #142844, #3254, .T. ) ;
#90906 = CARTESIAN_POINT ( 'NONE',  ( 27.27126352523142927, 4.472830434245838482, 4.472830434245842035 ) ) ;
#90907 = AXIS2_PLACEMENT_3D ( 'NONE', #130573, #11592, #55876 ) ;
#90908 = ORIENTED_EDGE ( 'NONE', *, *, #134238, .F. ) ;
#90909 = DIRECTION ( 'NONE',  ( -0.6830127018922180770, -0.6830127018922204085, -0.2588190451025213501 ) ) ;
#90910 = DIRECTION ( 'NONE',  ( 0.7071067811865487940, 0.7071067811865463515, 0.000000000000000000 ) ) ;
#90911 = CARTESIAN_POINT ( 'NONE',  ( 1.233736474768552860, 5.808823158059036373, 5.808823158059032821 ) ) ;
#90912 = CARTESIAN_POINT ( 'NONE',  ( 9.792893218813393474, -5.240707523384230626, 5.000000000000000000 ) ) ;
#90913 = ORIENTED_EDGE ( 'NONE', *, *, #92850, .T. ) ;
#90914 = CARTESIAN_POINT ( 'NONE',  ( -45.48921356237309510, -27.52281430457087197, 5.000000000000000000 ) ) ;
#90915 = CARTESIAN_POINT ( 'NONE',  ( -17.99999999999986855, -18.03360074219755660, 5.000000000000000000 ) ) ;
#90916 = DIRECTION ( 'NONE',  ( -0.7071067811865487940, 0.7071067811865463515, 0.000000000000000000 ) ) ;
#90917 = VECTOR ( 'NONE', #31370, 1000.000000000000000 ) ;
#90919 = ORIENTED_EDGE ( 'NONE', *, *, #48558, .F. ) ;
#90918 = DIRECTION ( 'NONE',  ( -1.000000000000000000, -1.224606353822377258E-16, -0.000000000000000000 ) ) ;
#90920 = VECTOR ( 'NONE', #101709, 1000.000000000000227 ) ;
#90921 = ORIENTED_EDGE ( 'NONE', *, *, #45482, .F. ) ;
#90922 = DIRECTION ( 'NONE',  ( -0.7071067811865486830, -0.7071067811865464625, -0.000000000000000000 ) ) ;
#90923 = CARTESIAN_POINT ( 'NONE',  ( 30.32816939922332367, -3.740707523384241728, 4.000000000000000000 ) ) ;
#90924 = VECTOR ( 'NONE', #139607, 1000.000000000000000 ) ;
#90925 = CARTESIAN_POINT ( 'NONE',  ( -7.433128002487371155, -21.74070752338405654, 6.915939825044092437 ) ) ;
#90927 = ORIENTED_EDGE ( 'NONE', *, *, #102486, .T. ) ;
#90926 = VECTOR ( 'NONE', #128506, 999.9999999999998863 ) ;
#90928 = DIRECTION ( 'NONE',  ( 1.000000000000000000, 0.000000000000000000, 0.000000000000000000 ) ) ;
#90929 = FACE_OUTER_BOUND ( 'NONE', #50255, .T. ) ;
#90930 = EDGE_CURVE ( 'NONE', #130856, #16952, #5385, .T. ) ;
#90931 = CARTESIAN_POINT ( 'NONE',  ( 34.92499999999998295, 11.81665438641033106, 4.500000000000000888 ) ) ;
#90932 = DIRECTION ( 'NONE',  ( 0.3543493200069163240, -0.000000000000000000, -0.9351131265310288487 ) ) ;
#90933 = DIRECTION ( 'NONE',  ( 0.6830127018922180770, -0.6830127018922204085, -0.2588190451025213501 ) ) ;
#90934 = VECTOR ( 'NONE', #87942, 999.9999999999998863 ) ;
#90935 = VECTOR ( 'NONE', #83132, 1000.000000000000227 ) ;
#90936 = DIRECTION ( 'NONE',  ( 0.7071067811865486830, -0.7071067811865464625, -0.000000000000000000 ) ) ;
#90937 = CARTESIAN_POINT ( 'NONE',  ( 13.37176554955607166, -8.240707523384193323, 11.38925528200749682 ) ) ;
#90938 = CARTESIAN_POINT ( 'NONE',  ( 21.04580628287044064, 5.278424836066143655, -3.047499999999997655 ) ) ;
#90940 = EDGE_CURVE ( 'NONE', #132371, #136694, #15530, .T. ) ;
#90939 = DIRECTION ( 'NONE',  ( 0.000000000000000000, -1.000000000000000000, 0.000000000000000000 ) ) ;
#90941 = CARTESIAN_POINT ( 'NONE',  ( 30.29974487139158867, -27.71228299555227537, 4.000000000000000000 ) ) ;
#90942 = ORIENTED_EDGE ( 'NONE', *, *, #2924, .T. ) ;
#90943 = ADVANCED_FACE ( 'NONE', ( #93846 ), #4627, .F. ) ;
#90944 = ORIENTED_EDGE ( 'NONE', *, *, #61549, .F. ) ;
#90945 = CARTESIAN_POINT ( 'NONE',  ( 28.49999999999980460, -13.53360074219760101, 5.000000000000000000 ) ) ;
#90946 = FACE_OUTER_BOUND ( 'NONE', #133744, .T. ) ;
#90947 = DIRECTION ( 'NONE',  ( 0.3543493200069162685, -0.000000000000000000, -0.9351131265310288487 ) ) ;
#90948 = AXIS2_PLACEMENT_3D ( 'NONE', #59753, #72078, #116250 ) ;
#90949 = CARTESIAN_POINT ( 'NONE',  ( -2.671830600776455178, -12.74070752338415602, 4.000000000000000000 ) ) ;
#90950 = CARTESIAN_POINT ( 'NONE',  ( -25.49999999999981526, 7.087461875839175640, 4.000000000000000000 ) ) ;
#90951 = CARTESIAN_POINT ( 'NONE',  ( 24.99507522778790758, -5.240707523384225297, 12.38332538355490442 ) ) ;
#90952 = ORIENTED_EDGE ( 'NONE', *, *, #76985, .T. ) ;
#90953 = LINE ( 'NONE', #1730, #14050 ) ;
#90954 = CARTESIAN_POINT ( 'NONE',  ( -13.49999999999990408, -10.04351517176479014, -1.623559851933856102 ) ) ;
#90955 = LINE ( 'NONE', #2464, #136199 ) ;
#90956 = CARTESIAN_POINT ( 'NONE',  ( 53.14126352523144448, 4.472830434245837594, 4.472830434245841147 ) ) ;
#90957 = ADVANCED_FACE ( 'NONE', ( #48936 ), #138072, .T. ) ;
#90958 = AXIS2_PLACEMENT_3D ( 'NONE', #57214, #125296, #47772 ) ;
#90959 = CARTESIAN_POINT ( 'NONE',  ( -20.81601139373100295, 28.73617430169773002, 5.000000000000000000 ) ) ;
#90960 = CARTESIAN_POINT ( 'NONE',  ( 5.671830600776431197, -3.740707523384244837, 4.000000000000000000 ) ) ;
#90961 = LINE ( 'NONE', #98002, #83465 ) ;
#90962 = AXIS2_PLACEMENT_3D ( 'NONE', #109075, #78614, #54036 ) ;
#90963 = ORIENTED_EDGE ( 'NONE', *, *, #62674, .T. ) ;
#90964 = FILL_AREA_STYLE_COLOUR ( '', #88252 ) ;
#90965 = ORIENTED_EDGE ( 'NONE', *, *, #34340, .F. ) ;
#90966 = AXIS2_PLACEMENT_3D ( 'NONE', #5370, #18372, #82964 ) ;
#90967 = DIRECTION ( 'NONE',  ( -1.000000000000000000, -1.224606353822377258E-16, -0.000000000000000000 ) ) ;
#90968 = AXIS2_PLACEMENT_3D ( 'NONE', #115012, #15690, #59974 ) ;
#90969 = CARTESIAN_POINT ( 'NONE',  ( -75.18398860626899705, 28.73617430169839793, 5.000000000000000000 ) ) ;
#90970 = CARTESIAN_POINT ( 'NONE',  ( -14.67183060077636725, 17.25929247661554200, 4.000000000000000000 ) ) ;
#90971 = CARTESIAN_POINT ( 'NONE',  ( -26.51078643762690845, -27.52281430457036748, 5.000000000000000000 ) ) ;
#90972 = DIRECTION ( 'NONE',  ( 0.000000000000000000, 0.000000000000000000, 1.000000000000000000 ) ) ;
#90973 = DIRECTION ( 'NONE',  ( -0.7071067811865487940, 0.7071067811865463515, -0.000000000000000000 ) ) ;
#90974 = ORIENTED_EDGE ( 'NONE', *, *, #141269, .T. ) ;
#90975 = ORIENTED_EDGE ( 'NONE', *, *, #85187, .F. ) ;
#90976 = CARTESIAN_POINT ( 'NONE',  ( 30.29974487139158867, -27.71228299555227537, 4.000000000000000000 ) ) ;
#90977 = PLANE ( 'NONE',  #67778 ) ;
#90978 = UNCERTAINTY_MEASURE_WITH_UNIT (LENGTH_MEASURE( 1.000000000000000082E-05 ), #122113, 'distance_accuracy_value', 'NONE');
#90979 = CARTESIAN_POINT ( 'NONE',  ( -69.18398860626899705, 28.73617430169835529, 5.000000000000000000 ) ) ;
#90980 = DIRECTION ( 'NONE',  ( 0.7071067811865486830, -0.7071067811865464625, -0.000000000000000000 ) ) ;
#90982 = EDGE_CURVE ( 'NONE', #62013, #135631, #137369, .T. ) ;
#90981 = AXIS2_PLACEMENT_3D ( 'NONE', #103731, #81324, #137836 ) ;
#90983 = CARTESIAN_POINT ( 'NONE',  ( 76.20419371712955581, -6.884901960086285300, -3.975000000000000089 ) ) ;
#90984 = PLANE ( 'NONE',  #37003 ) ;
#90985 = ADVANCED_FACE ( 'NONE', ( #91702 ), #126458, .T. ) ;
#90986 = CARTESIAN_POINT ( 'NONE',  ( 180.4193221990229574, -52.14999999999999147, -40.92499999999998295 ) ) ;
#90987 = VERTEX_POINT ( 'NONE', #6080 ) ;
#90988 = CARTESIAN_POINT ( 'NONE',  ( 72.02083333333334281, 7.949999999999999289, 2.130196079827431532 ) ) ;
#90989 = CARTESIAN_POINT ( 'NONE',  ( 54.18398860626899705, 28.73617430169825226, 5.000000000000000000 ) ) ;
#90990 = EDGE_CURVE ( 'NONE', #12370, #130351, #60546, .T. ) ;
#90991 = CARTESIAN_POINT ( 'NONE',  ( -33.29974487139158867, -27.71228299555229313, 4.000000000000000000 ) ) ;
#90993 = VECTOR ( 'NONE', #70557, 1000.000000000000000 ) ;
#90992 = LINE ( 'NONE', #35908, #123875 ) ;
#90994 = VECTOR ( 'NONE', #96278, 1000.000000000000227 ) ;
#90995 = ORIENTED_EDGE ( 'NONE', *, *, #115451, .T. ) ;
#90996 = ADVANCED_FACE ( 'NONE', ( #105423 ), #127179, .F. ) ;
#90997 = EDGE_CURVE ( 'NONE', #82989, #37103, #36096, .T. ) ;
#90998 = LINE ( 'NONE', #14829, #5076 ) ;
#90999 = PLANE ( 'NONE',  #51368 ) ;
#91000 = CARTESIAN_POINT ( 'NONE',  ( 67.22959685856476142, -6.110000000000000320, -1.637169565754161393 ) ) ;
#91001 = DIRECTION ( 'NONE',  ( -0.7071067811865486830, -0.7071067811865464625, 0.000000000000000000 ) ) ;
#91002 = VERTEX_POINT ( 'NONE', #98143 ) ;
#91003 = ORIENTED_EDGE ( 'NONE', *, *, #33946, .T. ) ;
#91004 = VECTOR ( 'NONE', #112235, 1000.000000000000000 ) ;
#91005 = FACE_OUTER_BOUND ( 'NONE', #62534, .T. ) ;
#91006 = LINE ( 'NONE', #80138, #41993 ) ;
#91007 = EDGE_CURVE ( 'NONE', #54885, #15309, #142367, .T. ) ;
#91008 = CARTESIAN_POINT ( 'NONE',  ( 43.29166666666665719, 3.975000000000003642, -6.884901960086285300 ) ) ;
#91009 = EDGE_CURVE ( 'NONE', #91146, #94083, #118442, .T. ) ;
#91010 = CARTESIAN_POINT ( 'NONE',  ( 26.99999999999981881, 17.58746187583906107, 4.000000000000000000 ) ) ;
#91012 = ORIENTED_EDGE ( 'NONE', *, *, #13072, .T. ) ;
#91011 = DIRECTION ( 'NONE',  ( -0.7071067811865487940, 0.7071067811865463515, -0.000000000000000000 ) ) ;
#91013 = PLANE ( 'NONE',  #50707 ) ;
#91014 = DIRECTION ( 'NONE',  ( 0.6830127018922180770, -0.6830127018922204085, -0.2588190451025213501 ) ) ;
#91015 = AXIS2_PLACEMENT_3D ( 'NONE', #34646, #2706, #12859 ) ;
#91016 = LINE ( 'NONE', #91696, #37817 ) ;
#91017 = SURFACE_SIDE_STYLE ('',( #42521 ) ) ;
#91018 = VERTEX_POINT ( 'NONE', #8230 ) ;
#91019 = ADVANCED_FACE ( 'NONE', ( #52473 ), #130792, .T. ) ;
#91020 = ORIENTED_EDGE ( 'NONE', *, *, #130962, .T. ) ;
#91021 = CARTESIAN_POINT ( 'NONE',  ( 52.06293019189809712, 1.637169565754157174, 6.110000000000002984 ) ) ;
#91022 = ORIENTED_EDGE ( 'NONE', *, *, #109184, .F. ) ;
#91023 = DIRECTION ( 'NONE',  ( -0.7071067811865486830, -0.7071067811865464625, 0.000000000000000000 ) ) ;
#91024 = CARTESIAN_POINT ( 'NONE',  ( -3.299744871391591339, -27.71228299555208352, 4.000000000000000000 ) ) ;
#91025 = CYLINDRICAL_SURFACE ( 'NONE', #128956, 0.5000000000000004441 ) ;
#91026 = DIRECTION ( 'NONE',  ( 1.000000000000000000, 0.000000000000000000, 0.000000000000000000 ) ) ;
#91027 = CARTESIAN_POINT ( 'NONE',  ( 24.18398860626899705, 28.73617430169804265, 5.000000000000000000 ) ) ;
#91028 = ORIENTED_EDGE ( 'NONE', *, *, #102266, .F. ) ;
#91030 = ADVANCED_FACE ( 'NONE', ( #64080 ), #32162, .F. ) ;
#91029 = VERTEX_POINT ( 'NONE', #96659 ) ;
#91031 = AXIS2_PLACEMENT_3D ( 'NONE', #40491, #93422, #52064 ) ;
#91032 = CARTESIAN_POINT ( 'NONE',  ( 28.17183060077626777, -8.240707523384203981, 4.000000000000000000 ) ) ;
#91033 = CARTESIAN_POINT ( 'NONE',  ( -16.63174071259636833, 0.4494130005253863525, -33.70036845157063254 ) ) ;
#91034 = AXIS2_PLACEMENT_3D ( 'NONE', #121203, #111023, #77030 ) ;
#91035 = VECTOR ( 'NONE', #69138, 1000.000000000000000 ) ;
#91036 = EDGE_LOOP ( 'NONE', ( #38468, #83417, #28247, #38238 ) ) ;
#91037 =( NAMED_UNIT ( * ) SI_UNIT ( $, .STERADIAN. ) SOLID_ANGLE_UNIT ( ) );
#91039 = LINE ( 'NONE', #77320, #129008 ) ;
#91038 = AXIS2_PLACEMENT_3D ( 'NONE', #16899, #61849, #82884 ) ;
#91040 = ADVANCED_FACE ( 'NONE', ( #75678 ), #117702, .T. ) ;
#91041 = DIRECTION ( 'NONE',  ( -0.7071067811865486830, -0.7071067811865464625, 0.000000000000000000 ) ) ;
#91042 = AXIS2_PLACEMENT_3D ( 'NONE', #92958, #15360, #83535 ) ;
#91043 = ORIENTED_EDGE ( 'NONE', *, *, #48182, .T. ) ;
#91044 = FACE_BOUND ( 'NONE', #107242, .T. ) ;
#91045 = DIRECTION ( 'NONE',  ( -0.7071067811865487940, 0.7071067811865463515, -0.000000000000000000 ) ) ;
#91046 = ADVANCED_FACE ( 'NONE', ( #140905 ), #40902, .T. ) ;
#91047 = FACE_OUTER_BOUND ( 'NONE', #119709, .T. ) ;
#91048 = CARTESIAN_POINT ( 'NONE',  ( 37.41252705046288440, -7.949999999999998401, -4.867971026610728450E-16 ) ) ;
#91049 = DIRECTION ( 'NONE',  ( 0.000000000000000000, -1.000000000000000000, 0.000000000000000000 ) ) ;
#91050 = LINE ( 'NONE', #79488, #67504 ) ;
#91052 = ADVANCED_FACE ( 'NONE', ( #95977 ), #74985, .T. ) ;
#91051 = DIRECTION ( 'NONE',  ( 1.000000000000000000, -3.383823774074210379E-26, 3.766053779379805060E-26 ) ) ;
#91053 = EDGE_LOOP ( 'NONE', ( #111573, #80318, #13182, #1604 ) ) ;
#91054 = VECTOR ( 'NONE', #100216, 1000.000000000000000 ) ;
#91055 = ORIENTED_EDGE ( 'NONE', *, *, #51734, .T. ) ;
#91056 = CARTESIAN_POINT ( 'NONE',  ( 99.07876352523145158, -7.482591942790325086E-16, 6.109999999999998543 ) ) ;
#91057 = ORIENTED_EDGE ( 'NONE', *, *, #122710, .F. ) ;
#91058 = CARTESIAN_POINT ( 'NONE',  ( -7.773258392821613683, -11.24070752338416135, 18.24660765846980937 ) ) ;
#91059 = ORIENTED_EDGE ( 'NONE', *, *, #26051, .F. ) ;
#91060 = CARTESIAN_POINT ( 'NONE',  ( -34.92500000000001137, -21.72500000000000142, 4.500000000000000888 ) ) ;
#91061 = DIRECTION ( 'NONE',  ( -0.000000000000000000, -1.000000000000000000, -0.000000000000000000 ) ) ;
#91062 = LINE ( 'NONE', #69296, #44856 ) ;
#91063 = ORIENTED_EDGE ( 'NONE', *, *, #114816, .F. ) ;
#91064 = DIRECTION ( 'NONE',  ( 0.000000000000000000, -1.000000000000000000, 0.000000000000000000 ) ) ;
#91065 = CARTESIAN_POINT ( 'NONE',  ( 18.17159235450331778, 9.902892378096218942E-16, 0.000000000000000000 ) ) ;
#91066 = VECTOR ( 'NONE', #5990, 1000.000000000000000 ) ;
#91067 = EDGE_CURVE ( 'NONE', #140445, #2581, #56434, .T. ) ;
#91068 = CARTESIAN_POINT ( 'NONE',  ( 25.40000000000001634, 7.525090494501557536, -2.550389573741807858 ) ) ;
#91069 = CARTESIAN_POINT ( 'NONE',  ( -14.99999999999989875, 2.342191155542430181, -5.001666872980051970 ) ) ;
#91070 = LINE ( 'NONE', #78751, #106963 ) ;
#91071 = ORIENTED_EDGE ( 'NONE', *, *, #93219, .T. ) ;
#91072 = DIRECTION ( 'NONE',  ( -0.7071067811865486830, -0.7071067811865464625, 0.000000000000000000 ) ) ;
#91073 = CARTESIAN_POINT ( 'NONE',  ( 0.000000000000000000, 0.000000000000000000, 5.000000000000000000 ) ) ;
#91074 = VECTOR ( 'NONE', #44602, 1000.000000000000000 ) ;
#91075 = ORIENTED_EDGE ( 'NONE', *, *, #28274, .F. ) ;
#91076 = VERTEX_POINT ( 'NONE', #11085 ) ;
#91077 = EDGE_CURVE ( 'NONE', #96885, #63562, #135084, .T. ) ;
#91078 = ORIENTED_EDGE ( 'NONE', *, *, #28799, .T. ) ;
#91079 = CARTESIAN_POINT ( 'NONE',  ( 54.54209685856477563, 5.291415217122923842, -3.054999999999996163 ) ) ;
#91080 = ORIENTED_EDGE ( 'NONE', *, *, #5050, .T. ) ;
#91081 = VECTOR ( 'NONE', #46880, 1000.000000000000000 ) ;
#91082 = MECHANICAL_DESIGN_GEOMETRIC_PRESENTATION_REPRESENTATION (  '', ( #56340 ), #128124 ) ;
#91083 = CARTESIAN_POINT ( 'NONE',  ( 8.358306282870437087, -1.633150327867689988, 6.094999999999989981 ) ) ;
#91084 = CARTESIAN_POINT ( 'NONE',  ( 94.06293019189810423, 1.637169565754157174, 6.110000000000002984 ) ) ;
#91085 = CARTESIAN_POINT ( 'NONE',  ( -34.45011844616454511, 19.51628081163728723, 5.000000000000000888 ) ) ;
#91086 = ORIENTED_EDGE ( 'NONE', *, *, #22940, .T. ) ;
#91087 = CARTESIAN_POINT ( 'NONE',  ( 34.92499999999998295, 9.691175483026997384, 9.749534648445568052 ) ) ;
#91088 = ORIENTED_EDGE ( 'NONE', *, *, #92771, .F. ) ;
#91089 = SURFACE_SIDE_STYLE ('',( #104044 ) ) ;
#91090 = VECTOR ( 'NONE', #57844, 1000.000000000000000 ) ;
#91091 = PLANE ( 'NONE',  #121132 ) ;
#91092 = ORIENTED_EDGE ( 'NONE', *, *, #125911, .F. ) ;
#91093 =( BOUNDED_CURVE ( )  B_SPLINE_CURVE ( 3, ( #7055, #71659, #4911, #73103 ),
 .UNSPECIFIED., .F., .F. ) 
 B_SPLINE_CURVE_WITH_KNOTS ( ( 4, 4 ),
 ( 2.001653308786169649, 3.503810798801449522 ),
 .UNSPECIFIED. ) 
 CURVE ( )  GEOMETRIC_REPRESENTATION_ITEM ( )  RATIONAL_B_SPLINE_CURVE ( ( 1.000000000000000000, 0.8206354192515243895, 0.8206354192515243895, 1.000000000000000000 ) ) 
 REPRESENTATION_ITEM ( '' )  );
#91094 = LINE ( 'NONE', #122245, #28302 ) ;
#91095 = DIRECTION ( 'NONE',  ( -0.000000000000000000, 0.3543493200069153248, 0.9351131265310292928 ) ) ;
#91096 = FACE_OUTER_BOUND ( 'NONE', #24826, .T. ) ;
#91097 = ORIENTED_EDGE ( 'NONE', *, *, #35784, .F. ) ;
#91098 = CARTESIAN_POINT ( 'NONE',  ( -25.39999999999996305, 3.061616997868383141E-16, -2.500000000000000000 ) ) ;
#91100 = ORIENTED_EDGE ( 'NONE', *, *, #60228, .T. ) ;
#91099 = EDGE_CURVE ( 'NONE', #2653, #98498, #21290, .T. ) ;
#91101 = ORIENTED_EDGE ( 'NONE', *, *, #52016, .F. ) ;
#91102 = VERTEX_POINT ( 'NONE', #44505 ) ;
#91103 = LINE ( 'NONE', #45464, #91104 ) ;
#91104 = VECTOR ( 'NONE', #133871, 1000.000000000000227 ) ;
#91105 = LINE ( 'NONE', #16337, #111742 ) ;
#91107 = EDGE_CURVE ( 'NONE', #76586, #81442, #107853, .T. ) ;
#91106 = CARTESIAN_POINT ( 'NONE',  ( 11.30840764549667554, -3.851859888774471706E-31, 2.500000000000001332 ) ) ;
#91108 = DIRECTION ( 'NONE',  ( 1.000000000000000000, 0.000000000000000000, 0.000000000000000000 ) ) ;
#91109 = ADVANCED_FACE ( 'NONE', ( #13239 ), #121304, .T. ) ;
#91110 = DIRECTION ( 'NONE',  ( 0.7071067811865487940, -0.7071067811865463515, 0.000000000000000000 ) ) ;
#91111 = AXIS2_PLACEMENT_3D ( 'NONE', #96134, #62117, #43928 ) ;
#91112 = ORIENTED_EDGE ( 'NONE', *, *, #97878, .F. ) ;
#91113 = CARTESIAN_POINT ( 'NONE',  ( 1.042387978378689573, 4.202752102959690472E-16, 0.000000000000000000 ) ) ;
#91114 = CARTESIAN_POINT ( 'NONE',  ( 24.33290314143522437, -3.967499999999994476, 6.871911579029513106 ) ) ;
#91115 = LINE ( 'NONE', #78085, #97074 ) ;
#91116 = VECTOR ( 'NONE', #94070, 1000.000000000000227 ) ;
#91117 = CARTESIAN_POINT ( 'NONE',  ( 28.04515773336648721, -21.74070752338406365, 21.72585301388591361 ) ) ;
#91118 = EDGE_CURVE ( 'NONE', #123251, #53550, #45916, .T. ) ;
#91119 = CARTESIAN_POINT ( 'NONE',  ( 0.7307956238753654521, 0.3999999999999995226, 2.467792535850613866 ) ) ;
#91120 = ORIENTED_EDGE ( 'NONE', *, *, #7377, .F. ) ;
#91121 = ORIENTED_EDGE ( 'NONE', *, *, #15831, .F. ) ;
#91122 = EDGE_LOOP ( 'NONE', ( #52061, #93149, #132666 ) ) ;
#91123 = CARTESIAN_POINT ( 'NONE',  ( 28.00000000000002487, -52.14999999999999147, -34.92499999999976978 ) ) ;
#91124 = DIRECTION ( 'NONE',  ( 0.6830127018922180770, -0.6830127018922204085, -0.2588190451025213501 ) ) ;
#91125 = UNCERTAINTY_MEASURE_WITH_UNIT (LENGTH_MEASURE( 1.000000000000000082E-05 ), #138315, 'distance_accuracy_value', 'NONE');
#91126 = DIRECTION ( 'NONE',  ( 1.000000000000000000, 0.000000000000000000, 0.000000000000000000 ) ) ;
#91127 = CARTESIAN_POINT ( 'NONE',  ( 34.45011844616451668, -11.99769585840593322, 5.000000000000000000 ) ) ;
#91128 = FACE_OUTER_BOUND ( 'NONE', #20607, .T. ) ;
#91129 = EDGE_CURVE ( 'NONE', #83991, #9245, #33619, .T. ) ;
#91130 = AXIS2_PLACEMENT_3D ( 'NONE', #41469, #20419, #131348 ) ;
#91131 = LINE ( 'NONE', #1897, #48421 ) ;
#91132 = CARTESIAN_POINT ( 'NONE',  ( 34.49999999999975842, 16.46425560840032531, 4.994342998332160555 ) ) ;
#91133 = CARTESIAN_POINT ( 'NONE',  ( 32.99451991528749062, 28.92564299267960948, 4.000000000000000000 ) ) ;
#91134 = CARTESIAN_POINT ( 'NONE',  ( 20.99065804761471199, 4.584330080086930965E-16, 0.000000000000000000 ) ) ;
#91135 = DIRECTION ( 'NONE',  ( -0.7071067811865486830, -0.7071067811865464625, 0.000000000000000000 ) ) ;
#91136 = DIRECTION ( 'NONE',  ( 0.7071067811865487940, 0.7071067811865463515, 0.000000000000000000 ) ) ;
#91137 = VERTEX_POINT ( 'NONE', #90100 ) ;
#91138 = EDGE_CURVE ( 'NONE', #10476, #91002, #109719, .T. ) ;
#91139 = DIRECTION ( 'NONE',  ( -0.3543493200069163240, 0.000000000000000000, -0.9351131265310288487 ) ) ;
#91140 = ORIENTED_EDGE ( 'NONE', *, *, #9729, .T. ) ;
#91141 = FACE_OUTER_BOUND ( 'NONE', #59551, .T. ) ;
#91143 = ORIENTED_EDGE ( 'NONE', *, *, #66779, .T. ) ;
#91142 = LINE ( 'NONE', #103391, #101986 ) ;
#91144 = LINE ( 'NONE', #79585, #118065 ) ;
#91145 = LINE ( 'NONE', #123769, #125953 ) ;
#91146 = VERTEX_POINT ( 'NONE', #32909 ) ;
#91147 = CARTESIAN_POINT ( 'NONE',  ( -44.99451991528749772, 28.92564299267969474, 4.000000000000000000 ) ) ;
#91148 = ORIENTED_EDGE ( 'NONE', *, *, #135363, .T. ) ;
#91149 = CARTESIAN_POINT ( 'NONE',  ( -24.48921356237309510, -27.52281430457072631, 5.000000000000000000 ) ) ;
#91150 = UNCERTAINTY_MEASURE_WITH_UNIT (LENGTH_MEASURE( 1.000000000000000082E-05 ), #71137, 'distance_accuracy_value', 'NONE');
#91151 = ORIENTED_EDGE ( 'NONE', *, *, #30777, .F. ) ;
#91152 = DIRECTION ( 'NONE',  ( -0.000000000000000000, 0.3543493200069153248, 0.9351131265310292928 ) ) ;
#91153 = CARTESIAN_POINT ( 'NONE',  ( 107.2666937171295558, -7.949999999999999289, 2.130196079827424427 ) ) ;
#91154 = PLANE ( 'NONE',  #83275 ) ;
#91155 = CIRCLE ( 'NONE', #74913, 5.968999999999998529 ) ;
#91156 = LINE ( 'NONE', #135377, #2226 ) ;
#91157 = EDGE_LOOP ( 'NONE', ( #97242, #82236, #46317, #114293 ) ) ;
#91158 = FACE_OUTER_BOUND ( 'NONE', #107061, .T. ) ;
#91160 = ADVANCED_FACE ( 'NONE', ( #77130 ), #23412, .F. ) ;
#91159 = DIRECTION ( 'NONE',  ( 0.6830127018922181881, 0.6830127018922202975, -0.2588190451025214056 ) ) ;
#91161 = LINE ( 'NONE', #46973, #76283 ) ;
#91162 = CARTESIAN_POINT ( 'NONE',  ( 16.18750000000000000, 4.461849672132297329, -4.461849672132302658 ) ) ;
#91163 = LINE ( 'NONE', #112881, #70025 ) ;
#91164 = CARTESIAN_POINT ( 'NONE',  ( 39.18398860626899705, 28.73617430169814568, 5.000000000000000000 ) ) ;
#91165 = CARTESIAN_POINT ( 'NONE',  ( -7.228506771386599361, 20.25929247661551003, 7.808871592221752422 ) ) ;
#91166 = EDGE_LOOP ( 'NONE', ( #6329, #5724, #67719, #137747 ) ) ;
#91167 = VECTOR ( 'NONE', #78597, 1000.000000000000227 ) ;
#91168 = EDGE_CURVE ( 'NONE', #80483, #57964, #66939, .T. ) ;
#91169 = EDGE_CURVE ( 'NONE', #136490, #64361, #21985, .T. ) ;
#91170 = DIRECTION ( 'NONE',  ( 0.7071067811865487940, -0.7071067811865463515, 0.000000000000000000 ) ) ;
#91171 = ORIENTED_EDGE ( 'NONE', *, *, #127176, .T. ) ;
#91172 = COLOUR_RGB ( '', 0.08235294, 0.09019608, 0.10196078) ;
#91173 = CARTESIAN_POINT ( 'NONE',  ( 96.83376352523144703, 6.110000000000001208, 1.122388791418549305E-15 ) ) ;
#91174 = DIRECTION ( 'NONE',  ( 1.000000000000000000, 0.000000000000000000, 0.000000000000000000 ) ) ;
#91175 = DIRECTION ( 'NONE',  ( 0.000000000000000000, 0.000000000000000000, 1.000000000000000000 ) ) ;
#91176 = DIRECTION ( 'NONE',  ( 1.000000000000000000, 0.000000000000000000, 0.000000000000000000 ) ) ;
#91177 = DIRECTION ( 'NONE',  ( -0.7071067811865486830, -0.7071067811865464625, 0.000000000000000000 ) ) ;
#91178 = ORIENTED_EDGE ( 'NONE', *, *, #5857, .T. ) ;
#91179 = EDGE_CURVE ( 'NONE', #142746, #62063, #10389, .T. ) ;
#91180 = DIRECTION ( 'NONE',  ( 0.5735764363510453823, -0.8191520442889923537, 1.003171929053525486E-16 ) ) ;
#91181 = VECTOR ( 'NONE', #48141, 1000.000000000000000 ) ;
#91182 = LINE ( 'NONE', #89718, #139172 ) ;
#91183 = EDGE_CURVE ( 'NONE', #88472, #12703, #56095, .T. ) ;
#91184 = ORIENTED_EDGE ( 'NONE', *, *, #28185, .T. ) ;
#91185 = PLANE ( 'NONE',  #120291 ) ;
#91186 = EDGE_CURVE ( 'NONE', #71167, #98841, #24145, .T. ) ;
#91187 = LINE ( 'NONE', #135402, #3100 ) ;
#91189 = ORIENTED_EDGE ( 'NONE', *, *, #38338, .T. ) ;
#91188 = CARTESIAN_POINT ( 'NONE',  ( 27.29974487139158512, -27.71228299555225405, 4.000000000000000000 ) ) ;
#91190 = CYLINDRICAL_SURFACE ( 'NONE', #62525, 2.500000000000000444 ) ;
#91191 = DIRECTION ( 'NONE',  ( -0.7071067811865487940, 0.7071067811865463515, -0.000000000000000000 ) ) ;
#91192 = PLANE ( 'NONE',  #19167 ) ;
#91193 = CARTESIAN_POINT ( 'NONE',  ( 17.39159235450332019, -2.500000000000000000, 3.061616997868384127E-16 ) ) ;
#91194 = VECTOR ( 'NONE', #24416, 1000.000000000000000 ) ;
#91195 =( NAMED_UNIT ( * ) SI_UNIT ( $, .STERADIAN. ) SOLID_ANGLE_UNIT ( ) );
#91196 = VECTOR ( 'NONE', #44548, 1000.000000000000000 ) ;
#91197 = ORIENTED_EDGE ( 'NONE', *, *, #105664, .T. ) ;
#91198 = ORIENTED_EDGE ( 'NONE', *, *, #18258, .T. ) ;
#91199 = VERTEX_POINT ( 'NONE', #89398 ) ;
#91201 = ADVANCED_FACE ( 'NONE', ( #133629 ), #34306, .T. ) ;
#91200 = CARTESIAN_POINT ( 'NONE',  ( 78.75043019189810423, 3.055000000000002824, -5.291415217122919401 ) ) ;
#91202 = VECTOR ( 'NONE', #121708, 1000.000000000000000 ) ;
#91203 = VERTEX_POINT ( 'NONE', #68400 ) ;
#91204 = EDGE_CURVE ( 'NONE', #59763, #109094, #45417, .T. ) ;
#91205 = DIRECTION ( 'NONE',  ( 0.7071067811865486830, -0.7071067811865464625, -0.000000000000000000 ) ) ;
#91206 = CARTESIAN_POINT ( 'NONE',  ( 13.49999999999991296, 0.05218569542916363935, 5.000000000000000000 ) ) ;
#91207 = VECTOR ( 'NONE', #35342, 1000.000000000000000 ) ;
#91208 = DIRECTION ( 'NONE',  ( 0.7071067811865486830, -0.7071067811865464625, -0.000000000000000000 ) ) ;
#91209 = PLANE ( 'NONE',  #31851 ) ;
#91210 = VERTEX_POINT ( 'NONE', #90852 ) ;
#91211 = ADVANCED_FACE ( 'NONE', ( #83347 ), #115936, .F. ) ;
#91212 = DIRECTION ( 'NONE',  ( 0.000000000000000000, -1.000000000000000000, 0.000000000000000000 ) ) ;
#91213 = CARTESIAN_POINT ( 'NONE',  ( 4.499999999999968914, -10.04351517176477948, -1.623559851933813469 ) ) ;
#91214 = CARTESIAN_POINT ( 'NONE',  ( 76.62043019189812298, 3.055000000000001936, -5.291415217122916737 ) ) ;
#91215 = EDGE_LOOP ( 'NONE', ( #30617, #34097, #61520, #19850 ) ) ;
#91216 = DIRECTION ( 'NONE',  ( -0.7071067811865486830, -0.7071067811865464625, 0.000000000000000000 ) ) ;
#91218 = EDGE_CURVE ( 'NONE', #89614, #95146, #105083, .T. ) ;
#91217 = VECTOR ( 'NONE', #5993, 1000.000000000000000 ) ;
#91219 = CARTESIAN_POINT ( 'NONE',  ( -6.183988606268994381, 28.73617430169791476, 5.000000000000000000 ) ) ;
#91220 = EDGE_LOOP ( 'NONE', ( #48086, #107345, #14241, #136692 ) ) ;
#91221 = ORIENTED_EDGE ( 'NONE', *, *, #111807, .T. ) ;
#91222 = FACE_OUTER_BOUND ( 'NONE', #58438, .T. ) ;
#91223 = DIRECTION ( 'NONE',  ( 0.000000000000000000, -1.000000000000000000, 0.000000000000000000 ) ) ;
#91224 = FACE_OUTER_BOUND ( 'NONE', #115437, .T. ) ;
#91225 = SURFACE_STYLE_FILL_AREA ( #58629 ) ;
#91226 = DIRECTION ( 'NONE',  ( -0.7071067811865486830, -0.7071067811865464625, 0.000000000000000000 ) ) ;
#91227 = LINE ( 'NONE', #23048, #75158 ) ;
#91229 = EDGE_CURVE ( 'NONE', #83610, #131121, #24850, .T. ) ;
#91228 = FILL_AREA_STYLE_COLOUR ( '', #127981 ) ;
#91230 = CONICAL_SURFACE ( 'NONE', #47272, 2.500000000000000444, 0.9599310885968830309 ) ;
#91231 = ORIENTED_EDGE ( 'NONE', *, *, #86027, .T. ) ;
#91232 = VERTEX_POINT ( 'NONE', #128977 ) ;
#91233 = PLANE ( 'NONE',  #13297 ) ;
#91234 = ORIENTED_EDGE ( 'NONE', *, *, #71448, .T. ) ;
#91235 = ORIENTED_EDGE ( 'NONE', *, *, #49164, .T. ) ;
#91236 = EDGE_CURVE ( 'NONE', #71568, #43634, #29649, .T. ) ;
#91237 = CIRCLE ( 'NONE', #51804, 2.055000000000000604 ) ;
#91238 = DIRECTION ( 'NONE',  ( -0.000000000000000000, 0.000000000000000000, 1.000000000000000000 ) ) ;
#91239 = ORIENTED_EDGE ( 'NONE', *, *, #23839, .T. ) ;
#91240 = CARTESIAN_POINT ( 'NONE',  ( 0.7307956238753654521, 0.4000000000000001887, -2.467792535850613866 ) ) ;
#91241 = CARTESIAN_POINT ( 'NONE',  ( -3.989119713460488104, -22.02621442084247860, 4.990779571109225543 ) ) ;
#91242 = DIRECTION ( 'NONE',  ( -1.000000000000000000, -1.224606353822377258E-16, -0.000000000000000000 ) ) ;
#91243 = DIRECTION ( 'NONE',  ( -0.6830127018922181881, 0.6830127018922202975, -0.2588190451025214056 ) ) ;
#91244 = ORIENTED_EDGE ( 'NONE', *, *, #6850, .T. ) ;
#91245 = DIRECTION ( 'NONE',  ( -0.000000000000000000, 0.3543493200069153248, 0.9351131265310292928 ) ) ;
#91246 = DIRECTION ( 'NONE',  ( 0.000000000000000000, 0.000000000000000000, -1.000000000000000000 ) ) ;
#91247 = EDGE_LOOP ( 'NONE', ( #109982, #56420, #113214, #137922 ) ) ;
#91248 = CARTESIAN_POINT ( 'NONE',  ( -57.48921356237308800, -27.52281430457095368, 5.000000000000000000 ) ) ;
#91249 = EDGE_LOOP ( 'NONE', ( #4281, #88349, #55940, #8282 ) ) ;
#91250 = VERTEX_POINT ( 'NONE', #39866 ) ;
#91251 = LINE ( 'NONE', #57201, #13491 ) ;
#91252 = VERTEX_POINT ( 'NONE', #7892 ) ;
#91253 = VERTEX_POINT ( 'NONE', #52134 ) ;
#91254 = VECTOR ( 'NONE', #62722, 1000.000000000000000 ) ;
#91255 = ORIENTED_EDGE ( 'NONE', *, *, #55911, .F. ) ;
#91256 = CARTESIAN_POINT ( 'NONE',  ( -12.48921356237309155, -27.52281430457064104, 5.000000000000000000 ) ) ;
#91257 = AXIS2_PLACEMENT_3D ( 'NONE', #102009, #91159, #68004 ) ;
#91258 = CARTESIAN_POINT ( 'NONE',  ( 56.00000000000004974, -49.14999999999999147, -40.92499999999998295 ) ) ;
#91259 = LINE ( 'NONE', #100689, #118992 ) ;
#91260 = CARTESIAN_POINT ( 'NONE',  ( 117.8337635252314470, 6.110000000000001208, 1.122388791418549305E-15 ) ) ;
#91261 = CARTESIAN_POINT ( 'NONE',  ( -45.18398860626900415, 28.73617430169818832, 5.000000000000000000 ) ) ;
#91262 = EDGE_CURVE ( 'NONE', #141074, #114780, #73894, .T. ) ;
#91263 = CARTESIAN_POINT ( 'NONE',  ( 32.99999999999977263, -3.485240976185046691, -4.108735105802321819 ) ) ;
#91265 = DIRECTION ( 'NONE',  ( 0.000000000000000000, 1.000000000000000000, 0.000000000000000000 ) ) ;
#91264 = DIRECTION ( 'NONE',  ( -0.000000000000000000, 0.000000000000000000, 1.000000000000000000 ) ) ;
#91266 = PLANE ( 'NONE',  #9889 ) ;
#91267 = ADVANCED_FACE ( 'NONE', ( #71771 ), #94005, .T. ) ;
#91268 = SURFACE_STYLE_FILL_AREA ( #104221 ) ;
#91269 = ORIENTED_EDGE ( 'NONE', *, *, #37619, .T. ) ;
#91270 = DIRECTION ( 'NONE',  ( -0.7071067811865486830, -0.7071067811865464625, 0.000000000000000000 ) ) ;
#91271 = STYLED_ITEM ( 'NONE', ( #81861 ), #87823 ) ;
#91272 = ORIENTED_EDGE ( 'NONE', *, *, #121688, .F. ) ;
#91273 = VERTEX_POINT ( 'NONE', #104353 ) ;
#91274 = LINE ( 'NONE', #135485, #102771 ) ;
#91275 = ORIENTED_EDGE ( 'NONE', *, *, #21067, .T. ) ;
#91276 = VECTOR ( 'NONE', #134999, 1000.000000000000000 ) ;
#91277 = ADVANCED_FACE ( 'NONE', ( #107219 ), #51439, .F. ) ;
#91278 = CARTESIAN_POINT ( 'NONE',  ( 25.49999999999982236, -11.56887692260770173, 4.000000000000000000 ) ) ;
#91279 = DIRECTION ( 'NONE',  ( -0.000000000000000000, -0.3543493200069152138, 0.9351131265310292928 ) ) ;
#91280 = AXIS2_PLACEMENT_3D ( 'NONE', #65436, #63982, #52374 ) ;
#91281 = ADVANCED_FACE ( 'NONE', ( #28253 ), #61620, .F. ) ;
#91282 = DIRECTION ( 'NONE',  ( -0.3543493200069162685, -0.000000000000000000, -0.9351131265310288487 ) ) ;
#91283 = LINE ( 'NONE', #59370, #136644 ) ;
#91284 = VERTEX_POINT ( 'NONE', #137739 ) ;
#91285 = VERTEX_POINT ( 'NONE', #63047 ) ;
#91288 = EDGE_CURVE ( 'NONE', #59073, #73381, #50716, .T. ) ;
#91287 = VECTOR ( 'NONE', #72588, 999.9999999999998863 ) ;
#91286 = DIRECTION ( 'NONE',  ( -2.781805975412905890E-17, 0.3543493200069152693, 0.9351131265310292928 ) ) ;
#91289 = EDGE_CURVE ( 'NONE', #137834, #11699, #5746, .T. ) ;
#91290 = VECTOR ( 'NONE', #95886, 1000.000000000000000 ) ;
#91291 = CARTESIAN_POINT ( 'NONE',  ( 29.37956980810188412, 3.967499999999998916, 6.871911579029510442 ) ) ;
#91292 = ORIENTED_EDGE ( 'NONE', *, *, #121981, .F. ) ;
#91293 = LINE ( 'NONE', #91968, #1869 ) ;
#91294 = EDGE_CURVE ( 'NONE', #94085, #56955, #62320, .T. ) ;
#91295 = PLANE ( 'NONE',  #18752 ) ;
#91296 = ORIENTED_EDGE ( 'NONE', *, *, #40405, .T. ) ;
#91297 = VERTEX_POINT ( 'NONE', #118063 ) ;
#91298 = ORIENTED_EDGE ( 'NONE', *, *, #44175, .T. ) ;
#91299 = CARTESIAN_POINT ( 'NONE',  ( -33.13499573751602156, 3.759292476615678336, 15.36553568819733862 ) ) ;
#91300 = DIRECTION ( 'NONE',  ( -0.7071067811865486830, 0.7071067811865464625, 0.000000000000000000 ) ) ;
#91301 = DIRECTION ( 'NONE',  ( -0.000000000000000000, 0.000000000000000000, 1.000000000000000000 ) ) ;
#91302 = CARTESIAN_POINT ( 'NONE',  ( 45.48921356237309510, -27.52281430457087197, 5.000000000000000000 ) ) ;
#91303 = EDGE_LOOP ( 'NONE', ( #5042, #143469, #44371, #136403 ) ) ;
#91304 = CARTESIAN_POINT ( 'NONE',  ( -39.18398860626899705, 28.73617430169814568, 5.000000000000000000 ) ) ;
#91305 = EDGE_CURVE ( 'NONE', #120446, #77094, #95631, .T. ) ;
#91306 = DIRECTION ( 'NONE',  ( -0.7071067811865486830, -0.7071067811865464625, 0.000000000000000000 ) ) ;
#91307 = FACE_OUTER_BOUND ( 'NONE', #45701, .T. ) ;
#91308 = ORIENTED_EDGE ( 'NONE', *, *, #92229, .F. ) ;
#91309 = AXIS2_PLACEMENT_3D ( 'NONE', #133363, #96570, #74153 ) ;
#91310 = EDGE_CURVE ( 'NONE', #103321, #104848, #18037, .T. ) ;
#91311 = LINE ( 'NONE', #62963, #44789 ) ;
#91312 = ORIENTED_EDGE ( 'NONE', *, *, #139111, .F. ) ;
#91314 = ORIENTED_EDGE ( 'NONE', *, *, #51078, .F. ) ;
#91313 = CARTESIAN_POINT ( 'NONE',  ( 58.17012237851979961, -48.09441802426614032, -35.89947574910193850 ) ) ;
#91315 = ORIENTED_EDGE ( 'NONE', *, *, #142390, .T. ) ;
#91316 = CARTESIAN_POINT ( 'NONE',  ( 24.48921356237309510, -27.52281430457072631, 5.000000000000000000 ) ) ;
#91317 = FACE_OUTER_BOUND ( 'NONE', #73592, .T. ) ;
#91318 = EDGE_CURVE ( 'NONE', #79126, #83227, #39129, .T. ) ;
#91319 = ORIENTED_EDGE ( 'NONE', *, *, #2451, .T. ) ;
#91320 = FILL_AREA_STYLE ('',( #692 ) ) ;
#91321 = LINE ( 'NONE', #115864, #28949 ) ;
#91322 = DIRECTION ( 'NONE',  ( 0.000000000000000000, -1.000000000000000000, 0.000000000000000000 ) ) ;
#91323 = DIRECTION ( 'NONE',  ( 0.7071067811865487940, 0.7071067811865463515, -0.000000000000000000 ) ) ;
#91324 = LINE ( 'NONE', #80445, #94863 ) ;
#91325 = DIRECTION ( 'NONE',  ( -0.7071067811865487940, 0.7071067811865463515, 0.000000000000000000 ) ) ;
#91326 = DIRECTION ( 'NONE',  ( 0.7071067811865487940, 0.7071067811865463515, -0.000000000000000000 ) ) ;
#91328 = ADVANCED_FACE ( 'NONE', ( #124170 ), #84767, .F. ) ;
#91327 = FACE_OUTER_BOUND ( 'NONE', #856, .T. ) ;
#91329 = DIRECTION ( 'NONE',  ( -0.000000000000000000, 0.3543493200069153248, 0.9351131265310291818 ) ) ;
#91330 = CARTESIAN_POINT ( 'NONE',  ( 24.62456980810188867, -6.871911579029512218, 3.967499999999996252 ) ) ;
#91331 = CARTESIAN_POINT ( 'NONE',  ( 0.000000000000000000, 0.000000000000000000, 5.000000000000000000 ) ) ;
#91332 = DIRECTION ( 'NONE',  ( -0.7071067811865486830, 0.7071067811865464625, 0.000000000000000000 ) ) ;
#91333 = DIRECTION ( 'NONE',  ( 0.3543493200069162685, -0.000000000000000000, -0.9351131265310288487 ) ) ;
#91334 = PLANE ( 'NONE',  #38497 ) ;
#91335 = VERTEX_POINT ( 'NONE', #60924 ) ;
#91336 = VECTOR ( 'NONE', #24709, 1000.000000000000000 ) ;
#91338 = ORIENTED_EDGE ( 'NONE', *, *, #60565, .F. ) ;
#91337 = EDGE_CURVE ( 'NONE', #89964, #57727, #27508, .T. ) ;
#91339 = EDGE_CURVE ( 'NONE', #96482, #64185, #75333, .T. ) ;
#91340 = CARTESIAN_POINT ( 'NONE',  ( 93.89583333333331439, -2.130196079827427091, 7.949999999999999289 ) ) ;
#91341 = ORIENTED_EDGE ( 'NONE', *, *, #49505, .T. ) ;
#91342 = VERTEX_POINT ( 'NONE', #131849 ) ;
#91343 = VERTEX_POINT ( 'NONE', #31813 ) ;
#91344 = LINE ( 'NONE', #113050, #29501 ) ;
#91345 = LINE ( 'NONE', #135555, #18568 ) ;
#91346 = CARTESIAN_POINT ( 'NONE',  ( 12.53018939210443428, 8.713309148047983399, 3.789081179538163369 ) ) ;
#91347 = ORIENTED_EDGE ( 'NONE', *, *, #100899, .T. ) ;
#91348 = DIRECTION ( 'NONE',  ( -0.7071067811865487940, 0.7071067811865463515, 0.000000000000000000 ) ) ;
#91349 = ADVANCED_FACE ( 'NONE', ( #9292 ), #110064, .T. ) ;
#91350 = CARTESIAN_POINT ( 'NONE',  ( 0.6183849060199635428, -2.240707523384260824, 13.37739548510239196 ) ) ;
#91351 = CARTESIAN_POINT ( 'NONE',  ( 21.79289321881330821, 9.759292476615618384, 5.000000000000000000 ) ) ;
#91352 = DIRECTION ( 'NONE',  ( -0.7071067811865486830, -0.7071067811865464625, -0.000000000000000000 ) ) ;
#91353 = EDGE_CURVE ( 'NONE', #56501, #8328, #55722, .T. ) ;
#91354 = CARTESIAN_POINT ( 'NONE',  ( 0.000000000000000000, 0.000000000000000000, 5.000000000000000000 ) ) ;
#91355 = CARTESIAN_POINT ( 'NONE',  ( 21.87889065874226091, 8.431076354171498366, 5.000000000000000000 ) ) ;
#91356 = CARTESIAN_POINT ( 'NONE',  ( 13.49999999999990408, 0.4311230773921762571, 4.000000000000000000 ) ) ;
#91357 = CARTESIAN_POINT ( 'NONE',  ( 6.938893903907228378E-15, 17.58746187583906462, 4.000000000000000000 ) ) ;
#91358 = VECTOR ( 'NONE', #58307, 1000.000000000000000 ) ;
#91359 = CARTESIAN_POINT ( 'NONE',  ( 26.99999999999998579, 5.473733291157039993, 4.253954074006194297 ) ) ;
#91360 = CARTESIAN_POINT ( 'NONE',  ( 20.11162361894746553, 9.759292476615614831, 17.35367589129208099 ) ) ;
#91361 = CARTESIAN_POINT ( 'NONE',  ( -19.17183060077633883, 21.75929247661549581, 4.000000000000000000 ) ) ;
#91362 = CARTESIAN_POINT ( 'NONE',  ( 86.55836038379621300, -7.949999999999996625, -2.130196079827426203 ) ) ;
#91363 = PLANE ( 'NONE',  #21414 ) ;
#91364 = EDGE_LOOP ( 'NONE', ( #92477, #75383, #124496, #98059 ) ) ;
#91365 = ORIENTED_EDGE ( 'NONE', *, *, #88127, .T. ) ;
#91366 = CARTESIAN_POINT ( 'NONE',  ( 110.9795968585647756, 6.109999999999999432, 1.637169565754164280 ) ) ;
#91367 = VERTEX_POINT ( 'NONE', #74622 ) ;
#91368 = ADVANCED_FACE ( 'NONE', ( #42713 ), #22323, .F. ) ;
#91369 = VECTOR ( 'NONE', #21426, 999.9999999999998863 ) ;
#91370 = CARTESIAN_POINT ( 'NONE',  ( 100.4583333333333286, 3.974999999999997424, 6.884901960086288852 ) ) ;
#91371 = DIRECTION ( 'NONE',  ( -0.6830127018922181881, 0.6830127018922202975, -0.2588190451025214056 ) ) ;
#91372 = EDGE_CURVE ( 'NONE', #103836, #15513, #33285, .T. ) ;
#91373 = CARTESIAN_POINT ( 'NONE',  ( -32.99999999999975131, 20.58746187583903620, 4.000000000000000000 ) ) ;
#91374 = DIRECTION ( 'NONE',  ( 0.7071067811865487940, 0.7071067811865463515, 0.000000000000000000 ) ) ;
#91375 = CARTESIAN_POINT ( 'NONE',  ( 103.4537635252314516, -6.109999999999998543, -3.741295971395162543E-16 ) ) ;
#91376 = AXIS2_PLACEMENT_3D ( 'NONE', #137472, #115663, #3349 ) ;
#91377 = ORIENTED_EDGE ( 'NONE', *, *, #84816, .F. ) ;
#91378 = EDGE_LOOP ( 'NONE', ( #24450, #39581, #121074, #56611 ) ) ;
#91379 = FACE_OUTER_BOUND ( 'NONE', #27701, .T. ) ;
#91380 = CARTESIAN_POINT ( 'NONE',  ( 98.41666666666667140, -6.884901960086287076, -3.975000000000000977 ) ) ;
#91381 = ORIENTED_EDGE ( 'NONE', *, *, #11425, .T. ) ;
#91382 = ORIENTED_EDGE ( 'NONE', *, *, #120981, .T. ) ;
#91383 = ORIENTED_EDGE ( 'NONE', *, *, #21136, .F. ) ;
#91384 = LINE ( 'NONE', #58062, #86146 ) ;
#91385 = CARTESIAN_POINT ( 'NONE',  ( 1.379569808101885897, 3.967499999999998916, 6.871911579029510442 ) ) ;
#91386 = AXIS2_PLACEMENT_3D ( 'NONE', #81291, #124768, #105842 ) ;
#91387 = EDGE_CURVE ( 'NONE', #20150, #15770, #55011, .T. ) ;
#91388 = CIRCLE ( 'NONE', #93658, 0.5000000000000004441 ) ;
#91389 = VECTOR ( 'NONE', #37617, 1000.000000000000000 ) ;
#91390 = CARTESIAN_POINT ( 'NONE',  ( 29.37043019189811233, -3.055000000000001492, 5.291415217122917625 ) ) ;
#91391 = EDGE_LOOP ( 'NONE', ( #78501, #106078, #47406, #106905 ) ) ;
#91392 = ORIENTED_EDGE ( 'NONE', *, *, #4519, .T. ) ;
#91393 = CARTESIAN_POINT ( 'NONE',  ( 14.99999999999989519, 13.93112307739203715, 4.000000000000000000 ) ) ;
#91394 = EDGE_LOOP ( 'NONE', ( #2374, #71857, #117393, #60381 ) ) ;
#91395 = ORIENTED_EDGE ( 'NONE', *, *, #111056, .F. ) ;
#91396 = DIRECTION ( 'NONE',  ( 0.6830127018922180770, -0.6830127018922204085, -0.2588190451025213501 ) ) ;
#91397 = PLANE ( 'NONE',  #3478 ) ;
#91398 = LINE ( 'NONE', #113834, #141441 ) ;
#91399 = ORIENTED_EDGE ( 'NONE', *, *, #80699, .T. ) ;
#91400 = CARTESIAN_POINT ( 'NONE',  ( 16.79601123714775213, -22.22500000000000142, -14.59902459068437786 ) ) ;
#91401 = DIRECTION ( 'NONE',  ( -0.7071067811865486830, -0.7071067811865464625, 0.000000000000000000 ) ) ;
#91402 = DIRECTION ( 'NONE',  ( -0.6830127018922180770, -0.6830127018922204085, -0.2588190451025213501 ) ) ;
#91403 = FACE_BOUND ( 'NONE', #87271, .T. ) ;
#91404 = VERTEX_POINT ( 'NONE', #99174 ) ;
#91405 = CARTESIAN_POINT ( 'NONE',  ( 184.1500000000000057, -30.18000000000009564, 15.92499999999935945 ) ) ;
#91406 = DIRECTION ( 'NONE',  ( 0.7071067811865486830, -0.7071067811865464625, -0.000000000000000000 ) ) ;
#91407 = ORIENTED_EDGE ( 'NONE', *, *, #45630, .T. ) ;
#91408 = CARTESIAN_POINT ( 'NONE',  ( -9.005480084712511157, 28.92564299267931816, 4.000000000000000000 ) ) ;
#91409 = ORIENTED_EDGE ( 'NONE', *, *, #106755, .F. ) ;
#91410 = ORIENTED_EDGE ( 'NONE', *, *, #124349, .F. ) ;
#91411 = ORIENTED_EDGE ( 'NONE', *, *, #94911, .F. ) ;
#91412 = CARTESIAN_POINT ( 'NONE',  ( 41.91209685856478728, 5.291415217122921177, -3.054999999999994831 ) ) ;
#91413 = VERTEX_POINT ( 'NONE', #142026 ) ;
#91414 = CARTESIAN_POINT ( 'NONE',  ( 2.999999999999975575, 13.93112307739204425, 4.000000000000000000 ) ) ;
#91415 = LINE ( 'NONE', #37012, #26528 ) ;
#91416 = ORIENTED_EDGE ( 'NONE', *, *, #73479, .F. ) ;
#91417 = CARTESIAN_POINT ( 'NONE',  ( -44.99451991528749772, 28.92564299267969474, 4.000000000000000000 ) ) ;
#91418 = VECTOR ( 'NONE', #48614, 1000.000000000000000 ) ;
#91419 = DIRECTION ( 'NONE',  ( -0.000000000000000000, 0.000000000000000000, 1.000000000000000000 ) ) ;
#91420 = DIRECTION ( 'NONE',  ( -1.000000000000000000, -1.224606353822377258E-16, -0.000000000000000000 ) ) ;
#91421 = PLANE ( 'NONE',  #49441 ) ;
#91422 = ORIENTED_EDGE ( 'NONE', *, *, #129605, .F. ) ;
#91423 = ADVANCED_FACE ( 'NONE', ( #20193 ), #76777, .F. ) ;
#91424 = ORIENTED_EDGE ( 'NONE', *, *, #113275, .F. ) ;
#91425 = ORIENTED_EDGE ( 'NONE', *, *, #71671, .T. ) ;
#91426 = EDGE_LOOP ( 'NONE', ( #23895, #91296, #71761, #41609, #38159 ) ) ;
#91427 = DIRECTION ( 'NONE',  ( -0.000000000000000000, -0.3543493200069152693, 0.9351131265310292928 ) ) ;
#91428 = ORIENTED_EDGE ( 'NONE', *, *, #135517, .F. ) ;
#91429 = ADVANCED_FACE ( 'NONE', ( #77487 ), #118811, .F. ) ;
#91431 = ORIENTED_EDGE ( 'NONE', *, *, #66270, .F. ) ;
#91430 = EDGE_CURVE ( 'NONE', #80319, #20411, #132592, .T. ) ;
#91432 = FACE_OUTER_BOUND ( 'NONE', #57449, .T. ) ;
#91433 = EDGE_CURVE ( 'NONE', #132258, #114780, #43406, .T. ) ;
#91434 = EDGE_CURVE ( 'NONE', #112333, #2363, #30384, .T. ) ;
#91435 = CARTESIAN_POINT ( 'NONE',  ( 33.18398860626899705, 28.73617430169810305, 5.000000000000000000 ) ) ;
#91436 = ORIENTED_EDGE ( 'NONE', *, *, #132256, .T. ) ;
#91437 = LINE ( 'NONE', #124763, #18613 ) ;
#91438 = ORIENTED_EDGE ( 'NONE', *, *, #41882, .F. ) ;
#91440 = ADVANCED_FACE ( 'NONE', ( #65180 ), #107907, .F. ) ;
#91439 = CARTESIAN_POINT ( 'NONE',  ( 0.3605397743886049056, 0.4000000000000001332, -2.166563419957293402 ) ) ;
#91441 = EDGE_CURVE ( 'NONE', #138495, #113729, #52822, .T. ) ;
#91442 = VECTOR ( 'NONE', #89722, 1000.000000000000000 ) ;
#91443 = CARTESIAN_POINT ( 'NONE',  ( 30.69206980810189123, -7.934999999999991616, -2.126176841940955242 ) ) ;
#91444 = CARTESIAN_POINT ( 'NONE',  ( -1.245430191898114103, -6.871911579029512218, 3.967499999999996252 ) ) ;
#91445 = EDGE_LOOP ( 'NONE', ( #124010, #103478, #130202, #47569 ) ) ;
#91447 = CARTESIAN_POINT ( 'NONE',  ( 24.29974487139158867, -27.71228299555223273, 4.000000000000000000 ) ) ;
#91446 = CARTESIAN_POINT ( 'NONE',  ( 109.5787635252314516, -7.482591942790327058E-16, 6.109999999999999432 ) ) ;
#91448 = AXIS2_PLACEMENT_3D ( 'NONE', #22284, #143382, #44843 ) ;
#91449 = EDGE_CURVE ( 'NONE', #16533, #103400, #31115, .T. ) ;
#91450 = CARTESIAN_POINT ( 'NONE',  ( -7.499999999999944045, 0.05218569542916710879, 5.000000000000000000 ) ) ;
#91451 = SURFACE_SIDE_STYLE ('',( #47278 ) ) ;
#91452 = ORIENTED_EDGE ( 'NONE', *, *, #27243, .F. ) ;
#91454 = ORIENTED_EDGE ( 'NONE', *, *, #46477, .T. ) ;
#91453 = CARTESIAN_POINT ( 'NONE',  ( 35.53839644629407246, -9.740707523384177335, 17.74957260769619083 ) ) ;
#91455 = LINE ( 'NONE', #100187, #120367 ) ;
#91456 = LINE ( 'NONE', #135670, #69500 ) ;
#91457 = CARTESIAN_POINT ( 'NONE',  ( 4.499999999999962697, -14.70932175296476352, -11.46312253303838347 ) ) ;
#91458 = CARTESIAN_POINT ( 'NONE',  ( -8.292893218813397027, 17.25929247661554911, 5.000000000000000000 ) ) ;
#91459 = DIRECTION ( 'NONE',  ( 0.6830127018922180770, -0.6830127018922204085, -0.2588190451025213501 ) ) ;
#91460 = VERTEX_POINT ( 'NONE', #21655 ) ;
#91461 = EDGE_CURVE ( 'NONE', #47238, #132969, #143421, .T. ) ;
#91462 = VECTOR ( 'NONE', #17972, 1000.000000000000227 ) ;
#91463 = CARTESIAN_POINT ( 'NONE',  ( -19.05000000000000071, 3.174999999999997158, 4.000000000000000000 ) ) ;
#91464 = FACE_OUTER_BOUND ( 'NONE', #79158, .T. ) ;
#91465 = ORIENTED_EDGE ( 'NONE', *, *, #108245, .F. ) ;
#91466 = CARTESIAN_POINT ( 'NONE',  ( 174.7500000000000000, 7.919999999999947526, 19.12499999999998224 ) ) ;
#91467 = CARTESIAN_POINT ( 'NONE',  ( -28.49999999999981171, 16.18958161055400069, -11.56426086740817638 ) ) ;
#91468 = ORIENTED_EDGE ( 'NONE', *, *, #108949, .F. ) ;
#91470 = ORIENTED_EDGE ( 'NONE', *, *, #84173, .F. ) ;
#91469 = DIRECTION ( 'NONE',  ( 1.000000000000000000, 1.224606353822377258E-16, 0.000000000000000000 ) ) ;
#91471 = VERTEX_POINT ( 'NONE', #110765 ) ;
#91472 = CARTESIAN_POINT ( 'NONE',  ( 4.161307151687957173, 13.37712895942531688, -24.65215201657544952 ) ) ;
#91473 = CARTESIAN_POINT ( 'NONE',  ( 29.99999999999979039, 5.966399257802205369, 5.000000000000000000 ) ) ;
#91474 = EDGE_CURVE ( 'NONE', #29352, #43087, #128785, .T. ) ;
#91475 = VERTEX_POINT ( 'NONE', #70205 ) ;
#91476 = PRESENTATION_LAYER_ASSIGNMENT (  '', '', ( #103055 ) ) ;
#91477 = SURFACE_STYLE_FILL_AREA ( #98249 ) ;
#91478 = AXIS2_PLACEMENT_3D ( 'NONE', #3154, #99605, #69159 ) ;
#91479 = VECTOR ( 'NONE', #50591, 1000.000000000000000 ) ;
#91480 = DIRECTION ( 'NONE',  ( -0.3543493200069162685, -0.000000000000000000, -0.9351131265310288487 ) ) ;
#91481 = ORIENTED_EDGE ( 'NONE', *, *, #92229, .T. ) ;
#91482 = VECTOR ( 'NONE', #6312, 1000.000000000000000 ) ;
#91483 = LINE ( 'NONE', #66872, #16521 ) ;
#91484 = LINE ( 'NONE', #69025, #42154 ) ;
#91486 = EDGE_CURVE ( 'NONE', #33609, #132528, #44887, .T. ) ;
#91485 = SURFACE_STYLE_FILL_AREA ( #26223 ) ;
#91487 = CARTESIAN_POINT ( 'NONE',  ( 2.999999999999999112, -1.600000000000012301, -20.40202195861969514 ) ) ;
#91488 = LINE ( 'NONE', #38526, #59927 ) ;
#91489 = LINE ( 'NONE', #125550, #90547 ) ;
#91490 = LINE ( 'NONE', #125551, #61601 ) ;
#91491 = ORIENTED_EDGE ( 'NONE', *, *, #128422, .T. ) ;
#91492 = ORIENTED_EDGE ( 'NONE', *, *, #100509, .F. ) ;
#91493 = ORIENTED_EDGE ( 'NONE', *, *, #46934, .T. ) ;
#91494 = EDGE_CURVE ( 'NONE', #50481, #52944, #114882, .T. ) ;
#91495 = CARTESIAN_POINT ( 'NONE',  ( 119.5624999999999716, -5.819803920172572198, -5.819803920172573086 ) ) ;
#91496 = ORIENTED_EDGE ( 'NONE', *, *, #48602, .T. ) ;
#91497 = VERTEX_POINT ( 'NONE', #125245 ) ;
#91498 = EDGE_CURVE ( 'NONE', #40538, #78627, #25204, .T. ) ;
#91499 = ORIENTED_EDGE ( 'NONE', *, *, #108077, .F. ) ;
#91500 = CARTESIAN_POINT ( 'NONE',  ( 0.8141326222277666114, -6.652716765028095836, -2.974119808974657886 ) ) ;
#91501 = LINE ( 'NONE', #24791, #92573 ) ;
#91502 = VERTEX_POINT ( 'NONE', #36115 ) ;
#91503 = DIRECTION ( 'NONE',  ( 0.000000000000000000, -1.000000000000000000, 0.000000000000000000 ) ) ;
#91505 = EDGE_CURVE ( 'NONE', #89689, #79010, #91893, .T. ) ;
#91504 = PLANE ( 'NONE',  #72234 ) ;
#91506 = DIRECTION ( 'NONE',  ( 0.6830127018922181881, 0.6830127018922202975, -0.2588190451025214056 ) ) ;
#91507 = FACE_OUTER_BOUND ( 'NONE', #73420, .T. ) ;
#91508 = CARTESIAN_POINT ( 'NONE',  ( 108.2087635252314470, -7.482591942790329030E-16, 6.110000000000001208 ) ) ;
#91509 = ORIENTED_EDGE ( 'NONE', *, *, #105500, .F. ) ;
#91510 = DIRECTION ( 'NONE',  ( 0.6830127018922180770, -0.6830127018922204085, -0.2588190451025213501 ) ) ;
#91511 = CARTESIAN_POINT ( 'NONE',  ( 4.499999999999969802, -13.53360074219760101, 5.000000000000000000 ) ) ;
#91512 = CARTESIAN_POINT ( 'NONE',  ( 0.4200025801390303015, 6.514529779848684754, -4.079159782690128466 ) ) ;
#91513 = EDGE_CURVE ( 'NONE', #52437, #110391, #56472, .T. ) ;
#91514 = CARTESIAN_POINT ( 'NONE',  ( -8.999999999999937828, 13.93112307739204603, 4.000000000000000000 ) ) ;
#91515 = DIRECTION ( 'NONE',  ( 0.7071067811865487940, 0.7071067811865463515, 0.000000000000000000 ) ) ;
#91516 = CARTESIAN_POINT ( 'NONE',  ( 49.66252705046289861, 7.949999999999998401, 1.460391307983218338E-15 ) ) ;
#91517 = CARTESIAN_POINT ( 'NONE',  ( 12.03892749862900402, 4.202752102959690472E-16, 0.000000000000000000 ) ) ;
#91518 = LINE ( 'NONE', #80648, #110889 ) ;
#91519 = ORIENTED_EDGE ( 'NONE', *, *, #22109, .T. ) ;
#91520 = VERTEX_POINT ( 'NONE', #68066 ) ;
#91521 = CARTESIAN_POINT ( 'NONE',  ( 36.58333333333332860, 6.884901960086290629, -3.974999999999994316 ) ) ;
#91522 = VERTEX_POINT ( 'NONE', #113643 ) ;
#91523 = ORIENTED_EDGE ( 'NONE', *, *, #6979, .F. ) ;
#91524 = EDGE_CURVE ( 'NONE', #5899, #126135, #1296, .T. ) ;
#91525 = PLANE ( 'NONE',  #78446 ) ;
#91526 = LINE ( 'NONE', #3066, #101013 ) ;
#91527 = VERTEX_POINT ( 'NONE', #79660 ) ;
#91528 = DIRECTION ( 'NONE',  ( -0.7071067811865486830, -0.7071067811865464625, -0.000000000000000000 ) ) ;
#91529 = DIRECTION ( 'NONE',  ( -0.000000000000000000, 0.3543493200069153248, 0.9351131265310292928 ) ) ;
#91530 = CARTESIAN_POINT ( 'NONE',  ( 38.50043019189809712, -3.055000000000002380, 5.291415217122920289 ) ) ;
#91531 = EDGE_CURVE ( 'NONE', #91750, #87099, #69461, .T. ) ;
#91532 = ORIENTED_EDGE ( 'NONE', *, *, #20291, .T. ) ;
#91533 = DIRECTION ( 'NONE',  ( -0.6830127018922181881, 0.6830127018922202975, -0.2588190451025214056 ) ) ;
#91534 = ORIENTED_EDGE ( 'NONE', *, *, #40080, .F. ) ;
#91535 = LINE ( 'NONE', #45900, #109869 ) ;
#91536 = CARTESIAN_POINT ( 'NONE',  ( 60.18398860626900415, 28.73617430169829490, 5.000000000000000000 ) ) ;
#91538 =( BOUNDED_CURVE ( )  B_SPLINE_CURVE ( 3, ( #130190, #64214, #97532, #52605 ),
 .UNSPECIFIED., .F., .F. ) 
 B_SPLINE_CURVE_WITH_KNOTS ( ( 4, 4 ),
 ( 5.920967161967926273, 7.341195215986594746 ),
 .UNSPECIFIED. ) 
 CURVE ( )  GEOMETRIC_REPRESENTATION_ITEM ( )  RATIONAL_B_SPLINE_CURVE ( ( 1.000000000000000000, 0.8388583629366703764, 0.8388583629366703764, 1.000000000000000000 ) ) 
 REPRESENTATION_ITEM ( '' )  );
#91537 = SURFACE_STYLE_FILL_AREA ( #102432 ) ;
#91539 = LINE ( 'NONE', #100268, #7070 ) ;
#91540 = VERTEX_POINT ( 'NONE', #23797 ) ;
#91541 = EDGE_CURVE ( 'NONE', #117995, #104048, #111509, .T. ) ;
#91542 = ORIENTED_EDGE ( 'NONE', *, *, #108238, .T. ) ;
#91543 = CARTESIAN_POINT ( 'NONE',  ( 38.57919371712956291, 3.975000000000002753, -6.884901960086283523 ) ) ;
#91544 = CARTESIAN_POINT ( 'NONE',  ( -30.70701326429283640, -21.74070752338405654, 4.999753212805224223 ) ) ;
#91545 = CARTESIAN_POINT ( 'NONE',  ( 10.17183060077640633, -20.24070752338407075, 4.000000000000000000 ) ) ;
#91546 = LINE ( 'NONE', #124163, #94922 ) ;
#91547 = FACE_OUTER_BOUND ( 'NONE', #10861, .T. ) ;
#91548 = VECTOR ( 'NONE', #138062, 1000.000000000000000 ) ;
#91549 = CARTESIAN_POINT ( 'NONE',  ( 55.76626352523145869, 4.472830434245839371, -4.472830434245838482 ) ) ;
#91550 = AXIS2_PLACEMENT_3D ( 'NONE', #93139, #25731, #47546 ) ;
#91551 = CARTESIAN_POINT ( 'NONE',  ( 124.6666666666666572, 6.884901960086285300, 3.975000000000003642 ) ) ;
#91552 = CARTESIAN_POINT ( 'NONE',  ( 27.48921356237309155, -27.52281430457074762, 5.000000000000000000 ) ) ;
#91553 = ORIENTED_EDGE ( 'NONE', *, *, #132966, .T. ) ;
#91554 = EDGE_LOOP ( 'NONE', ( #51316, #92138, #85341, #59406 ) ) ;
#91555 = DIRECTION ( 'NONE',  ( 0.000000000000000000, 0.000000000000000000, 1.000000000000000000 ) ) ;
#91556 = VERTEX_POINT ( 'NONE', #100650 ) ;
#91557 = EDGE_CURVE ( 'NONE', #121547, #42504, #81046, .T. ) ;
#91558 = ADVANCED_FACE ( 'NONE', ( #2739 ), #90480, .F. ) ;
#91559 = VECTOR ( 'NONE', #72444, 1000.000000000000000 ) ;
#91560 = CARTESIAN_POINT ( 'NONE',  ( 27.45983838949723221, 18.75929247661552068, 8.305906642995550371 ) ) ;
#91561 = VERTEX_POINT ( 'NONE', #68750 ) ;
#91562 = LINE ( 'NONE', #135097, #114072 ) ;
#91563 = FACE_BOUND ( 'NONE', #143151, .T. ) ;
#91564 = EDGE_CURVE ( 'NONE', #68485, #106451, #112933, .T. ) ;
#91565 = LINE ( 'NONE', #114712, #15529 ) ;
#91566 = CARTESIAN_POINT ( 'NONE',  ( -5.700255128608413102, -27.71228299555201957, 4.000000000000000000 ) ) ;
#91567 = CARTESIAN_POINT ( 'NONE',  ( 152.4000000000000057, 0.000000000000000000, 0.000000000000000000 ) ) ;
#91569 = ORIENTED_EDGE ( 'NONE', *, *, #65723, .F. ) ;
#91568 = CARTESIAN_POINT ( 'NONE',  ( 34.49999999999976552, -4.535744391599457082, 4.994342998332164107 ) ) ;
#91570 = DIRECTION ( 'NONE',  ( -0.6830127018922180770, -0.6830127018922204085, -0.2588190451025213501 ) ) ;
#91571 = VECTOR ( 'NONE', #53539, 1000.000000000000000 ) ;
#91572 = ORIENTED_EDGE ( 'NONE', *, *, #20739, .F. ) ;
#91574 = ORIENTED_EDGE ( 'NONE', *, *, #99598, .F. ) ;
#91573 = AXIS2_PLACEMENT_3D ( 'NONE', #32328, #110560, #98981 ) ;
#91575 = CARTESIAN_POINT ( 'NONE',  ( 66.55793019189812298, 6.110000000000000320, -1.637169565754156064 ) ) ;
#91576 = ORIENTED_EDGE ( 'NONE', *, *, #123548, .T. ) ;
#91577 = CIRCLE ( 'NONE', #10525, 2.500000000000000444 ) ;
#91578 = CARTESIAN_POINT ( 'NONE',  ( 34.77149322861314573, 20.25929247661551358, 7.808871592221849234 ) ) ;
#91579 = ORIENTED_EDGE ( 'NONE', *, *, #121653, .F. ) ;
#91580 = CARTESIAN_POINT ( 'NONE',  ( 36.48921356237310221, -27.52281430457080802, 5.000000000000000000 ) ) ;
#91581 = ADVANCED_FACE ( 'NONE', ( #27335 ), #92594, .F. ) ;
#91582 = DIRECTION ( 'NONE',  ( 0.6830127018922181881, 0.6830127018922202975, -0.2588190451025214056 ) ) ;
#91583 = CARTESIAN_POINT ( 'NONE',  ( 0.000000000000000000, -43.14999999999999147, 31.92499999999998295 ) ) ;
#91585 = PLANE ( 'NONE',  #95924 ) ;
#91584 = CARTESIAN_POINT ( 'NONE',  ( -26.99999999999980105, 1.931123077392163712, 4.000000000000000000 ) ) ;
#91586 = CARTESIAN_POINT ( 'NONE',  ( 31.17183060077625711, 3.759292476615683665, 4.000000000000000000 ) ) ;
#91587 = DIRECTION ( 'NONE',  ( -0.000000000000000000, 0.000000000000000000, 1.000000000000000000 ) ) ;
#91588 = ORIENTED_EDGE ( 'NONE', *, *, #62945, .F. ) ;
#91589 = VERTEX_POINT ( 'NONE', #29479 ) ;
#91590 = CARTESIAN_POINT ( 'NONE',  ( 33.18398860626899705, 28.73617430169810305, 5.000000000000000000 ) ) ;
#91591 = DIRECTION ( 'NONE',  ( -0.000000000000000000, -1.000000000000000000, -0.000000000000000000 ) ) ;
#91592 = EDGE_LOOP ( 'NONE', ( #76756, #5035, #18909, #95850, #76941 ) ) ;
#91593 = VERTEX_POINT ( 'NONE', #17870 ) ;
#91594 = ORIENTED_EDGE ( 'NONE', *, *, #105814, .T. ) ;
#91595 = EDGE_CURVE ( 'NONE', #41627, #78241, #40399, .T. ) ;
#91596 = DIRECTION ( 'NONE',  ( -1.000000000000000000, 0.000000000000000000, -0.000000000000000000 ) ) ;
#91597 = ORIENTED_EDGE ( 'NONE', *, *, #134903, .T. ) ;
#91598 = CARTESIAN_POINT ( 'NONE',  ( 12.42327845806345721, 11.25929247661559529, 17.85071094206581321 ) ) ;
#91600 = EDGE_CURVE ( 'NONE', #50386, #31310, #125973, .T. ) ;
#91599 = DIRECTION ( 'NONE',  ( 0.000000000000000000, 0.000000000000000000, -1.000000000000000000 ) ) ;
#91601 = EDGE_CURVE ( 'NONE', #119206, #109845, #38950, .T. ) ;
#91602 = CARTESIAN_POINT ( 'NONE',  ( 1.817069808101886341, -2.126176841940956130, 7.934999999999991616 ) ) ;
#91603 = FACE_OUTER_BOUND ( 'NONE', #45789, .T. ) ;
#91604 = ADVANCED_FACE ( 'NONE', ( #117192 ), #87187, .T. ) ;
#91605 = ORIENTED_EDGE ( 'NONE', *, *, #115481, .F. ) ;
#91606 = LINE ( 'NONE', #125675, #135983 ) ;
#91607 = EDGE_CURVE ( 'NONE', #127807, #20442, #50538, .T. ) ;
#91608 = DIRECTION ( 'NONE',  ( -0.7071067811865487940, 0.7071067811865463515, -0.000000000000000000 ) ) ;
#91609 = DIRECTION ( 'NONE',  ( -0.7071067811865487940, 0.7071067811865463515, -0.000000000000000000 ) ) ;
#91611 = ORIENTED_EDGE ( 'NONE', *, *, #38412, .F. ) ;
#91610 = CARTESIAN_POINT ( 'NONE',  ( 34.92499999999998295, 8.454535441273616669, -0.2181437882982223408 ) ) ;
#91612 = VERTEX_POINT ( 'NONE', #117889 ) ;
#91613 = EDGE_CURVE ( 'NONE', #118849, #110220, #84606, .T. ) ;
#91614 = LINE ( 'NONE', #35846, #61209 ) ;
#91615 = LINE ( 'NONE', #137270, #42287 ) ;
#91616 = CARTESIAN_POINT ( 'NONE',  ( 3.299744871391591339, -27.71228299555208352, 4.000000000000000000 ) ) ;
#91617 = VERTEX_POINT ( 'NONE', #49137 ) ;
#91618 = DIRECTION ( 'NONE',  ( -0.000000000000000000, 0.3543493200069153248, 0.9351131265310291818 ) ) ;
#91619 = LINE ( 'NONE', #46747, #101208 ) ;
#91620 = EDGE_CURVE ( 'NONE', #54976, #15318, #136828, .T. ) ;
#91621 =( NAMED_UNIT ( * ) PLANE_ANGLE_UNIT ( ) SI_UNIT ( $, .RADIAN. ) );
#91622 = CARTESIAN_POINT ( 'NONE',  ( 27.68749999999998579, -5.819803920172573974, 5.819803920172573086 ) ) ;
#91623 = DIRECTION ( 'NONE',  ( 0.7071067811865486830, -0.7071067811865464625, -0.000000000000000000 ) ) ;
#91624 = ORIENTED_EDGE ( 'NONE', *, *, #26972, .F. ) ;
#91625 = DIRECTION ( 'NONE',  ( 0.000000000000000000, -0.5150380749100594846, -0.8571673007021091140 ) ) ;
#91626 = DIRECTION ( 'NONE',  ( 0.9707728879609285322, 0.000000000000000000, 0.2399999999999971323 ) ) ;
#91627 = CARTESIAN_POINT ( 'NONE',  ( 21.48330628287043709, 6.094999999999991758, 1.633150327867686880 ) ) ;
#91628 = EDGE_CURVE ( 'NONE', #24049, #89715, #104913, .T. ) ;
#91629 = LINE ( 'NONE', #125703, #132783 ) ;
#91630 = DIRECTION ( 'NONE',  ( 0.000000000000000000, 0.000000000000000000, 1.000000000000000000 ) ) ;
#91631 = EDGE_CURVE ( 'NONE', #21885, #55035, #5581, .T. ) ;
#91632 = VERTEX_POINT ( 'NONE', #60004 ) ;
#91633 = EDGE_LOOP ( 'NONE', ( #130688, #79900, #56681, #135117 ) ) ;
#91634 = FACE_OUTER_BOUND ( 'NONE', #21476, .T. ) ;
#91635 = DIRECTION ( 'NONE',  ( 0.7071067811865487940, 0.7071067811865463515, -0.000000000000000000 ) ) ;
#91636 = EDGE_CURVE ( 'NONE', #77481, #22051, #28801, .T. ) ;
#91637 = CARTESIAN_POINT ( 'NONE',  ( 6.541236474768553855, 0.000000000000000000, 7.934999999999990727 ) ) ;
#91638 = VECTOR ( 'NONE', #83830, 999.9999999999998863 ) ;
#91639 = CARTESIAN_POINT ( 'NONE',  ( 26.99451991528749417, 28.92564299267956685, 4.000000000000000000 ) ) ;
#91640 = LINE ( 'NONE', #46018, #90080 ) ;
#91641 = LINE ( 'NONE', #14789, #131711 ) ;
#91642 = LINE ( 'NONE', #6014, #130129 ) ;
#91643 = AXIS2_PLACEMENT_3D ( 'NONE', #131482, #119158, #61959 ) ;
#91644 = ORIENTED_EDGE ( 'NONE', *, *, #64070, .T. ) ;
#91645 = CARTESIAN_POINT ( 'NONE',  ( 8.999999999999941380, 4.552185695429119328, 5.000000000000000000 ) ) ;
#91646 = LINE ( 'NONE', #134453, #131556 ) ;
#91647 = CARTESIAN_POINT ( 'NONE',  ( 56.20376352523144448, 6.109999999999999432, 1.122388791418549108E-15 ) ) ;
#91648 = DIRECTION ( 'NONE',  ( -0.000000000000000000, 0.3543493200069153248, 0.9351131265310292928 ) ) ;
#91649 = CARTESIAN_POINT ( 'NONE',  ( 31.28752705046289151, 0.000000000000000000, -7.949999999999998401 ) ) ;
#91650 = ORIENTED_EDGE ( 'NONE', *, *, #31380, .F. ) ;
#91651 = VECTOR ( 'NONE', #49321, 1000.000000000000000 ) ;
#91652 = DIRECTION ( 'NONE',  ( 0.7071067811865487940, 0.7071067811865463515, -0.000000000000000000 ) ) ;
#91653 = ADVANCED_FACE ( 'NONE', ( #51265 ), #95460, .F. ) ;
#91654 = VERTEX_POINT ( 'NONE', #127375 ) ;
#91655 = CARTESIAN_POINT ( 'NONE',  ( -39.18398860626899705, 28.73617430169814568, 5.000000000000000000 ) ) ;
#91656 = FACE_OUTER_BOUND ( 'NONE', #138278, .T. ) ;
#91657 = FACE_OUTER_BOUND ( 'NONE', #60347, .T. ) ;
#91658 = CARTESIAN_POINT ( 'NONE',  ( 3.299744871391591339, -27.71228299555208352, 4.000000000000000000 ) ) ;
#91659 = CARTESIAN_POINT ( 'NONE',  ( 42.48921356237308800, -27.52281430457085065, 5.000000000000000000 ) ) ;
#91660 = ORIENTED_EDGE ( 'NONE', *, *, #91505, .T. ) ;
#91661 = ORIENTED_EDGE ( 'NONE', *, *, #47878, .F. ) ;
#91662 = CARTESIAN_POINT ( 'NONE',  ( -18.79289321881331887, 9.759292476615614831, 5.000000000000000000 ) ) ;
#91663 = CARTESIAN_POINT ( 'NONE',  ( 9.591592354503321260, -5.777789833161707559E-31, 2.500000000000001332 ) ) ;
#91664 = CARTESIAN_POINT ( 'NONE',  ( -21.29974487139158512, -27.71228299555221142, 4.000000000000000000 ) ) ;
#91665 = ADVANCED_FACE ( 'NONE', ( #28074 ), #81777, .T. ) ;
#91666 = VECTOR ( 'NONE', #115719, 1000.000000000000000 ) ;
#91667 = CARTESIAN_POINT ( 'NONE',  ( 117.6666666666666714, 6.884901960086285300, 3.975000000000003642 ) ) ;
#91668 = CARTESIAN_POINT ( 'NONE',  ( 76.05836038379621300, -7.949999999999997513, -2.130196079827425759 ) ) ;
#91669 = VECTOR ( 'NONE', #24132, 1000.000000000000227 ) ;
#91670 = DIRECTION ( 'NONE',  ( -4.681814790819591790E-17, -0.3543493200069152693, 0.9351131265310292928 ) ) ;
#91671 = ORIENTED_EDGE ( 'NONE', *, *, #86390, .F. ) ;
#91672 = CARTESIAN_POINT ( 'NONE',  ( 67.93750000000000000, 5.819803920172573974, -5.819803920172572198 ) ) ;
#91673 = AXIS2_PLACEMENT_3D ( 'NONE', #79904, #68998, #124781 ) ;
#91674 = CARTESIAN_POINT ( 'NONE',  ( -15.29974487139158867, -27.71228299555216879, 4.000000000000000000 ) ) ;
#91675 = VECTOR ( 'NONE', #97932, 1000.000000000000000 ) ;
#91676 = EDGE_CURVE ( 'NONE', #96881, #135052, #116510, .T. ) ;
#91677 = DIRECTION ( 'NONE',  ( 0.3543493200069163240, -0.000000000000000000, 0.9351131265310288487 ) ) ;
#91678 = VECTOR ( 'NONE', #66708, 999.9999999999998863 ) ;
#91679 = ORIENTED_EDGE ( 'NONE', *, *, #80076, .F. ) ;
#91680 = DIRECTION ( 'NONE',  ( 0.7071067811865487940, 0.7071067811865463515, 0.000000000000000000 ) ) ;
#91681 = EDGE_CURVE ( 'NONE', #65370, #76484, #105601, .T. ) ;
#91682 = DIRECTION ( 'NONE',  ( -0.7071067811865487940, 0.7071067811865463515, 0.000000000000000000 ) ) ;
#91683 = CARTESIAN_POINT ( 'NONE',  ( 63.87543019189810423, -5.291415217122920289, -3.055000000000001492 ) ) ;
#91684 = DIRECTION ( 'NONE',  ( -0.6830127018922180770, -0.6830127018922204085, -0.2588190451025213501 ) ) ;
#91685 = ORIENTED_EDGE ( 'NONE', *, *, #123402, .F. ) ;
#91686 = ORIENTED_EDGE ( 'NONE', *, *, #125848, .T. ) ;
#91687 = CARTESIAN_POINT ( 'NONE',  ( 9.707106781186483957, 2.259292476615696099, 5.000000000000000000 ) ) ;
#91688 = CARTESIAN_POINT ( 'NONE',  ( 12.29974487139158512, -27.71228299555214747, 4.000000000000000000 ) ) ;
#91689 = CARTESIAN_POINT ( 'NONE',  ( 43.72916666666666430, 7.950000000000001954, -2.130196079827421762 ) ) ;
#91690 = EDGE_CURVE ( 'NONE', #79341, #31148, #128115, .T. ) ;
#91691 = CARTESIAN_POINT ( 'NONE',  ( 33.79289321881321939, -11.24070752338417023, 5.000000000000000000 ) ) ;
#91693 = EDGE_LOOP ( 'NONE', ( #94710, #21396, #84501, #37694 ) ) ;
#91692 = LINE ( 'NONE', #14120, #17424 ) ;
#91694 = FACE_OUTER_BOUND ( 'NONE', #137368, .T. ) ;
#91695 = DIRECTION ( 'NONE',  ( -1.000000000000000000, 0.000000000000000000, 0.000000000000000000 ) ) ;
#91696 = CARTESIAN_POINT ( 'NONE',  ( -36.48921356237310221, -27.52281430457080802, 5.000000000000000000 ) ) ;
#91697 = FACE_OUTER_BOUND ( 'NONE', #68327, .T. ) ;
#91698 = ORIENTED_EDGE ( 'NONE', *, *, #34780, .F. ) ;
#91699 = ORIENTED_EDGE ( 'NONE', *, *, #77951, .F. ) ;
#91700 = EDGE_CURVE ( 'NONE', #47857, #90251, #95930, .T. ) ;
#91701 = ORIENTED_EDGE ( 'NONE', *, *, #139529, .F. ) ;
#91702 = FACE_OUTER_BOUND ( 'NONE', #115509, .T. ) ;
#91703 = PLANE ( 'NONE',  #29491 ) ;
#91704 = CARTESIAN_POINT ( 'NONE',  ( 34.91107144025653497, 21.84219451764873909, 4.000000000000000000 ) ) ;
#91705 = DIRECTION ( 'NONE',  ( -1.000000000000000000, -0.000000000000000000, -0.000000000000000000 ) ) ;
#91706 = LINE ( 'NONE', #14855, #52423 ) ;
#91707 = VERTEX_POINT ( 'NONE', #108440 ) ;
#91708 = VERTEX_POINT ( 'NONE', #30205 ) ;
#91709 = AXIS2_PLACEMENT_3D ( 'NONE', #102416, #124852, #36425 ) ;
#91710 = LINE ( 'NONE', #36612, #104720 ) ;
#91711 = CARTESIAN_POINT ( 'NONE',  ( -19.92362232443690218, -3.158997490844367206, -35.05992480806695255 ) ) ;
#91712 = ADVANCED_FACE ( 'NONE', ( #43247 ), #132426, .F. ) ;
#91713 = ORIENTED_EDGE ( 'NONE', *, *, #43133, .F. ) ;
#91714 = EDGE_CURVE ( 'NONE', #32886, #133889, #77326, .T. ) ;
#91715 = CARTESIAN_POINT ( 'NONE',  ( -34.92499999999997584, 0.000000000000000000, -40.00000000000000000 ) ) ;
#91716 = ORIENTED_EDGE ( 'NONE', *, *, #62800, .T. ) ;
#91717 = CARTESIAN_POINT ( 'NONE',  ( 24.18398860626899705, 28.73617430169804265, 5.000000000000000000 ) ) ;
#91718 = DIRECTION ( 'NONE',  ( -0.7071067811865486830, -0.7071067811865464625, -0.000000000000000000 ) ) ;
#91719 = ORIENTED_EDGE ( 'NONE', *, *, #69792, .F. ) ;
#91720 = FACE_BOUND ( 'NONE', #103795, .T. ) ;
#91721 = EDGE_CURVE ( 'NONE', #81979, #7814, #64272, .T. ) ;
#91722 = LINE ( 'NONE', #112069, #57209 ) ;
#91723 = DIRECTION ( 'NONE',  ( -2.781805975412905890E-17, 0.3543493200069152693, 0.9351131265310292928 ) ) ;
#91724 = CARTESIAN_POINT ( 'NONE',  ( 37.70419371712956291, -6.884901960086285300, -3.975000000000000089 ) ) ;
#91725 = CARTESIAN_POINT ( 'NONE',  ( 2.816011393730999401, 28.73617430169785436, 5.000000000000000000 ) ) ;
#91726 = PRODUCT_DEFINITION ( 'UNKNOWN', '', #111928, #38605 ) ;
#91727 = PRESENTATION_STYLE_ASSIGNMENT (( #99748 ) ) ;
#91728 = DIRECTION ( 'NONE',  ( -1.174948068637433935E-32, 1.000000000000000000, 5.385658160551468748E-32 ) ) ;
#91730 = VERTEX_POINT ( 'NONE', #74452 ) ;
#91729 = VECTOR ( 'NONE', #140258, 1000.000000000000000 ) ;
#91731 = EDGE_LOOP ( 'NONE', ( #54624, #119857, #103633, #39928 ) ) ;
#91732 = CARTESIAN_POINT ( 'NONE',  ( 97.76626352523145158, 4.472830434245838482, -4.472830434245837594 ) ) ;
#91733 = VERTEX_POINT ( 'NONE', #109192 ) ;
#91734 = VECTOR ( 'NONE', #16447, 1000.000000000000000 ) ;
#91735 = DIRECTION ( 'NONE',  ( -0.7071067811865486830, -0.7071067811865464625, -0.000000000000000000 ) ) ;
#91736 = DIRECTION ( 'NONE',  ( -0.7071067811865486830, 0.7071067811865464625, 0.000000000000000000 ) ) ;
#91737 = DIRECTION ( 'NONE',  ( 0.000000000000000000, -1.000000000000000000, 0.000000000000000000 ) ) ;
#91738 = CARTESIAN_POINT ( 'NONE',  ( 36.48921356237310221, -27.52281430457080802, 5.000000000000000000 ) ) ;
#91739 = EDGE_LOOP ( 'NONE', ( #124192, #52695, #10177, #12315, #138392 ) ) ;
#91740 = DIRECTION ( 'NONE',  ( 0.6830127018922181881, 0.6830127018922202975, -0.2588190451025214056 ) ) ;
#91741 = CARTESIAN_POINT ( 'NONE',  ( -33.79289321881321939, -14.24070752338414003, 5.000000000000000000 ) ) ;
#91742 = VECTOR ( 'NONE', #83352, 1000.000000000000000 ) ;
#91743 = CARTESIAN_POINT ( 'NONE',  ( -18.48921356237309510, -27.52281430457068367, 5.000000000000000000 ) ) ;
#91744 = CARTESIAN_POINT ( 'NONE',  ( 69.25000000000000000, -9.735942053221458872E-16, 7.950000000000000178 ) ) ;
#91745 = FACE_OUTER_BOUND ( 'NONE', #75832, .T. ) ;
#91746 = CARTESIAN_POINT ( 'NONE',  ( 8.585466709768445170, 3.821174125832445049E-16, 0.000000000000000000 ) ) ;
#91747 = ORIENTED_EDGE ( 'NONE', *, *, #123761, .F. ) ;
#91748 = DIRECTION ( 'NONE',  ( -0.6830127018922181881, 0.6830127018922202975, -0.2588190451025214056 ) ) ;
#91749 = CARTESIAN_POINT ( 'NONE',  ( -18.31657961132778212, -6.740707523384209310, 11.88629033278128588 ) ) ;
#91750 = VERTEX_POINT ( 'NONE', #85285 ) ;
#91752 = ORIENTED_EDGE ( 'NONE', *, *, #111619, .F. ) ;
#91751 = AXIS2_PLACEMENT_3D ( 'NONE', #21639, #66579, #132575 ) ;
#91753 = VERTEX_POINT ( 'NONE', #118644 ) ;
#91754 = CARTESIAN_POINT ( 'NONE',  ( 54.39626352523143993, 4.472830434245840259, -4.472830434245838482 ) ) ;
#91755 = ORIENTED_EDGE ( 'NONE', *, *, #107848, .T. ) ;
#91756 = VECTOR ( 'NONE', #24844, 1000.000000000000227 ) ;
#91757 = VECTOR ( 'NONE', #143066, 1000.000000000000000 ) ;
#91759 = EDGE_CURVE ( 'NONE', #53420, #102617, #22165, .T. ) ;
#91758 = AXIS2_PLACEMENT_3D ( 'NONE', #115927, #15195, #59472 ) ;
#91760 = CARTESIAN_POINT ( 'NONE',  ( 1.941639616203772123, -6.094999999999989093, 1.633150327867691765 ) ) ;
#91761 = VERTEX_POINT ( 'NONE', #20027 ) ;
#91762 = EDGE_CURVE ( 'NONE', #24475, #94208, #9877, .T. ) ;
#91763 = DIRECTION ( 'NONE',  ( 0.7071067811865486830, -0.7071067811865464625, -0.000000000000000000 ) ) ;
#91765 = EDGE_LOOP ( 'NONE', ( #846, #78658, #108477, #113718 ) ) ;
#91764 = EDGE_CURVE ( 'NONE', #90219, #109971, #32361, .T. ) ;
#91766 = CARTESIAN_POINT ( 'NONE',  ( -30.18398860626900060, 28.73617430169808173, 5.000000000000000000 ) ) ;
#91767 = VECTOR ( 'NONE', #141975, 1000.000000000000000 ) ;
#91769 = EDGE_LOOP ( 'NONE', ( #64328, #66994, #135298, #12268, #76551 ) ) ;
#91768 = CARTESIAN_POINT ( 'NONE',  ( -25.39999999999996305, 0.000000000000000000, 2.500000000000000000 ) ) ;
#91770 = ORIENTED_EDGE ( 'NONE', *, *, #99790, .T. ) ;
#91771 = EDGE_CURVE ( 'NONE', #17205, #89689, #97593, .T. ) ;
#91772 = DIRECTION ( 'NONE',  ( 0.7071067811865487940, -0.7071067811865463515, 0.000000000000000000 ) ) ;
#91773 = CARTESIAN_POINT ( 'NONE',  ( 81.48921356237309510, -27.52281430457112066, 5.000000000000000000 ) ) ;
#91774 = CARTESIAN_POINT ( 'NONE',  ( 128.3912635252314374, -4.472830434245839371, -4.472830434245839371 ) ) ;
#91775 = ORIENTED_EDGE ( 'NONE', *, *, #10546, .T. ) ;
#91776 = CARTESIAN_POINT ( 'NONE',  ( 18.70701326429291456, -21.74070752338405654, 4.999753212805210012 ) ) ;
#91777 = ORIENTED_EDGE ( 'NONE', *, *, #104560, .T. ) ;
#91778 = EDGE_LOOP ( 'NONE', ( #85925, #33236, #70652, #37838 ) ) ;
#91779 = ORIENTED_EDGE ( 'NONE', *, *, #70567, .T. ) ;
#91780 = DIRECTION ( 'NONE',  ( -0.7071067811865486830, -0.7071067811865464625, 0.000000000000000000 ) ) ;
#91781 = PLANE ( 'NONE',  #102455 ) ;
#91782 = ADVANCED_FACE ( 'NONE', ( #86752 ), #130972, .F. ) ;
#91783 = DIRECTION ( 'NONE',  ( 0.6830127018922181881, 0.6830127018922202975, -0.2588190451025214056 ) ) ;
#91784 = DIRECTION ( 'NONE',  ( 0.000000000000000000, -1.000000000000000000, 0.000000000000000000 ) ) ;
#91785 = ADVANCED_FACE ( 'NONE', ( #109909 ), #107944, .T. ) ;
#91786 = LINE ( 'NONE', #102689, #30339 ) ;
#91787 = VERTEX_POINT ( 'NONE', #120776 ) ;
#91788 = EDGE_CURVE ( 'NONE', #108392, #27000, #21486, .T. ) ;
#91789 = CARTESIAN_POINT ( 'NONE',  ( 27.10373647476855652, 5.808823158059036373, 5.808823158059032821 ) ) ;
#91790 = CARTESIAN_POINT ( 'NONE',  ( 0.000000000000000000, 0.000000000000000000, 5.000000000000000000 ) ) ;
#91791 = DIRECTION ( 'NONE',  ( 0.6830127018922181881, 0.6830127018922202975, -0.2588190451025214056 ) ) ;
#91792 = DIRECTION ( 'NONE',  ( -0.000000000000000000, 0.3543493200069153248, 0.9351131265310292928 ) ) ;
#91793 = ORIENTED_EDGE ( 'NONE', *, *, #104405, .F. ) ;
#91794 = VERTEX_POINT ( 'NONE', #10572 ) ;
#91795 = ORIENTED_EDGE ( 'NONE', *, *, #121448, .T. ) ;
#91796 = CARTESIAN_POINT ( 'NONE',  ( 14.27718569542929572, -21.72500000000000142, 5.000000000000000000 ) ) ;
#91797 = DIRECTION ( 'NONE',  ( 0.7071067811865487940, 0.7071067811865463515, 0.000000000000000000 ) ) ;
#91798 = ADVANCED_FACE ( 'NONE', ( #107752 ), #99016, .F. ) ;
#91799 = DIRECTION ( 'NONE',  ( 0.6830127018922181881, 0.6830127018922202975, -0.2588190451025214056 ) ) ;
#91800 = AXIS2_PLACEMENT_3D ( 'NONE', #53741, #118234, #88507 ) ;
#91801 = LINE ( 'NONE', #37447, #79909 ) ;
#91802 = CARTESIAN_POINT ( 'NONE',  ( -42.48921356237308800, -27.52281430457085065, 5.000000000000000000 ) ) ;
#91803 = CARTESIAN_POINT ( 'NONE',  ( 26.29289321881326913, 20.25929247661551713, 5.000000000000000000 ) ) ;
#91804 = LINE ( 'NONE', #4743, #138985 ) ;
#91805 = DIRECTION ( 'NONE',  ( -0.000000000000000000, 0.3543493200069153248, 0.9351131265310292928 ) ) ;
#91806 = DIRECTION ( 'NONE',  ( -0.7071067811865486830, -0.7071067811865464625, 0.000000000000000000 ) ) ;
#91807 = LINE ( 'NONE', #137480, #99915 ) ;
#91808 = CARTESIAN_POINT ( 'NONE',  ( 36.48921356237310221, -27.52281430457080802, 5.000000000000000000 ) ) ;
#91809 = LINE ( 'NONE', #135355, #141444 ) ;
#91810 = EDGE_CURVE ( 'NONE', #107864, #63125, #52668, .T. ) ;
#91811 = AXIS2_PLACEMENT_3D ( 'NONE', #14804, #106063, #61907 ) ;
#91812 = ORIENTED_EDGE ( 'NONE', *, *, #66273, .F. ) ;
#91813 = CARTESIAN_POINT ( 'NONE',  ( 16.45742106731621490, 0.9613713492673634509, -33.49048331797055766 ) ) ;
#91814 = VERTEX_POINT ( 'NONE', #41808 ) ;
#91815 = DIRECTION ( 'NONE',  ( -0.7071067811865486830, -0.7071067811865464625, 0.000000000000000000 ) ) ;
#91817 = ORIENTED_EDGE ( 'NONE', *, *, #89180, .F. ) ;
#91816 = LINE ( 'NONE', #57803, #90392 ) ;
#91818 = VECTOR ( 'NONE', #133468, 1000.000000000000000 ) ;
#91819 = CARTESIAN_POINT ( 'NONE',  ( 39.48921356237310221, -27.52281430457082934, 5.000000000000000000 ) ) ;
#91820 = CARTESIAN_POINT ( 'NONE',  ( 0.000000000000000000, 9.735942053221458872E-16, -7.950000000000000178 ) ) ;
#91821 = ORIENTED_EDGE ( 'NONE', *, *, #103825, .T. ) ;
#91822 = LINE ( 'NONE', #135367, #53046 ) ;
#91823 = EDGE_LOOP ( 'NONE', ( #47410, #142909, #87242, #97530 ) ) ;
#91824 =( NAMED_UNIT ( * ) PLANE_ANGLE_UNIT ( ) SI_UNIT ( $, .RADIAN. ) );
#91825 = ORIENTED_EDGE ( 'NONE', *, *, #97169, .F. ) ;
#91826 = CARTESIAN_POINT ( 'NONE',  ( 15.18398860626900237, 28.73617430169797871, 5.000000000000000000 ) ) ;
#91827 = EDGE_CURVE ( 'NONE', #3834, #112546, #86022, .T. ) ;
#91828 = VECTOR ( 'NONE', #13993, 999.9999999999998863 ) ;
#91829 = CARTESIAN_POINT ( 'NONE',  ( 104.9333603837962130, 2.130196079827431532, -7.949999999999997513 ) ) ;
#91830 = CARTESIAN_POINT ( 'NONE',  ( 71.87500000000000000, 7.950000000000000178, 1.460391307983218535E-15 ) ) ;
#91831 = DIRECTION ( 'NONE',  ( 0.7071067811865486830, -0.7071067811865464625, -0.000000000000000000 ) ) ;
#91832 = ORIENTED_EDGE ( 'NONE', *, *, #61867, .T. ) ;
#91833 = VECTOR ( 'NONE', #23613, 999.9999999999998863 ) ;
#91834 = LINE ( 'NONE', #136059, #28747 ) ;
#91835 = DIRECTION ( 'NONE',  ( 0.7071067811865486830, -0.7071067811865464625, -0.000000000000000000 ) ) ;
#91836 =( GEOMETRIC_REPRESENTATION_CONTEXT ( 3 ) GLOBAL_UNCERTAINTY_ASSIGNED_CONTEXT ( ( #129076 ) ) GLOBAL_UNIT_ASSIGNED_CONTEXT ( ( #99489, #161, #41555 ) ) REPRESENTATION_CONTEXT ( 'NONE', 'WORKASPACE' ) );
#91837 = CARTESIAN_POINT ( 'NONE',  ( 23.47916666666666785, 6.094999999999988205, -1.633150327867694651 ) ) ;
#91838 = CARTESIAN_POINT ( 'NONE',  ( -9.838293875473743455, -6.740707523384205757, 16.75550250614864822 ) ) ;
#91839 =( LENGTH_UNIT ( ) NAMED_UNIT ( * ) SI_UNIT ( .MILLI., .METRE. ) );
#91840 = LINE ( 'NONE', #25880, #36227 ) ;
#91841 = VERTEX_POINT ( 'NONE', #99744 ) ;
#91842 = DIRECTION ( 'NONE',  ( -0.7071067811865487940, 0.7071067811865463515, 0.000000000000000000 ) ) ;
#91843 = ORIENTED_EDGE ( 'NONE', *, *, #31053, .F. ) ;
#91844 = ADVANCED_FACE ( 'NONE', ( #78721 ), #47564, .F. ) ;
#91845 = CARTESIAN_POINT ( 'NONE',  ( 93.18793019189809002, 6.110000000000002984, -1.637169565754156730 ) ) ;
#91846 = FACE_OUTER_BOUND ( 'NONE', #110027, .T. ) ;
#91847 = LINE ( 'NONE', #73512, #76155 ) ;
#91848 = LINE ( 'NONE', #135395, #9873 ) ;
#91849 = DIRECTION ( 'NONE',  ( 0.6830127018922180770, -0.6830127018922204085, -0.2588190451025213501 ) ) ;
#91850 = ORIENTED_EDGE ( 'NONE', *, *, #111540, .T. ) ;
#91851 = CARTESIAN_POINT ( 'NONE',  ( 6.471592354503322042, -2.500000000000000000, 3.061616997868384127E-16 ) ) ;
#91852 = DIRECTION ( 'NONE',  ( -1.000000000000000000, -1.224606353822377258E-16, -0.000000000000000000 ) ) ;
#91853 = VECTOR ( 'NONE', #88885, 1000.000000000000000 ) ;
#91854 = ORIENTED_EDGE ( 'NONE', *, *, #10607, .T. ) ;
#91855 = EDGE_CURVE ( 'NONE', #49148, #89661, #12009, .T. ) ;
#91856 = PLANE ( 'NONE',  #84170 ) ;
#91858 = ORIENTED_EDGE ( 'NONE', *, *, #81799, .T. ) ;
#91857 = CARTESIAN_POINT ( 'NONE',  ( 0.000000000000000000, 0.000000000000000000, 7.950000000000000178 ) ) ;
#91859 = CARTESIAN_POINT ( 'NONE',  ( -10.36246187583893175, 22.22500000000000853, 4.000000000000000000 ) ) ;
#91860 = DIRECTION ( 'NONE',  ( -0.3543493200069162685, -0.000000000000000000, -0.9351131265310288487 ) ) ;
#91861 = DIRECTION ( 'NONE',  ( 1.000000000000000000, 0.000000000000000000, 0.000000000000000000 ) ) ;
#91862 = AXIS2_PLACEMENT_3D ( 'NONE', #21100, #87791, #121124 ) ;
#91863 = PRESENTATION_STYLE_ASSIGNMENT (( #70860 ) ) ;
#91865 = AXIS2_PLACEMENT_3D ( 'NONE', #97342, #42309, #75636 ) ;
#91864 = VECTOR ( 'NONE', #26818, 1000.000000000000227 ) ;
#91866 = EDGE_LOOP ( 'NONE', ( #1997, #141312, #70687, #124693 ) ) ;
#91867 = EDGE_LOOP ( 'NONE', ( #137580, #48119, #82581, #102858, #118321 ) ) ;
#91868 = EDGE_LOOP ( 'NONE', ( #9167, #128467, #58769, #118988 ) ) ;
#91869 = VECTOR ( 'NONE', #114997, 1000.000000000000000 ) ;
#91870 = CARTESIAN_POINT ( 'NONE',  ( 85.16709685856477563, -3.055000000000000160, -5.291415217122921177 ) ) ;
#91871 = ORIENTED_EDGE ( 'NONE', *, *, #127720, .F. ) ;
#91872 = DIRECTION ( 'NONE',  ( 0.000000000000000000, 0.000000000000000000, 1.000000000000000000 ) ) ;
#91873 = AXIS2_PLACEMENT_3D ( 'NONE', #57142, #135409, #46266 ) ;
#91874 = LINE ( 'NONE', #70870, #101215 ) ;
#91876 = AXIS2_PLACEMENT_3D ( 'NONE', #63382, #6061, #97363 ) ;
#91875 = LINE ( 'NONE', #72322, #13306 ) ;
#91877 = LINE ( 'NONE', #81029, #124155 ) ;
#91878 = ORIENTED_EDGE ( 'NONE', *, *, #91762, .F. ) ;
#91879 = DIRECTION ( 'NONE',  ( 0.7071067811865486830, -0.7071067811865464625, -0.000000000000000000 ) ) ;
#91880 = LINE ( 'NONE', #111494, #95250 ) ;
#91881 = DIRECTION ( 'NONE',  ( 0.7071067811865486830, -0.7071067811865464625, -0.000000000000000000 ) ) ;
#91882 = CARTESIAN_POINT ( 'NONE',  ( 74.57876352523145158, -7.482591942790325086E-16, 6.109999999999998543 ) ) ;
#91883 = VERTEX_POINT ( 'NONE', #88903 ) ;
#91884 = EDGE_CURVE ( 'NONE', #30305, #122724, #79484, .T. ) ;
#91885 = CARTESIAN_POINT ( 'NONE',  ( -3.489213562373097322, -27.52281430457057709, 5.000000000000000000 ) ) ;
#91886 = CARTESIAN_POINT ( 'NONE',  ( 156.1500000000000057, -57.14999999999999147, -49.92499999999968452 ) ) ;
#91887 = LINE ( 'NONE', #89749, #86340 ) ;
#91888 = ORIENTED_EDGE ( 'NONE', *, *, #5928, .T. ) ;
#91889 = ORIENTED_EDGE ( 'NONE', *, *, #90982, .T. ) ;
#91890 = EDGE_CURVE ( 'NONE', #89147, #57984, #13421, .T. ) ;
#91891 = CARTESIAN_POINT ( 'NONE',  ( -29.99451991528749417, 28.92564299267958816, 4.000000000000000000 ) ) ;
#91892 = EDGE_CURVE ( 'NONE', #37103, #92014, #50256, .T. ) ;
#91893 = LINE ( 'NONE', #57883, #142658 ) ;
#91894 = CARTESIAN_POINT ( 'NONE',  ( 14.99451991528749595, 28.92564299267948513, 4.000000000000000000 ) ) ;
#91895 = CIRCLE ( 'NONE', #124295, 2.500000000000000888 ) ;
#91896 = CARTESIAN_POINT ( 'NONE',  ( 12.82439460721831104, -2.055000000000000160, 2.789133085058097101E-16 ) ) ;
#91897 = DIRECTION ( 'NONE',  ( -0.7071067811865486830, -0.7071067811865464625, 0.000000000000000000 ) ) ;
#91898 = CARTESIAN_POINT ( 'NONE',  ( -51.18398860626899705, 28.73617430169823095, 5.000000000000000000 ) ) ;
#91899 = PRESENTATION_STYLE_ASSIGNMENT (( #68757 ) ) ;
#91900 = VECTOR ( 'NONE', #82147, 1000.000000000000000 ) ;
#91901 = VERTEX_POINT ( 'NONE', #1809 ) ;
#91902 = VERTEX_POINT ( 'NONE', #133123 ) ;
#91903 = CARTESIAN_POINT ( 'NONE',  ( -15.48921356237309510, -27.52281430457066236, 5.000000000000000000 ) ) ;
#91904 = VERTEX_POINT ( 'NONE', #67885 ) ;
#91905 = VECTOR ( 'NONE', #57155, 1000.000000000000000 ) ;
#91906 = EDGE_CURVE ( 'NONE', #75984, #19139, #91722, .T. ) ;
#91907 =( BOUNDED_CURVE ( )  B_SPLINE_CURVE ( 3, ( #24325, #33109, #134537, #56291 ),
 .UNSPECIFIED., .F., .F. ) 
 B_SPLINE_CURVE_WITH_KNOTS ( ( 4, 4 ),
 ( 2.779374508378135378, 4.199602562396851368 ),
 .UNSPECIFIED. ) 
 CURVE ( )  GEOMETRIC_REPRESENTATION_ITEM ( )  RATIONAL_B_SPLINE_CURVE ( ( 1.000000000000000000, 0.8388583629366601624, 0.8388583629366601624, 1.000000000000000000 ) ) 
 REPRESENTATION_ITEM ( '' )  );
#91908 = DIRECTION ( 'NONE',  ( -1.000000000000000000, -1.224606353822377258E-16, -0.000000000000000000 ) ) ;
#91909 = VERTEX_POINT ( 'NONE', #46111 ) ;
#91910 = LINE ( 'NONE', #89765, #140881 ) ;
#91911 = CARTESIAN_POINT ( 'NONE',  ( -30.32816939922332367, -21.74070752338405654, 4.000000000000000000 ) ) ;
#91912 = LINE ( 'NONE', #46320, #29507 ) ;
#91913 = VECTOR ( 'NONE', #106606, 1000.000000000000000 ) ;
#91914 = CARTESIAN_POINT ( 'NONE',  ( 15.52000000000000135, -2.055000000000000160, 0.000000000000000000 ) ) ;
#91915 =( BOUNDED_SURFACE ( )  B_SPLINE_SURFACE ( 1, 2, ( 
 ( #127822, #7423, #3320, #91774, #95159, #29193, #36000, #73434, #18287, #51684, #36674, #134597, #103349, #35295, #48272, #79538, #24382, #68631, #112814, #2609, #13471, #46916, #101945, #135317, #80226, #124410, #135998, #14921, #42244, #85003, #132103, #66136, #85703, #131375, #109609, #40802, #108865, #110301, #10978, #75574, #10287, #32058, #97269, #8816, #63979, #141540, #140125, #119743, #19745, #118333, #108149, #86455, #95877, #74140, #129948, #98036, #130682, #30649, #76290, #9559, #20443, #53832, #119055, #21175, #129211, #74880, #53074, #42955, #31355, #142269, #64695, #87152, #65431, #29898, #21886, #120447, #54546, #19036, #32797, #107468, #63300, #98724, #8131, #142953, #43645, #87864, #52371, #77020, #121193, #96558, #140796, #41494, #121893, #55982, #47275, #67572, #36348, #57398, #13128, #89294, #78423, #124065, #88601, #133519, #122621, #2241, #34206, #101578, #45811, #46553, #24740, #99426, #124771, #45117, #13839, #113895, #135659, #66835, #69712, #79892, #55246, #90742, #68986, #23292, #25442, #134969, #80576, #22566, #111764, #35667, #111014, #100180, #91446, #12430, #91, #113165, #58136, #56713, #102333, #100874, #44394, #1529, #830, #2981, #68298, #123375, #132832, #33516, #89987, #77717, #11694, #134236, #34929, #79171, #24039, #112475, #105846, #84161, #93577, #37046, #126205, #138512, #39199, #39942, #26185, #60256, #116015, #128360, #137083, #115274, #83425, #127638, #59545, #50085, #105157, #16720, #104432, #28331, #126887, #60998, #71849, #72592, #14583, #29032, #5810, #70447, #82708, #114592, #116747, #94276, #17428, #61685, #73269, #15964, #5093, #3664, #50786, #58865, #4346, #6505, #94974, #103025, #27584, #47961, #92125, #137810, #139247, #136355, #49394, #71129, #26882, #38485, #81294, #125498, #82026, #15260, #103700, #48650, #92847, #37785, #107293, #119575, #107979, #52203, #97860, #130506, #141352, #75400, #42785, #86976, #106555, #20271, #131199, #20993, #31886, #97093, #117433, #73967, #85525, #64512, #18108, #31185, #10124, #43478, #19573, #7239, #41316, #129762, #131925, #120277, #87690, #98560, #62392, #108688, #76107, #65256, #63118, #9374, #109439, #51514, #95706, #53649, #139958, #96392, #54385, #52889, #63817, #142099, #142787, #32618, #140630, #118885, #8652, #40636, #84839, #129046, #29718, #118144, #42068, #86282, #18851, #7964, #30463, #74704, #143491, #21724, #668, #44211, #88427, #134064, #10815, #78261, #76850, #122444, #100720, #1365, #44959, #22403, #23109, #34753, #132667, #89136, #79729, #134799, #89822, #100004, #121025, #133354, #78990, #111583, #12262, #101414, #65978, #123198, #67394, #56549, #45648, #34046, #110135, #66667, #35496, #23871, #55078, #33359, #99248, #68136, #46376, #77557, #2065, #112314, #12963, #121727, #110831, #57240, #90562, #11521, #123912, #55802, #95377, #62779, #94649, #117121, #38867, #93951, #5494, #83087, #81687, #61382, #104827, #59919, #49772, #127290, #37449, #15630, #27254, #39601, #29404, #138184, #18504, #83833, #138908, #71502, #62069, #115665, #106961, #27988, #126564, #17795, #50465, #105527, #106228, #128727, #16360, #6900, #40323, #70805, #128041, #17114, #72258, #28721, #73639, #7641, #116428, #104087, #6189, #51178, #139644, #51901, #49044, #72965, #84532, #96081, #60663, #117815, #125889, #26562, #82387, #114950, #4741, #93241, #137474, #38167, #109102, #142475, #54064, #54756, #140319, #11185, #98252, #8336, #64915, #52585, #98936, #32282, #76513, #87376, #110515, #97507, #86669, #129429, #33024, #55466, #130171, #120681, #10498, #85206, #9791, #30866, #143171, #22091, #43164, #21402, #141767, #53296, #108354, #42469, #41006, #20663, #64196, #19254, #9031, #130895, #30117, #118553, #75094, #131591, #31567, #119261, #65666, #109830, #43873, #88088, #19952, #132331, #74365, #75790, #119953, #77241, #121408, #66348, #63510, #107676, #96763, #141015, #41721, #85933, #58365, #14796, #36550, #111237, #114112, #124275, #99651, #101807, #113379, #78638, #69944, #57616, #80785, #22773, #122850, #135188, #67051, #100396, #77933, #2465, #122119, #23530, #102545, #35154, #1734, #35877, #124986, #25666, #67801, #101085, #46028, #322, #91647, #69196, #3196, #88815, #79398, #123599, #11925, #14069, #56213, #44623, #1039, #133043, #56912, #45327, #89503, #80093, #133737, #24254, #33726, #134454, #46774, #90956, #12644, #34413, #68501, #24941, #111992, #90212, #112680, #13348, #47484, #135870, #59068, #126403, #105363, #38700, #127114, #61900, #103225, #6021, #49607, #82927, #93789, #27095, #117642, #114793, #106055, #16944, #29234, #81516, #128561, #71337, #50299, #73476, #61219, #82231, #38005, #6722, #28547, #125723, #16189, #3875, #26403, #48153, #92333, #95205, #51007, #136562, #37273, #27814, #15474, #70649, #94485, #59755, #5326, #103916, #104654, #115491, #60480, #4565, #17627, #138015, #127869, #72806, #48872, #138734, #116960, #139475, #40160, #72081, #93077, #137306, #116254, #39428, #83660, #84372, #54582, #87901, #64022, #51727, #85752, #30692, #32839, #21218, #132145, #143000, #62599, #9601, #87194, #76326, #107510, #31391, #131421, #106785, #120488, #8171, #75613, #32100, #7468, #140161, #64727, #40838, #140836, #65473, #97314, #108191, #53879, #43687, #77060, #41526, #19782, #8851, #18324, #10327, #109653, #98762, #95922, #141585, #42285, #85047, #129251, #74182, #29939, #118376, #19077, #119099, #63339, #52410, #98074, #96596, #86494, #129987, #53113, #20481, #108911, #74921, #130725, #119788, #142309, #42993, #122660, #49248, #4948, #114460, #133565, #121234, #45158, #26048, #100914, #47834, #126082, #21927, #70310, #111806, #3535, #12472, #89333, #38350, #33559, #26748, #81150, #93441, #136, #137676, #34247, #15136, #66173, #125360, #867, #100218, #70998, #92706, #44438, #78469, #110343, #88638, #11020, #55294, #15820, #115147, #99464, #132869, #92000, #77759, #121936 ),
 ( #11741, #23344, #59418, #67617, #103575, #56755, #4212, #48504, #22608, #66877, #111051, #81890, #56027, #60117, #136218, #36903, #136939, #37652, #104283, #52765, #39799, #28899, #71700, #118745, #96956, #72445, #117998, #96252, #27440, #95566, #116613, #140497, #107850, #139830, #18700, #84025, #139096, #50644, #128221, #126756, #106405, #6367, #105013, #94832, #73134, #82566, #60857, #17293, #84703, #117303, #61558, #62979, #40503, #7095, #128909, #105707, #7833, #115867, #17973, #62251, #29589, #51372, #73826, #107154, #52078, #41184, #16566, #8516, #85394, #129618, #141208, #19440, #94133, #5685, #30319, #49950, #74557, #63690, #138370, #39056, #83278, #127488, #28186, #20855, #77432, #108549, #42654, #33906, #54254, #22973, #44064, #143357, #75970, #66532, #120142, #111441, #9988, #131064, #22264, #54948, #110009, #110699, #133230, #65115, #11377, #44821, #75275, #88284, #21593, #98434, #132532, #78126, #12122, #120882, #64378, #142655, #55658, #99859, #67240, #53508, #87559, #33219, #56407, #109305, #43348, #522, #89006, #86856, #121596, #122299, #100588, #131785, #41924, #10674, #86136, #99113, #130364, #31055, #119440, #20137, #97713, #9226, #141967, #31753, #32474, #76713, #65853, #25137, #68684, #23727, #13535, #91153, #1231, #123051, #134656, #3373, #135374, #79595, #125184, #14274, #69392, #102727, #24436, #70139, #34608, #35350, #112871, #91829, #123778, #47668, #36056, #136054, #114300, #45515, #70828, #57815, #103406, #59947, #81712, #12828, #15658, #25867, #89694, #36737, #14974, #102004, #114975, #80976, #125912, #67998, #2667, #59252, #112182, #1922, #136761, #46966, #26584, #4053, #48338, #80278, #92528, #124469, #133920, #113576, #90409, #37478, #58559, #78843, #57101, #101284, #46228, #128747, #106988, #137499, #106251, #83859, #116451, #51206, #51925, #30143, #39632, #126588, #72285, #84554, #29426, #129457, #115688, #6211, #62093, #74394, #83113, #61404, #73666, #117841, #5518, #139667, #95404, #6924, #50488, #18527, #72987, #40346, #17820, #62809, #104109, #118582, #7670, #16389, #28745, #60690, #96105, #140343, #41030, #85234, #19279, #105548, #94674, #93266, #4772, #49073, #93972, #38192, #82406, #27278, #117142, #138206, #71533, #104852, #49796, #38892, #138930, #17138, #128063, #127315, #28017, #120716, #75118, #131622, #119288, #22114, #98958, #143199, #10520, #33751, #20695, #9821, #52611, #99678, #77955, #53323, #43900, #77266, #8359, #76540, #97541, #121436, #88841, #21428, #88113, #64942, #119980, #31593, #109135, #107701, #87404, #130921, #85964, #75816, #54091, #63537, #41749, #141794, #65691, #98278, #42492, #132362, #109854, #32311, #54781, #86696, #33054, #96795, #142503, #43189, #66369, #110540, #11214, #55495, #354, #44650, #141045, #133069, #122139, #130199, #30890, #19974, #64221, #108382, #9063, #37296, #24965, #36569, #1756, #136589, #124299, #3896, #89528, #46057, #58388, #133757, #23558, #14818, #35179, #48172, #69224, #113408, #56936, #47507, #101109, #92360, #134480, #112015, #3215, #35899, #90983, #91668, #114134, #90236, #135891, #25692, #56240, #14091, #2486, #79425, #102571, #59088, #81543, #101833, #45352, #123622, #80817, #125010, #22803, #34439, #68523, #69969, #67077, #24275, #112707, #103248, #111262, #67826, #11954, #100420, #1066, #13369, #78663, #135211, #122871, #80115, #12667, #57646, #46801, #51755, #140181, #18351, #117665, #95946, #70670, #6046, #82250, #4589, #72831, #48897, #72104, #125747, #27838, #49633, #82944, #59776, #84393, #116277, #51030, #95229, #114814, #127892, #139501, #29260, #40184, #105387, #26422, #126425, #93810, #28572, #15496, #138759, #62627, #40866, #16971, #103942, #138037, #38723, #93102, #128584, #137333, #106807, #38026, #116981, #73502, #7497, #71360, #39455, #27116, #115518, #16212, #17652, #60503, #104681, #5349, #61242, #50319, #61924, #127142, #94506, #83684, #106076, #6749, #110372, #77089, #54607, #87928, #74209, #20504, #64759, #8192, #98789, #140862, #55320, #52434, #118402, #42313, #96622, #41559, #21246, #63367, #108941, #85072, #119814, #87224, #131447, #141610, #119125, #9631, #120520, #85782, #86523, #11045, #99493, #76352, #97346, #129277, #8876, #32124, #53909, #98103, #132173, #29966, #65504, #75642, #142334, #43015, #53143, #165, #130012, #32867, #109683, #19101, #107535, #30721, #130749, #10353, #74946, #143028, #108214, #64047, #121265, #43714, #19806, #31420, #21953, #66198, #56783, #44462, #111840, #90810, #24113, #112540, #47348, #88667, #135047, #35007, #68366, #79250, #12502, #103099, #100244, #91516, #2314, #14659, #66900, #113968, #100941, #35741, #58937, #46632, #67647, #23375, #135729, #13915, #111082, #1599, #132901, #11772, #33584, #77783, #80645, #36415, #121965, #22637, #13200, #898, #56056, #79959, #45184, #134309, #89360, #90059, #45884, #123455, #133594, #34272, #78493, #124130, #122690, #24813, #57474, #101656, #69058, #113238, #58215, #102407, #3053, #124842, #25517, #69791, #50153, #137882, #5884, #72662, #48024, #73340, #137160, #105919, #62459, #84231, #15332, #18184, #28399, #3734, #94350, #17500, #126275, #117509, #105230, #128428, #70520, #26951, #39280, #114662, #4415, #139326, #16038, #29102, #138586, #83503, #37861, #116819, #82095, #92195, #115351, #92925, #127717, #16796, #71927, #61754, #95056, #71204, #6583, #50858, #37117, #40015, #126969, #60330, #136424, #81372, #125579, #82783, #26256, #104511, #59619, #103775, #48724, #5169, #49467, #93655, #38555, #27660, #116096, #61073, #118225, #8720, #64588, #76922, #85603, #63890, #87055, #31958, #8035, #142170, #53731, #108761, #52973, #131270, #75474, #9451, #20342, #21065, #106628, #121096, #97933, #18932, #31259, #63199, #65334, #42856, #76187, #120347, #21794, #108052, #97168, #95779, #142860, #7323, #96459, #109515, #10190, #51585, #119643, #140702, #54453, #132000, #98628, #43547 ) ),
 .UNSPECIFIED., .F., .F., .T. ) 
 B_SPLINE_SURFACE_WITH_KNOTS ( ( 2, 2 ),
 ( 3, 2, 2, 2, 2, 2, 2, 2, 2, 2, 2, 2, 2, 2, 2, 2, 2, 2, 2, 2, 2, 2, 2, 2, 2, 2, 2, 2, 2, 2, 2, 2, 2, 2, 2, 2, 2, 2, 2, 2, 2, 2, 2, 2, 2, 2, 2, 2, 2, 2, 2, 2, 2, 2, 2, 2, 2, 2, 2, 2, 2, 2, 2, 2, 2, 2, 2, 2, 2, 2, 2, 2, 2, 2, 2, 2, 2, 2, 2, 2, 2, 2, 2, 2, 2, 2, 2, 2, 2, 2, 2, 2, 2, 2, 2, 2, 2, 2, 2, 2, 2, 2, 2, 2, 2, 2, 2, 2, 2, 2, 2, 2, 2, 2, 2, 2, 2, 2, 2, 2, 2, 2, 2, 2, 2, 2, 2, 2, 2, 2, 2, 2, 2, 2, 2, 2, 2, 2, 2, 2, 2, 2, 2, 2, 2, 2, 2, 2, 2, 2, 2, 2, 2, 2, 2, 2, 2, 2, 2, 2, 2, 2, 2, 2, 2, 2, 2, 2, 2, 2, 2, 2, 2, 2, 2, 2, 2, 2, 2, 2, 2, 2, 2, 2, 2, 2, 2, 2, 2, 2, 2, 2, 2, 2, 2, 2, 2, 2, 2, 2, 2, 2, 2, 2, 2, 2, 2, 2, 2, 2, 2, 2, 2, 2, 2, 2, 2, 2, 2, 2, 2, 2, 2, 2, 2, 2, 2, 2, 2, 2, 2, 2, 2, 2, 2, 2, 2, 2, 2, 2, 2, 2, 2, 2, 2, 2, 2, 2, 2, 2, 2, 2, 2, 2, 2, 2, 2, 2, 2, 2, 2, 2, 2, 2, 2, 2, 2, 2, 2, 2, 2, 2, 2, 2, 2, 2, 2, 2, 2, 2, 2, 2, 2, 2, 2, 2, 2, 2, 2, 2, 2, 2, 2, 2, 2, 2, 2, 2, 2, 2, 2, 2, 2, 2, 2, 2, 2, 2, 2, 2, 2, 2, 2, 2, 2, 2, 2, 2, 2, 2, 2, 2, 2, 2, 2, 2, 2, 2, 2, 2, 2, 2, 2, 2, 2, 2, 2, 2, 2, 2, 2, 2, 2, 2, 2, 2, 2, 2, 2, 2, 2, 3 ),
 ( 0.000000000000000000, 1.000000000000000000 ),
 ( 0.000000000000000000, 0.002777777777777777884, 0.005555555555555555768, 0.008333333333333333218, 0.01111111111111111154, 0.01388888888888888812, 0.01666666666666666644, 0.01944444444444444475, 0.02222222222222222307, 0.02500000000000000139, 0.02777777777777777624, 0.03055555555555555455, 0.03333333333333333287, 0.03611111111111110772, 0.03888888888888888951, 0.04166666666666666435, 0.04444444444444444614, 0.04722222222222222099, 0.05000000000000000278, 0.05277777777777777762, 0.05555555555555555247, 0.05833333333333333426, 0.06111111111111110911, 0.06388888888888888395, 0.06666666666666666574, 0.06944444444444444753, 0.07222222222222221544, 0.07499999999999999722, 0.07777777777777777901, 0.08055555555555556080, 0.08333333333333332871, 0.08611111111111111049, 0.08888888888888889228, 0.09166666666666666019, 0.09444444444444444198, 0.09722222222222222376, 0.1000000000000000056, 0.1027777777777777735, 0.1055555555555555552, 0.1083333333333333370, 0.1111111111111111049, 0.1138888888888888867, 0.1166666666666666685, 0.1194444444444444503, 0.1222222222222222182, 0.1250000000000000000, 0.1277777777777777679, 0.1305555555555555636, 0.1333333333333333315, 0.1361111111111110994, 0.1388888888888888951, 0.1416666666666666630, 0.1444444444444444309, 0.1472222222222222265, 0.1499999999999999944, 0.1527777777777777901, 0.1555555555555555580, 0.1583333333333333259, 0.1611111111111111216, 0.1638888888888888895, 0.1666666666666666574, 0.1694444444444444531, 0.1722222222222222210, 0.1749999999999999889, 0.1777777777777777846, 0.1805555555555555525, 0.1833333333333333204, 0.1861111111111111160, 0.1888888888888888840, 0.1916666666666666796, 0.1944444444444444475, 0.1972222222222222154, 0.2000000000000000111, 0.2027777777777777790, 0.2055555555555555469, 0.2083333333333333426, 0.2111111111111111105, 0.2138888888888888784, 0.2166666666666666741, 0.2194444444444444420, 0.2222222222222222099, 0.2250000000000000056, 0.2277777777777777735, 0.2305555555555555691, 0.2333333333333333370, 0.2361111111111111049, 0.2388888888888889006, 0.2416666666666666685, 0.2444444444444444364, 0.2472222222222222321, 0.2500000000000000000, 0.2527777777777777679, 0.2555555555555555358, 0.2583333333333333592, 0.2611111111111111271, 0.2638888888888888951, 0.2666666666666666630, 0.2694444444444444309, 0.2722222222222221988, 0.2750000000000000222, 0.2777777777777777901, 0.2805555555555555580, 0.2833333333333333259, 0.2861111111111110938, 0.2888888888888888618, 0.2916666666666666852, 0.2944444444444444531, 0.2972222222222222210, 0.2999999999999999889, 0.3027777777777777568, 0.3055555555555555802, 0.3083333333333333481, 0.3111111111111111160, 0.3138888888888888840, 0.3166666666666666519, 0.3194444444444444198, 0.3222222222222222432, 0.3250000000000000111, 0.3277777777777777790, 0.3305555555555555469, 0.3333333333333333148, 0.3361111111111111382, 0.3388888888888889062, 0.3416666666666666741, 0.3444444444444444420, 0.3472222222222222099, 0.3499999999999999778, 0.3527777777777778012, 0.3555555555555555691, 0.3583333333333333370, 0.3611111111111111049, 0.3638888888888888729, 0.3666666666666666408, 0.3694444444444444642, 0.3722222222222222321, 0.3750000000000000000, 0.3777777777777777679, 0.3805555555555555358, 0.3833333333333333592, 0.3861111111111111271, 0.3888888888888888951, 0.3916666666666666630, 0.3944444444444444309, 0.3972222222222221988, 0.4000000000000000222, 0.4027777777777777901, 0.4055555555555555580, 0.4083333333333333259, 0.4111111111111110938, 0.4138888888888888618, 0.4166666666666666852, 0.4194444444444444531, 0.4222222222222222210, 0.4249999999999999889, 0.4277777777777777568, 0.4305555555555555802, 0.4333333333333333481, 0.4361111111111111160, 0.4388888888888888840, 0.4416666666666666519, 0.4444444444444444198, 0.4472222222222222432, 0.4500000000000000111, 0.4527777777777777790, 0.4555555555555555469, 0.4583333333333333148, 0.4611111111111111382, 0.4638888888888889062, 0.4666666666666666741, 0.4694444444444444420, 0.4722222222222222099, 0.4749999999999999778, 0.4777777777777778012, 0.4805555555555555691, 0.4833333333333333370, 0.4861111111111111049, 0.4888888888888888729, 0.4916666666666666408, 0.4944444444444444642, 0.4972222222222222321, 0.5000000000000000000, 0.5027777777777777679, 0.5055555555555555358, 0.5083333333333333037, 0.5111111111111110716, 0.5138888888888888395, 0.5166666666666667185, 0.5194444444444444864, 0.5222222222222222543, 0.5250000000000000222, 0.5277777777777777901, 0.5305555555555555580, 0.5333333333333333259, 0.5361111111111110938, 0.5388888888888888618, 0.5416666666666666297, 0.5444444444444443976, 0.5472222222222222765, 0.5500000000000000444, 0.5527777777777778123, 0.5555555555555555802, 0.5583333333333333481, 0.5611111111111111160, 0.5638888888888888840, 0.5666666666666666519, 0.5694444444444444198, 0.5722222222222221877, 0.5749999999999999556, 0.5777777777777777235, 0.5805555555555556024, 0.5833333333333333703, 0.5861111111111111382, 0.5888888888888889062, 0.5916666666666666741, 0.5944444444444444420, 0.5972222222222222099, 0.5999999999999999778, 0.6027777777777777457, 0.6055555555555555136, 0.6083333333333332815, 0.6111111111111111605, 0.6138888888888889284, 0.6166666666666666963, 0.6194444444444444642, 0.6222222222222222321, 0.6250000000000000000, 0.6277777777777777679, 0.6305555555555555358, 0.6333333333333333037, 0.6361111111111110716, 0.6388888888888888395, 0.6416666666666667185, 0.6444444444444444864, 0.6472222222222222543, 0.6500000000000000222, 0.6527777777777777901, 0.6555555555555555580, 0.6583333333333333259, 0.6611111111111110938, 0.6638888888888888618, 0.6666666666666666297, 0.6694444444444443976, 0.6722222222222222765, 0.6750000000000000444, 0.6777777777777778123, 0.6805555555555555802, 0.6833333333333333481, 0.6861111111111111160, 0.6888888888888888840, 0.6916666666666666519, 0.6944444444444444198, 0.6972222222222221877, 0.6999999999999999556, 0.7027777777777777235, 0.7055555555555556024, 0.7083333333333333703, 0.7111111111111111382, 0.7138888888888889062, 0.7166666666666666741, 0.7194444444444444420, 0.7222222222222222099, 0.7249999999999999778, 0.7277777777777777457, 0.7305555555555555136, 0.7333333333333332815, 0.7361111111111111605, 0.7388888888888889284, 0.7416666666666666963, 0.7444444444444444642, 0.7472222222222222321, 0.7500000000000000000, 0.7527777777777777679, 0.7555555555555555358, 0.7583333333333333037, 0.7611111111111110716, 0.7638888888888888395, 0.7666666666666667185, 0.7694444444444444864, 0.7722222222222222543, 0.7750000000000000222, 0.7777777777777777901, 0.7805555555555555580, 0.7833333333333333259, 0.7861111111111110938, 0.7888888888888888618, 0.7916666666666666297, 0.7944444444444443976, 0.7972222222222222765, 0.8000000000000000444, 0.8027777777777778123, 0.8055555555555555802, 0.8083333333333333481, 0.8111111111111111160, 0.8138888888888888840, 0.8166666666666666519, 0.8194444444444444198, 0.8222222222222221877, 0.8249999999999999556, 0.8277777777777777235, 0.8305555555555556024, 0.8333333333333333703, 0.8361111111111111382, 0.8388888888888889062, 0.8416666666666666741, 0.8444444444444444420, 0.8472222222222222099, 0.8499999999999999778, 0.8527777777777777457, 0.8555555555555555136, 0.8583333333333332815, 0.8611111111111111605, 0.8638888888888889284, 0.8666666666666666963, 0.8694444444444444642, 0.8722222222222222321, 0.8750000000000000000, 0.8777777777777777679, 0.8805555555555555358, 0.8833333333333333037, 0.8861111111111110716, 0.8888888888888888395, 0.8916666666666667185, 0.8944444444444444864, 0.8972222222222222543, 0.9000000000000000222, 0.9027777777777777901, 0.9055555555555555580, 0.9083333333333333259, 0.9111111111111110938, 0.9138888888888888618, 0.9166666666666666297, 0.9194444444444443976, 0.9222222222222222765, 0.9250000000000000444, 0.9277777777777778123, 0.9305555555555555802, 0.9333333333333333481, 0.9361111111111111160, 0.9388888888888888840, 0.9416666666666666519, 0.9444444444444444198, 0.9472222222222221877, 0.9499999999999999556, 0.9527777777777777235, 0.9555555555555556024, 0.9583333333333333703, 0.9611111111111111382, 0.9638888888888889062, 0.9666666666666666741, 0.9694444444444444420, 0.9722222222222222099, 0.9749999999999999778 ),
 .UNSPECIFIED. ) 
 GEOMETRIC_REPRESENTATION_ITEM ( )  RATIONAL_B_SPLINE_SURFACE ( (
 ( 1.000000000000000000, 0.9659258262890683122, 1.000000000000000000, 0.9659258262890683122, 1.000000000000000000, 0.9659258262890683122, 1.000000000000000000, 0.9659258262890683122, 1.000000000000000000, 0.9659258262890683122, 1.000000000000000000, 0.9659258262890683122, 1.000000000000000000, 0.9659258262890683122, 1.000000000000000000, 0.9659258262890683122, 1.000000000000000000, 0.9659258262890683122, 1.000000000000000000, 0.9659258262890683122, 1.000000000000000000, 0.9659258262890683122, 1.000000000000000000, 0.9659258262890683122, 1.000000000000000000, 0.9659258262890683122, 1.000000000000000000, 0.9659258262890683122, 1.000000000000000000, 0.9659258262890683122, 1.000000000000000000, 0.9659258262890683122, 1.000000000000000000, 0.9659258262890683122, 1.000000000000000000, 0.9659258262890683122, 1.000000000000000000, 0.9659258262890683122, 1.000000000000000000, 0.9659258262890683122, 1.000000000000000000, 0.9659258262890683122, 1.000000000000000000, 0.9659258262890683122, 1.000000000000000000, 0.9659258262890683122, 1.000000000000000000, 0.9659258262890683122, 1.000000000000000000, 0.9659258262890683122, 1.000000000000000000, 0.9659258262890683122, 1.000000000000000000, 0.9659258262890683122, 1.000000000000000000, 0.9659258262890683122, 1.000000000000000000, 0.9659258262890683122, 1.000000000000000000, 0.9659258262890683122, 1.000000000000000000, 0.9659258262890683122, 1.000000000000000000, 0.9659258262890683122, 1.000000000000000000, 0.9659258262890683122, 1.000000000000000000, 0.9659258262890683122, 1.000000000000000000, 0.9659258262890683122, 1.000000000000000000, 0.9659258262890683122, 1.000000000000000000, 0.9659258262890683122, 1.000000000000000000, 0.9659258262890683122, 1.000000000000000000, 0.9659258262890683122, 1.000000000000000000, 0.9659258262890683122, 1.000000000000000000, 0.9659258262890683122, 1.000000000000000000, 0.9659258262890683122, 1.000000000000000000, 0.9659258262890683122, 1.000000000000000000, 0.9659258262890683122, 1.000000000000000000, 0.9659258262890683122, 1.000000000000000000, 0.9659258262890683122, 1.000000000000000000, 0.9659258262890683122, 1.000000000000000000, 0.9659258262890683122, 1.000000000000000000, 0.9659258262890683122, 1.000000000000000000, 0.9659258262890683122, 1.000000000000000000, 0.9659258262890683122, 1.000000000000000000, 0.9659258262890683122, 1.000000000000000000, 0.9659258262890683122, 1.000000000000000000, 0.9659258262890683122, 1.000000000000000000, 0.9659258262890683122, 1.000000000000000000, 0.9659258262890683122, 1.000000000000000000, 0.9659258262890683122, 1.000000000000000000, 0.9659258262890683122, 1.000000000000000000, 0.9659258262890683122, 1.000000000000000000, 0.9659258262890683122, 1.000000000000000000, 0.9659258262890683122, 1.000000000000000000, 0.9659258262890683122, 1.000000000000000000, 0.9659258262890683122, 1.000000000000000000, 0.9659258262890683122, 1.000000000000000000, 0.9659258262890683122, 1.000000000000000000, 0.9659258262890683122, 1.000000000000000000, 0.9659258262890683122, 1.000000000000000000, 0.9659258262890683122, 1.000000000000000000, 0.9659258262890683122, 1.000000000000000000, 0.9659258262890683122, 1.000000000000000000, 0.9659258262890683122, 1.000000000000000000, 0.9659258262890683122, 1.000000000000000000, 0.9659258262890683122, 1.000000000000000000, 0.9659258262890683122, 1.000000000000000000, 0.9659258262890683122, 1.000000000000000000, 0.9659258262890683122, 1.000000000000000000, 0.9659258262890683122, 1.000000000000000000, 0.9659258262890683122, 1.000000000000000000, 0.9659258262890683122, 1.000000000000000000, 0.9659258262890683122, 1.000000000000000000, 0.9659258262890683122, 1.000000000000000000, 0.9659258262890683122, 1.000000000000000000, 0.9659258262890683122, 1.000000000000000000, 0.9659258262890683122, 1.000000000000000000, 0.9659258262890683122, 1.000000000000000000, 0.9659258262890683122, 1.000000000000000000, 0.9659258262890683122, 1.000000000000000000, 0.9659258262890683122, 1.000000000000000000, 0.9659258262890683122, 1.000000000000000000, 0.9659258262890683122, 1.000000000000000000, 0.9659258262890683122, 1.000000000000000000, 0.9659258262890683122, 1.000000000000000000, 0.9659258262890683122, 1.000000000000000000, 0.9659258262890683122, 1.000000000000000000, 0.9659258262890683122, 1.000000000000000000, 0.9659258262890683122, 1.000000000000000000, 0.9659258262890683122, 1.000000000000000000, 0.9659258262890683122, 1.000000000000000000, 0.9659258262890683122, 1.000000000000000000, 0.9659258262890683122, 1.000000000000000000, 0.9659258262890683122, 1.000000000000000000, 0.9659258262890683122, 1.000000000000000000, 0.9659258262890683122, 1.000000000000000000, 0.9659258262890683122, 1.000000000000000000, 0.9659258262890683122, 1.000000000000000000, 0.9659258262890683122, 1.000000000000000000, 0.9659258262890683122, 1.000000000000000000, 0.9659258262890683122, 1.000000000000000000, 0.9659258262890683122, 1.000000000000000000, 0.9659258262890683122, 1.000000000000000000, 0.9659258262890683122, 1.000000000000000000, 0.9659258262890683122, 1.000000000000000000, 0.9659258262890683122, 1.000000000000000000, 0.9659258262890683122, 1.000000000000000000, 0.9659258262890683122, 1.000000000000000000, 0.9659258262890683122, 1.000000000000000000, 0.9659258262890683122, 1.000000000000000000, 0.9659258262890683122, 1.000000000000000000, 0.9659258262890683122, 1.000000000000000000, 0.9659258262890683122, 1.000000000000000000, 0.9659258262890683122, 1.000000000000000000, 0.9659258262890683122, 1.000000000000000000, 0.9659258262890683122, 1.000000000000000000, 0.9659258262890683122, 1.000000000000000000, 0.9659258262890683122, 1.000000000000000000, 0.9659258262890683122, 1.000000000000000000, 0.9659258262890683122, 1.000000000000000000, 0.9659258262890683122, 1.000000000000000000, 0.9659258262890683122, 1.000000000000000000, 0.9659258262890683122, 1.000000000000000000, 0.9659258262890683122, 1.000000000000000000, 0.9659258262890683122, 1.000000000000000000, 0.9659258262890683122, 1.000000000000000000, 0.9659258262890683122, 1.000000000000000000, 0.9659258262890683122, 1.000000000000000000, 0.9659258262890683122, 1.000000000000000000, 0.9659258262890683122, 1.000000000000000000, 0.9659258262890683122, 1.000000000000000000, 0.9659258262890683122, 1.000000000000000000, 0.9659258262890683122, 1.000000000000000000, 0.9659258262890683122, 1.000000000000000000, 0.9659258262890683122, 1.000000000000000000, 0.9659258262890683122, 1.000000000000000000, 0.9659258262890683122, 1.000000000000000000, 0.9659258262890683122, 1.000000000000000000, 0.9659258262890683122, 1.000000000000000000, 0.9659258262890683122, 1.000000000000000000, 0.9659258262890683122, 1.000000000000000000, 0.9659258262890683122, 1.000000000000000000, 0.9659258262890683122, 1.000000000000000000, 0.9659258262890683122, 1.000000000000000000, 0.9659258262890683122, 1.000000000000000000, 0.9659258262890683122, 1.000000000000000000, 0.9659258262890683122, 1.000000000000000000, 0.9659258262890683122, 1.000000000000000000, 0.9659258262890683122, 1.000000000000000000, 0.9659258262890683122, 1.000000000000000000, 0.9659258262890683122, 1.000000000000000000, 0.9659258262890683122, 1.000000000000000000, 0.9659258262890683122, 1.000000000000000000, 0.9659258262890683122, 1.000000000000000000, 0.9659258262890683122, 1.000000000000000000, 0.9659258262890683122, 1.000000000000000000, 0.9659258262890683122, 1.000000000000000000, 0.9659258262890683122, 1.000000000000000000, 0.9659258262890683122, 1.000000000000000000, 0.9659258262890683122, 1.000000000000000000, 0.9659258262890683122, 1.000000000000000000, 0.9659258262890683122, 1.000000000000000000, 0.9659258262890683122, 1.000000000000000000, 0.9659258262890683122, 1.000000000000000000, 0.9659258262890683122, 1.000000000000000000, 0.9659258262890683122, 1.000000000000000000, 0.9659258262890683122, 1.000000000000000000, 0.9659258262890683122, 1.000000000000000000, 0.9659258262890683122, 1.000000000000000000, 0.9659258262890683122, 1.000000000000000000, 0.9659258262890683122, 1.000000000000000000, 0.9659258262890683122, 1.000000000000000000, 0.9659258262890683122, 1.000000000000000000, 0.9659258262890683122, 1.000000000000000000, 0.9659258262890683122, 1.000000000000000000, 0.9659258262890683122, 1.000000000000000000, 0.9659258262890683122, 1.000000000000000000, 0.9659258262890683122, 1.000000000000000000, 0.9659258262890683122, 1.000000000000000000, 0.9659258262890683122, 1.000000000000000000, 0.9659258262890683122, 1.000000000000000000, 0.9659258262890683122, 1.000000000000000000, 0.9659258262890683122, 1.000000000000000000, 0.9659258262890683122, 1.000000000000000000, 0.9659258262890683122, 1.000000000000000000, 0.9659258262890683122, 1.000000000000000000, 0.9659258262890683122, 1.000000000000000000, 0.9659258262890683122, 1.000000000000000000, 0.9659258262890683122, 1.000000000000000000, 0.9659258262890683122, 1.000000000000000000, 0.9659258262890683122, 1.000000000000000000, 0.9659258262890683122, 1.000000000000000000, 0.9659258262890683122, 1.000000000000000000, 0.9659258262890683122, 1.000000000000000000, 0.9659258262890683122, 1.000000000000000000, 0.9659258262890683122, 1.000000000000000000, 0.9659258262890683122, 1.000000000000000000, 0.9659258262890683122, 1.000000000000000000, 0.9659258262890683122, 1.000000000000000000, 0.9659258262890683122, 1.000000000000000000, 0.9659258262890683122, 1.000000000000000000, 0.9659258262890683122, 1.000000000000000000, 0.9659258262890683122, 1.000000000000000000, 0.9659258262890683122, 1.000000000000000000, 0.9659258262890683122, 1.000000000000000000, 0.9659258262890683122, 1.000000000000000000, 0.9659258262890683122, 1.000000000000000000, 0.9659258262890683122, 1.000000000000000000, 0.9659258262890683122, 1.000000000000000000, 0.9659258262890683122, 1.000000000000000000, 0.9659258262890683122, 1.000000000000000000, 0.9659258262890683122, 1.000000000000000000, 0.9659258262890683122, 1.000000000000000000, 0.9659258262890683122, 1.000000000000000000, 0.9659258262890683122, 1.000000000000000000, 0.9659258262890683122, 1.000000000000000000, 0.9659258262890683122, 1.000000000000000000, 0.9659258262890683122, 1.000000000000000000, 0.9659258262890683122, 1.000000000000000000, 0.9659258262890683122, 1.000000000000000000, 0.9659258262890683122, 1.000000000000000000, 0.9659258262890683122, 1.000000000000000000, 0.9659258262890683122, 1.000000000000000000, 0.9659258262890683122, 1.000000000000000000, 0.9659258262890683122, 1.000000000000000000, 0.9659258262890683122, 1.000000000000000000, 0.9659258262890683122, 1.000000000000000000, 0.9659258262890683122, 1.000000000000000000, 0.9659258262890683122, 1.000000000000000000, 0.9659258262890683122, 1.000000000000000000, 0.9659258262890683122, 1.000000000000000000, 0.9659258262890683122, 1.000000000000000000, 0.9659258262890683122, 1.000000000000000000, 0.9659258262890683122, 1.000000000000000000, 0.9659258262890683122, 1.000000000000000000, 0.9659258262890683122, 1.000000000000000000, 0.9659258262890683122, 1.000000000000000000, 0.9659258262890683122, 1.000000000000000000, 0.9659258262890683122, 1.000000000000000000, 0.9659258262890683122, 1.000000000000000000, 0.9659258262890683122, 1.000000000000000000, 0.9659258262890683122, 1.000000000000000000, 0.9659258262890683122, 1.000000000000000000, 0.9659258262890683122, 1.000000000000000000, 0.9659258262890683122, 1.000000000000000000, 0.9659258262890683122, 1.000000000000000000, 0.9659258262890683122, 1.000000000000000000, 0.9659258262890683122, 1.000000000000000000, 0.9659258262890683122, 1.000000000000000000, 0.9659258262890683122, 1.000000000000000000, 0.9659258262890683122, 1.000000000000000000, 0.9659258262890683122, 1.000000000000000000, 0.9659258262890683122, 1.000000000000000000, 0.9659258262890683122, 1.000000000000000000, 0.9659258262890683122, 1.000000000000000000, 0.9659258262890683122, 1.000000000000000000, 0.9659258262890683122, 1.000000000000000000, 0.9659258262890683122, 1.000000000000000000, 0.9659258262890683122, 1.000000000000000000, 0.9659258262890683122, 1.000000000000000000, 0.9659258262890683122, 1.000000000000000000, 0.9659258262890683122, 1.000000000000000000, 0.9659258262890683122, 1.000000000000000000, 0.9659258262890683122, 1.000000000000000000, 0.9659258262890683122, 1.000000000000000000, 0.9659258262890683122, 1.000000000000000000, 0.9659258262890683122, 1.000000000000000000, 0.9659258262890683122, 1.000000000000000000, 0.9659258262890683122, 1.000000000000000000, 0.9659258262890683122, 1.000000000000000000, 0.9659258262890683122, 1.000000000000000000, 0.9659258262890683122, 1.000000000000000000, 0.9659258262890683122, 1.000000000000000000, 0.9659258262890683122, 1.000000000000000000, 0.9659258262890683122, 1.000000000000000000, 0.9659258262890683122, 1.000000000000000000, 0.9659258262890683122, 1.000000000000000000, 0.9659258262890683122, 1.000000000000000000, 0.9659258262890683122, 1.000000000000000000, 0.9659258262890683122, 1.000000000000000000, 0.9659258262890683122, 1.000000000000000000, 0.9659258262890683122, 1.000000000000000000, 0.9659258262890683122, 1.000000000000000000, 0.9659258262890683122, 1.000000000000000000, 0.9659258262890683122, 1.000000000000000000, 0.9659258262890683122, 1.000000000000000000, 0.9659258262890683122, 1.000000000000000000, 0.9659258262890683122, 1.000000000000000000, 0.9659258262890683122, 1.000000000000000000, 0.9659258262890683122, 1.000000000000000000, 0.9659258262890683122, 1.000000000000000000, 0.9659258262890683122, 1.000000000000000000, 0.9659258262890683122, 1.000000000000000000, 0.9659258262890683122, 1.000000000000000000, 0.9659258262890683122, 1.000000000000000000, 0.9659258262890683122, 1.000000000000000000, 0.9659258262890683122, 1.000000000000000000, 0.9659258262890683122, 1.000000000000000000, 0.9659258262890683122, 1.000000000000000000, 0.9659258262890683122, 1.000000000000000000, 0.9659258262890683122, 1.000000000000000000, 0.9659258262890683122, 1.000000000000000000, 0.9659258262890683122, 1.000000000000000000, 0.9659258262890683122, 1.000000000000000000, 0.9659258262890683122, 1.000000000000000000, 0.9659258262890683122, 1.000000000000000000, 0.9659258262890683122, 1.000000000000000000, 0.9659258262890683122, 1.000000000000000000, 0.9659258262890683122, 1.000000000000000000, 0.9659258262890683122, 1.000000000000000000, 0.9659258262890683122, 1.000000000000000000, 0.9659258262890683122, 1.000000000000000000, 0.9659258262890683122, 1.000000000000000000, 0.9659258262890683122, 1.000000000000000000, 0.9659258262890683122, 1.000000000000000000, 0.9659258262890683122, 1.000000000000000000, 0.9659258262890683122, 1.000000000000000000, 0.9659258262890683122, 1.000000000000000000, 0.9659258262890683122, 1.000000000000000000, 0.9659258262890683122, 1.000000000000000000, 0.9659258262890683122, 1.000000000000000000, 0.9659258262890683122, 1.000000000000000000, 0.9659258262890683122, 1.000000000000000000, 0.9659258262890683122, 1.000000000000000000, 0.9659258262890683122, 1.000000000000000000, 0.9659258262890683122, 1.000000000000000000, 0.9659258262890683122, 1.000000000000000000, 0.9659258262890683122, 1.000000000000000000, 0.9659258262890683122, 1.000000000000000000, 0.9659258262890683122, 1.000000000000000000, 0.9659258262890683122, 1.000000000000000000, 0.9659258262890683122, 1.000000000000000000, 0.9659258262890683122, 1.000000000000000000, 0.9659258262890683122, 1.000000000000000000, 0.9659258262890683122, 1.000000000000000000, 0.9659258262890683122, 1.000000000000000000, 0.9659258262890683122, 1.000000000000000000, 0.9659258262890683122, 1.000000000000000000, 0.9659258262890683122, 1.000000000000000000, 0.9659258262890683122, 1.000000000000000000, 0.9659258262890683122, 1.000000000000000000, 0.9659258262890683122, 1.000000000000000000, 0.9659258262890683122, 1.000000000000000000, 0.9659258262890683122, 1.000000000000000000),
 ( 1.000000000000000000, 0.9659258262890683122, 1.000000000000000000, 0.9659258262890683122, 1.000000000000000000, 0.9659258262890683122, 1.000000000000000000, 0.9659258262890683122, 1.000000000000000000, 0.9659258262890683122, 1.000000000000000000, 0.9659258262890683122, 1.000000000000000000, 0.9659258262890683122, 1.000000000000000000, 0.9659258262890683122, 1.000000000000000000, 0.9659258262890683122, 1.000000000000000000, 0.9659258262890683122, 1.000000000000000000, 0.9659258262890683122, 1.000000000000000000, 0.9659258262890683122, 1.000000000000000000, 0.9659258262890683122, 1.000000000000000000, 0.9659258262890683122, 1.000000000000000000, 0.9659258262890683122, 1.000000000000000000, 0.9659258262890683122, 1.000000000000000000, 0.9659258262890683122, 1.000000000000000000, 0.9659258262890683122, 1.000000000000000000, 0.9659258262890683122, 1.000000000000000000, 0.9659258262890683122, 1.000000000000000000, 0.9659258262890683122, 1.000000000000000000, 0.9659258262890683122, 1.000000000000000000, 0.9659258262890683122, 1.000000000000000000, 0.9659258262890683122, 1.000000000000000000, 0.9659258262890683122, 1.000000000000000000, 0.9659258262890683122, 1.000000000000000000, 0.9659258262890683122, 1.000000000000000000, 0.9659258262890683122, 1.000000000000000000, 0.9659258262890683122, 1.000000000000000000, 0.9659258262890683122, 1.000000000000000000, 0.9659258262890683122, 1.000000000000000000, 0.9659258262890683122, 1.000000000000000000, 0.9659258262890683122, 1.000000000000000000, 0.9659258262890683122, 1.000000000000000000, 0.9659258262890683122, 1.000000000000000000, 0.9659258262890683122, 1.000000000000000000, 0.9659258262890683122, 1.000000000000000000, 0.9659258262890683122, 1.000000000000000000, 0.9659258262890683122, 1.000000000000000000, 0.9659258262890683122, 1.000000000000000000, 0.9659258262890683122, 1.000000000000000000, 0.9659258262890683122, 1.000000000000000000, 0.9659258262890683122, 1.000000000000000000, 0.9659258262890683122, 1.000000000000000000, 0.9659258262890683122, 1.000000000000000000, 0.9659258262890683122, 1.000000000000000000, 0.9659258262890683122, 1.000000000000000000, 0.9659258262890683122, 1.000000000000000000, 0.9659258262890683122, 1.000000000000000000, 0.9659258262890683122, 1.000000000000000000, 0.9659258262890683122, 1.000000000000000000, 0.9659258262890683122, 1.000000000000000000, 0.9659258262890683122, 1.000000000000000000, 0.9659258262890683122, 1.000000000000000000, 0.9659258262890683122, 1.000000000000000000, 0.9659258262890683122, 1.000000000000000000, 0.9659258262890683122, 1.000000000000000000, 0.9659258262890683122, 1.000000000000000000, 0.9659258262890683122, 1.000000000000000000, 0.9659258262890683122, 1.000000000000000000, 0.9659258262890683122, 1.000000000000000000, 0.9659258262890683122, 1.000000000000000000, 0.9659258262890683122, 1.000000000000000000, 0.9659258262890683122, 1.000000000000000000, 0.9659258262890683122, 1.000000000000000000, 0.9659258262890683122, 1.000000000000000000, 0.9659258262890683122, 1.000000000000000000, 0.9659258262890683122, 1.000000000000000000, 0.9659258262890683122, 1.000000000000000000, 0.9659258262890683122, 1.000000000000000000, 0.9659258262890683122, 1.000000000000000000, 0.9659258262890683122, 1.000000000000000000, 0.9659258262890683122, 1.000000000000000000, 0.9659258262890683122, 1.000000000000000000, 0.9659258262890683122, 1.000000000000000000, 0.9659258262890683122, 1.000000000000000000, 0.9659258262890683122, 1.000000000000000000, 0.9659258262890683122, 1.000000000000000000, 0.9659258262890683122, 1.000000000000000000, 0.9659258262890683122, 1.000000000000000000, 0.9659258262890683122, 1.000000000000000000, 0.9659258262890683122, 1.000000000000000000, 0.9659258262890683122, 1.000000000000000000, 0.9659258262890683122, 1.000000000000000000, 0.9659258262890683122, 1.000000000000000000, 0.9659258262890683122, 1.000000000000000000, 0.9659258262890683122, 1.000000000000000000, 0.9659258262890683122, 1.000000000000000000, 0.9659258262890683122, 1.000000000000000000, 0.9659258262890683122, 1.000000000000000000, 0.9659258262890683122, 1.000000000000000000, 0.9659258262890683122, 1.000000000000000000, 0.9659258262890683122, 1.000000000000000000, 0.9659258262890683122, 1.000000000000000000, 0.9659258262890683122, 1.000000000000000000, 0.9659258262890683122, 1.000000000000000000, 0.9659258262890683122, 1.000000000000000000, 0.9659258262890683122, 1.000000000000000000, 0.9659258262890683122, 1.000000000000000000, 0.9659258262890683122, 1.000000000000000000, 0.9659258262890683122, 1.000000000000000000, 0.9659258262890683122, 1.000000000000000000, 0.9659258262890683122, 1.000000000000000000, 0.9659258262890683122, 1.000000000000000000, 0.9659258262890683122, 1.000000000000000000, 0.9659258262890683122, 1.000000000000000000, 0.9659258262890683122, 1.000000000000000000, 0.9659258262890683122, 1.000000000000000000, 0.9659258262890683122, 1.000000000000000000, 0.9659258262890683122, 1.000000000000000000, 0.9659258262890683122, 1.000000000000000000, 0.9659258262890683122, 1.000000000000000000, 0.9659258262890683122, 1.000000000000000000, 0.9659258262890683122, 1.000000000000000000, 0.9659258262890683122, 1.000000000000000000, 0.9659258262890683122, 1.000000000000000000, 0.9659258262890683122, 1.000000000000000000, 0.9659258262890683122, 1.000000000000000000, 0.9659258262890683122, 1.000000000000000000, 0.9659258262890683122, 1.000000000000000000, 0.9659258262890683122, 1.000000000000000000, 0.9659258262890683122, 1.000000000000000000, 0.9659258262890683122, 1.000000000000000000, 0.9659258262890683122, 1.000000000000000000, 0.9659258262890683122, 1.000000000000000000, 0.9659258262890683122, 1.000000000000000000, 0.9659258262890683122, 1.000000000000000000, 0.9659258262890683122, 1.000000000000000000, 0.9659258262890683122, 1.000000000000000000, 0.9659258262890683122, 1.000000000000000000, 0.9659258262890683122, 1.000000000000000000, 0.9659258262890683122, 1.000000000000000000, 0.9659258262890683122, 1.000000000000000000, 0.9659258262890683122, 1.000000000000000000, 0.9659258262890683122, 1.000000000000000000, 0.9659258262890683122, 1.000000000000000000, 0.9659258262890683122, 1.000000000000000000, 0.9659258262890683122, 1.000000000000000000, 0.9659258262890683122, 1.000000000000000000, 0.9659258262890683122, 1.000000000000000000, 0.9659258262890683122, 1.000000000000000000, 0.9659258262890683122, 1.000000000000000000, 0.9659258262890683122, 1.000000000000000000, 0.9659258262890683122, 1.000000000000000000, 0.9659258262890683122, 1.000000000000000000, 0.9659258262890683122, 1.000000000000000000, 0.9659258262890683122, 1.000000000000000000, 0.9659258262890683122, 1.000000000000000000, 0.9659258262890683122, 1.000000000000000000, 0.9659258262890683122, 1.000000000000000000, 0.9659258262890683122, 1.000000000000000000, 0.9659258262890683122, 1.000000000000000000, 0.9659258262890683122, 1.000000000000000000, 0.9659258262890683122, 1.000000000000000000, 0.9659258262890683122, 1.000000000000000000, 0.9659258262890683122, 1.000000000000000000, 0.9659258262890683122, 1.000000000000000000, 0.9659258262890683122, 1.000000000000000000, 0.9659258262890683122, 1.000000000000000000, 0.9659258262890683122, 1.000000000000000000, 0.9659258262890683122, 1.000000000000000000, 0.9659258262890683122, 1.000000000000000000, 0.9659258262890683122, 1.000000000000000000, 0.9659258262890683122, 1.000000000000000000, 0.9659258262890683122, 1.000000000000000000, 0.9659258262890683122, 1.000000000000000000, 0.9659258262890683122, 1.000000000000000000, 0.9659258262890683122, 1.000000000000000000, 0.9659258262890683122, 1.000000000000000000, 0.9659258262890683122, 1.000000000000000000, 0.9659258262890683122, 1.000000000000000000, 0.9659258262890683122, 1.000000000000000000, 0.9659258262890683122, 1.000000000000000000, 0.9659258262890683122, 1.000000000000000000, 0.9659258262890683122, 1.000000000000000000, 0.9659258262890683122, 1.000000000000000000, 0.9659258262890683122, 1.000000000000000000, 0.9659258262890683122, 1.000000000000000000, 0.9659258262890683122, 1.000000000000000000, 0.9659258262890683122, 1.000000000000000000, 0.9659258262890683122, 1.000000000000000000, 0.9659258262890683122, 1.000000000000000000, 0.9659258262890683122, 1.000000000000000000, 0.9659258262890683122, 1.000000000000000000, 0.9659258262890683122, 1.000000000000000000, 0.9659258262890683122, 1.000000000000000000, 0.9659258262890683122, 1.000000000000000000, 0.9659258262890683122, 1.000000000000000000, 0.9659258262890683122, 1.000000000000000000, 0.9659258262890683122, 1.000000000000000000, 0.9659258262890683122, 1.000000000000000000, 0.9659258262890683122, 1.000000000000000000, 0.9659258262890683122, 1.000000000000000000, 0.9659258262890683122, 1.000000000000000000, 0.9659258262890683122, 1.000000000000000000, 0.9659258262890683122, 1.000000000000000000, 0.9659258262890683122, 1.000000000000000000, 0.9659258262890683122, 1.000000000000000000, 0.9659258262890683122, 1.000000000000000000, 0.9659258262890683122, 1.000000000000000000, 0.9659258262890683122, 1.000000000000000000, 0.9659258262890683122, 1.000000000000000000, 0.9659258262890683122, 1.000000000000000000, 0.9659258262890683122, 1.000000000000000000, 0.9659258262890683122, 1.000000000000000000, 0.9659258262890683122, 1.000000000000000000, 0.9659258262890683122, 1.000000000000000000, 0.9659258262890683122, 1.000000000000000000, 0.9659258262890683122, 1.000000000000000000, 0.9659258262890683122, 1.000000000000000000, 0.9659258262890683122, 1.000000000000000000, 0.9659258262890683122, 1.000000000000000000, 0.9659258262890683122, 1.000000000000000000, 0.9659258262890683122, 1.000000000000000000, 0.9659258262890683122, 1.000000000000000000, 0.9659258262890683122, 1.000000000000000000, 0.9659258262890683122, 1.000000000000000000, 0.9659258262890683122, 1.000000000000000000, 0.9659258262890683122, 1.000000000000000000, 0.9659258262890683122, 1.000000000000000000, 0.9659258262890683122, 1.000000000000000000, 0.9659258262890683122, 1.000000000000000000, 0.9659258262890683122, 1.000000000000000000, 0.9659258262890683122, 1.000000000000000000, 0.9659258262890683122, 1.000000000000000000, 0.9659258262890683122, 1.000000000000000000, 0.9659258262890683122, 1.000000000000000000, 0.9659258262890683122, 1.000000000000000000, 0.9659258262890683122, 1.000000000000000000, 0.9659258262890683122, 1.000000000000000000, 0.9659258262890683122, 1.000000000000000000, 0.9659258262890683122, 1.000000000000000000, 0.9659258262890683122, 1.000000000000000000, 0.9659258262890683122, 1.000000000000000000, 0.9659258262890683122, 1.000000000000000000, 0.9659258262890683122, 1.000000000000000000, 0.9659258262890683122, 1.000000000000000000, 0.9659258262890683122, 1.000000000000000000, 0.9659258262890683122, 1.000000000000000000, 0.9659258262890683122, 1.000000000000000000, 0.9659258262890683122, 1.000000000000000000, 0.9659258262890683122, 1.000000000000000000, 0.9659258262890683122, 1.000000000000000000, 0.9659258262890683122, 1.000000000000000000, 0.9659258262890683122, 1.000000000000000000, 0.9659258262890683122, 1.000000000000000000, 0.9659258262890683122, 1.000000000000000000, 0.9659258262890683122, 1.000000000000000000, 0.9659258262890683122, 1.000000000000000000, 0.9659258262890683122, 1.000000000000000000, 0.9659258262890683122, 1.000000000000000000, 0.9659258262890683122, 1.000000000000000000, 0.9659258262890683122, 1.000000000000000000, 0.9659258262890683122, 1.000000000000000000, 0.9659258262890683122, 1.000000000000000000, 0.9659258262890683122, 1.000000000000000000, 0.9659258262890683122, 1.000000000000000000, 0.9659258262890683122, 1.000000000000000000, 0.9659258262890683122, 1.000000000000000000, 0.9659258262890683122, 1.000000000000000000, 0.9659258262890683122, 1.000000000000000000, 0.9659258262890683122, 1.000000000000000000, 0.9659258262890683122, 1.000000000000000000, 0.9659258262890683122, 1.000000000000000000, 0.9659258262890683122, 1.000000000000000000, 0.9659258262890683122, 1.000000000000000000, 0.9659258262890683122, 1.000000000000000000, 0.9659258262890683122, 1.000000000000000000, 0.9659258262890683122, 1.000000000000000000, 0.9659258262890683122, 1.000000000000000000, 0.9659258262890683122, 1.000000000000000000, 0.9659258262890683122, 1.000000000000000000, 0.9659258262890683122, 1.000000000000000000, 0.9659258262890683122, 1.000000000000000000, 0.9659258262890683122, 1.000000000000000000, 0.9659258262890683122, 1.000000000000000000, 0.9659258262890683122, 1.000000000000000000, 0.9659258262890683122, 1.000000000000000000, 0.9659258262890683122, 1.000000000000000000, 0.9659258262890683122, 1.000000000000000000, 0.9659258262890683122, 1.000000000000000000, 0.9659258262890683122, 1.000000000000000000, 0.9659258262890683122, 1.000000000000000000, 0.9659258262890683122, 1.000000000000000000, 0.9659258262890683122, 1.000000000000000000, 0.9659258262890683122, 1.000000000000000000, 0.9659258262890683122, 1.000000000000000000, 0.9659258262890683122, 1.000000000000000000, 0.9659258262890683122, 1.000000000000000000, 0.9659258262890683122, 1.000000000000000000, 0.9659258262890683122, 1.000000000000000000, 0.9659258262890683122, 1.000000000000000000, 0.9659258262890683122, 1.000000000000000000, 0.9659258262890683122, 1.000000000000000000, 0.9659258262890683122, 1.000000000000000000, 0.9659258262890683122, 1.000000000000000000, 0.9659258262890683122, 1.000000000000000000, 0.9659258262890683122, 1.000000000000000000, 0.9659258262890683122, 1.000000000000000000, 0.9659258262890683122, 1.000000000000000000, 0.9659258262890683122, 1.000000000000000000, 0.9659258262890683122, 1.000000000000000000, 0.9659258262890683122, 1.000000000000000000, 0.9659258262890683122, 1.000000000000000000, 0.9659258262890683122, 1.000000000000000000, 0.9659258262890683122, 1.000000000000000000, 0.9659258262890683122, 1.000000000000000000, 0.9659258262890683122, 1.000000000000000000, 0.9659258262890683122, 1.000000000000000000, 0.9659258262890683122, 1.000000000000000000, 0.9659258262890683122, 1.000000000000000000, 0.9659258262890683122, 1.000000000000000000, 0.9659258262890683122, 1.000000000000000000, 0.9659258262890683122, 1.000000000000000000, 0.9659258262890683122, 1.000000000000000000, 0.9659258262890683122, 1.000000000000000000, 0.9659258262890683122, 1.000000000000000000, 0.9659258262890683122, 1.000000000000000000, 0.9659258262890683122, 1.000000000000000000, 0.9659258262890683122, 1.000000000000000000, 0.9659258262890683122, 1.000000000000000000, 0.9659258262890683122, 1.000000000000000000, 0.9659258262890683122, 1.000000000000000000, 0.9659258262890683122, 1.000000000000000000, 0.9659258262890683122, 1.000000000000000000, 0.9659258262890683122, 1.000000000000000000, 0.9659258262890683122, 1.000000000000000000, 0.9659258262890683122, 1.000000000000000000, 0.9659258262890683122, 1.000000000000000000, 0.9659258262890683122, 1.000000000000000000, 0.9659258262890683122, 1.000000000000000000, 0.9659258262890683122, 1.000000000000000000, 0.9659258262890683122, 1.000000000000000000, 0.9659258262890683122, 1.000000000000000000, 0.9659258262890683122, 1.000000000000000000, 0.9659258262890683122, 1.000000000000000000, 0.9659258262890683122, 1.000000000000000000, 0.9659258262890683122, 1.000000000000000000, 0.9659258262890683122, 1.000000000000000000, 0.9659258262890683122, 1.000000000000000000, 0.9659258262890683122, 1.000000000000000000, 0.9659258262890683122, 1.000000000000000000, 0.9659258262890683122, 1.000000000000000000, 0.9659258262890683122, 1.000000000000000000, 0.9659258262890683122, 1.000000000000000000, 0.9659258262890683122, 1.000000000000000000, 0.9659258262890683122, 1.000000000000000000, 0.9659258262890683122, 1.000000000000000000, 0.9659258262890683122, 1.000000000000000000, 0.9659258262890683122, 1.000000000000000000, 0.9659258262890683122, 1.000000000000000000) ) ) 
 REPRESENTATION_ITEM ( '' )  SURFACE ( )  );
#91916 = FACE_OUTER_BOUND ( 'NONE', #89733, .T. ) ;
#91917 = ORIENTED_EDGE ( 'NONE', *, *, #66006, .T. ) ;
#91918 = CARTESIAN_POINT ( 'NONE',  ( 19.89359858452208130, 4.202752102959690472E-16, 0.000000000000000000 ) ) ;
#91919 = FACE_OUTER_BOUND ( 'NONE', #115890, .T. ) ;
#91920 = VERTEX_POINT ( 'NONE', #122193 ) ;
#91921 = LINE ( 'NONE', #55754, #17938 ) ;
#91922 = ORIENTED_EDGE ( 'NONE', *, *, #73753, .T. ) ;
#91923 = ORIENTED_EDGE ( 'NONE', *, *, #70723, .F. ) ;
#91924 = DIRECTION ( 'NONE',  ( -0.7071067811865486830, -0.7071067811865464625, 0.000000000000000000 ) ) ;
#91925 = ORIENTED_EDGE ( 'NONE', *, *, #96843, .F. ) ;
#91926 = ORIENTED_EDGE ( 'NONE', *, *, #91433, .F. ) ;
#91927 = DIRECTION ( 'NONE',  ( 0.7071067811865487940, 0.7071067811865463515, -0.000000000000000000 ) ) ;
#91928 = ORIENTED_EDGE ( 'NONE', *, *, #5336, .T. ) ;
#91929 = CARTESIAN_POINT ( 'NONE',  ( 23.99999999999983302, -0.1606350220012988939, 4.664761815935144718 ) ) ;
#91930 = EDGE_CURVE ( 'NONE', #71270, #83728, #3273, .T. ) ;
#91931 = FACE_OUTER_BOUND ( 'NONE', #82947, .T. ) ;
#91932 = MECHANICAL_DESIGN_GEOMETRIC_PRESENTATION_REPRESENTATION (  '', ( #3930 ), #142954 ) ;
#91933 = CARTESIAN_POINT ( 'NONE',  ( 122.2087635252314328, -7.482591942790329030E-16, 6.110000000000001208 ) ) ;
#91934 = DIRECTION ( 'NONE',  ( -0.6830127018922180770, -0.6830127018922204085, -0.2588190451025213501 ) ) ;
#91935 = EDGE_CURVE ( 'NONE', #85852, #3387, #90291, .T. ) ;
#91936 = DIRECTION ( 'NONE',  ( -0.6830127018922181881, 0.6830127018922202975, -0.2588190451025214056 ) ) ;
#91937 = CARTESIAN_POINT ( 'NONE',  ( 51.48921356237309510, -27.52281430457091460, 5.000000000000000000 ) ) ;
#91938 = DIRECTION ( 'NONE',  ( -0.7071067811865486830, -0.7071067811865464625, 0.000000000000000000 ) ) ;
#91939 = FACE_OUTER_BOUND ( 'NONE', #44661, .T. ) ;
#91940 = EDGE_CURVE ( 'NONE', #97576, #23170, #133811, .T. ) ;
#91941 = EDGE_CURVE ( 'NONE', #74437, #6107, #123676, .T. ) ;
#91942 = CARTESIAN_POINT ( 'NONE',  ( 8.968407645496675684, -1.925929944387235853E-31, 2.500000000000001332 ) ) ;
#91943 = DIRECTION ( 'NONE',  ( -0.3543493200069163240, 0.000000000000000000, -0.9351131265310288487 ) ) ;
#91944 = ORIENTED_EDGE ( 'NONE', *, *, #41276, .F. ) ;
#91945 = DIRECTION ( 'NONE',  ( -1.000000000000000000, -1.224606353822377258E-16, -0.000000000000000000 ) ) ;
#91946 = DIRECTION ( 'NONE',  ( 0.6830127018922180770, -0.6830127018922204085, -0.2588190451025213501 ) ) ;
#91947 = ORIENTED_EDGE ( 'NONE', *, *, #82014, .T. ) ;
#91948 = VERTEX_POINT ( 'NONE', #100479 ) ;
#91949 = LINE ( 'NONE', #58681, #63463 ) ;
#91950 = ORIENTED_EDGE ( 'NONE', *, *, #73588, .F. ) ;
#91951 = LINE ( 'NONE', #60807, #113911 ) ;
#91952 = CARTESIAN_POINT ( 'NONE',  ( 113.4374999999999858, 5.819803920172574863, -5.819803920172573086 ) ) ;
#91953 = CARTESIAN_POINT ( 'NONE',  ( -14.99999999999989519, 14.87792677143807651, -11.06722581663443350 ) ) ;
#91954 = COLOUR_RGB ( '', 0.09019608, 0.27058824, 0.51372549) ;
#91955 = EDGE_CURVE ( 'NONE', #96580, #1511, #80873, .T. ) ;
#91956 = CARTESIAN_POINT ( 'NONE',  ( 19.05000000000000071, 3.174999999999997158, 4.000000000000000000 ) ) ;
#91957 = EDGE_CURVE ( 'NONE', #26241, #89121, #33801, .T. ) ;
#91958 = DIRECTION ( 'NONE',  ( -0.7071067811865487940, 0.7071067811865463515, -0.000000000000000000 ) ) ;
#91959 = ORIENTED_EDGE ( 'NONE', *, *, #34004, .F. ) ;
#91960 = LINE ( 'NONE', #115820, #51154 ) ;
#91961 = ORIENTED_EDGE ( 'NONE', *, *, #25164, .F. ) ;
#91962 = AXIS2_PLACEMENT_3D ( 'NONE', #103992, #6093, #137384 ) ;
#91964 = DIRECTION ( 'NONE',  ( -0.7071067811865487940, 0.7071067811865463515, -0.000000000000000000 ) ) ;
#91963 = VECTOR ( 'NONE', #106874, 1000.000000000000227 ) ;
#91965 = AXIS2_PLACEMENT_3D ( 'NONE', #106643, #7333, #51597 ) ;
#91966 = CARTESIAN_POINT ( 'NONE',  ( 28.21290314143522338, 3.967499999999992699, -6.871911579029513994 ) ) ;
#91967 = EDGE_CURVE ( 'NONE', #54589, #19758, #101888, .T. ) ;
#91968 = CARTESIAN_POINT ( 'NONE',  ( -9.489213562373095101, -27.52281430457062328, 5.000000000000000000 ) ) ;
#91969 = CARTESIAN_POINT ( 'NONE',  ( -24.29974487139158867, -27.71228299555223273, 4.000000000000000000 ) ) ;
#91970 = ORIENTED_EDGE ( 'NONE', *, *, #16156, .F. ) ;
#91971 = ORIENTED_EDGE ( 'NONE', *, *, #133253, .T. ) ;
#91972 = ORIENTED_EDGE ( 'NONE', *, *, #141252, .F. ) ;
#91973 = LINE ( 'NONE', #123919, #5575 ) ;
#91974 = LINE ( 'NONE', #38323, #90393 ) ;
#91975 = VECTOR ( 'NONE', #90272, 1000.000000000000000 ) ;
#91976 = EDGE_CURVE ( 'NONE', #98989, #59733, #1127, .T. ) ;
#91977 = LINE ( 'NONE', #136194, #114531 ) ;
#91978 = LINE ( 'NONE', #126728, #98293 ) ;
#91979 = ORIENTED_EDGE ( 'NONE', *, *, #16269, .F. ) ;
#91980 = DIRECTION ( 'NONE',  ( 0.7071067811865487940, -0.7071067811865463515, 0.000000000000000000 ) ) ;
#91981 = FACE_OUTER_BOUND ( 'NONE', #140043, .T. ) ;
#91982 = DIRECTION ( 'NONE',  ( -0.7071067811865486830, -0.7071067811865464625, -0.000000000000000000 ) ) ;
#91983 = DIRECTION ( 'NONE',  ( 0.7071067811865487940, 0.7071067811865463515, -0.000000000000000000 ) ) ;
#91984 = ORIENTED_EDGE ( 'NONE', *, *, #103513, .F. ) ;
#91985 = EDGE_CURVE ( 'NONE', #23205, #131546, #14156, .T. ) ;
#91986 = CARTESIAN_POINT ( 'NONE',  ( -32.99451991528749062, 28.92564299267960948, 4.000000000000000000 ) ) ;
#91987 = VERTEX_POINT ( 'NONE', #80169 ) ;
#91989 = VERTEX_POINT ( 'NONE', #124359 ) ;
#91988 = PRESENTATION_STYLE_ASSIGNMENT (( #34777 ) ) ;
#91990 = EDGE_LOOP ( 'NONE', ( #13379, #72993, #108945, #97628 ) ) ;
#91991 = EDGE_CURVE ( 'NONE', #54699, #16019, #142865, .T. ) ;
#91992 = DIRECTION ( 'NONE',  ( -0.7071067811865486830, 0.7071067811865464625, 0.000000000000000000 ) ) ;
#91994 = EDGE_CURVE ( 'NONE', #25602, #20468, #58446, .T. ) ;
#91993 = VECTOR ( 'NONE', #46734, 1000.000000000000227 ) ;
#91995 = ORIENTED_EDGE ( 'NONE', *, *, #116883, .F. ) ;
#91996 = CARTESIAN_POINT ( 'NONE',  ( -5.999999999999946709, -19.44781430457062754, 5.000000000000000000 ) ) ;
#91997 = FACE_OUTER_BOUND ( 'NONE', #38895, .T. ) ;
#91998 = DIRECTION ( 'NONE',  ( -0.000000000000000000, 0.3543493200069153248, 0.9351131265310292928 ) ) ;
#91999 = ADVANCED_FACE ( 'NONE', ( #139554 ), #25753, .T. ) ;
#92000 = CARTESIAN_POINT ( 'NONE',  ( 26.74543019189810877, -5.291415217122919401, -3.055000000000000604 ) ) ;
#92001 = VECTOR ( 'NONE', #86831, 1000.000000000000000 ) ;
#92002 = FACE_OUTER_BOUND ( 'NONE', #73492, .T. ) ;
#92003 = CARTESIAN_POINT ( 'NONE',  ( 48.35002705046287730, -5.819803920172573086, -5.819803920172573086 ) ) ;
#92004 = CARTESIAN_POINT ( 'NONE',  ( 25.39999999999999858, 7.464222240803104598E-16, -6.094999999999989093 ) ) ;
#92005 = DIRECTION ( 'NONE',  ( -0.7071067811865487940, 0.7071067811865463515, 0.000000000000000000 ) ) ;
#92006 = CARTESIAN_POINT ( 'NONE',  ( -33.18398860626899705, 28.73617430169810305, 5.000000000000000000 ) ) ;
#92007 = LINE ( 'NONE', #56589, #39131 ) ;
#92008 = CARTESIAN_POINT ( 'NONE',  ( 30.74956980810188867, 3.967499999999998916, 6.871911579029510442 ) ) ;
#92010 = VECTOR ( 'NONE', #30928, 1000.000000000000227 ) ;
#92009 = CARTESIAN_POINT ( 'NONE',  ( 0.2890851266676670583, -7.934999999999988951, 1.853802869168066358 ) ) ;
#92011 = CARTESIAN_POINT ( 'NONE',  ( 26.99999999999981881, -4.447814304570781196, 5.000000000000000000 ) ) ;
#92012 = CARTESIAN_POINT ( 'NONE',  ( 5.999999999999958256, 15.45873954670186201, -0.03131636524295391966 ) ) ;
#92013 = CARTESIAN_POINT ( 'NONE',  ( 29.29289321881325137, 5.259292476615669010, 5.000000000000000000 ) ) ;
#92014 = VERTEX_POINT ( 'NONE', #5404 ) ;
#92015 = ORIENTED_EDGE ( 'NONE', *, *, #55572, .F. ) ;
#92016 = CARTESIAN_POINT ( 'NONE',  ( 91.85416666666668561, -2.130196079827425315, -7.950000000000001066 ) ) ;
#92017 = VERTEX_POINT ( 'NONE', #93157 ) ;
#92018 = VERTEX_POINT ( 'NONE', #70021 ) ;
#92019 = AXIS2_PLACEMENT_3D ( 'NONE', #74024, #131255, #109500 ) ;
#92020 = DIRECTION ( 'NONE',  ( 0.000000000000000000, -2.921639538487157626E-15, 1.000000000000000000 ) ) ;
#92021 = DIRECTION ( 'NONE',  ( 0.7071067811865487940, -0.7071067811865463515, 0.000000000000000000 ) ) ;
#92022 = CARTESIAN_POINT ( 'NONE',  ( -23.29289321881329755, -12.74070752338414891, 5.000000000000000000 ) ) ;
#92023 = ORIENTED_EDGE ( 'NONE', *, *, #4292, .F. ) ;
#92024 = CARTESIAN_POINT ( 'NONE',  ( 0.000000000000000000, 0.000000000000000000, 5.000000000000000000 ) ) ;
#92025 = DIRECTION ( 'NONE',  ( 0.000000000000000000, 1.137193330093851361E-16, -1.000000000000000000 ) ) ;
#92026 = DIRECTION ( 'NONE',  ( -0.6830127018922181881, 0.6830127018922202975, -0.2588190451025214056 ) ) ;
#92027 = CARTESIAN_POINT ( 'NONE',  ( 126.8792446338207753, 3.521890969138218086, 5.552962617327368733 ) ) ;
#92028 = FACE_OUTER_BOUND ( 'NONE', #42457, .T. ) ;
#92029 = LINE ( 'NONE', #60889, #102935 ) ;
#92030 = DIRECTION ( 'NONE',  ( 0.7071067811865487940, 0.7071067811865463515, 0.000000000000000000 ) ) ;
#92031 = LINE ( 'NONE', #136254, #130325 ) ;
#92032 = LINE ( 'NONE', #67474, #100981 ) ;
#92033 = LINE ( 'NONE', #136257, #98497 ) ;
#92034 = SURFACE_STYLE_FILL_AREA ( #126795 ) ;
#92035 = ORIENTED_EDGE ( 'NONE', *, *, #65172, .F. ) ;
#92036 = ORIENTED_EDGE ( 'NONE', *, *, #107060, .F. ) ;
#92037 = CARTESIAN_POINT ( 'NONE',  ( 115.2087635252314470, -7.482591942790329030E-16, 6.110000000000001208 ) ) ;
#92038 = AXIS2_PLACEMENT_3D ( 'NONE', #27534, #114552, #137764 ) ;
#92039 = ORIENTED_EDGE ( 'NONE', *, *, #17750, .F. ) ;
#92040 = PLANE ( 'NONE',  #121899 ) ;
#92041 = CARTESIAN_POINT ( 'NONE',  ( -4.983273985306034929E-14, -39.92999999999999261, -40.00000000000000000 ) ) ;
#92042 = ORIENTED_EDGE ( 'NONE', *, *, #26546, .F. ) ;
#92043 = CARTESIAN_POINT ( 'NONE',  ( 28.49999999999980815, -17.56887692260762535, 4.000000000000000000 ) ) ;
#92044 = DIRECTION ( 'NONE',  ( -1.000000000000000000, -0.000000000000000000, -0.000000000000000000 ) ) ;
#92045 = CARTESIAN_POINT ( 'NONE',  ( 104.6204301918981230, 3.055000000000001936, -5.291415217122916737 ) ) ;
#92046 = EDGE_LOOP ( 'NONE', ( #127595, #20806, #126024, #74223 ) ) ;
#92047 = VERTEX_POINT ( 'NONE', #95290 ) ;
#92048 = LINE ( 'NONE', #26105, #107849 ) ;
#92049 = CARTESIAN_POINT ( 'NONE',  ( 0.000000000000000000, 0.000000000000000000, 5.000000000000000000 ) ) ;
#92050 = VECTOR ( 'NONE', #121543, 1000.000000000000000 ) ;
#92051 = EDGE_LOOP ( 'NONE', ( #47736, #141256, #20216 ) ) ;
#92052 = ORIENTED_EDGE ( 'NONE', *, *, #84429, .T. ) ;
#92053 = VECTOR ( 'NONE', #111328, 1000.000000000000227 ) ;
#92054 = EDGE_CURVE ( 'NONE', #73062, #23978, #50376, .T. ) ;
#92055 = ORIENTED_EDGE ( 'NONE', *, *, #139906, .F. ) ;
#92056 = DIRECTION ( 'NONE',  ( -0.000000000000000000, -0.3543493200069152693, 0.9351131265310292928 ) ) ;
#92057 = APPLICATION_CONTEXT ( 'automotive_design' ) ;
#92058 = ADVANCED_FACE ( 'NONE', ( #126481 ), #117040, .F. ) ;
#92059 =( LENGTH_UNIT ( ) NAMED_UNIT ( * ) SI_UNIT ( .MILLI., .METRE. ) );
#92060 = AXIS2_PLACEMENT_3D ( 'NONE', #108733, #29764, #41359 ) ;
#92061 = TOROIDAL_SURFACE ( 'NONE', #68926, 9.000000000000001776, 3.000000000000000000 ) ;
#92062 = DIRECTION ( 'NONE',  ( 0.000000000000000000, -1.000000000000000000, 0.000000000000000000 ) ) ;
#92063 = EDGE_LOOP ( 'NONE', ( #74462, #65158, #64251, #55328 ) ) ;
#92065 = VERTEX_POINT ( 'NONE', #51096 ) ;
#92064 = EDGE_CURVE ( 'NONE', #124621, #36267, #84914, .T. ) ;
#92066 = CARTESIAN_POINT ( 'NONE',  ( 5.999999999999965361, -9.033600742197647193, 5.000000000000000000 ) ) ;
#92067 = ORIENTED_EDGE ( 'NONE', *, *, #8309, .T. ) ;
#92068 = ORIENTED_EDGE ( 'NONE', *, *, #50166, .T. ) ;
#92069 = LINE ( 'NONE', #124714, #139712 ) ;
#92070 = EDGE_CURVE ( 'NONE', #46120, #59760, #61980, .T. ) ;
#92071 = DIRECTION ( 'NONE',  ( -0.7071067811865487940, 0.7071067811865463515, 0.000000000000000000 ) ) ;
#92072 = ORIENTED_EDGE ( 'NONE', *, *, #23343, .T. ) ;
#92073 = CARTESIAN_POINT ( 'NONE',  ( 0.000000000000000000, 0.000000000000000000, 5.000000000000000000 ) ) ;
#92074 = CARTESIAN_POINT ( 'NONE',  ( -29.29289321881324426, 8.259292476615632594, 5.000000000000000000 ) ) ;
#92075 = LINE ( 'NONE', #15908, #129406 ) ;
#92076 = ADVANCED_FACE ( 'NONE', ( #49684 ), #6812, .T. ) ;
#92077 = CARTESIAN_POINT ( 'NONE',  ( 60.48921356237309510, -27.52281430457097500, 5.000000000000000000 ) ) ;
#92078 = FACE_BOUND ( 'NONE', #36721, .T. ) ;
#92079 = ORIENTED_EDGE ( 'NONE', *, *, #139089, .F. ) ;
#92080 = DIRECTION ( 'NONE',  ( 0.7071067811865486830, -0.7071067811865464625, -0.000000000000000000 ) ) ;
#92081 = LINE ( 'NONE', #101535, #124865 ) ;
#92082 = SURFACE_STYLE_FILL_AREA ( #103656 ) ;
#92083 = ORIENTED_EDGE ( 'NONE', *, *, #43085, .F. ) ;
#92084 = LINE ( 'NONE', #91408, #143090 ) ;
#92085 = ORIENTED_EDGE ( 'NONE', *, *, #72711, .F. ) ;
#92086 = VECTOR ( 'NONE', #120245, 1000.000000000000000 ) ;
#92088 = VERTEX_POINT ( 'NONE', #39515 ) ;
#92087 = ADVANCED_FACE ( 'NONE', ( #48222 ), #136650, .F. ) ;
#92089 =( BOUNDED_CURVE ( )  B_SPLINE_CURVE ( 2, ( #32443, #44033, #33876, #45485, #13504, #131757, #57073, #101252, #143329, #110670, #100558, #24409, #79563 ),
 .UNSPECIFIED., .F., .T. ) 
 B_SPLINE_CURVE_WITH_KNOTS ( ( 3, 2, 2, 2, 2, 2, 3 ),
 ( 0.6500000000000000222, 0.6527777777777777901, 0.6555555555555555580, 0.6583333333333333259, 0.6611111111111110938, 0.6638888888888888618, 0.6666666666666666297 ),
 .UNSPECIFIED. ) 
 CURVE ( )  GEOMETRIC_REPRESENTATION_ITEM ( )  RATIONAL_B_SPLINE_CURVE ( ( 1.000000000000000000, 0.9659258262890683122, 1.000000000000000000, 0.9659258262890683122, 1.000000000000000000, 0.9659258262890683122, 1.000000000000000000, 0.9659258262890683122, 1.000000000000000000, 0.9659258262890683122, 1.000000000000000000, 0.9659258262890683122, 1.000000000000000000 ) ) 
 REPRESENTATION_ITEM ( '' )  );
#92090 = EDGE_LOOP ( 'NONE', ( #66603, #117242, #140616, #132842 ) ) ;
#92091 = CARTESIAN_POINT ( 'NONE',  ( 38.55793019189811588, 6.110000000000000320, -1.637169565754156064 ) ) ;
#92092 = ORIENTED_EDGE ( 'NONE', *, *, #10344, .T. ) ;
#92093 = PLANE ( 'NONE',  #81133 ) ;
#92094 = DIRECTION ( 'NONE',  ( 0.3543493200069162685, -0.000000000000000000, -0.9351131265310288487 ) ) ;
#92095 = CARTESIAN_POINT ( 'NONE',  ( -26.29289321881326913, -15.74070752338412049, 5.000000000000000000 ) ) ;
#92096 = ADVANCED_FACE ( 'NONE', ( #59832 ), #59147, .T. ) ;
#92097 = EDGE_LOOP ( 'NONE', ( #72575, #62386, #95514, #57245 ) ) ;
#92098 = CARTESIAN_POINT ( 'NONE',  ( 34.49999999999975131, -2.568876922607791879, 4.000000000000000000 ) ) ;
#92099 = PLANE ( 'NONE',  #42215 ) ;
#92100 = ADVANCED_FACE ( 'NONE', ( #127199 ), #38080, .F. ) ;
#92101 = EDGE_CURVE ( 'NONE', #21299, #17453, #137388, .T. ) ;
#92102 = FACE_OUTER_BOUND ( 'NONE', #124454, .T. ) ;
#92103 = CARTESIAN_POINT ( 'NONE',  ( 41.78752705046289151, 0.000000000000000000, -7.949999999999998401 ) ) ;
#92104 = CARTESIAN_POINT ( 'NONE',  ( 156.1499999999997783, -49.14999999999999147, -34.92499999999975557 ) ) ;
#92105 = FACE_OUTER_BOUND ( 'NONE', #104307, .T. ) ;
#92106 = ORIENTED_EDGE ( 'NONE', *, *, #16948, .F. ) ;
#92107 = ORIENTED_EDGE ( 'NONE', *, *, #24460, .T. ) ;
#92108 = VERTEX_POINT ( 'NONE', #70726 ) ;
#92109 = ORIENTED_EDGE ( 'NONE', *, *, #110774, .F. ) ;
#92110 = LINE ( 'NONE', #136337, #17069 ) ;
#92111 = ORIENTED_EDGE ( 'NONE', *, *, #28610, .F. ) ;
#92112 = EDGE_CURVE ( 'NONE', #89225, #79591, #71418, .T. ) ;
#92113 = ORIENTED_EDGE ( 'NONE', *, *, #58594, .T. ) ;
#92114 = DIRECTION ( 'NONE',  ( -1.000000000000000000, -1.224606353822377258E-16, -0.000000000000000000 ) ) ;
#92115 = ADVANCED_FACE ( 'NONE', ( #60568, #104741 ), #93862, .F. ) ;
#92116 = ADVANCED_FACE ( 'NONE', ( #19865 ), #119179, .F. ) ;
#92117 = CARTESIAN_POINT ( 'NONE',  ( 0.005480084712502889671, 28.92564299267938210, 4.000000000000000000 ) ) ;
#92118 = VERTEX_POINT ( 'NONE', #74273 ) ;
#92119 = CARTESIAN_POINT ( 'NONE',  ( 16.49999999999988631, 12.05218569542904561, 5.000000000000000000 ) ) ;
#92120 = VERTEX_POINT ( 'NONE', #40926 ) ;
#92121 = CARTESIAN_POINT ( 'NONE',  ( 0.000000000000000000, 0.000000000000000000, 5.000000000000000000 ) ) ;
#92122 = CARTESIAN_POINT ( 'NONE',  ( 33.18398860626899705, 28.73617430169810305, 5.000000000000000000 ) ) ;
#92123 = CARTESIAN_POINT ( 'NONE',  ( 4.879569808101885897, 3.967499999999998916, 6.871911579029510442 ) ) ;
#92124 = ORIENTED_EDGE ( 'NONE', *, *, #14160, .T. ) ;
#92126 = CARTESIAN_POINT ( 'NONE',  ( 34.42499999999998295, 0.000000000000000000, 4.500000000000000888 ) ) ;
#92125 = CARTESIAN_POINT ( 'NONE',  ( 99.07876352523145158, -7.482591942790327058E-16, 6.109999999999999432 ) ) ;
#92127 = EDGE_CURVE ( 'NONE', #122527, #139318, #20573, .T. ) ;
#92128 = LINE ( 'NONE', #113166, #81319 ) ;
#92129 = SURFACE_STYLE_USAGE ( .BOTH. , #91451 ) ;
#92130 = ORIENTED_EDGE ( 'NONE', *, *, #102059, .F. ) ;
#92131 = ORIENTED_EDGE ( 'NONE', *, *, #52527, .T. ) ;
#92132 = CARTESIAN_POINT ( 'NONE',  ( 18.17159235450331778, 9.902892378096218942E-16, 0.000000000000000000 ) ) ;
#92133 = ORIENTED_EDGE ( 'NONE', *, *, #18392, .F. ) ;
#92134 = DIRECTION ( 'NONE',  ( -0.6830127018922181881, 0.6830127018922202975, -0.2588190451025214056 ) ) ;
#92135 = DIRECTION ( 'NONE',  ( 0.7071067811865487940, -0.7071067811865463515, 0.000000000000000000 ) ) ;
#92136 = ADVANCED_FACE ( 'NONE', ( #41623 ), #53966, .F. ) ;
#92137 = LINE ( 'NONE', #58147, #19182 ) ;
#92138 = ORIENTED_EDGE ( 'NONE', *, *, #32006, .T. ) ;
#92139 = DIRECTION ( 'NONE',  ( -0.7071067811865486830, 0.7071067811865464625, 0.000000000000000000 ) ) ;
#92140 = VECTOR ( 'NONE', #130748, 1000.000000000000000 ) ;
#92141 = FILL_AREA_STYLE ('',( #105172 ) ) ;
#92142 = DIRECTION ( 'NONE',  ( -0.7071067811865487940, 0.7071067811865463515, 0.000000000000000000 ) ) ;
#92143 = VERTEX_POINT ( 'NONE', #8249 ) ;
#92144 = DIRECTION ( 'NONE',  ( -0.000000000000000000, 0.000000000000000000, 1.000000000000000000 ) ) ;
#92145 = LINE ( 'NONE', #135682, #2918 ) ;
#92146 = ORIENTED_EDGE ( 'NONE', *, *, #33033, .T. ) ;
#92147 = VECTOR ( 'NONE', #86586, 1000.000000000000000 ) ;
#92149 = ORIENTED_EDGE ( 'NONE', *, *, #20533, .F. ) ;
#92148 = DIRECTION ( 'NONE',  ( 0.7071067811865487940, 0.7071067811865463515, -0.000000000000000000 ) ) ;
#92150 = EDGE_LOOP ( 'NONE', ( #141752, #88570, #29414, #132691 ) ) ;
#92151 = LINE ( 'NONE', #37072, #49389 ) ;
#92152 = CARTESIAN_POINT ( 'NONE',  ( -14.99999999999990230, -16.02097659208072855, -11.96015758381205707 ) ) ;
#92153 = VECTOR ( 'NONE', #15407, 1000.000000000000000 ) ;
#92154 = VERTEX_POINT ( 'NONE', #18411 ) ;
#92155 = CARTESIAN_POINT ( 'NONE',  ( 111.3958333333333144, -2.130196079827427091, 7.949999999999998401 ) ) ;
#92156 = AXIS2_PLACEMENT_3D ( 'NONE', #111539, #10772, #55040 ) ;
#92157 = EDGE_CURVE ( 'NONE', #82012, #101812, #52510, .T. ) ;
#92158 = LINE ( 'NONE', #16754, #38261 ) ;
#92159 = EDGE_CURVE ( 'NONE', #19533, #119254, #120588, .T. ) ;
#92160 = DIRECTION ( 'NONE',  ( -0.3543493200069162685, -0.000000000000000000, -0.9351131265310288487 ) ) ;
#92161 = VERTEX_POINT ( 'NONE', #129341 ) ;
#92162 = CARTESIAN_POINT ( 'NONE',  ( -14.27718569542929572, -21.72500000000000142, 5.000000000000000000 ) ) ;
#92163 = DIRECTION ( 'NONE',  ( -1.000000000000000000, -1.224606353822377258E-16, -0.000000000000000000 ) ) ;
#92164 = LINE ( 'NONE', #27627, #42039 ) ;
#92165 = LINE ( 'NONE', #4389, #28592 ) ;
#92166 = DIRECTION ( 'NONE',  ( -1.000000000000000000, -0.000000000000000000, -0.000000000000000000 ) ) ;
#92167 = EDGE_CURVE ( 'NONE', #68527, #22961, #31478, .T. ) ;
#92168 = FACE_OUTER_BOUND ( 'NONE', #70214, .T. ) ;
#92169 = CARTESIAN_POINT ( 'NONE',  ( -42.29974487139158157, -27.71228299555235708, 4.000000000000000000 ) ) ;
#92170 = ORIENTED_EDGE ( 'NONE', *, *, #93622, .T. ) ;
#92171 = ORIENTED_EDGE ( 'NONE', *, *, #46314, .T. ) ;
#92172 = ORIENTED_EDGE ( 'NONE', *, *, #11226, .T. ) ;
#92173 = CARTESIAN_POINT ( 'NONE',  ( 123.5000000000000000, 0.000000000000000000, -7.950000000000000178 ) ) ;
#92174 = VERTEX_POINT ( 'NONE', #65569 ) ;
#92175 = ORIENTED_EDGE ( 'NONE', *, *, #81387, .T. ) ;
#92176 = ORIENTED_EDGE ( 'NONE', *, *, #7924, .F. ) ;
#92177 = DIRECTION ( 'NONE',  ( 0.000000000000000000, -1.000000000000000000, 0.000000000000000000 ) ) ;
#92178 = VECTOR ( 'NONE', #124644, 999.9999999999998863 ) ;
#92179 = DIRECTION ( 'NONE',  ( 0.000000000000000000, 0.000000000000000000, 1.000000000000000000 ) ) ;
#92180 = ORIENTED_EDGE ( 'NONE', *, *, #84266, .T. ) ;
#92181 = CARTESIAN_POINT ( 'NONE',  ( -13.49999999999990408, 21.43112307739196609, 4.000000000000000000 ) ) ;
#92182 = VECTOR ( 'NONE', #44612, 1000.000000000000000 ) ;
#92183 = FACE_OUTER_BOUND ( 'NONE', #18064, .T. ) ;
#92184 = DIRECTION ( 'NONE',  ( 0.6830127018922180770, -0.6830127018922204085, -0.2588190451025213501 ) ) ;
#92185 = CARTESIAN_POINT ( 'NONE',  ( 113.4587635252314470, 0.000000000000000000, -6.110000000000001208 ) ) ;
#92186 = ORIENTED_EDGE ( 'NONE', *, *, #58232, .T. ) ;
#92187 = DIRECTION ( 'NONE',  ( -0.7071067811865486830, -0.7071067811865464625, 0.000000000000000000 ) ) ;
#92188 = DIRECTION ( 'NONE',  ( 0.7071067811865487940, 0.7071067811865463515, -0.000000000000000000 ) ) ;
#92189 = VECTOR ( 'NONE', #55054, 1000.000000000000000 ) ;
#92190 = LINE ( 'NONE', #58210, #123741 ) ;
#92191 = CARTESIAN_POINT ( 'NONE',  ( 1.179137009529055646, 2.860328551334985203, 6.310333628962586872 ) ) ;
#92192 = CARTESIAN_POINT ( 'NONE',  ( 17.99999999999987566, -9.033600742197641864, 5.000000000000000000 ) ) ;
#92193 = CARTESIAN_POINT ( 'NONE',  ( -29.99451991528749417, 28.92564299267958816, 4.000000000000000000 ) ) ;
#92194 = DIRECTION ( 'NONE',  ( -0.7071067811865487940, 0.7071067811865463515, 0.000000000000000000 ) ) ;
#92195 = CARTESIAN_POINT ( 'NONE',  ( 37.70419371712956291, -6.884901960086285300, -3.975000000000000089 ) ) ;
#92196 = CARTESIAN_POINT ( 'NONE',  ( 41.99451991528749062, 28.92564299267967343, 4.000000000000000000 ) ) ;
#92197 =( NAMED_UNIT ( * ) PLANE_ANGLE_UNIT ( ) SI_UNIT ( $, .RADIAN. ) );
#92198 = VERTEX_POINT ( 'NONE', #143085 ) ;
#92199 = VERTEX_POINT ( 'NONE', #32186 ) ;
#92200 = CARTESIAN_POINT ( 'NONE',  ( 33.37499999999998579, 7.950000000000000178, 1.460391307983218535E-15 ) ) ;
#92201 = ORIENTED_EDGE ( 'NONE', *, *, #77749, .F. ) ;
#92202 = VERTEX_POINT ( 'NONE', #8942 ) ;
#92203 = DIRECTION ( 'NONE',  ( 0.7071067811865487940, 0.7071067811865463515, -0.000000000000000000 ) ) ;
#92204 = ADVANCED_FACE ( 'NONE', ( #75700 ), #53206, .T. ) ;
#92205 =( NAMED_UNIT ( * ) PLANE_ANGLE_UNIT ( ) SI_UNIT ( $, .RADIAN. ) );
#92206 = ORIENTED_EDGE ( 'NONE', *, *, #124245, .F. ) ;
#92207 = AXIS2_PLACEMENT_3D ( 'NONE', #70931, #68797, #62732 ) ;
#92208 = LINE ( 'NONE', #69806, #94132 ) ;
#92210 =( GEOMETRIC_REPRESENTATION_CONTEXT ( 3 ) GLOBAL_UNCERTAINTY_ASSIGNED_CONTEXT ( ( #126078 ) ) GLOBAL_UNIT_ASSIGNED_CONTEXT ( ( #1733, #13347, #82230 ) ) REPRESENTATION_CONTEXT ( 'NONE', 'WORKASPACE' ) );
#92209 = PLANE ( 'NONE',  #63100 ) ;
#92211 = DIRECTION ( 'NONE',  ( 0.000000000000000000, -1.000000000000000000, 0.000000000000000000 ) ) ;
#92212 = CARTESIAN_POINT ( 'NONE',  ( 28.00043019189810067, -3.055000000000002380, 5.291415217122920289 ) ) ;
#92213 = ORIENTED_EDGE ( 'NONE', *, *, #111397, .F. ) ;
#92214 = CARTESIAN_POINT ( 'NONE',  ( -12.48921356237309155, -27.52281430457064104, 5.000000000000000000 ) ) ;
#92215 = ORIENTED_EDGE ( 'NONE', *, *, #138182, .F. ) ;
#92216 = CARTESIAN_POINT ( 'NONE',  ( -10.49999999999992539, 22.22500000000000853, 4.362957392718823435 ) ) ;
#92217 = CARTESIAN_POINT ( 'NONE',  ( -29.99451991528749417, 28.92564299267958816, 4.000000000000000000 ) ) ;
#92218 = CYLINDRICAL_SURFACE ( 'NONE', #104577, 2.552699999999994418 ) ;
#92219 = EDGE_CURVE ( 'NONE', #36583, #36166, #97414, .T. ) ;
#92220 = CARTESIAN_POINT ( 'NONE',  ( 2.999999999999981792, -1.068876922607802538, 4.000000000000000000 ) ) ;
#92221 = ORIENTED_EDGE ( 'NONE', *, *, #112248, .F. ) ;
#92222 = EDGE_CURVE ( 'NONE', #25213, #26153, #27053, .T. ) ;
#92223 = ADVANCED_FACE ( 'NONE', ( #43778 ), #140929, .T. ) ;
#92224 = EDGE_LOOP ( 'NONE', ( #8165, #112459, #59203, #91075 ) ) ;
#92225 = CARTESIAN_POINT ( 'NONE',  ( 39.01669371712955581, 7.950000000000000178, -2.130196079827421318 ) ) ;
#92226 = CARTESIAN_POINT ( 'NONE',  ( 0.000000000000000000, 0.000000000000000000, 5.000000000000000000 ) ) ;
#92227 = DIRECTION ( 'NONE',  ( -1.000000000000000000, -0.000000000000000000, -0.000000000000000000 ) ) ;
#92228 = DIRECTION ( 'NONE',  ( -0.000000000000000000, 0.3543493200069153248, 0.9351131265310292928 ) ) ;
#92229 = EDGE_CURVE ( 'NONE', #98543, #66493, #87285, .T. ) ;
#92230 = ADVANCED_FACE ( 'NONE', ( #95996 ), #99555, .F. ) ;
#92231 = CARTESIAN_POINT ( 'NONE',  ( 45.12043019189810877, 3.055000000000001936, -5.291415217122916737 ) ) ;
#92232 = CARTESIAN_POINT ( 'NONE',  ( -24.29974487139158867, -27.71228299555223273, 4.000000000000000000 ) ) ;
#92233 = EDGE_CURVE ( 'NONE', #115804, #92397, #58275, .T. ) ;
#92234 = CARTESIAN_POINT ( 'NONE',  ( 32.99999999999977263, -6.108550654416931458, -3.114665004254893343 ) ) ;
#92235 = ORIENTED_EDGE ( 'NONE', *, *, #16315, .T. ) ;
#92236 = EDGE_LOOP ( 'NONE', ( #114504, #43337, #7360, #64901 ) ) ;
#92237 = DIRECTION ( 'NONE',  ( 0.7071067811865486830, -0.7071067811865464625, -0.000000000000000000 ) ) ;
#92238 = ORIENTED_EDGE ( 'NONE', *, *, #76601, .F. ) ;
#92239 = EDGE_CURVE ( 'NONE', #103031, #116321, #23437, .T. ) ;
#92240 = CARTESIAN_POINT ( 'NONE',  ( 34.79316404164333676, 22.27000000000000668, -10.13466756456404916 ) ) ;
#92241 = ORIENTED_EDGE ( 'NONE', *, *, #53551, .T. ) ;
#92242 = CARTESIAN_POINT ( 'NONE',  ( 9.183988606268997046, 28.73617430169793607, 5.000000000000000000 ) ) ;
#92244 = EDGE_CURVE ( 'NONE', #31004, #115675, #57530, .T. ) ;
#92243 = AXIS2_PLACEMENT_3D ( 'NONE', #116526, #25953, #37556 ) ;
#92245 = VECTOR ( 'NONE', #114765, 1000.000000000000000 ) ;
#92246 = VECTOR ( 'NONE', #8763, 1000.000000000000000 ) ;
#92247 = CARTESIAN_POINT ( 'NONE',  ( 0.7307956238753654521, -0.3999999999999997446, -2.467792535850613866 ) ) ;
#92248 = AXIS2_PLACEMENT_3D ( 'NONE', #109559, #76974, #122561 ) ;
#92249 = FACE_BOUND ( 'NONE', #136890, .T. ) ;
#92250 = DIRECTION ( 'NONE',  ( 0.6830127018922181881, 0.6830127018922202975, -0.2588190451025214056 ) ) ;
#92251 = CARTESIAN_POINT ( 'NONE',  ( 23.70025512860841133, -27.71228299555189523, 4.000000000000000000 ) ) ;
#92252 = CARTESIAN_POINT ( 'NONE',  ( 21.70710678118639692, 11.25929247661560417, 5.000000000000000000 ) ) ;
#92253 = CARTESIAN_POINT ( 'NONE',  ( 20.67906569311139009, 4.202752102959690472E-16, 0.000000000000000000 ) ) ;
#92255 = EDGE_LOOP ( 'NONE', ( #49847, #13114, #15644, #31266 ) ) ;
#92254 = LINE ( 'NONE', #35793, #62082 ) ;
#92256 = EDGE_CURVE ( 'NONE', #98989, #44722, #124187, .T. ) ;
#92257 = VECTOR ( 'NONE', #110990, 1000.000000000000000 ) ;
#92258 = AXIS2_PLACEMENT_3D ( 'NONE', #69985, #138053, #114148 ) ;
#92259 = CARTESIAN_POINT ( 'NONE',  ( -7.140000000000001457, -35.13237070076360169, 17.62370837922860289 ) ) ;
#92260 = VERTEX_POINT ( 'NONE', #957 ) ;
#92261 = ORIENTED_EDGE ( 'NONE', *, *, #51160, .F. ) ;
#92262 = CARTESIAN_POINT ( 'NONE',  ( 65.82876352523145158, 0.000000000000000000, -6.109999999999998543 ) ) ;
#92263 = ORIENTED_EDGE ( 'NONE', *, *, #122102, .T. ) ;
#92264 = DIRECTION ( 'NONE',  ( -0.6830127018922181881, 0.6830127018922202975, -0.2588190451025214056 ) ) ;
#92265 = EDGE_CURVE ( 'NONE', #99187, #64475, #132240, .T. ) ;
#92266 = ORIENTED_EDGE ( 'NONE', *, *, #141566, .F. ) ;
#92267 = CARTESIAN_POINT ( 'NONE',  ( 32.20710678118632586, -20.24070752338407075, 5.000000000000000000 ) ) ;
#92268 = PRESENTATION_LAYER_ASSIGNMENT (  '', '', ( #59915 ) ) ;
#92269 = DIRECTION ( 'NONE',  ( -0.7071067811865486830, 0.7071067811865464625, 0.000000000000000000 ) ) ;
#92270 = EDGE_CURVE ( 'NONE', #71223, #61774, #11833, .T. ) ;
#92271 = AXIS2_PLACEMENT_3D ( 'NONE', #127893, #27839, #28574 ) ;
#92272 = CARTESIAN_POINT ( 'NONE',  ( 101.4791666666666430, -7.950000000000000178, 2.130196079827424427 ) ) ;
#92273 = CARTESIAN_POINT ( 'NONE',  ( -63.48921356237309510, -27.52281430457099631, 5.000000000000000000 ) ) ;
#92274 = EDGE_CURVE ( 'NONE', #55534, #4302, #12557, .T. ) ;
#92275 = CARTESIAN_POINT ( 'NONE',  ( 16.04166666666666785, 3.047499999999993214, -5.278424836066146320 ) ) ;
#92276 = PLANE ( 'NONE',  #20747 ) ;
#92277 = ORIENTED_EDGE ( 'NONE', *, *, #104858, .T. ) ;
#92278 = AXIS2_PLACEMENT_3D ( 'NONE', #111636, #45695, #102197 ) ;
#92279 = ORIENTED_EDGE ( 'NONE', *, *, #100564, .F. ) ;
#92280 = DIRECTION ( 'NONE',  ( -1.000000000000000000, 0.000000000000000000, 0.000000000000000000 ) ) ;
#92281 = DIRECTION ( 'NONE',  ( 1.000000000000000000, 0.000000000000000000, 0.000000000000000000 ) ) ;
#92282 = ORIENTED_EDGE ( 'NONE', *, *, #48782, .T. ) ;
#92284 = EDGE_CURVE ( 'NONE', #81393, #64729, #46690, .T. ) ;
#92283 = CIRCLE ( 'NONE', #18170, 1.000000000000000888 ) ;
#92285 = ORIENTED_EDGE ( 'NONE', *, *, #80394, .T. ) ;
#92286 = VERTEX_POINT ( 'NONE', #100997 ) ;
#92287 = DIRECTION ( 'NONE',  ( 0.6830127018922180770, -0.6830127018922204085, -0.2588190451025213501 ) ) ;
#92288 = ORIENTED_EDGE ( 'NONE', *, *, #42325, .T. ) ;
#92289 = VECTOR ( 'NONE', #65298, 1000.000000000000000 ) ;
#92290 = CARTESIAN_POINT ( 'NONE',  ( -16.82816939922340893, -20.24070752338407431, 4.000000000000000000 ) ) ;
#92291 = AXIS2_PLACEMENT_3D ( 'NONE', #1335, #2030, #34716 ) ;
#92292 = CARTESIAN_POINT ( 'NONE',  ( 26.40000000000000568, -16.48000000000005016, -12.70000000000043272 ) ) ;
#92293 = CARTESIAN_POINT ( 'NONE',  ( 8.817069808101885897, -2.126176841940956130, 7.934999999999991616 ) ) ;
#92294 = CARTESIAN_POINT ( 'NONE',  ( -18.48921356237309510, -27.52281430457068367, 5.000000000000000000 ) ) ;
#92295 = VERTEX_POINT ( 'NONE', #2368 ) ;
#92296 = EDGE_CURVE ( 'NONE', #68931, #34970, #60199, .T. ) ;
#92297 = DIRECTION ( 'NONE',  ( -0.7071067811865486830, -0.7071067811865464625, 0.000000000000000000 ) ) ;
#92298 = CARTESIAN_POINT ( 'NONE',  ( 25.38743044895410961, -6.094999999999989093, -0.1392054293825079614 ) ) ;
#92299 = VECTOR ( 'NONE', #133717, 1000.000000000000000 ) ;
#92301 = ORIENTED_EDGE ( 'NONE', *, *, #121237, .F. ) ;
#92300 = DIRECTION ( 'NONE',  ( -0.000000000000000000, 0.3543493200069152138, -0.9351131265310292928 ) ) ;
#92302 = ORIENTED_EDGE ( 'NONE', *, *, #96098, .F. ) ;
#92303 = LINE ( 'NONE', #81483, #54256 ) ;
#92304 = LINE ( 'NONE', #71308, #23745 ) ;
#92305 = CARTESIAN_POINT ( 'NONE',  ( 11.99999999999991296, -16.02097659208071079, -11.96015758381211569 ) ) ;
#92306 = ORIENTED_EDGE ( 'NONE', *, *, #14963, .F. ) ;
#92307 = LINE ( 'NONE', #136530, #92245 ) ;
#92308 = EDGE_CURVE ( 'NONE', #9331, #122655, #45239, .T. ) ;
#92309 = CARTESIAN_POINT ( 'NONE',  ( 34.92499999999998295, -19.29806943317882784, 4.500000000000000888 ) ) ;
#92310 = CARTESIAN_POINT ( 'NONE',  ( -14.99999999999989875, 10.93112307739207623, 4.000000000000000000 ) ) ;
#92311 = LINE ( 'NONE', #93765, #14295 ) ;
#92312 = ORIENTED_EDGE ( 'NONE', *, *, #97429, .T. ) ;
#92313 = CARTESIAN_POINT ( 'NONE',  ( -3.489213562373097322, -27.52281430457057709, 5.000000000000000000 ) ) ;
#92314 = CARTESIAN_POINT ( 'NONE',  ( 34.92499999999998295, 12.66246187583888450, 4.000000000000000000 ) ) ;
#92315 = FACE_OUTER_BOUND ( 'NONE', #71020, .T. ) ;
#92316 = LINE ( 'NONE', #35862, #79514 ) ;
#92317 = ADVANCED_FACE ( 'NONE', ( #11103 ), #89416, .F. ) ;
#92318 = DIRECTION ( 'NONE',  ( -1.000000000000000000, -0.000000000000000000, -0.000000000000000000 ) ) ;
#92319 = VERTEX_POINT ( 'NONE', #78555 ) ;
#92320 = VERTEX_POINT ( 'NONE', #111894 ) ;
#92321 = CARTESIAN_POINT ( 'NONE',  ( 25.01899999999999835, 3.174999999999997158, 1.444000000000000394 ) ) ;
#92322 = SURFACE_STYLE_USAGE ( .BOTH. , #116240 ) ;
#92323 = CARTESIAN_POINT ( 'NONE',  ( 3.624569808101886448, -6.871911579029512218, 3.967499999999996252 ) ) ;
#92324 = CARTESIAN_POINT ( 'NONE',  ( 64.82919371712955581, -3.975000000000001865, 6.884901960086284411 ) ) ;
#92325 = EDGE_CURVE ( 'NONE', #29884, #16488, #35069, .T. ) ;
#92326 = CARTESIAN_POINT ( 'NONE',  ( 42.18398860626899705, 28.73617430169816700, 5.000000000000000000 ) ) ;
#92327 = CARTESIAN_POINT ( 'NONE',  ( 15.48921356237309510, -27.52281430457066236, 5.000000000000000000 ) ) ;
#92328 = CARTESIAN_POINT ( 'NONE',  ( -30.79289321881324071, -17.24070752338410628, 5.000000000000000000 ) ) ;
#92329 = VERTEX_POINT ( 'NONE', #1653 ) ;
#92330 = FACE_OUTER_BOUND ( 'NONE', #91866, .T. ) ;
#92331 = DIRECTION ( 'NONE',  ( 0.7071067811865487940, 0.7071067811865463515, -0.000000000000000000 ) ) ;
#92332 = DIRECTION ( 'NONE',  ( -1.000000000000000000, -1.224606353822377258E-16, -0.000000000000000000 ) ) ;
#92333 = CARTESIAN_POINT ( 'NONE',  ( 46.87043019189811588, -3.055000000000001936, 5.291415217122918513 ) ) ;
#92334 = EDGE_CURVE ( 'NONE', #142484, #5541, #45936, .T. ) ;
#92335 = CARTESIAN_POINT ( 'NONE',  ( 39.48921356237310221, -27.52281430457082934, 5.000000000000000000 ) ) ;
#92336 = ADVANCED_FACE ( 'NONE', ( #77152 ), #112602, .F. ) ;
#92337 = ORIENTED_EDGE ( 'NONE', *, *, #42043, .T. ) ;
#92338 = PLANE ( 'NONE',  #81259 ) ;
#92339 = ORIENTED_EDGE ( 'NONE', *, *, #11098, .T. ) ;
#92340 = LINE ( 'NONE', #50830, #127070 ) ;
#92341 = VERTEX_POINT ( 'NONE', #24869 ) ;
#92342 = CARTESIAN_POINT ( 'NONE',  ( -47.99451991528749062, 28.92564299267971251, 4.000000000000000000 ) ) ;
#92343 = AXIS2_PLACEMENT_3D ( 'NONE', #94585, #92432, #137405 ) ;
#92344 = AXIS2_PLACEMENT_3D ( 'NONE', #18492, #38154, #51168 ) ;
#92345 = STYLED_ITEM ( 'NONE', ( #22667 ), #63034 ) ;
#92346 = DIRECTION ( 'NONE',  ( 0.7071067811865487940, 0.7071067811865463515, 0.000000000000000000 ) ) ;
#92347 = DIRECTION ( 'NONE',  ( 0.6830127018922181881, 0.6830127018922202975, -0.2588190451025214056 ) ) ;
#92348 = AXIS2_PLACEMENT_3D ( 'NONE', #110088, #88375, #132613 ) ;
#92349 = CARTESIAN_POINT ( 'NONE',  ( 15.42327845806343944, 11.25929247661560240, 17.85071094206580966 ) ) ;
#92350 = EDGE_CURVE ( 'NONE', #43579, #84626, #69111, .T. ) ;
#92351 = DIRECTION ( 'NONE',  ( -0.6830127018922180770, -0.6830127018922204085, -0.2588190451025214056 ) ) ;
#92352 = CARTESIAN_POINT ( 'NONE',  ( 11.95833333333333393, -3.047499999999997211, -5.278424836066143655 ) ) ;
#92353 = VERTEX_POINT ( 'NONE', #3110 ) ;
#92354 = CARTESIAN_POINT ( 'NONE',  ( -9.781626882924873811, 21.74787736706806740, 4.999607392498049308 ) ) ;
#92355 = CARTESIAN_POINT ( 'NONE',  ( -32.99451991528749062, 28.92564299267960948, 4.000000000000000000 ) ) ;
#92356 = UNCERTAINTY_MEASURE_WITH_UNIT (LENGTH_MEASURE( 1.000000000000000082E-05 ), #54916, 'distance_accuracy_value', 'NONE');
#92357 = VECTOR ( 'NONE', #131413, 1000.000000000000000 ) ;
#92358 = CARTESIAN_POINT ( 'NONE',  ( -5.241399257802002332, 21.72500000000000853, 5.000000000000000000 ) ) ;
#92359 = CARTESIAN_POINT ( 'NONE',  ( 117.0833333333333286, 6.884901960086290629, -3.974999999999994316 ) ) ;
#92360 = CARTESIAN_POINT ( 'NONE',  ( 76.93336038379621300, 2.130196079827431532, -7.949999999999997513 ) ) ;
#92361 = CARTESIAN_POINT ( 'NONE',  ( 21.32816939922337696, -12.74070752338415424, 4.000000000000000000 ) ) ;
#92362 = ORIENTED_EDGE ( 'NONE', *, *, #101720, .F. ) ;
#92363 = VERTEX_POINT ( 'NONE', #32932 ) ;
#92364 = CARTESIAN_POINT ( 'NONE',  ( 61.08333333333332149, 6.884901960086290629, -3.974999999999994316 ) ) ;
#92365 = LINE ( 'NONE', #102576, #102580 ) ;
#92366 = CARTESIAN_POINT ( 'NONE',  ( -19.49999999999986500, -7.533600742197656963, 5.000000000000000000 ) ) ;
#92367 = DIRECTION ( 'NONE',  ( -0.000000000000000000, 0.3543493200069153248, 0.9351131265310292928 ) ) ;
#92368 = AXIS2_PLACEMENT_3D ( 'NONE', #88457, #79022, #123937 ) ;
#92369 = ORIENTED_EDGE ( 'NONE', *, *, #86213, .F. ) ;
#92370 = CARTESIAN_POINT ( 'NONE',  ( 10.96659967656970736, 6.759292476615645917, 12.28218704918524828 ) ) ;
#92371 = VECTOR ( 'NONE', #110375, 1000.000000000000000 ) ;
#92372 = CARTESIAN_POINT ( 'NONE',  ( 59.50043019189810423, -3.055000000000002380, 5.291415217122920289 ) ) ;
#92373 = DIRECTION ( 'NONE',  ( 0.7071067811865487940, -0.7071067811865463515, 0.000000000000000000 ) ) ;
#92374 = ORIENTED_EDGE ( 'NONE', *, *, #39764, .T. ) ;
#92375 = VERTEX_POINT ( 'NONE', #71977 ) ;
#92376 = FACE_OUTER_BOUND ( 'NONE', #83793, .T. ) ;
#92377 = VECTOR ( 'NONE', #83716, 1000.000000000000227 ) ;
#92378 = AXIS2_PLACEMENT_3D ( 'NONE', #118567, #62797, #63522 ) ;
#92379 = CARTESIAN_POINT ( 'NONE',  ( 19.49999999999987210, 10.08746187583914278, 4.000000000000000000 ) ) ;
#92380 = DIRECTION ( 'NONE',  ( -1.000000000000000000, -0.000000000000000000, -0.000000000000000000 ) ) ;
#92381 = AXIS2_PLACEMENT_3D ( 'NONE', #86832, #109989, #19416 ) ;
#92382 = CARTESIAN_POINT ( 'NONE',  ( 1.199999999999999956, 0.000000000000000000, 0.000000000000000000 ) ) ;
#92383 = PLANE ( 'NONE',  #67366 ) ;
#92384 = EDGE_CURVE ( 'NONE', #106219, #19553, #135781, .T. ) ;
#92385 = EDGE_CURVE ( 'NONE', #107048, #125144, #115405, .T. ) ;
#92387 = EDGE_LOOP ( 'NONE', ( #16843, #91140, #68436, #98859 ) ) ;
#92386 = CARTESIAN_POINT ( 'NONE',  ( -17.99999999999986855, -19.44781430457062754, 5.000000000000000000 ) ) ;
#92388 = CARTESIAN_POINT ( 'NONE',  ( -19.49999999999986500, -15.29013452822856145, 0.3645803511609898018 ) ) ;
#92389 = LINE ( 'NONE', #4617, #45442 ) ;
#92390 = CARTESIAN_POINT ( 'NONE',  ( -3.489213562373097322, -27.52281430457057709, 5.000000000000000000 ) ) ;
#92391 = VECTOR ( 'NONE', #130930, 1000.000000000000000 ) ;
#92392 =( NAMED_UNIT ( * ) PLANE_ANGLE_UNIT ( ) SI_UNIT ( $, .RADIAN. ) );
#92393 = AXIS2_PLACEMENT_3D ( 'NONE', #134967, #109607, #101576 ) ;
#92395 = ORIENTED_EDGE ( 'NONE', *, *, #32028, .F. ) ;
#92394 = EDGE_CURVE ( 'NONE', #133168, #143141, #38612, .T. ) ;
#92396 = ADVANCED_FACE ( 'NONE', ( #72721 ), #92989, .T. ) ;
#92397 = VERTEX_POINT ( 'NONE', #25573 ) ;
#92398 = EDGE_CURVE ( 'NONE', #13957, #80820, #103824, .T. ) ;
#92399 = DIRECTION ( 'NONE',  ( 0.7071067811865486830, -0.7071067811865464625, -0.000000000000000000 ) ) ;
#92400 = LINE ( 'NONE', #82286, #120460 ) ;
#92402 = EDGE_CURVE ( 'NONE', #91522, #11791, #15384, .T. ) ;
#92401 = LINE ( 'NONE', #136628, #15497 ) ;
#92403 = PLANE ( 'NONE',  #77915 ) ;
#92404 = CARTESIAN_POINT ( 'NONE',  ( 73.14169371712955581, -2.130196079827424871, -7.949999999999998401 ) ) ;
#92405 = ORIENTED_EDGE ( 'NONE', *, *, #49478, .T. ) ;
#92406 = VERTEX_POINT ( 'NONE', #83560 ) ;
#92407 = PRESENTATION_LAYER_ASSIGNMENT (  '', '', ( #64698 ) ) ;
#92408 = EDGE_CURVE ( 'NONE', #71767, #22720, #17546, .T. ) ;
#92409 = CARTESIAN_POINT ( 'NONE',  ( -20.56494995367816614, -2.598550695876024275, 5.000000000000000000 ) ) ;
#92410 = EDGE_CURVE ( 'NONE', #126070, #104812, #80704, .T. ) ;
#92411 = ORIENTED_EDGE ( 'NONE', *, *, #91099, .F. ) ;
#92412 = CARTESIAN_POINT ( 'NONE',  ( -21.52400138585434064, 22.03583458319437582, 4.979811245910087614 ) ) ;
#92413 = EDGE_LOOP ( 'NONE', ( #95084, #107215, #75986, #70980 ) ) ;
#92414 = CARTESIAN_POINT ( 'NONE',  ( -44.99451991528749772, 28.92564299267969474, 4.000000000000000000 ) ) ;
#92415 = EDGE_CURVE ( 'NONE', #35605, #49913, #116873, .T. ) ;
#92416 = FACE_BOUND ( 'NONE', #72197, .T. ) ;
#92417 = CARTESIAN_POINT ( 'NONE',  ( 0.000000000000000000, 0.000000000000000000, 5.000000000000000000 ) ) ;
#92418 = DIRECTION ( 'NONE',  ( 0.7071067811865487940, 0.7071067811865463515, 0.000000000000000000 ) ) ;
#92419 = CARTESIAN_POINT ( 'NONE',  ( 38.14169371712954870, -2.130196079827424871, -7.949999999999998401 ) ) ;
#92420 = DIRECTION ( 'NONE',  ( 2.781805975412905890E-17, -0.3543493200069152693, 0.9351131265310292928 ) ) ;
#92421 = EDGE_CURVE ( 'NONE', #67571, #92905, #124428, .T. ) ;
#92422 = LINE ( 'NONE', #58451, #122734 ) ;
#92423 = CARTESIAN_POINT ( 'NONE',  ( 152.4000000000000057, 4.744999999999950369, 0.07499999999998610556 ) ) ;
#92424 = ORIENTED_EDGE ( 'NONE', *, *, #22429, .F. ) ;
#92425 = ORIENTED_EDGE ( 'NONE', *, *, #30413, .T. ) ;
#92426 = CARTESIAN_POINT ( 'NONE',  ( 91.20376352523145158, 6.109999999999998543, 1.122388791418548911E-15 ) ) ;
#92427 = VERTEX_POINT ( 'NONE', #127024 ) ;
#92428 = DIRECTION ( 'NONE',  ( 0.6830127018922181881, 0.6830127018922202975, -0.2588190451025214056 ) ) ;
#92429 = LINE ( 'NONE', #14887, #16640 ) ;
#92430 = LINE ( 'NONE', #73574, #130500 ) ;
#92431 = VERTEX_POINT ( 'NONE', #48067 ) ;
#92432 = DIRECTION ( 'NONE',  ( -0.6830127018922180770, -0.6830127018922204085, -0.2588190451025213501 ) ) ;
#92433 = CARTESIAN_POINT ( 'NONE',  ( 21.71757738642552127, -21.73023691814493574, 5.000000000000000888 ) ) ;
#92435 = DIRECTION ( 'NONE',  ( 0.6830127018922181881, 0.6830127018922202975, -0.2588190451025214056 ) ) ;
#92434 = DIRECTION ( 'NONE',  ( 0.7071067811865487940, 0.7071067811865463515, 0.000000000000000000 ) ) ;
#92436 = ADVANCED_FACE ( 'NONE', ( #58988 ), #36469, .F. ) ;
#92437 = CARTESIAN_POINT ( 'NONE',  ( 24.48921356237309510, -27.52281430457072631, 5.000000000000000000 ) ) ;
#92438 = AXIS2_PLACEMENT_3D ( 'NONE', #117193, #27336, #17871 ) ;
#92439 = COLOUR_RGB ( '', 0.08235294, 0.09019608, 0.10196078) ;
#92440 = VECTOR ( 'NONE', #123330, 1000.000000000000227 ) ;
#92441 = DIRECTION ( 'NONE',  ( -0.7071067811865486830, -0.7071067811865464625, 0.000000000000000000 ) ) ;
#92442 = AXIS2_PLACEMENT_3D ( 'NONE', #53943, #142363, #200 ) ;
#92443 = ORIENTED_EDGE ( 'NONE', *, *, #54043, .T. ) ;
#92444 = DIRECTION ( 'NONE',  ( 0.7071067811865487940, 0.7071067811865463515, -0.000000000000000000 ) ) ;
#92445 = EDGE_CURVE ( 'NONE', #127400, #133889, #91565, .T. ) ;
#92446 = DIRECTION ( 'NONE',  ( 0.7071067811865486830, -0.7071067811865464625, -0.000000000000000000 ) ) ;
#92447 = VECTOR ( 'NONE', #98361, 999.9999999999998863 ) ;
#92448 = ORIENTED_EDGE ( 'NONE', *, *, #107981, .T. ) ;
#92449 = VERTEX_POINT ( 'NONE', #104574 ) ;
#92450 = ORIENTED_EDGE ( 'NONE', *, *, #73282, .F. ) ;
#92451 = CARTESIAN_POINT ( 'NONE',  ( 48.56293019189809712, 1.637169565754157174, 6.110000000000002984 ) ) ;
#92452 = ORIENTED_EDGE ( 'NONE', *, *, #45048, .F. ) ;
#92453 = AXIS2_PLACEMENT_3D ( 'NONE', #83279, #82567, #106406 ) ;
#92454 = EDGE_CURVE ( 'NONE', #14410, #122126, #16860, .T. ) ;
#92455 = VECTOR ( 'NONE', #16922, 1000.000000000000227 ) ;
#92456 = CARTESIAN_POINT ( 'NONE',  ( 2.816639616203772789, -1.633150327867691987, -6.094999999999989093 ) ) ;
#92457 = CARTESIAN_POINT ( 'NONE',  ( -13.68197150847072230, 5.985828926257079630, -31.40491832948329787 ) ) ;
#92458 = VERTEX_POINT ( 'NONE', #105281 ) ;
#92459 = ADVANCED_FACE ( 'NONE', ( #93705 ), #103144, .F. ) ;
#92460 = DIRECTION ( 'NONE',  ( -1.000000000000000000, -1.224606353822377258E-16, -0.000000000000000000 ) ) ;
#92461 = EDGE_LOOP ( 'NONE', ( #77788, #83039, #129810, #1574 ) ) ;
#92462 = CARTESIAN_POINT ( 'NONE',  ( -60.29974487139158867, -27.71228299555248142, 4.000000000000000000 ) ) ;
#92463 = VECTOR ( 'NONE', #33899, 1000.000000000000000 ) ;
#92464 = VECTOR ( 'NONE', #56189, 1000.000000000000000 ) ;
#92465 = PLANE ( 'NONE',  #15072 ) ;
#92467 = ORIENTED_EDGE ( 'NONE', *, *, #16166, .F. ) ;
#92466 = LINE ( 'NONE', #133858, #14673 ) ;
#92468 = EDGE_LOOP ( 'NONE', ( #3715, #45091, #79296, #119605 ) ) ;
#92469 = CARTESIAN_POINT ( 'NONE',  ( -34.75611968250420603, -12.18706574529249842, 4.955485411084898040 ) ) ;
#92470 = CARTESIAN_POINT ( 'NONE',  ( -81.29974487139159578, -27.71228299555262709, 4.000000000000000000 ) ) ;
#92471 = ORIENTED_EDGE ( 'NONE', *, *, #103869, .T. ) ;
#92472 = AXIS2_PLACEMENT_3D ( 'NONE', #52629, #19994, #65713 ) ;
#92473 = CARTESIAN_POINT ( 'NONE',  ( -13.82816939922343202, -14.24070752338414003, 4.000000000000000000 ) ) ;
#92474 = ORIENTED_EDGE ( 'NONE', *, *, #73746, .T. ) ;
#92475 = VERTEX_POINT ( 'NONE', #27721 ) ;
#92476 = EDGE_CURVE ( 'NONE', #69904, #13983, #81433, .T. ) ;
#92477 = ORIENTED_EDGE ( 'NONE', *, *, #104390, .F. ) ;
#92478 = ORIENTED_EDGE ( 'NONE', *, *, #71175, .T. ) ;
#92479 = CARTESIAN_POINT ( 'NONE',  ( 184.1500000000000057, 26.96999999999993847, 34.92499999999998295 ) ) ;
#92480 = VECTOR ( 'NONE', #101688, 999.9999999999998863 ) ;
#92481 = VECTOR ( 'NONE', #101641, 1000.000000000000000 ) ;
#92482 = CARTESIAN_POINT ( 'NONE',  ( 9.792893218813395251, -2.240707523384257716, 5.000000000000000000 ) ) ;
#92483 = VECTOR ( 'NONE', #50826, 1000.000000000000000 ) ;
#92484 = DIRECTION ( 'NONE',  ( -1.000000000000000000, -1.224606353822377258E-16, -0.000000000000000000 ) ) ;
#92485 = EDGE_CURVE ( 'NONE', #116152, #46717, #137930, .T. ) ;
#92486 = DIRECTION ( 'NONE',  ( 0.000000000000000000, 0.000000000000000000, 1.000000000000000000 ) ) ;
#92487 = EDGE_CURVE ( 'NONE', #83102, #104888, #127771, .T. ) ;
#92488 = VECTOR ( 'NONE', #71356, 1000.000000000000000 ) ;
#92489 = FACE_OUTER_BOUND ( 'NONE', #120689, .T. ) ;
#92490 = ORIENTED_EDGE ( 'NONE', *, *, #78847, .F. ) ;
#92491 = VECTOR ( 'NONE', #61932, 1000.000000000000000 ) ;
#92492 = DIRECTION ( 'NONE',  ( 1.055184596092948005E-16, -1.000000000000000000, 0.000000000000000000 ) ) ;
#92493 = CARTESIAN_POINT ( 'NONE',  ( 18.79123647476855652, -9.717572351234235426E-16, -7.934999999999990727 ) ) ;
#92494 = CARTESIAN_POINT ( 'NONE',  ( 29.99999999999979750, -0.2811185226893990752, -5.995736974527582142 ) ) ;
#92495 = CARTESIAN_POINT ( 'NONE',  ( 95.79166666666665719, 3.975000000000003642, -6.884901960086285300 ) ) ;
#92496 = LINE ( 'NONE', #61370, #139256 ) ;
#92497 = VERTEX_POINT ( 'NONE', #108821 ) ;
#92498 = ORIENTED_EDGE ( 'NONE', *, *, #65123, .F. ) ;
#92499 = VERTEX_POINT ( 'NONE', #107424 ) ;
#92500 = PLANE ( 'NONE',  #18586 ) ;
#92501 = CARTESIAN_POINT ( 'NONE',  ( 17.85999999999999943, 9.521314400968980422E-16, 0.000000000000000000 ) ) ;
#92502 = VECTOR ( 'NONE', #12656, 999.9999999999998863 ) ;
#92503 = FACE_OUTER_BOUND ( 'NONE', #93547, .T. ) ;
#92504 = DIRECTION ( 'NONE',  ( -0.000000000000000000, 0.000000000000000000, 1.000000000000000000 ) ) ;
#92505 = CARTESIAN_POINT ( 'NONE',  ( 34.49999999999975842, -4.912538124160710673, 4.000000000000000000 ) ) ;
#92506 = CARTESIAN_POINT ( 'NONE',  ( 9.179067077831442489, 8.505508952922598453, 4.232065175675569613 ) ) ;
#92507 = EDGE_CURVE ( 'NONE', #110817, #35724, #75524, .T. ) ;
#92508 = CARTESIAN_POINT ( 'NONE',  ( 80.18749999999998579, -5.819803920172573974, 5.819803920172573086 ) ) ;
#92509 = CARTESIAN_POINT ( 'NONE',  ( 9.279999999999999361, 9.521314400968980422E-16, 0.000000000000000000 ) ) ;
#92510 = EDGE_CURVE ( 'NONE', #129125, #96996, #8083, .T. ) ;
#92511 = CARTESIAN_POINT ( 'NONE',  ( -65.99451991528749772, 28.92564299267984396, 4.000000000000000000 ) ) ;
#92512 = DIRECTION ( 'NONE',  ( -0.5735764363510507113, 0.8191520442889885789, 1.003171929053520926E-16 ) ) ;
#92513 = LINE ( 'NONE', #117127, #32587 ) ;
#92514 = VERTEX_POINT ( 'NONE', #21124 ) ;
#92515 = CARTESIAN_POINT ( 'NONE',  ( 4.499999999999967137, 12.43112307739206024, 4.000000000000000000 ) ) ;
#92516 = VERTEX_POINT ( 'NONE', #9507 ) ;
#92517 = DIRECTION ( 'NONE',  ( 0.000000000000000000, -0.3543493200069153248, -0.9351131265310291818 ) ) ;
#92519 = VERTEX_POINT ( 'NONE', #51639 ) ;
#92518 = CARTESIAN_POINT ( 'NONE',  ( 9.279999999999999361, 9.521314400968980422E-16, 0.000000000000000000 ) ) ;
#92520 = EDGE_CURVE ( 'NONE', #139777, #24725, #106685, .T. ) ;
#92521 = CARTESIAN_POINT ( 'NONE',  ( -36.29974487139159578, -27.71228299555231445, 4.000000000000000000 ) ) ;
#92522 = CARTESIAN_POINT ( 'NONE',  ( 24.09999999999999787, 2.055000000000001492, 0.000000000000000000 ) ) ;
#92523 = ORIENTED_EDGE ( 'NONE', *, *, #90770, .T. ) ;
#92524 = CARTESIAN_POINT ( 'NONE',  ( 13.49999999999990408, -5.568876922607754132, 4.000000000000000000 ) ) ;
#92525 = EDGE_LOOP ( 'NONE', ( #2702, #65255, #135617, #101090 ) ) ;
#92526 = ORIENTED_EDGE ( 'NONE', *, *, #66912, .F. ) ;
#92527 = LINE ( 'NONE', #80974, #126017 ) ;
#92528 = CARTESIAN_POINT ( 'NONE',  ( 100.1208603837962272, -6.884901960086286188, 3.974999999999997424 ) ) ;
#92529 = LINE ( 'NONE', #25868, #39411 ) ;
#92530 = CARTESIAN_POINT ( 'NONE',  ( 11.51078643762690490, -27.52281430457047406, 5.000000000000000000 ) ) ;
#92531 = ORIENTED_EDGE ( 'NONE', *, *, #142052, .F. ) ;
#92532 = CARTESIAN_POINT ( 'NONE',  ( 19.41972383043609440, -2.500000000000000444, 3.061616997868384127E-16 ) ) ;
#92533 = CARTESIAN_POINT ( 'NONE',  ( -0.1349957375162171014, 3.759292476615678336, 15.36553568819726223 ) ) ;
#92534 = CARTESIAN_POINT ( 'NONE',  ( 3.241694584251855193, 0.7592924766157104211, 14.37146558664982265 ) ) ;
#92535 = CARTESIAN_POINT ( 'NONE',  ( 21.14583333333333570, -1.633150327867689988, 6.094999999999989981 ) ) ;
#92536 = DIRECTION ( 'NONE',  ( -0.7071067811865486830, -0.7071067811865464625, 0.000000000000000000 ) ) ;
#92537 = PLANE ( 'NONE',  #53601 ) ;
#92538 = EDGE_LOOP ( 'NONE', ( #44850, #55229, #118576, #60038 ) ) ;
#92539 = CARTESIAN_POINT ( 'NONE',  ( 15.32816939922341426, -15.74070752338413470, 4.000000000000000000 ) ) ;
#92540 = VERTEX_POINT ( 'NONE', #52326 ) ;
#92541 = CARTESIAN_POINT ( 'NONE',  ( 93.04209685856476142, 5.291415217122923842, -3.054999999999996163 ) ) ;
#92542 = CARTESIAN_POINT ( 'NONE',  ( 0.000000000000000000, 0.000000000000000000, 5.000000000000000000 ) ) ;
#92543 = FACE_OUTER_BOUND ( 'NONE', #82643, .T. ) ;
#92544 = PLANE ( 'NONE',  #118730 ) ;
#92545 = LINE ( 'NONE', #62107, #24703 ) ;
#92546 = ORIENTED_EDGE ( 'NONE', *, *, #437, .T. ) ;
#92547 = CIRCLE ( 'NONE', #11499, 5.968999999999998529 ) ;
#92548 = VECTOR ( 'NONE', #53466, 1000.000000000000000 ) ;
#92549 = VECTOR ( 'NONE', #122000, 1000.000000000000114 ) ;
#92550 = DIRECTION ( 'NONE',  ( -0.000000000000000000, 0.3543493200069153248, 0.9351131265310292928 ) ) ;
#92551 = AXIS2_PLACEMENT_3D ( 'NONE', #43103, #22031, #109764 ) ;
#92552 = LINE ( 'NONE', #28042, #55762 ) ;
#92553 = EDGE_LOOP ( 'NONE', ( #49235, #3360, #85364, #137137 ) ) ;
#92554 = FACE_OUTER_BOUND ( 'NONE', #38599, .T. ) ;
#92555 = CARTESIAN_POINT ( 'NONE',  ( 14.48334561358944406, 22.22500000000000142, 4.500000000000000888 ) ) ;
#92557 = EDGE_LOOP ( 'NONE', ( #66999, #12764, #112083, #124221, #65391 ) ) ;
#92556 = DIRECTION ( 'NONE',  ( -0.3543493200069162685, -0.000000000000000000, -0.9351131265310288487 ) ) ;
#92558 = CARTESIAN_POINT ( 'NONE',  ( -34.92500000000001137, 21.72500000000000142, 5.000000000000000000 ) ) ;
#92559 = CARTESIAN_POINT ( 'NONE',  ( -34.75611968250421313, 2.812934254707341264, 4.955485411084894487 ) ) ;
#92560 = CARTESIAN_POINT ( 'NONE',  ( -34.92500000000001137, -20.99387692260785343, 4.000000000000000000 ) ) ;
#92561 = AXIS2_PLACEMENT_3D ( 'NONE', #93642, #6571, #137871 ) ;
#92562 = DIRECTION ( 'NONE',  ( -0.7071067811865486830, -0.7071067811865464625, 0.000000000000000000 ) ) ;
#92563 = ORIENTED_EDGE ( 'NONE', *, *, #64862, .F. ) ;
#92564 = ORIENTED_EDGE ( 'NONE', *, *, #49623, .F. ) ;
#92565 = ORIENTED_EDGE ( 'NONE', *, *, #49454, .F. ) ;
#92566 = EDGE_CURVE ( 'NONE', #125982, #132969, #45728, .T. ) ;
#92567 = CARTESIAN_POINT ( 'NONE',  ( 86.91709685856477563, 3.054999999999998828, 5.291415217122922066 ) ) ;
#92568 = ORIENTED_EDGE ( 'NONE', *, *, #72367, .F. ) ;
#92569 = ADVANCED_FACE ( 'NONE', ( #97985 ), #96514, .F. ) ;
#92570 = CARTESIAN_POINT ( 'NONE',  ( -42.48921356237308800, -27.52281430457085065, 5.000000000000000000 ) ) ;
#92571 = FACE_OUTER_BOUND ( 'NONE', #130113, .T. ) ;
#92572 = EDGE_CURVE ( 'NONE', #17308, #30830, #18237, .T. ) ;
#92573 = VECTOR ( 'NONE', #877, 1000.000000000000000 ) ;
#92574 = DIRECTION ( 'NONE',  ( 0.3543493200069162685, -0.000000000000000000, -0.9351131265310288487 ) ) ;
#92575 = DIRECTION ( 'NONE',  ( -0.7071067811865487940, 0.7071067811865463515, -0.000000000000000000 ) ) ;
#92576 = ORIENTED_EDGE ( 'NONE', *, *, #80238, .F. ) ;
#92577 = ADVANCED_FACE ( 'NONE', ( #85658 ), #120401, .F. ) ;
#92578 = FACE_OUTER_BOUND ( 'NONE', #63757, .T. ) ;
#92579 = CARTESIAN_POINT ( 'NONE',  ( 0.000000000000000000, -21.72500000000000142, 4.500000000000000888 ) ) ;
#92580 = VECTOR ( 'NONE', #44491, 1000.000000000000227 ) ;
#92581 = CARTESIAN_POINT ( 'NONE',  ( 74.28709685856478018, 3.054999999999997495, 5.291415217122919401 ) ) ;
#92582 = ORIENTED_EDGE ( 'NONE', *, *, #15629, .F. ) ;
#92583 = EDGE_CURVE ( 'NONE', #112964, #129502, #74834, .T. ) ;
#92584 = LINE ( 'NONE', #23791, #28130 ) ;
#92585 = CARTESIAN_POINT ( 'NONE',  ( 52.39921342269823867, -49.14999999999999147, -40.57473644908944266 ) ) ;
#92586 = FACE_OUTER_BOUND ( 'NONE', #116713, .T. ) ;
#92587 = VECTOR ( 'NONE', #68194, 1000.000000000000114 ) ;
#92588 = ORIENTED_EDGE ( 'NONE', *, *, #9826, .T. ) ;
#92589 = ORIENTED_EDGE ( 'NONE', *, *, #38511, .T. ) ;
#92590 = EDGE_CURVE ( 'NONE', #99775, #33858, #140081, .T. ) ;
#92591 = DIRECTION ( 'NONE',  ( -0.000000000000000000, 0.000000000000000000, 1.000000000000000000 ) ) ;
#92592 = ADVANCED_FACE ( 'NONE', ( #84962 ), #50920, .F. ) ;
#92593 = AXIS2_PLACEMENT_3D ( 'NONE', #123100, #110740, #3418 ) ;
#92594 = PLANE ( 'NONE',  #54712 ) ;
#92595 = DIRECTION ( 'NONE',  ( 0.7071067811865486830, -0.7071067811865464625, -0.000000000000000000 ) ) ;
#92596 = AXIS2_PLACEMENT_3D ( 'NONE', #9459, #73350, #65341 ) ;
#92597 = DIRECTION ( 'NONE',  ( 0.7071067811865486830, -0.7071067811865464625, -0.000000000000000000 ) ) ;
#92598 = ADVANCED_FACE ( 'NONE', ( #142225 ), #30606, .F. ) ;
#92599 = LINE ( 'NONE', #19862, #99832 ) ;
#92600 = CARTESIAN_POINT ( 'NONE',  ( -15.48921356237309510, -27.52281430457066236, 5.000000000000000000 ) ) ;
#92601 =( LENGTH_UNIT ( ) NAMED_UNIT ( * ) SI_UNIT ( .MILLI., .METRE. ) );
#92602 = AXIS2_PLACEMENT_3D ( 'NONE', #127034, #116173, #37183 ) ;
#92603 = ORIENTED_EDGE ( 'NONE', *, *, #33135, .T. ) ;
#92604 = ORIENTED_EDGE ( 'NONE', *, *, #55165, .F. ) ;
#92605 = MANIFOLD_SOLID_BREP ( '#37 (0.104) Diameter Hole1', #46449 ) ;
#92606 = CARTESIAN_POINT ( 'NONE',  ( 9.916666666666667851, 5.278424836066147208, 3.047499999999990550 ) ) ;
#92607 = ORIENTED_EDGE ( 'NONE', *, *, #93396, .F. ) ;
#92608 = AXIS2_PLACEMENT_3D ( 'NONE', #8182, #95934, #61232 ) ;
#92609 = PLANE ( 'NONE',  #133106 ) ;
#92610 = ORIENTED_EDGE ( 'NONE', *, *, #72877, .T. ) ;
#92611 = DIRECTION ( 'NONE',  ( 0.000000000000000000, 0.000000000000000000, 1.000000000000000000 ) ) ;
#92612 = LINE ( 'NONE', #68770, #140557 ) ;
#92613 = EDGE_CURVE ( 'NONE', #9860, #118163, #40068, .T. ) ;
#92614 = CARTESIAN_POINT ( 'NONE',  ( -34.75611968250421313, 17.81293425470718716, 4.955485411084894487 ) ) ;
#92615 = AXIS2_PLACEMENT_3D ( 'NONE', #121187, #100867, #134230 ) ;
#92616 = CARTESIAN_POINT ( 'NONE',  ( -20.51078643762690490, -27.52281430457041012, 5.000000000000000000 ) ) ;
#92617 = EDGE_LOOP ( 'NONE', ( #122425, #64461, #122427, #93404 ) ) ;
#92618 = DIRECTION ( 'NONE',  ( -0.6830127018922181881, 0.6830127018922202975, -0.2588190451025214056 ) ) ;
#92619 = CARTESIAN_POINT ( 'NONE',  ( 19.05000000000000071, 3.174999999999997158, 4.000000000000000000 ) ) ;
#92620 = ORIENTED_EDGE ( 'NONE', *, *, #8372, .F. ) ;
#92621 = FACE_OUTER_BOUND ( 'NONE', #45135, .T. ) ;
#92622 = ORIENTED_EDGE ( 'NONE', *, *, #92159, .F. ) ;
#92623 = ORIENTED_EDGE ( 'NONE', *, *, #5030, .T. ) ;
#92624 = CARTESIAN_POINT ( 'NONE',  ( -54.18398860626899705, 28.73617430169825226, 5.000000000000000000 ) ) ;
#92625 = ORIENTED_EDGE ( 'NONE', *, *, #59710, .T. ) ;
#92626 = EDGE_CURVE ( 'NONE', #15103, #131987, #35618, .T. ) ;
#92627 = EDGE_LOOP ( 'NONE', ( #1935, #40501, #103232, #82536 ) ) ;
#92628 = CARTESIAN_POINT ( 'NONE',  ( 72.47959685856477563, 6.109999999999999432, 1.637169565754164280 ) ) ;
#92630 = VERTEX_POINT ( 'NONE', #110963 ) ;
#92629 = AXIS2_PLACEMENT_3D ( 'NONE', #28737, #17813, #40338 ) ;
#92631 = CARTESIAN_POINT ( 'NONE',  ( 94.18750000000000000, -5.819803920172573974, 5.819803920172573086 ) ) ;
#92632 = PLANE ( 'NONE',  #17175 ) ;
#92633 = CARTESIAN_POINT ( 'NONE',  ( 110.1045968585647756, 1.637169565754164946, -6.109999999999999432 ) ) ;
#92634 = PLANE ( 'NONE',  #49532 ) ;
#92635 = ADVANCED_FACE ( 'NONE', ( #55200 ), #2188, .F. ) ;
#92636 = CARTESIAN_POINT ( 'NONE',  ( -7.940000000000001279, -60.26999999999998892, -10.00000000000000178 ) ) ;
#92637 = CARTESIAN_POINT ( 'NONE',  ( 13.49999999999990408, -19.53360074219754594, 5.000000000000000000 ) ) ;
#92638 = FACE_OUTER_BOUND ( 'NONE', #110913, .T. ) ;
#92639 = DIRECTION ( 'NONE',  ( -1.000000000000000000, -0.000000000000000000, -0.000000000000000000 ) ) ;
#92640 = PLANE ( 'NONE',  #9647 ) ;
#92641 = CARTESIAN_POINT ( 'NONE',  ( -31.49999999999977973, -10.53360074219763121, 5.000000000000000000 ) ) ;
#92643 = ORIENTED_EDGE ( 'NONE', *, *, #24785, .F. ) ;
#92642 = VECTOR ( 'NONE', #17931, 1000.000000000000000 ) ;
#92644 = DIRECTION ( 'NONE',  ( 0.7071067811865486830, -0.7071067811865464625, -0.000000000000000000 ) ) ;
#92645 = DIRECTION ( 'NONE',  ( -0.6830127018922180770, -0.6830127018922204085, -0.2588190451025213501 ) ) ;
#92646 = ADVANCED_FACE ( 'NONE', ( #23992 ), #111716, .T. ) ;
#92647 = ORIENTED_EDGE ( 'NONE', *, *, #34700, .F. ) ;
#92648 = ORIENTED_EDGE ( 'NONE', *, *, #252, .T. ) ;
#92649 = VECTOR ( 'NONE', #103805, 1000.000000000000000 ) ;
#92650 = CARTESIAN_POINT ( 'NONE',  ( 23.99999999999983302, -13.97847968911258221, -0.1324546996126253762 ) ) ;
#92651 = VECTOR ( 'NONE', #131914, 1000.000000000000227 ) ;
#92652 = VECTOR ( 'NONE', #100738, 1000.000000000000000 ) ;
#92653 = VERTEX_POINT ( 'NONE', #10240 ) ;
#92654 = AXIS2_PLACEMENT_3D ( 'NONE', #7247, #73975, #18859 ) ;
#92655 = AXIS2_PLACEMENT_3D ( 'NONE', #86074, #17238, #105647 ) ;
#92656 = LINE ( 'NONE', #58684, #23674 ) ;
#92657 = CARTESIAN_POINT ( 'NONE',  ( 113.5833333333333428, 6.884901960086290629, -3.974999999999994316 ) ) ;
#92658 = EDGE_CURVE ( 'NONE', #16399, #75683, #121843, .T. ) ;
#92659 = DIRECTION ( 'NONE',  ( 0.7071067811865487940, 0.7071067811865463515, 0.000000000000000000 ) ) ;
#92660 = CARTESIAN_POINT ( 'NONE',  ( 12.72281430457050710, -21.72500000000000142, 5.000000000000000000 ) ) ;
#92661 = VERTEX_POINT ( 'NONE', #12384 ) ;
#92663 = ORIENTED_EDGE ( 'NONE', *, *, #141272, .F. ) ;
#92662 = VECTOR ( 'NONE', #8708, 1000.000000000000000 ) ;
#92664 = FACE_OUTER_BOUND ( 'NONE', #59536, .T. ) ;
#92665 = CARTESIAN_POINT ( 'NONE',  ( 27.77540314143521982, -2.126176841940958351, -7.934999999999989839 ) ) ;
#92666 = CARTESIAN_POINT ( 'NONE',  ( 8.378320375002967779, -8.650595726116820927, 3.928333035411932794 ) ) ;
#92667 = CARTESIAN_POINT ( 'NONE',  ( 14.67075049121845431, -9.486428195927288698, -0.5820279030346748872 ) ) ;
#92668 = EDGE_LOOP ( 'NONE', ( #79178, #119860, #75133, #21686 ) ) ;
#92669 = ORIENTED_EDGE ( 'NONE', *, *, #45609, .T. ) ;
#92670 = EDGE_LOOP ( 'NONE', ( #87345, #85787, #85689, #131823 ) ) ;
#92672 = VECTOR ( 'NONE', #136963, 1000.000000000000000 ) ;
#92671 = PLANE ( 'NONE',  #116732 ) ;
#92673 = CARTESIAN_POINT ( 'NONE',  ( -20.29289321881331176, -3.740707523384246613, 5.000000000000000000 ) ) ;
#92674 = CARTESIAN_POINT ( 'NONE',  ( -2.999999999999981792, -8.151047557385073361, -8.977947279169791628 ) ) ;
#92675 = CARTESIAN_POINT ( 'NONE',  ( 3.328169399223507519, -3.740707523384244837, 4.000000000000000000 ) ) ;
#92676 = ORIENTED_EDGE ( 'NONE', *, *, #41601, .F. ) ;
#92677 = LINE ( 'NONE', #49222, #136552 ) ;
#92678 = PLANE ( 'NONE',  #38823 ) ;
#92679 = CIRCLE ( 'NONE', #32590, 2.055000000000000604 ) ;
#92680 = VECTOR ( 'NONE', #46523, 1000.000000000000000 ) ;
#92681 = CARTESIAN_POINT ( 'NONE',  ( -33.18398860626899705, 28.73617430169810305, 5.000000000000000000 ) ) ;
#92682 = ADVANCED_FACE ( 'NONE', ( #45074 ), #79123, .T. ) ;
#92683 = LINE ( 'NONE', #57974, #44269 ) ;
#92684 = DIRECTION ( 'NONE',  ( 0.7071067811865486830, -0.7071067811865464625, -0.000000000000000000 ) ) ;
#92685 = AXIS2_PLACEMENT_3D ( 'NONE', #122135, #22796, #11207 ) ;
#92686 = EDGE_LOOP ( 'NONE', ( #114901, #60357, #68877, #45531 ) ) ;
#92687 = CARTESIAN_POINT ( 'NONE',  ( 1.499999999999991784, 15.43112307739202471, 4.000000000000000000 ) ) ;
#92689 = CIRCLE ( 'NONE', #111210, 2.999999999999997335 ) ;
#92688 = DIRECTION ( 'NONE',  ( -0.6830127018922181881, 0.6830127018922202975, -0.2588190451025214056 ) ) ;
#92690 = ORIENTED_EDGE ( 'NONE', *, *, #6261, .F. ) ;
#92691 = CARTESIAN_POINT ( 'NONE',  ( -24.79289321881327979, -20.24070752338407431, 5.000000000000000000 ) ) ;
#92692 = EDGE_CURVE ( 'NONE', #36317, #125403, #132054, .T. ) ;
#92694 = ORIENTED_EDGE ( 'NONE', *, *, #63536, .T. ) ;
#92693 = PLANE ( 'NONE',  #20839 ) ;
#92695 = EDGE_LOOP ( 'NONE', ( #89159, #84456, #21590, #13310, #74282 ) ) ;
#92696 = AXIS2_PLACEMENT_3D ( 'NONE', #42626, #120115, #20824 ) ;
#92697 = EDGE_CURVE ( 'NONE', #72213, #134483, #132786, .T. ) ;
#92698 = DIRECTION ( 'NONE',  ( -0.7071067811865486830, -0.7071067811865464625, -0.000000000000000000 ) ) ;
#92699 = DIRECTION ( 'NONE',  ( -0.000000000000000000, -0.3543493200069152693, 0.9351131265310292928 ) ) ;
#92700 = CARTESIAN_POINT ( 'NONE',  ( 104.3958333333333286, -2.130196079827389344, 7.950000000000021494 ) ) ;
#92701 = VERTEX_POINT ( 'NONE', #34886 ) ;
#92702 = LINE ( 'NONE', #105008, #72124 ) ;
#92703 = ORIENTED_EDGE ( 'NONE', *, *, #28888, .T. ) ;
#92704 = CARTESIAN_POINT ( 'NONE',  ( 47.99451991528749062, 28.92564299267971251, 4.000000000000000000 ) ) ;
#92705 = LINE ( 'NONE', #112342, #60161 ) ;
#92706 = CARTESIAN_POINT ( 'NONE',  ( 28.34959685856477662, 6.109999999999997655, 1.637169565754163836 ) ) ;
#92707 = DIRECTION ( 'NONE',  ( -0.000000000000000000, 0.000000000000000000, 1.000000000000000000 ) ) ;
#92708 = VECTOR ( 'NONE', #91806, 1000.000000000000000 ) ;
#92709 = FACE_OUTER_BOUND ( 'NONE', #113096, .T. ) ;
#92710 = PLANE ( 'NONE',  #21328 ) ;
#92711 = DIRECTION ( 'NONE',  ( 0.000000000000000000, 0.000000000000000000, 1.000000000000000000 ) ) ;
#92712 = CARTESIAN_POINT ( 'NONE',  ( 27.32816939922333432, -15.74070752338412760, 4.000000000000000000 ) ) ;
#92714 = VECTOR ( 'NONE', #30342, 1000.000000000000000 ) ;
#92713 = CARTESIAN_POINT ( 'NONE',  ( 32.79123647476855297, -9.717572351234235426E-16, -7.934999999999990727 ) ) ;
#92715 = CARTESIAN_POINT ( 'NONE',  ( 8.145403141435220817, -2.126176841940958351, -7.934999999999988951 ) ) ;
#92716 = LINE ( 'NONE', #60866, #8830 ) ;
#92717 = CARTESIAN_POINT ( 'NONE',  ( -24.79289321881328334, -14.24070752338413648, 5.000000000000000000 ) ) ;
#92718 = CARTESIAN_POINT ( 'NONE',  ( -27.18398860626900060, 28.73617430169806042, 5.000000000000000000 ) ) ;
#92719 = ORIENTED_EDGE ( 'NONE', *, *, #59603, .F. ) ;
#92720 = EDGE_CURVE ( 'NONE', #80031, #38512, #77673, .T. ) ;
#92721 = ORIENTED_EDGE ( 'NONE', *, *, #110071, .T. ) ;
#92722 = CARTESIAN_POINT ( 'NONE',  ( 96.22916666666667140, 7.950000000000001954, -2.130196079827421762 ) ) ;
#92723 = VERTEX_POINT ( 'NONE', #89248 ) ;
#92724 = VERTEX_POINT ( 'NONE', #66086 ) ;
#92725 = LINE ( 'NONE', #84044, #66587 ) ;
#92726 = LINE ( 'NONE', #102918, #115832 ) ;
#92727 = VECTOR ( 'NONE', #50779, 1000.000000000000000 ) ;
#92728 = CARTESIAN_POINT ( 'NONE',  ( 14.55667305106308973, 9.434713282303595960, 1.148153153331950227 ) ) ;
#92729 = ORIENTED_EDGE ( 'NONE', *, *, #43848, .T. ) ;
#92730 = CARTESIAN_POINT ( 'NONE',  ( 19.73159235450332005, 9.902892378096218942E-16, 0.000000000000000000 ) ) ;
#92731 = DIRECTION ( 'NONE',  ( 0.7071067811865487940, 0.7071067811865463515, 0.000000000000000000 ) ) ;
#92732 = FACE_OUTER_BOUND ( 'NONE', #12962, .T. ) ;
#92733 = CARTESIAN_POINT ( 'NONE',  ( 125.6578181545542918, -1.266560775613104317, -7.692714378292049737 ) ) ;
#92734 = DIRECTION ( 'NONE',  ( -0.6830127018922181881, 0.6830127018922202975, -0.2588190451025214056 ) ) ;
#92735 = CARTESIAN_POINT ( 'NONE',  ( 1.179999999999999272, 10.00000000000000178, 6.750000000000000888 ) ) ;
#92736 = FACE_OUTER_BOUND ( 'NONE', #65004, .T. ) ;
#92737 = DIRECTION ( 'NONE',  ( -0.7071067811865486830, -0.7071067811865464625, 0.000000000000000000 ) ) ;
#92738 = VECTOR ( 'NONE', #103932, 1000.000000000000000 ) ;
#92739 = CARTESIAN_POINT ( 'NONE',  ( 14.20710678118644665, -17.24070752338410628, 5.000000000000000000 ) ) ;
#92740 = DIRECTION ( 'NONE',  ( -0.7071067811865486830, -0.7071067811865464625, 0.000000000000000000 ) ) ;
#92741 = FACE_OUTER_BOUND ( 'NONE', #124333, .T. ) ;
#92742 = DIRECTION ( 'NONE',  ( -0.000000000000000000, 0.000000000000000000, 1.000000000000000000 ) ) ;
#92743 = EDGE_LOOP ( 'NONE', ( #44814, #134756, #492, #133386 ) ) ;
#92744 = ORIENTED_EDGE ( 'NONE', *, *, #103378, .F. ) ;
#92745 = ADVANCED_FACE ( 'NONE', ( #121145 ), #133474, .T. ) ;
#92746 = CARTESIAN_POINT ( 'NONE',  ( 108.6462635252314186, -4.472830434245840259, 4.472830434245839371 ) ) ;
#92747 = VERTEX_POINT ( 'NONE', #90694 ) ;
#92748 = EDGE_CURVE ( 'NONE', #58595, #138592, #24879, .T. ) ;
#92749 = LINE ( 'NONE', #84068, #61726 ) ;
#92750 = LINE ( 'NONE', #2895, #64253 ) ;
#92751 = ORIENTED_EDGE ( 'NONE', *, *, #67634, .F. ) ;
#92752 = EDGE_CURVE ( 'NONE', #83776, #63645, #78379, .T. ) ;
#92753 = EDGE_CURVE ( 'NONE', #82669, #127957, #68253, .T. ) ;
#92754 = CARTESIAN_POINT ( 'NONE',  ( 19.58200623001875940, 0.000000000000000000, 2.500000000000000444 ) ) ;
#92756 =( BOUNDED_CURVE ( )  B_SPLINE_CURVE ( 3, ( #17759, #16326, #92469, #27221 ),
 .UNSPECIFIED., .F., .F. ) 
 B_SPLINE_CURVE_WITH_KNOTS ( ( 4, 4 ),
 ( 2.779374508378135378, 4.199602562396853145 ),
 .UNSPECIFIED. ) 
 CURVE ( )  GEOMETRIC_REPRESENTATION_ITEM ( )  RATIONAL_B_SPLINE_CURVE ( ( 1.000000000000000000, 0.8388583629366597183, 0.8388583629366597183, 1.000000000000000000 ) ) 
 REPRESENTATION_ITEM ( '' )  );
#92755 = FACE_OUTER_BOUND ( 'NONE', #132858, .T. ) ;
#92757 = VECTOR ( 'NONE', #105108, 1000.000000000000000 ) ;
#92758 = AXIS2_PLACEMENT_3D ( 'NONE', #126460, #104719, #27156 ) ;
#92759 = CARTESIAN_POINT ( 'NONE',  ( 104.7662635252314516, 4.472830434245839371, -4.472830434245838482 ) ) ;
#92760 = ORIENTED_EDGE ( 'NONE', *, *, #57594, .T. ) ;
#92761 = ORIENTED_EDGE ( 'NONE', *, *, #52644, .T. ) ;
#92762 = DIRECTION ( 'NONE',  ( 0.7071067811865486830, -0.7071067811865464625, -0.000000000000000000 ) ) ;
#92763 = VECTOR ( 'NONE', #103892, 1000.000000000000000 ) ;
#92764 = VECTOR ( 'NONE', #124453, 1000.000000000000000 ) ;
#92765 = AXIS2_PLACEMENT_3D ( 'NONE', #47802, #4182, #70284 ) ;
#92766 = CARTESIAN_POINT ( 'NONE',  ( -30.79289321881323360, 12.75929247661558463, 5.000000000000000000 ) ) ;
#92767 =( BOUNDED_CURVE ( )  B_SPLINE_CURVE ( 2, ( #54862, #43976, #95653, #63771, #88196, #28279, #105794, #10595, #84113, #40588, #132447, #96337, #121507 ),
 .UNSPECIFIED., .F., .T. ) 
 B_SPLINE_CURVE_WITH_KNOTS ( ( 3, 2, 2, 2, 2, 2, 3 ),
 ( 0.8500000000000000888, 0.8527777777777778567, 0.8555555555555556246, 0.8583333333333333925, 0.8611111111111112715, 0.8638888888888890394, 0.8666666666666668073 ),
 .UNSPECIFIED. ) 
 CURVE ( )  GEOMETRIC_REPRESENTATION_ITEM ( )  RATIONAL_B_SPLINE_CURVE ( ( 0.9999999999999986677, 0.9659258262890696445, 1.000000000000000000, 0.9659258262890683122, 1.000000000000000000, 0.9659258262890683122, 1.000000000000000000, 0.9659258262890683122, 1.000000000000000000, 0.9659258262890683122, 1.000000000000000000, 0.9659258262890669799, 1.000000000000001332 ) ) 
 REPRESENTATION_ITEM ( '' )  );
#92768 = AXIS2_PLACEMENT_3D ( 'NONE', #1857, #47603, #35290 ) ;
#92769 = ORIENTED_EDGE ( 'NONE', *, *, #42727, .T. ) ;
#92770 = EDGE_LOOP ( 'NONE', ( #88023, #29229, #94540, #93857 ) ) ;
#92771 = EDGE_CURVE ( 'NONE', #7159, #78369, #33472, .T. ) ;
#92772 = ORIENTED_EDGE ( 'NONE', *, *, #45649, .T. ) ;
#92773 = FACE_OUTER_BOUND ( 'NONE', #12940, .T. ) ;
#92774 = ADVANCED_FACE ( 'NONE', ( #109565 ), #54501, .F. ) ;
#92775 = CARTESIAN_POINT ( 'NONE',  ( 0.3587364747685527488, 5.808823158059031044, -5.808823158059037262 ) ) ;
#92776 = VECTOR ( 'NONE', #129643, 1000.000000000000000 ) ;
#92777 = EDGE_CURVE ( 'NONE', #86782, #114073, #10979, .T. ) ;
#92778 = ORIENTED_EDGE ( 'NONE', *, *, #38022, .T. ) ;
#92779 = VERTEX_POINT ( 'NONE', #81976 ) ;
#92780 = VECTOR ( 'NONE', #2926, 999.9999999999998863 ) ;
#92781 = DIRECTION ( 'NONE',  ( -0.000000000000000000, 0.3543493200069153248, 0.9351131265310292928 ) ) ;
#92782 = ORIENTED_EDGE ( 'NONE', *, *, #43142, .F. ) ;
#92783 = ORIENTED_EDGE ( 'NONE', *, *, #101437, .T. ) ;
#92784 = AXIS2_PLACEMENT_3D ( 'NONE', #108533, #18686, #74544 ) ;
#92785 = EDGE_CURVE ( 'NONE', #134614, #66046, #36300, .T. ) ;
#92786 = DIRECTION ( 'NONE',  ( 0.6830127018922181881, 0.6830127018922202975, -0.2588190451025214056 ) ) ;
#92787 = AXIS2_PLACEMENT_3D ( 'NONE', #118251, #29822, #97957 ) ;
#92788 = VECTOR ( 'NONE', #115545, 1000.000000000000227 ) ;
#92789 = DIRECTION ( 'NONE',  ( 0.3543493200069162685, -0.000000000000000000, -0.9351131265310288487 ) ) ;
#92790 = EDGE_LOOP ( 'NONE', ( #26866, #137714, #82627, #101381 ) ) ;
#92791 = DIRECTION ( 'NONE',  ( 0.3543493200069162685, -0.000000000000000000, -0.9351131265310288487 ) ) ;
#92792 = VECTOR ( 'NONE', #76916, 1000.000000000000000 ) ;
#92793 = CARTESIAN_POINT ( 'NONE',  ( -23.21837311707488993, 21.74787736706806029, 4.999607392498049308 ) ) ;
#92794 = EDGE_CURVE ( 'NONE', #130142, #110486, #105112, .T. ) ;
#92795 = PLANE ( 'NONE',  #46043 ) ;
#92796 = VECTOR ( 'NONE', #90785, 1000.000000000000000 ) ;
#92797 = DIRECTION ( 'NONE',  ( -0.7071067811865487940, 0.7071067811865463515, -0.000000000000000000 ) ) ;
#92798 = DIRECTION ( 'NONE',  ( -1.000000000000000000, -1.224606353822377258E-16, -0.000000000000000000 ) ) ;
#92799 = FACE_BOUND ( 'NONE', #48866, .T. ) ;
#92800 = ORIENTED_EDGE ( 'NONE', *, *, #25058, .F. ) ;
#92801 = CARTESIAN_POINT ( 'NONE',  ( -3.005480084712505828, 28.92564299267936079, 4.000000000000000000 ) ) ;
#92802 = CARTESIAN_POINT ( 'NONE',  ( 47.99451991528749062, 28.92564299267971251, 4.000000000000000000 ) ) ;
#92803 = COLOUR_RGB ( '', 0.08235294, 0.09019608, 0.10196078) ;
#92804 = CARTESIAN_POINT ( 'NONE',  ( 27.99999999999999645, -49.14999999999999147, -49.92499999999968452 ) ) ;
#92805 = ORIENTED_EDGE ( 'NONE', *, *, #52842, .F. ) ;
#92806 = EDGE_CURVE ( 'NONE', #24327, #49400, #2937, .T. ) ;
#92807 = LINE ( 'NONE', #68953, #131618 ) ;
#92808 = ORIENTED_EDGE ( 'NONE', *, *, #138854, .F. ) ;
#92809 = ORIENTED_EDGE ( 'NONE', *, *, #132739, .T. ) ;
#92810 = ORIENTED_EDGE ( 'NONE', *, *, #133117, .T. ) ;
#92811 = EDGE_CURVE ( 'NONE', #104032, #106976, #115966, .T. ) ;
#92812 = CARTESIAN_POINT ( 'NONE',  ( 36.80793019189809456, -6.109999999999998543, 1.637169565754158507 ) ) ;
#92813 = ORIENTED_EDGE ( 'NONE', *, *, #100813, .T. ) ;
#92814 = AXIS2_PLACEMENT_3D ( 'NONE', #60757, #38251, #115756 ) ;
#92815 = DIRECTION ( 'NONE',  ( -0.7071067811865486830, -0.7071067811865464625, 0.000000000000000000 ) ) ;
#92816 = DIRECTION ( 'NONE',  ( -0.7071067811865486830, 0.7071067811865464625, 0.000000000000000000 ) ) ;
#92817 = DIRECTION ( 'NONE',  ( -0.6830127018922180770, -0.6830127018922204085, -0.2588190451025213501 ) ) ;
#92818 = ORIENTED_EDGE ( 'NONE', *, *, #42046, .T. ) ;
#92819 = CARTESIAN_POINT ( 'NONE',  ( -25.39999999999996305, 0.000000000000000000, 2.500000000000000000 ) ) ;
#92821 = DIRECTION ( 'NONE',  ( 0.6830127018922180770, -0.6830127018922204085, -0.2588190451025213501 ) ) ;
#92820 = VECTOR ( 'NONE', #551, 1000.000000000000000 ) ;
#92822 = CIRCLE ( 'NONE', #111339, 2.500000000000000888 ) ;
#92823 = DIRECTION ( 'NONE',  ( 0.7071067811865487940, 0.7071067811865463515, -0.000000000000000000 ) ) ;
#92824 = CARTESIAN_POINT ( 'NONE',  ( 2.999999999999983569, 19.93112307739198030, 4.000000000000000000 ) ) ;
#92825 = DIRECTION ( 'NONE',  ( 0.7071067811865487940, 0.7071067811865463515, 0.000000000000000000 ) ) ;
#92826 = DIRECTION ( 'NONE',  ( 0.6830127018922181881, 0.6830127018922202975, -0.2588190451025214056 ) ) ;
#92827 = LINE ( 'NONE', #50762, #61048 ) ;
#92828 = VERTEX_POINT ( 'NONE', #94229 ) ;
#92829 = VERTEX_POINT ( 'NONE', #59498 ) ;
#92830 = ORIENTED_EDGE ( 'NONE', *, *, #53984, .T. ) ;
#92831 = VECTOR ( 'NONE', #26541, 1000.000000000000000 ) ;
#92832 = VERTEX_POINT ( 'NONE', #36994 ) ;
#92833 = DIRECTION ( 'NONE',  ( -0.5735764363510499342, -0.8191520442889891340, 0.000000000000000000 ) ) ;
#92834 = EDGE_LOOP ( 'NONE', ( #44975, #26938, #74656, #112324 ) ) ;
#92835 = ORIENTED_EDGE ( 'NONE', *, *, #70653, .T. ) ;
#92836 = DIRECTION ( 'NONE',  ( 0.7071067811865487940, 0.7071067811865463515, 0.000000000000000000 ) ) ;
#92837 = DIRECTION ( 'NONE',  ( 0.6830127018922180770, -0.6830127018922204085, -0.2588190451025213501 ) ) ;
#92838 = CARTESIAN_POINT ( 'NONE',  ( 48.18398860626899705, 28.73617430169820608, 5.000000000000000000 ) ) ;
#92839 = EDGE_LOOP ( 'NONE', ( #137823, #60895, #5382, #9544, #89101, #91292 ) ) ;
#92840 = CARTESIAN_POINT ( 'NONE',  ( -25.39999999999996305, 0.000000000000000000, 2.500000000000000000 ) ) ;
#92841 = CIRCLE ( 'NONE', #35042, 1.142820323027524232 ) ;
#92842 = ORIENTED_EDGE ( 'NONE', *, *, #115303, .F. ) ;
#92843 = CARTESIAN_POINT ( 'NONE',  ( -60.48921356237309510, -27.52281430457097500, 5.000000000000000000 ) ) ;
#92844 = LINE ( 'NONE', #47957, #19538 ) ;
#92845 = CARTESIAN_POINT ( 'NONE',  ( 0.3587364747685527488, 5.808823158059031044, -5.808823158059038150 ) ) ;
#92846 = ORIENTED_EDGE ( 'NONE', *, *, #109766, .F. ) ;
#92847 = CARTESIAN_POINT ( 'NONE',  ( 97.03709685856479439, -3.054999999999999272, -5.291415217122919401 ) ) ;
#92848 = LINE ( 'NONE', #4349, #18879 ) ;
#92849 = FACE_OUTER_BOUND ( 'NONE', #50720, .T. ) ;
#92850 = EDGE_CURVE ( 'NONE', #77053, #67112, #70404, .T. ) ;
#92851 = ORIENTED_EDGE ( 'NONE', *, *, #102761, .T. ) ;
#92852 = ORIENTED_EDGE ( 'NONE', *, *, #18812, .F. ) ;
#92853 = SURFACE_SIDE_STYLE ('',( #28337 ) ) ;
#92854 = ORIENTED_EDGE ( 'NONE', *, *, #30229, .F. ) ;
#92855 = LINE ( 'NONE', #124779, #115784 ) ;
#92856 =( NAMED_UNIT ( * ) SI_UNIT ( $, .STERADIAN. ) SOLID_ANGLE_UNIT ( ) );
#92857 = VECTOR ( 'NONE', #48652, 1000.000000000000227 ) ;
#92858 = LINE ( 'NONE', #80589, #60937 ) ;
#92859 = ORIENTED_EDGE ( 'NONE', *, *, #17173, .F. ) ;
#92860 = VECTOR ( 'NONE', #69311, 999.9999999999998863 ) ;
#92861 = DIRECTION ( 'NONE',  ( -1.451651444332056451E-15, -1.000000000000000000, 0.000000000000000000 ) ) ;
#92862 = VECTOR ( 'NONE', #48764, 1000.000000000000000 ) ;
#92863 = CARTESIAN_POINT ( 'NONE',  ( -20.99999999999984723, -8.731860332648860634, -2.120594902707586549 ) ) ;
#92864 = LINE ( 'NONE', #137102, #81592 ) ;
#92865 = ORIENTED_EDGE ( 'NONE', *, *, #134840, .F. ) ;
#92866 = DIRECTION ( 'NONE',  ( -0.7071067811865486830, -0.7071067811865464625, 0.000000000000000000 ) ) ;
#92867 = STYLED_ITEM ( 'NONE', ( #103041 ), #72019 ) ;
#92868 = VECTOR ( 'NONE', #69210, 1000.000000000000227 ) ;
#92869 = AXIS2_PLACEMENT_3D ( 'NONE', #71160, #27620, #72618 ) ;
#92870 = AXIS2_PLACEMENT_3D ( 'NONE', #94886, #84073, #73186 ) ;
#92871 = CARTESIAN_POINT ( 'NONE',  ( 8.671830600776420539, 17.25929247661555266, 4.000000000000000000 ) ) ;
#92873 = ORIENTED_EDGE ( 'NONE', *, *, #84605, .T. ) ;
#92872 = VECTOR ( 'NONE', #32059, 1000.000000000000000 ) ;
#92874 = ADVANCED_FACE ( 'NONE', ( #125452 ), #82663, .F. ) ;
#92876 = ORIENTED_EDGE ( 'NONE', *, *, #108484, .F. ) ;
#92875 = DIRECTION ( 'NONE',  ( 0.6830127018922181881, 0.6830127018922202975, -0.2588190451025214056 ) ) ;
#92878 = ORIENTED_EDGE ( 'NONE', *, *, #82850, .F. ) ;
#92877 = ADVANCED_FACE ( 'NONE', ( #138469 ), #71085, .F. ) ;
#92879 = CARTESIAN_POINT ( 'NONE',  ( -15.90492180865371274, 6.766090994904859102, -28.60278292646719933 ) ) ;
#92880 = AXIS2_PLACEMENT_3D ( 'NONE', #82967, #4609, #125031 ) ;
#92881 = LINE ( 'NONE', #71879, #106224 ) ;
#92882 = EDGE_LOOP ( 'NONE', ( #38184, #63918, #114909, #3929 ) ) ;
#92883 = LINE ( 'NONE', #18889, #69736 ) ;
#92884 = FACE_OUTER_BOUND ( 'NONE', #25237, .T. ) ;
#92885 = CARTESIAN_POINT ( 'NONE',  ( 25.19159235450331735, 3.061616997868380183E-16, -2.500000000000001332 ) ) ;
#92886 = EDGE_LOOP ( 'NONE', ( #134335, #125232, #114586, #25935, #58456, #136278 ) ) ;
#92887 = EDGE_CURVE ( 'NONE', #28959, #141805, #39154, .T. ) ;
#92888 = VECTOR ( 'NONE', #89593, 1000.000000000000000 ) ;
#92889 = LINE ( 'NONE', #82060, #43886 ) ;
#92890 = DIRECTION ( 'NONE',  ( -0.6830127018922180770, -0.6830127018922204085, -0.2588190451025213501 ) ) ;
#92891 = PLANE ( 'NONE',  #37489 ) ;
#92892 = PLANE ( 'NONE',  #79491 ) ;
#92893 = DIRECTION ( 'NONE',  ( -0.7071067811865486830, -0.7071067811865464625, 0.000000000000000000 ) ) ;
#92894 = CARTESIAN_POINT ( 'NONE',  ( 7.499999999999951150, 16.18958161055403622, -11.56426086740809644 ) ) ;
#92895 = DIRECTION ( 'NONE',  ( 1.000000000000000000, -0.000000000000000000, -0.000000000000000000 ) ) ;
#92896 = LINE ( 'NONE', #92169, #66243 ) ;
#92897 = ORIENTED_EDGE ( 'NONE', *, *, #45482, .T. ) ;
#92898 = ADVANCED_FACE ( 'NONE', ( #26136 ), #69666, .F. ) ;
#92899 = AXIS2_PLACEMENT_3D ( 'NONE', #135100, #57527, #93702 ) ;
#92900 = ORIENTED_EDGE ( 'NONE', *, *, #139148, .F. ) ;
#92901 = ORIENTED_EDGE ( 'NONE', *, *, #19200, .F. ) ;
#92902 = CARTESIAN_POINT ( 'NONE',  ( 124.6666666666666572, 6.884901960086285300, 3.975000000000003642 ) ) ;
#92903 = VECTOR ( 'NONE', #40553, 1000.000000000000000 ) ;
#92904 = ORIENTED_EDGE ( 'NONE', *, *, #69261, .F. ) ;
#92905 = VERTEX_POINT ( 'NONE', #103653 ) ;
#92906 = AXIS2_PLACEMENT_3D ( 'NONE', #88215, #33841, #20064 ) ;
#92907 = VERTEX_POINT ( 'NONE', #91405 ) ;
#92908 = DIRECTION ( 'NONE',  ( 0.7071067811865487940, -0.7071067811865463515, 0.000000000000000000 ) ) ;
#92909 = DIRECTION ( 'NONE',  ( 0.3543493200069162685, -0.000000000000000000, -0.9351131265310288487 ) ) ;
#92910 = EDGE_CURVE ( 'NONE', #134985, #49111, #4297, .T. ) ;
#92911 = EDGE_CURVE ( 'NONE', #31004, #42434, #5046, .T. ) ;
#92912 = CIRCLE ( 'NONE', #46720, 2.500000000000000444 ) ;
#92913 = EDGE_LOOP ( 'NONE', ( #86619, #30404, #42544, #68432 ) ) ;
#92914 = CARTESIAN_POINT ( 'NONE',  ( 45.48921356237309510, -27.52281430457087197, 5.000000000000000000 ) ) ;
#92915 = FACE_OUTER_BOUND ( 'NONE', #90902, .T. ) ;
#92916 = DIRECTION ( 'NONE',  ( 0.7071067811865487940, 0.7071067811865463515, 0.000000000000000000 ) ) ;
#92917 = CARTESIAN_POINT ( 'NONE',  ( 112.5837635252314470, -6.110000000000001208, -3.741295971395164515E-16 ) ) ;
#92918 = AXIS2_PLACEMENT_3D ( 'NONE', #40342, #18523, #130194 ) ;
#92919 = ORIENTED_EDGE ( 'NONE', *, *, #103131, .F. ) ;
#92920 = LINE ( 'NONE', #50147, #83523 ) ;
#92921 = CARTESIAN_POINT ( 'NONE',  ( 27.18398860626900060, 28.73617430169806042, 5.000000000000000000 ) ) ;
#92922 = DIRECTION ( 'NONE',  ( -1.000000000000000000, 0.000000000000000000, 0.000000000000000000 ) ) ;
#92923 = DIRECTION ( 'NONE',  ( -0.6830127018922181881, 0.6830127018922202975, -0.2588190451025214056 ) ) ;
#92924 = CARTESIAN_POINT ( 'NONE',  ( 8.999999999999937828, 1.761378380278691314, -6.096875308897234724 ) ) ;
#92925 = CARTESIAN_POINT ( 'NONE',  ( 37.41252705046288440, -7.949999999999998401, -4.867971026610728450E-16 ) ) ;
#92926 = LINE ( 'NONE', #116097, #39860 ) ;
#92927 = PLANE ( 'NONE',  #18364 ) ;
#92928 = AXIS2_PLACEMENT_3D ( 'NONE', #78726, #46117, #112768 ) ;
#92929 = ORIENTED_EDGE ( 'NONE', *, *, #85407, .T. ) ;
#92930 = VERTEX_POINT ( 'NONE', #137033 ) ;
#92931 = CARTESIAN_POINT ( 'NONE',  ( 36.72916666666666430, 7.950000000000001954, -2.130196079827421762 ) ) ;
#92932 = ORIENTED_EDGE ( 'NONE', *, *, #42522, .F. ) ;
#92933 = ORIENTED_EDGE ( 'NONE', *, *, #45139, .T. ) ;
#92934 = CARTESIAN_POINT ( 'NONE',  ( -14.99451991528749595, 28.92564299267948513, 4.000000000000000000 ) ) ;
#92935 = EDGE_CURVE ( 'NONE', #90062, #116147, #104635, .T. ) ;
#92936 = VECTOR ( 'NONE', #10894, 1000.000000000000227 ) ;
#92937 = DIRECTION ( 'NONE',  ( -0.7071067811865486830, -0.7071067811865464625, 0.000000000000000000 ) ) ;
#92938 = VERTEX_POINT ( 'NONE', #14541 ) ;
#92939 = AXIS2_PLACEMENT_3D ( 'NONE', #113554, #83655, #57795 ) ;
#92940 = LINE ( 'NONE', #13213, #75643 ) ;
#92942 = EDGE_CURVE ( 'NONE', #116108, #93902, #97803, .T. ) ;
#92941 = CARTESIAN_POINT ( 'NONE',  ( 33.18398860626899705, 28.73617430169810305, 5.000000000000000000 ) ) ;
#92943 = EDGE_CURVE ( 'NONE', #21885, #139855, #107246, .T. ) ;
#92944 = FACE_OUTER_BOUND ( 'NONE', #90301, .T. ) ;
#92945 = CARTESIAN_POINT ( 'NONE',  ( 32.52126352523142572, -4.472830434245839371, -4.472830434245840259 ) ) ;
#92946 = EDGE_LOOP ( 'NONE', ( #21977, #31944, #15693, #62315 ) ) ;
#92947 = DIRECTION ( 'NONE',  ( -0.7071067811865486830, -0.7071067811865464625, 0.000000000000000000 ) ) ;
#92948 = ORIENTED_EDGE ( 'NONE', *, *, #108009, .F. ) ;
#92949 = AXIS2_PLACEMENT_3D ( 'NONE', #117457, #97880, #21011 ) ;
#92950 = DIRECTION ( 'NONE',  ( -0.000000000000000000, -0.000000000000000000, -1.000000000000000000 ) ) ;
#92951 = EDGE_CURVE ( 'NONE', #143112, #121799, #7190, .T. ) ;
#92952 = LINE ( 'NONE', #16824, #105512 ) ;
#92953 = LINE ( 'NONE', #38577, #23212 ) ;
#92954 = DIRECTION ( 'NONE',  ( -0.7071067811865486830, 0.7071067811865464625, 0.000000000000000000 ) ) ;
#92955 = EDGE_LOOP ( 'NONE', ( #61541, #128456, #98893, #84764 ) ) ;
#92956 = EDGE_CURVE ( 'NONE', #42124, #116559, #129000, .T. ) ;
#92957 = ORIENTED_EDGE ( 'NONE', *, *, #121556, .F. ) ;
#92958 = CARTESIAN_POINT ( 'NONE',  ( 6.183988606268994381, 28.73617430169791476, 5.000000000000000000 ) ) ;
#92959 = EDGE_CURVE ( 'NONE', #15191, #48074, #51464, .T. ) ;
#92960 = CARTESIAN_POINT ( 'NONE',  ( -5.292893218813420120, -9.740707523384182664, 5.000000000000000000 ) ) ;
#92961 = CARTESIAN_POINT ( 'NONE',  ( -18.48921356237309510, -27.52281430457068367, 5.000000000000000000 ) ) ;
#92962 = AXIS2_PLACEMENT_3D ( 'NONE', #100051, #108735, #121770 ) ;
#92963 =( BOUNDED_CURVE ( )  B_SPLINE_CURVE ( 3, ( #7675, #9828, #119985, #119296 ),
 .UNSPECIFIED., .F., .T. ) 
 B_SPLINE_CURVE_WITH_KNOTS ( ( 4, 4 ),
 ( 1.864375635226946049, 1.933014472006540752 ),
 .UNSPECIFIED. ) 
 CURVE ( )  GEOMETRIC_REPRESENTATION_ITEM ( )  RATIONAL_B_SPLINE_CURVE ( ( 1.000000000000000000, 0.9996074310407766506, 0.9996074310407766506, 1.000000000000000000 ) ) 
 REPRESENTATION_ITEM ( '' )  );
#92964 = EDGE_CURVE ( 'NONE', #103024, #69036, #95655, .T. ) ;
#92965 = EDGE_CURVE ( 'NONE', #17540, #19275, #438, .T. ) ;
#92966 = CARTESIAN_POINT ( 'NONE',  ( 53.28709685856478018, 3.054999999999997495, 5.291415217122919401 ) ) ;
#92967 = EDGE_LOOP ( 'NONE', ( #6340, #58870, #69129, #112743 ) ) ;
#92968 = LINE ( 'NONE', #102444, #64960 ) ;
#92969 = CARTESIAN_POINT ( 'NONE',  ( 35.99451991528749772, 28.92564299267963079, 4.000000000000000000 ) ) ;
#92970 = ORIENTED_EDGE ( 'NONE', *, *, #65362, .F. ) ;
#92971 = ORIENTED_EDGE ( 'NONE', *, *, #76454, .T. ) ;
#92972 = CARTESIAN_POINT ( 'NONE',  ( 39.18398860626899705, 28.73617430169814568, 5.000000000000000000 ) ) ;
#92974 = ADVANCED_FACE ( 'NONE', ( #50742 ), #20220, .F. ) ;
#92973 = VECTOR ( 'NONE', #70105, 1000.000000000000000 ) ;
#92975 = EDGE_LOOP ( 'NONE', ( #106420, #132525, #101630, #18059 ) ) ;
#92976 = VECTOR ( 'NONE', #74306, 1000.000000000000000 ) ;
#92977 = CIRCLE ( 'NONE', #130026, 2.500000000000000888 ) ;
#92978 = DIRECTION ( 'NONE',  ( 0.7071067811865487940, 0.7071067811865463515, 0.000000000000000000 ) ) ;
#92979 = ORIENTED_EDGE ( 'NONE', *, *, #56613, .F. ) ;
#92980 = CARTESIAN_POINT ( 'NONE',  ( -39.18398860626899705, 28.73617430169814568, 5.000000000000000000 ) ) ;
#92981 = VECTOR ( 'NONE', #42636, 1000.000000000000000 ) ;
#92983 = CARTESIAN_POINT ( 'NONE',  ( 63.48921356237309510, -27.52281430457099631, 5.000000000000000000 ) ) ;
#92982 = VECTOR ( 'NONE', #2298, 999.9999999999998863 ) ;
#92984 =( GEOMETRIC_REPRESENTATION_CONTEXT ( 3 ) GLOBAL_UNCERTAINTY_ASSIGNED_CONTEXT ( ( #123048 ) ) GLOBAL_UNIT_ASSIGNED_CONTEXT ( ( #57990, #93435, #72441 ) ) REPRESENTATION_CONTEXT ( 'NONE', 'WORKASPACE' ) );
#92985 = VECTOR ( 'NONE', #123828, 1000.000000000000000 ) ;
#92986 = AXIS2_PLACEMENT_3D ( 'NONE', #106307, #118646, #38247 ) ;
#92987 = DIRECTION ( 'NONE',  ( -0.3543493200069162685, -0.000000000000000000, -0.9351131265310288487 ) ) ;
#92988 = FACE_BOUND ( 'NONE', #84976, .T. ) ;
#92989 = CYLINDRICAL_SURFACE ( 'NONE', #43415, 2.500000000000000444 ) ;
#92990 = CARTESIAN_POINT ( 'NONE',  ( 34.47516574401890921, 10.49051761211551437, 4.998110765256833510 ) ) ;
#92992 = LINE ( 'NONE', #13973, #94439 ) ;
#92991 = VECTOR ( 'NONE', #136103, 1000.000000000000000 ) ;
#92994 = ORIENTED_EDGE ( 'NONE', *, *, #139883, .T. ) ;
#92993 = CARTESIAN_POINT ( 'NONE',  ( -14.20003122016828101, 8.259292476615634371, 16.85664084051844469 ) ) ;
#92995 = CARTESIAN_POINT ( 'NONE',  ( -4.171830600776443632, 15.75929247661556332, 4.000000000000000000 ) ) ;
#92996 = EDGE_LOOP ( 'NONE', ( #103392, #26209, #140687, #76831 ) ) ;
#92997 = EDGE_CURVE ( 'NONE', #106040, #102218, #29677, .T. ) ;
#92998 = ADVANCED_FACE ( 'NONE', ( #73917 ), #116705, .F. ) ;
#92999 = ORIENTED_EDGE ( 'NONE', *, *, #67581, .F. ) ;
#93000 = CARTESIAN_POINT ( 'NONE',  ( 69.03709685856478018, -3.054999999999998828, -5.291415217122919401 ) ) ;
#93001 = ORIENTED_EDGE ( 'NONE', *, *, #132742, .T. ) ;
#93002 = CARTESIAN_POINT ( 'NONE',  ( 57.48921356237308800, -27.52281430457095368, 5.000000000000000000 ) ) ;
#93003 = DIRECTION ( 'NONE',  ( 0.7071067811865487940, 0.7071067811865463515, 0.000000000000000000 ) ) ;
#93004 = ORIENTED_EDGE ( 'NONE', *, *, #72299, .F. ) ;
#93005 = CARTESIAN_POINT ( 'NONE',  ( -34.92500000000001137, -22.22500000000000142, 4.500000000000000888 ) ) ;
#93006 = EDGE_CURVE ( 'NONE', #109576, #78218, #73222, .T. ) ;
#93007 = AXIS2_PLACEMENT_3D ( 'NONE', #71079, #81244, #124722 ) ;
#93008 = AXIS2_PLACEMENT_3D ( 'NONE', #91715, #136639, #102618 ) ;
#93009 = LINE ( 'NONE', #137236, #94201 ) ;
#93010 = FACE_OUTER_BOUND ( 'NONE', #96929, .T. ) ;
#93011 = FACE_OUTER_BOUND ( 'NONE', #108116, .T. ) ;
#93012 = VECTOR ( 'NONE', #82695, 1000.000000000000000 ) ;
#93013 = CARTESIAN_POINT ( 'NONE',  ( -11.29289321881337571, -18.74070752338409562, 5.000000000000000000 ) ) ;
#93014 = ORIENTED_EDGE ( 'NONE', *, *, #35845, .T. ) ;
#93015 = ORIENTED_EDGE ( 'NONE', *, *, #12180, .T. ) ;
#93016 = AXIS2_PLACEMENT_3D ( 'NONE', #68367, #88669, #43715 ) ;
#93017 = PLANE ( 'NONE',  #33510 ) ;
#93018 = CARTESIAN_POINT ( 'NONE',  ( 0.000000000000000000, 0.000000000000000000, 5.000000000000000000 ) ) ;
#93019 = ORIENTED_EDGE ( 'NONE', *, *, #60483, .F. ) ;
#93020 = ORIENTED_EDGE ( 'NONE', *, *, #76032, .F. ) ;
#93021 = ORIENTED_EDGE ( 'NONE', *, *, #41090, .F. ) ;
#93022 = DIRECTION ( 'NONE',  ( 0.6830127018922181881, 0.6830127018922202975, -0.2588190451025214056 ) ) ;
#93023 = CARTESIAN_POINT ( 'NONE',  ( -3.489213562373097322, -27.52281430457057709, 5.000000000000000000 ) ) ;
#93024 = VERTEX_POINT ( 'NONE', #108643 ) ;
#93025 = LINE ( 'NONE', #30644, #131986 ) ;
#93026 = AXIS2_PLACEMENT_3D ( 'NONE', #126341, #70585, #35807 ) ;
#93027 = CARTESIAN_POINT ( 'NONE',  ( 7.650403141435218934, 7.934999999999989839, -2.126176841940961904 ) ) ;
#93028 = DIRECTION ( 'NONE',  ( -0.000000000000000000, -0.3543493200069152693, 0.9351131265310292928 ) ) ;
#93029 = VERTEX_POINT ( 'NONE', #52160 ) ;
#93030 = FACE_OUTER_BOUND ( 'NONE', #119682, .T. ) ;
#93032 = EDGE_CURVE ( 'NONE', #36041, #106598, #651, .T. ) ;
#93031 = DIRECTION ( 'NONE',  ( 1.000000000000000000, 0.000000000000000000, 0.000000000000000000 ) ) ;
#93033 = VECTOR ( 'NONE', #100637, 1000.000000000000227 ) ;
#93034 = CARTESIAN_POINT ( 'NONE',  ( -31.49999999999977973, -2.568876922607794988, 4.000000000000000000 ) ) ;
#93036 = ORIENTED_EDGE ( 'NONE', *, *, #112617, .F. ) ;
#93035 = CARTESIAN_POINT ( 'NONE',  ( -30.18398860626900060, 28.73617430169808173, 5.000000000000000000 ) ) ;
#93038 = VECTOR ( 'NONE', #46595, 1000.000000000000000 ) ;
#93037 = CARTESIAN_POINT ( 'NONE',  ( -7.499999999999951150, 14.14708470758590408, -0.5283514160166384865 ) ) ;
#93039 = EDGE_LOOP ( 'NONE', ( #114958, #125443, #10227, #64309, #124194 ) ) ;
#93040 = DIRECTION ( 'NONE',  ( -0.000000000000000000, -0.3543493200069152693, 0.9351131265310292928 ) ) ;
#93041 = CARTESIAN_POINT ( 'NONE',  ( -34.92500000000001137, -22.22500000000000142, 4.000000000000000000 ) ) ;
#93042 = CARTESIAN_POINT ( 'NONE',  ( 109.0625000000000000, -5.819803920172573086, -5.819803920172573974 ) ) ;
#93043 = ORIENTED_EDGE ( 'NONE', *, *, #3919, .F. ) ;
#93045 = EDGE_CURVE ( 'NONE', #77094, #86149, #100501, .T. ) ;
#93044 = DIRECTION ( 'NONE',  ( 0.3543493200069162685, -0.000000000000000000, -0.9351131265310288487 ) ) ;
#93046 = CARTESIAN_POINT ( 'NONE',  ( -51.29974487139158867, -27.71228299555242103, 4.000000000000000000 ) ) ;
#93047 = CARTESIAN_POINT ( 'NONE',  ( 34.92499999999998295, 2.718490437204236443, 4.759050581649325373 ) ) ;
#93048 = LINE ( 'NONE', #39397, #81492 ) ;
#93049 = VECTOR ( 'NONE', #97286, 1000.000000000000000 ) ;
#93050 = EDGE_LOOP ( 'NONE', ( #59192, #123067, #83125, #71901 ) ) ;
#93051 = DIRECTION ( 'NONE',  ( 0.3543493200069162685, -0.000000000000000000, -0.9351131265310288487 ) ) ;
#93052 = CARTESIAN_POINT ( 'NONE',  ( -32.99999999999977263, -8.151047557385101783, -8.977947279169725903 ) ) ;
#93053 = CARTESIAN_POINT ( 'NONE',  ( 8.212472949537106715, 0.000000000000000000, 6.094999999999989981 ) ) ;
#93054 = ADVANCED_FACE ( 'NONE', ( #14181 ), #122143, .T. ) ;
#93055 = CARTESIAN_POINT ( 'NONE',  ( 12.69999999999999574, 0.000000000000000000, -39.50000000000000000 ) ) ;
#93056 = DIRECTION ( 'NONE',  ( 0.3543493200069162685, -0.000000000000000000, -0.9351131265310288487 ) ) ;
#93057 = ADVANCED_FACE ( 'NONE', ( #58473 ), #45430, .F. ) ;
#93058 = VERTEX_POINT ( 'NONE', #33823 ) ;
#93059 = ORIENTED_EDGE ( 'NONE', *, *, #60897, .F. ) ;
#93060 = COLOUR_RGB ( '', 0.72549020, 0.75294118, 0.79215686) ;
#93061 = FACE_OUTER_BOUND ( 'NONE', #140961, .T. ) ;
#93062 = DIRECTION ( 'NONE',  ( -0.7071067811865486830, -0.7071067811865464625, 0.000000000000000000 ) ) ;
#93063 = EDGE_CURVE ( 'NONE', #107560, #11112, #70050, .T. ) ;
#93064 = ADVANCED_FACE ( 'NONE', ( #122219 ), #46134, .F. ) ;
#93065 = CARTESIAN_POINT ( 'NONE',  ( 2.603736474768552522, 5.808823158059036373, 5.808823158059032821 ) ) ;
#93066 = DIRECTION ( 'NONE',  ( -0.7071067811865487940, 0.7071067811865463515, 0.000000000000000000 ) ) ;
#93067 = CARTESIAN_POINT ( 'NONE',  ( 22.85159235450332105, -2.500000000000000000, 3.061616997868384127E-16 ) ) ;
#93068 = CARTESIAN_POINT ( 'NONE',  ( 48.48921356237309510, -27.52281430457089328, 5.000000000000000000 ) ) ;
#93069 = DIRECTION ( 'NONE',  ( 0.6830127018922181881, 0.6830127018922202975, -0.2588190451025214056 ) ) ;
#93070 = ORIENTED_EDGE ( 'NONE', *, *, #25360, .T. ) ;
#93071 = ADVANCED_FACE ( 'NONE', ( #35971 ), #12036, .F. ) ;
#93072 = CARTESIAN_POINT ( 'NONE',  ( -14.00492477221185972, -5.240707523384228850, 12.38332538355499146 ) ) ;
#93073 = DIRECTION ( 'NONE',  ( -0.6830127018922181881, 0.6830127018922202975, -0.2588190451025214056 ) ) ;
#93074 = VECTOR ( 'NONE', #119780, 999.9999999999998863 ) ;
#93075 = AXIS2_PLACEMENT_3D ( 'NONE', #92121, #68293, #124767 ) ;
#93076 = FACE_OUTER_BOUND ( 'NONE', #105578, .T. ) ;
#93077 = CARTESIAN_POINT ( 'NONE',  ( 43.07876352523144448, -7.482591942790327058E-16, 6.109999999999999432 ) ) ;
#93078 = PLANE ( 'NONE',  #14042 ) ;
#93079 = VECTOR ( 'NONE', #77, 1000.000000000000227 ) ;
#93080 = EDGE_CURVE ( 'NONE', #26531, #89946, #113484, .T. ) ;
#93081 = STYLED_ITEM ( 'NONE', ( #3786 ), #15692 ) ;
#93082 = ORIENTED_EDGE ( 'NONE', *, *, #38142, .F. ) ;
#93083 = CYLINDRICAL_SURFACE ( 'NONE', #32615, 0.5000000000000004441 ) ;
#93084 = ORIENTED_EDGE ( 'NONE', *, *, #47054, .T. ) ;
#93085 = ORIENTED_EDGE ( 'NONE', *, *, #95752, .F. ) ;
#93086 = VECTOR ( 'NONE', #101845, 1000.000000000000000 ) ;
#93087 = AXIS2_PLACEMENT_3D ( 'NONE', #78118, #68680, #123047 ) ;
#93088 = DIRECTION ( 'NONE',  ( 0.000000000000000000, 0.000000000000000000, -1.000000000000000000 ) ) ;
#93089 = EDGE_CURVE ( 'NONE', #113425, #129006, #101913, .T. ) ;
#93090 = CARTESIAN_POINT ( 'NONE',  ( -0.1839886062690032631, 28.73617430169787568, 5.000000000000000000 ) ) ;
#93091 = DIRECTION ( 'NONE',  ( 0.7071067811865487940, -0.7071067811865463515, 0.000000000000000000 ) ) ;
#93092 = PLANE ( 'NONE',  #90245 ) ;
#93093 = LINE ( 'NONE', #72094, #30241 ) ;
#93094 = CARTESIAN_POINT ( 'NONE',  ( 48.18398860626899705, 28.73617430169820608, 5.000000000000000000 ) ) ;
#93095 = ORIENTED_EDGE ( 'NONE', *, *, #72351, .F. ) ;
#93096 = FACE_OUTER_BOUND ( 'NONE', #65212, .T. ) ;
#93097 = DIRECTION ( 'NONE',  ( 0.000000000000000000, -1.000000000000000000, 0.000000000000000000 ) ) ;
#93098 = EDGE_CURVE ( 'NONE', #118931, #88406, #46884, .T. ) ;
#93099 = CARTESIAN_POINT ( 'NONE',  ( 18.32840764549667512, -3.851859888774471706E-31, 2.500000000000001332 ) ) ;
#93100 = CARTESIAN_POINT ( 'NONE',  ( 21.48921356237309155, -27.52281430457070499, 5.000000000000000000 ) ) ;
#93101 = CARTESIAN_POINT ( 'NONE',  ( -34.49999999999975842, 12.05432934483081553, 4.994342998332167660 ) ) ;
#93102 = CARTESIAN_POINT ( 'NONE',  ( 64.82919371712955581, -3.975000000000001865, 6.884901960086284411 ) ) ;
#93103 = CARTESIAN_POINT ( 'NONE',  ( -77.99451991528749772, 28.92564299267992567, 4.000000000000000000 ) ) ;
#93104 = ORIENTED_EDGE ( 'NONE', *, *, #29054, .F. ) ;
#93105 = EDGE_LOOP ( 'NONE', ( #41987, #132037, #717, #131881 ) ) ;
#93106 = CARTESIAN_POINT ( 'NONE',  ( 64.43749999999998579, 5.819803920172573974, -5.819803920172572198 ) ) ;
#93107 = CARTESIAN_POINT ( 'NONE',  ( -20.95341186370443154, 14.25929247661556332, 18.84478104361332385 ) ) ;
#93108 = CARTESIAN_POINT ( 'NONE',  ( 0.000000000000000000, 0.000000000000000000, 5.000000000000000000 ) ) ;
#93109 = CARTESIAN_POINT ( 'NONE',  ( 34.92500000000001847, -7.729999999999995097, 3.180000000000000160 ) ) ;
#93110 = EDGE_CURVE ( 'NONE', #143315, #39146, #71226, .T. ) ;
#93111 = VERTEX_POINT ( 'NONE', #111346 ) ;
#93112 = AXIS2_PLACEMENT_3D ( 'NONE', #53414, #130996, #30974 ) ;
#93113 = CARTESIAN_POINT ( 'NONE',  ( 32.79166666666666430, 3.975000000000003642, -6.884901960086285300 ) ) ;
#93114 = ADVANCED_FACE ( 'NONE', ( #138839 ), #28658, .T. ) ;
#93115 = VECTOR ( 'NONE', #77829, 999.9999999999998863 ) ;
#93116 = DIRECTION ( 'NONE',  ( -1.000000000000000000, 7.120242111146219159E-15, 0.000000000000000000 ) ) ;
#93117 = CARTESIAN_POINT ( 'NONE',  ( 56.14626352523143282, -4.472830434245840259, 4.472830434245839371 ) ) ;
#93118 = ADVANCED_FACE ( 'NONE', ( #84471 ), #94587, .F. ) ;
#93119 = VECTOR ( 'NONE', #33345, 1000.000000000000000 ) ;
#93120 = DIRECTION ( 'NONE',  ( -0.3543493200069162685, -0.000000000000000000, -0.9351131265310288487 ) ) ;
#93121 = VERTEX_POINT ( 'NONE', #126502 ) ;
#93122 = VERTEX_POINT ( 'NONE', #29334 ) ;
#93123 = VECTOR ( 'NONE', #85427, 1000.000000000000000 ) ;
#93124 = DIRECTION ( 'NONE',  ( 0.7071067811865487940, -0.7071067811865463515, 0.000000000000000000 ) ) ;
#93125 = EDGE_CURVE ( 'NONE', #122891, #6488, #114891, .T. ) ;
#93126 = CARTESIAN_POINT ( 'NONE',  ( 23.99999999999983302, -4.068876922607771895, 4.000000000000000000 ) ) ;
#93127 = FACE_OUTER_BOUND ( 'NONE', #22410, .T. ) ;
#93128 = CARTESIAN_POINT ( 'NONE',  ( -36.18398860626899705, 28.73617430169812437, 5.000000000000000000 ) ) ;
#93130 = ORIENTED_EDGE ( 'NONE', *, *, #17529, .T. ) ;
#93129 = DIRECTION ( 'NONE',  ( 0.7071067811865487940, 0.7071067811865463515, 0.000000000000000000 ) ) ;
#93131 = DIRECTION ( 'NONE',  ( -1.000000000000000000, -0.000000000000000000, -0.000000000000000000 ) ) ;
#93132 = CARTESIAN_POINT ( 'NONE',  ( 27.48921356237309155, -27.52281430457074762, 5.000000000000000000 ) ) ;
#93133 = DIRECTION ( 'NONE',  ( -0.6830127018922181881, 0.6830127018922202975, -0.2588190451025214056 ) ) ;
#93134 = PRESENTATION_LAYER_ASSIGNMENT (  '', '', ( #5124 ) ) ;
#93135 = CARTESIAN_POINT ( 'NONE',  ( -9.119999999999999218, 0.000000000000000000, 10.00000000000000000 ) ) ;
#93136 = ORIENTED_EDGE ( 'NONE', *, *, #27571, .T. ) ;
#93137 = ORIENTED_EDGE ( 'NONE', *, *, #86824, .T. ) ;
#93138 = EDGE_CURVE ( 'NONE', #116001, #84730, #59850, .T. ) ;
#93139 = CARTESIAN_POINT ( 'NONE',  ( 0.000000000000000000, 0.000000000000000000, 5.000000000000000000 ) ) ;
#93140 = CARTESIAN_POINT ( 'NONE',  ( -34.49999999999975842, -15.29013452822857388, 0.3645803511609551073 ) ) ;
#93141 = AXIS2_PLACEMENT_3D ( 'NONE', #102612, #136634, #37345 ) ;
#93142 = DIRECTION ( 'NONE',  ( -0.6830127018922180770, -0.6830127018922204085, -0.2588190451025213501 ) ) ;
#93143 = CARTESIAN_POINT ( 'NONE',  ( 72.41252705046288440, -7.949999999999998401, -4.867971026610728450E-16 ) ) ;
#93144 = ORIENTED_EDGE ( 'NONE', *, *, #30517, .T. ) ;
#93145 = ORIENTED_EDGE ( 'NONE', *, *, #96319, .F. ) ;
#93146 = COLOUR_RGB ( '', 0.31764706, 0.68627451, 0.89019608) ;
#93148 = EDGE_CURVE ( 'NONE', #133007, #109272, #15569, .T. ) ;
#93147 = LINE ( 'NONE', #17015, #42191 ) ;
#93149 = ORIENTED_EDGE ( 'NONE', *, *, #126323, .T. ) ;
#93150 = CARTESIAN_POINT ( 'NONE',  ( 3.793339364578457662, 21.75929247661549937, 4.998822639870711626 ) ) ;
#93151 = VERTEX_POINT ( 'NONE', #17052 ) ;
#93152 = CARTESIAN_POINT ( 'NONE',  ( 61.91252705046289151, -7.949999999999998401, -4.867971026610728450E-16 ) ) ;
#93153 = PLANE ( 'NONE',  #67948 ) ;
#93154 = AXIS2_PLACEMENT_3D ( 'NONE', #114447, #80427, #113013 ) ;
#93155 = PRESENTATION_LAYER_ASSIGNMENT (  '', '', ( #9840 ) ) ;
#93156 = FACE_BOUND ( 'NONE', #82913, .T. ) ;
#93157 = CARTESIAN_POINT ( 'NONE',  ( 19.49999999999986500, -5.568876922607755908, 4.000000000000000000 ) ) ;
#93158 = DIRECTION ( 'NONE',  ( -0.7071067811865487940, 0.7071067811865463515, -0.000000000000000000 ) ) ;
#93159 = CARTESIAN_POINT ( 'NONE',  ( -16.17183060077635304, 12.75929247661558286, 4.000000000000000000 ) ) ;
#93160 = VECTOR ( 'NONE', #121262, 1000.000000000000000 ) ;
#93161 = CARTESIAN_POINT ( 'NONE',  ( 0.000000000000000000, 0.000000000000000000, 5.000000000000000000 ) ) ;
#93162 = CARTESIAN_POINT ( 'NONE',  ( 0.000000000000000000, 0.000000000000000000, 5.000000000000000000 ) ) ;
#93163 = APPLICATION_PROTOCOL_DEFINITION ( 'draft international standard', 'automotive_design', 1998, #22594 ) ;
#93164 = VERTEX_POINT ( 'NONE', #125824 ) ;
#93165 = EDGE_CURVE ( 'NONE', #25917, #68002, #83765, .T. ) ;
#93166 = ORIENTED_EDGE ( 'NONE', *, *, #129288, .F. ) ;
#93167 = CARTESIAN_POINT ( 'NONE',  ( 92.22459685856479439, -1.637169565754160949, 6.109999999999997655 ) ) ;
#93168 = VERTEX_POINT ( 'NONE', #7574 ) ;
#93169 = FACE_OUTER_BOUND ( 'NONE', #35525, .T. ) ;
#93170 = CARTESIAN_POINT ( 'NONE',  ( 22.88959668761254207, -22.22500000000000142, -16.90811190805141706 ) ) ;
#93171 = VECTOR ( 'NONE', #33551, 1000.000000000000000 ) ;
#93172 = AXIS2_PLACEMENT_3D ( 'NONE', #37539, #36799, #48391 ) ;
#93173 = VECTOR ( 'NONE', #117773, 1000.000000000000000 ) ;
#93174 = VECTOR ( 'NONE', #106510, 999.9999999999998863 ) ;
#93175 = LINE ( 'NONE', #6117, #14691 ) ;
#93176 = EDGE_LOOP ( 'NONE', ( #48373, #30471, #5248, #129811 ) ) ;
#93177 = CARTESIAN_POINT ( 'NONE',  ( 1.734723475976807094E-15, -19.22509904557636418, 1.855685503482177978 ) ) ;
#93178 = FACE_OUTER_BOUND ( 'NONE', #88736, .T. ) ;
#93179 = DIRECTION ( 'NONE',  ( -0.6830127018922180770, -0.6830127018922204085, -0.2588190451025213501 ) ) ;
#93180 = DIRECTION ( 'NONE',  ( 0.7071067811865486830, -0.7071067811865464625, -0.000000000000000000 ) ) ;
#93181 = DIRECTION ( 'NONE',  ( 0.7071067811865487940, -0.7071067811865463515, 0.000000000000000000 ) ) ;
#93182 = VECTOR ( 'NONE', #65498, 1000.000000000000000 ) ;
#93183 = PRESENTATION_LAYER_ASSIGNMENT (  '', '', ( #74686 ) ) ;
#93184 = LINE ( 'NONE', #138846, #67802 ) ;
#93185 = ORIENTED_EDGE ( 'NONE', *, *, #20349, .F. ) ;
#93186 = CARTESIAN_POINT ( 'NONE',  ( -4.499999999999976019, 1.030536316426498233, -5.498701923753791299 ) ) ;
#93187 = LINE ( 'NONE', #81628, #92860 ) ;
#93188 = ORIENTED_EDGE ( 'NONE', *, *, #100797, .T. ) ;
#93189 = ORIENTED_EDGE ( 'NONE', *, *, #120725, .F. ) ;
#93190 = ORIENTED_EDGE ( 'NONE', *, *, #23338, .F. ) ;
#93191 = CARTESIAN_POINT ( 'NONE',  ( 48.85459685856476852, -1.637169565754161615, 6.110000000000000320 ) ) ;
#93192 = ORIENTED_EDGE ( 'NONE', *, *, #33910, .T. ) ;
#93193 = CARTESIAN_POINT ( 'NONE',  ( 14.77497294953710494, 4.461849672132300881, 4.461849672132299105 ) ) ;
#93194 =( NAMED_UNIT ( * ) SI_UNIT ( $, .STERADIAN. ) SOLID_ANGLE_UNIT ( ) );
#93195 = VERTEX_POINT ( 'NONE', #61319 ) ;
#93196 = FACE_OUTER_BOUND ( 'NONE', #41952, .T. ) ;
#93197 = EDGE_LOOP ( 'NONE', ( #12269, #43760, #100378, #63142, #120136 ) ) ;
#93198 = FACE_OUTER_BOUND ( 'NONE', #32339, .T. ) ;
#93200 = ORIENTED_EDGE ( 'NONE', *, *, #121301, .T. ) ;
#93199 = CARTESIAN_POINT ( 'NONE',  ( -29.67183060077626422, 11.25929247661560595, 4.000000000000000000 ) ) ;
#93201 = ORIENTED_EDGE ( 'NONE', *, *, #132894, .F. ) ;
#93202 = PLANE ( 'NONE',  #28413 ) ;
#93203 = AXIS2_PLACEMENT_3D ( 'NONE', #22719, #37761, #25413 ) ;
#93204 = DIRECTION ( 'NONE',  ( -1.000000000000000000, -1.224606353822377258E-16, -0.000000000000000000 ) ) ;
#93205 = ORIENTED_EDGE ( 'NONE', *, *, #122322, .F. ) ;
#93206 = DIRECTION ( 'NONE',  ( 0.7071067811865487940, 0.7071067811865463515, -0.000000000000000000 ) ) ;
#93207 = ORIENTED_EDGE ( 'NONE', *, *, #86218, .F. ) ;
#93208 = PRODUCT_DEFINITION_SHAPE ( 'NONE', 'NONE',  #143559 ) ;
#93209 = ORIENTED_EDGE ( 'NONE', *, *, #85357, .T. ) ;
#93210 = CIRCLE ( 'NONE', #7509, 6.349999999999997868 ) ;
#93211 = ORIENTED_EDGE ( 'NONE', *, *, #83115, .F. ) ;
#93212 = VERTEX_POINT ( 'NONE', #4678 ) ;
#93213 = CARTESIAN_POINT ( 'NONE',  ( 0.000000000000000000, 0.000000000000000000, 5.000000000000000000 ) ) ;
#93214 = CIRCLE ( 'NONE', #51535, 3.000000000000002665 ) ;
#93215 = STYLED_ITEM ( 'NONE', ( #83890 ), #62638 ) ;
#93216 = LINE ( 'NONE', #82362, #58506 ) ;
#93217 = FACE_OUTER_BOUND ( 'NONE', #98712, .T. ) ;
#93218 = DIRECTION ( 'NONE',  ( 0.7071067811865487940, 0.7071067811865463515, 0.000000000000000000 ) ) ;
#93219 = EDGE_CURVE ( 'NONE', #129026, #76029, #95311, .T. ) ;
#93220 = ADVANCED_FACE ( 'NONE', ( #71437 ), #82320, .F. ) ;
#93221 = LINE ( 'NONE', #36013, #67415 ) ;
#93222 = ORIENTED_EDGE ( 'NONE', *, *, #138465, .T. ) ;
#93223 = DIRECTION ( 'NONE',  ( -1.000000000000000000, -0.000000000000000000, -0.000000000000000000 ) ) ;
#93224 = ADVANCED_FACE ( 'NONE', ( #105457 ), #60591, .F. ) ;
#93225 = ADVANCED_FACE ( 'NONE', ( #6122 ), #50400, .F. ) ;
#93226 = CARTESIAN_POINT ( 'NONE',  ( 20.54123647476855652, 0.000000000000000000, 7.934999999999990727 ) ) ;
#93227 = PLANE ( 'NONE',  #20743 ) ;
#93228 = CARTESIAN_POINT ( 'NONE',  ( 95.64583333333332860, 2.130196079827431976, -7.949999999999998401 ) ) ;
#93229 = DIRECTION ( 'NONE',  ( 0.7071067811865487940, -0.7071067811865463515, 0.000000000000000000 ) ) ;
#93230 = ORIENTED_EDGE ( 'NONE', *, *, #104661, .T. ) ;
#93231 = VERTEX_POINT ( 'NONE', #137408 ) ;
#93232 = EDGE_CURVE ( 'NONE', #121879, #114032, #134292, .T. ) ;
#93233 = ORIENTED_EDGE ( 'NONE', *, *, #136647, .F. ) ;
#93234 = DIRECTION ( 'NONE',  ( -1.000000000000000000, -1.224606353822377258E-16, -0.000000000000000000 ) ) ;
#93235 = CARTESIAN_POINT ( 'NONE',  ( 95.74586038379622721, 3.974999999999996980, 6.884901960086287964 ) ) ;
#93236 = CARTESIAN_POINT ( 'NONE',  ( -34.17183060077623225, 9.759292476615625489, 4.000000000000000000 ) ) ;
#93237 = VECTOR ( 'NONE', #112021, 999.9999999999998863 ) ;
#93238 = EDGE_CURVE ( 'NONE', #79175, #56422, #5427, .T. ) ;
#93239 = DIRECTION ( 'NONE',  ( -1.000000000000000000, 0.000000000000000000, -0.000000000000000000 ) ) ;
#93240 = SURFACE_STYLE_FILL_AREA ( #134629 ) ;
#93241 = CARTESIAN_POINT ( 'NONE',  ( 70.64126352523145158, 4.472830434245837594, 4.472830434245841147 ) ) ;
#93242 = CARTESIAN_POINT ( 'NONE',  ( 81.06249999999998579, -5.819803920172573086, -5.819803920172573974 ) ) ;
#93243 = ADVANCED_FACE ( 'NONE', ( #128664 ), #38855, .T. ) ;
#93244 = DIRECTION ( 'NONE',  ( 0.7071067811865487940, -0.7071067811865463515, -0.000000000000000000 ) ) ;
#93245 = LINE ( 'NONE', #47646, #92708 ) ;
#93246 = DIRECTION ( 'NONE',  ( -0.7071067811865486830, -0.7071067811865464625, 0.000000000000000000 ) ) ;
#93247 = FACE_OUTER_BOUND ( 'NONE', #107670, .T. ) ;
#93248 = VERTEX_POINT ( 'NONE', #62713 ) ;
#93249 = VECTOR ( 'NONE', #125240, 1000.000000000000227 ) ;
#93250 = DIRECTION ( 'NONE',  ( 0.6830127018922180770, -0.6830127018922204085, -0.2588190451025213501 ) ) ;
#93251 = ORIENTED_EDGE ( 'NONE', *, *, #65609, .F. ) ;
#93252 = EDGE_CURVE ( 'NONE', #10395, #30730, #132266, .T. ) ;
#93253 = CARTESIAN_POINT ( 'NONE',  ( 14.27159235450332098, 9.902892378096218942E-16, 0.000000000000000000 ) ) ;
#93255 = ORIENTED_EDGE ( 'NONE', *, *, #81991, .T. ) ;
#93254 = DIRECTION ( 'NONE',  ( -0.3543493200069162685, -0.000000000000000000, -0.9351131265310288487 ) ) ;
#93256 = LINE ( 'NONE', #103396, #85697 ) ;
#93257 = CARTESIAN_POINT ( 'NONE',  ( -17.99999999999987566, 9.631307414974306980, -9.079085613539584543 ) ) ;
#93258 = VERTEX_POINT ( 'NONE', #131522 ) ;
#93259 = CARTESIAN_POINT ( 'NONE',  ( 180.4193221990230143, -49.14999999999999147, 40.92499999999998295 ) ) ;
#93261 = EDGE_LOOP ( 'NONE', ( #79936, #129317, #47943, #124807 ) ) ;
#93260 = VECTOR ( 'NONE', #98462, 1000.000000000000000 ) ;
#93262 = LINE ( 'NONE', #27275, #53678 ) ;
#93263 = ORIENTED_EDGE ( 'NONE', *, *, #33201, .F. ) ;
#93264 = EDGE_CURVE ( 'NONE', #63012, #8822, #30799, .T. ) ;
#93265 = DIRECTION ( 'NONE',  ( 0.7071067811865487940, 0.7071067811865463515, 0.000000000000000000 ) ) ;
#93266 = CARTESIAN_POINT ( 'NONE',  ( 91.80836038379622721, 7.949999999999997513, 2.130196079827431088 ) ) ;
#93267 = FILL_AREA_STYLE ('',( #106253 ) ) ;
#93268 = ORIENTED_EDGE ( 'NONE', *, *, #8135, .F. ) ;
#93269 = DIRECTION ( 'NONE',  ( 0.7071067811865487940, 0.7071067811865463515, -0.000000000000000000 ) ) ;
#93270 = CARTESIAN_POINT ( 'NONE',  ( -34.49999999999976552, 6.054329344830883031, 4.994342998332166772 ) ) ;
#93271 = CARTESIAN_POINT ( 'NONE',  ( 26.97916666666666785, 6.094999999999988205, -1.633150327867694651 ) ) ;
#93272 = EDGE_CURVE ( 'NONE', #31242, #82671, #108292, .T. ) ;
#93273 = DIRECTION ( 'NONE',  ( 0.000000000000000000, 0.000000000000000000, 1.000000000000000000 ) ) ;
#93274 = VECTOR ( 'NONE', #70469, 999.9999999999998863 ) ;
#93275 = CARTESIAN_POINT ( 'NONE',  ( 6.471592354503322042, 3.061616997868380183E-16, -2.500000000000001332 ) ) ;
#93276 = ORIENTED_EDGE ( 'NONE', *, *, #80818, .T. ) ;
#93277 = VECTOR ( 'NONE', #52382, 1000.000000000000000 ) ;
#93278 = VECTOR ( 'NONE', #56144, 1000.000000000000000 ) ;
#93279 = DIRECTION ( 'NONE',  ( -0.6830127018922180770, -0.6830127018922204085, -0.2588190451025213501 ) ) ;
#93280 = EDGE_CURVE ( 'NONE', #117911, #92907, #19882, .T. ) ;
#93281 = ORIENTED_EDGE ( 'NONE', *, *, #111040, .T. ) ;
#93282 = CARTESIAN_POINT ( 'NONE',  ( 81.22959685856476142, -6.110000000000000320, -1.637169565754161393 ) ) ;
#93283 = EDGE_CURVE ( 'NONE', #89124, #130861, #31497, .T. ) ;
#93284 = LINE ( 'NONE', #27295, #80158 ) ;
#93286 = CARTESIAN_POINT ( 'NONE',  ( 45.29974487139158867, -27.71228299555237840, 4.000000000000000000 ) ) ;
#93285 = AXIS2_PLACEMENT_3D ( 'NONE', #26603, #105565, #70846 ) ;
#93287 = STYLED_ITEM ( 'NONE', ( #41813 ), #77733 ) ;
#93288 = CARTESIAN_POINT ( 'NONE',  ( 24.39999999999999858, 1.399999999999986366, 20.40202195861970580 ) ) ;
#93289 = ORIENTED_EDGE ( 'NONE', *, *, #53280, .F. ) ;
#93290 = DIRECTION ( 'NONE',  ( -0.7071067811865486830, -0.7071067811865464625, -0.000000000000000000 ) ) ;
#93291 = EDGE_CURVE ( 'NONE', #118704, #122228, #65591, .T. ) ;
#93292 = ADVANCED_FACE ( 'NONE', ( #141693 ), #130102, .F. ) ;
#93293 = FACE_OUTER_BOUND ( 'NONE', #115056, .T. ) ;
#93294 = CARTESIAN_POINT ( 'NONE',  ( 11.99999999999992006, -7.447814304570750998, 5.000000000000000000 ) ) ;
#93295 = CARTESIAN_POINT ( 'NONE',  ( 3.328169399223507519, 2.259292476615690770, 4.000000000000000000 ) ) ;
#93297 = ORIENTED_EDGE ( 'NONE', *, *, #44094, .T. ) ;
#93296 = CARTESIAN_POINT ( 'NONE',  ( 0.000000000000000000, 0.000000000000000000, 5.000000000000000000 ) ) ;
#93298 = CARTESIAN_POINT ( 'NONE',  ( 12.83333333333333393, 5.278424836066143655, -3.047499999999997655 ) ) ;
#93299 = CARTESIAN_POINT ( 'NONE',  ( -22.89835756248665888, 7.738675393078206177, 4.667276354320995857 ) ) ;
#93300 = CARTESIAN_POINT ( 'NONE',  ( 1.971958729986437842, -5.986773400458673677, 1.339903956443486477 ) ) ;
#93301 = DIRECTION ( 'NONE',  ( 0.000000000000000000, 0.000000000000000000, -1.000000000000000000 ) ) ;
#93302 = ORIENTED_EDGE ( 'NONE', *, *, #37347, .T. ) ;
#93303 = VERTEX_POINT ( 'NONE', #53989 ) ;
#93304 = ORIENTED_EDGE ( 'NONE', *, *, #92394, .F. ) ;
#93305 = CARTESIAN_POINT ( 'NONE',  ( 80.06293019189810423, 1.637169565754157174, 6.110000000000002984 ) ) ;
#93306 = VECTOR ( 'NONE', #87899, 1000.000000000000000 ) ;
#93307 = ORIENTED_EDGE ( 'NONE', *, *, #56795, .F. ) ;
#93308 = EDGE_CURVE ( 'NONE', #110817, #103815, #77173, .T. ) ;
#93309 =( LENGTH_UNIT ( ) NAMED_UNIT ( * ) SI_UNIT ( .MILLI., .METRE. ) );
#93310 = DIRECTION ( 'NONE',  ( -0.7071067811865486830, -0.7071067811865464625, 0.000000000000000000 ) ) ;
#93311 = CARTESIAN_POINT ( 'NONE',  ( 7.939999999999994174, -39.93000000000000682, -7.752100000000004876 ) ) ;
#93312 = LINE ( 'NONE', #107030, #105921 ) ;
#93313 = VERTEX_POINT ( 'NONE', #121343 ) ;
#93314 = LINE ( 'NONE', #51255, #127824 ) ;
#93315 = CARTESIAN_POINT ( 'NONE',  ( -2.816011393730999401, 28.73617430169785436, 5.000000000000000000 ) ) ;
#93316 = CIRCLE ( 'NONE', #128005, 0.5000000000000004441 ) ;
#93317 = VERTEX_POINT ( 'NONE', #66278 ) ;
#93318 = EDGE_CURVE ( 'NONE', #84223, #132339, #87306, .T. ) ;
#93319 = VECTOR ( 'NONE', #15446, 1000.000000000000000 ) ;
#93320 = DIRECTION ( 'NONE',  ( -0.7071067811865486830, -0.7071067811865464625, 0.000000000000000000 ) ) ;
#93321 = CARTESIAN_POINT ( 'NONE',  ( -16.17183060077635659, 18.75929247661552424, 4.000000000000000000 ) ) ;
#93322 = LINE ( 'NONE', #17866, #28489 ) ;
#93323 = ORIENTED_EDGE ( 'NONE', *, *, #129937, .T. ) ;
#93324 = ORIENTED_EDGE ( 'NONE', *, *, #128213, .F. ) ;
#93325 = EDGE_CURVE ( 'NONE', #112402, #4116, #42396, .T. ) ;
#93326 = CARTESIAN_POINT ( 'NONE',  ( -29.67183060077626422, 8.259292476615639700, 4.000000000000000000 ) ) ;
#93327 = DIRECTION ( 'NONE',  ( -1.000000000000000000, 0.000000000000000000, 0.000000000000000000 ) ) ;
#93328 = DIRECTION ( 'NONE',  ( -0.7071067811865486830, -0.7071067811865464625, 0.000000000000000000 ) ) ;
#93329 = DIRECTION ( 'NONE',  ( 0.7071067811865487940, 0.7071067811865463515, 0.000000000000000000 ) ) ;
#93330 = DIRECTION ( 'NONE',  ( -1.000000000000000000, -0.000000000000000000, -0.000000000000000000 ) ) ;
#93331 = SURFACE_SIDE_STYLE ('',( #115044 ) ) ;
#93332 = CARTESIAN_POINT ( 'NONE',  ( 10.77958563595370833, -2.500000000000000444, 3.061616997868384127E-16 ) ) ;
#93333 = VECTOR ( 'NONE', #50819, 999.9999999999998863 ) ;
#93334 = FACE_OUTER_BOUND ( 'NONE', #55523, .T. ) ;
#93335 = FILL_AREA_STYLE_COLOUR ( '', #26239 ) ;
#93336 = ORIENTED_EDGE ( 'NONE', *, *, #61737, .F. ) ;
#93337 = VECTOR ( 'NONE', #14054, 1000.000000000000000 ) ;
#93338 = ORIENTED_EDGE ( 'NONE', *, *, #38670, .T. ) ;
#93339 =( BOUNDED_CURVE ( )  B_SPLINE_CURVE ( 3, ( #121532, #77369, #130303, #76643 ),
 .UNSPECIFIED., .F., .T. ) 
 B_SPLINE_CURVE_WITH_KNOTS ( ( 4, 4 ),
 ( 1.964434688349479652, 3.503810798801452187 ),
 .UNSPECIFIED. ) 
 CURVE ( )  GEOMETRIC_REPRESENTATION_ITEM ( )  RATIONAL_B_SPLINE_CURVE ( ( 1.000000000000000000, 0.8120851936182260644, 0.8120851936182260644, 1.000000000000000000 ) ) 
 REPRESENTATION_ITEM ( '' )  );
#93340 = ORIENTED_EDGE ( 'NONE', *, *, #94807, .F. ) ;
#93341 = EDGE_LOOP ( 'NONE', ( #14489, #99842, #36699, #35964, #129190, #17143 ) ) ;
#93342 = AXIS2_PLACEMENT_3D ( 'NONE', #49639, #36574, #71366 ) ;
#93343 = ADVANCED_FACE ( 'NONE', ( #110449 ), #96704, .F. ) ;
#93344 = PLANE ( 'NONE',  #26970 ) ;
#93346 = EDGE_CURVE ( 'NONE', #41198, #18669, #75027, .T. ) ;
#93345 = FILL_AREA_STYLE_COLOUR ( '', #142304 ) ;
#93347 = ORIENTED_EDGE ( 'NONE', *, *, #65026, .T. ) ;
#93348 = SURFACE_SIDE_STYLE ('',( #17213 ) ) ;
#93349 = DIRECTION ( 'NONE',  ( -1.000000000000000000, -0.000000000000000000, -0.000000000000000000 ) ) ;
#93350 = PLANE ( 'NONE',  #52603 ) ;
#93351 = DIRECTION ( 'NONE',  ( 0.7071067811865486830, -0.7071067811865464625, -0.000000000000000000 ) ) ;
#93352 = AXIS2_PLACEMENT_3D ( 'NONE', #85179, #106937, #29372 ) ;
#93353 = DIRECTION ( 'NONE',  ( 0.7071067811865487940, 0.7071067811865463515, 0.000000000000000000 ) ) ;
#93354 = ORIENTED_EDGE ( 'NONE', *, *, #34335, .F. ) ;
#93355 = LINE ( 'NONE', #71613, #58796 ) ;
#93356 = CARTESIAN_POINT ( 'NONE',  ( -19.69064382391260892, -2.759520746520534473, 4.000000000000000000 ) ) ;
#93357 = ORIENTED_EDGE ( 'NONE', *, *, #122099, .T. ) ;
#93358 = DIRECTION ( 'NONE',  ( -0.7071067811865486830, 0.7071067811865464625, 0.000000000000000000 ) ) ;
#93359 = ORIENTED_EDGE ( 'NONE', *, *, #53076, .T. ) ;
#93360 = ADVANCED_FACE ( 'NONE', ( #143106 ), #75719, .F. ) ;
#93361 = VERTEX_POINT ( 'NONE', #142413 ) ;
#93362 = CARTESIAN_POINT ( 'NONE',  ( -6.489213562373093325, -27.52281430457059841, 5.000000000000000000 ) ) ;
#93363 = ORIENTED_EDGE ( 'NONE', *, *, #121089, .F. ) ;
#93364 = ORIENTED_EDGE ( 'NONE', *, *, #116674, .F. ) ;
#93365 = AXIS2_PLACEMENT_3D ( 'NONE', #67857, #57678, #122906 ) ;
#93366 = CARTESIAN_POINT ( 'NONE',  ( 76.27126352523144703, 4.472830434245838482, 4.472830434245842035 ) ) ;
#93367 = VERTEX_POINT ( 'NONE', #119200 ) ;
#93368 = CARTESIAN_POINT ( 'NONE',  ( 60.29974487139158867, -27.71228299555248142, 4.000000000000000000 ) ) ;
#93369 = CARTESIAN_POINT ( 'NONE',  ( -31.88982677111766506, -22.22500000000000142, 4.785647885939354751 ) ) ;
#93370 = CARTESIAN_POINT ( 'NONE',  ( 111.5629301918981184, 1.637169565754157174, 6.110000000000002984 ) ) ;
#93371 = DIRECTION ( 'NONE',  ( -0.6830127018922181881, 0.6830127018922202975, -0.2588190451025214056 ) ) ;
#93372 = LINE ( 'NONE', #91263, #1932 ) ;
#93373 = FACE_OUTER_BOUND ( 'NONE', #50781, .T. ) ;
#93374 = VECTOR ( 'NONE', #56570, 999.9999999999998863 ) ;
#93375 = CARTESIAN_POINT ( 'NONE',  ( -23.67183060077630685, -15.74070752338411339, 4.000000000000000000 ) ) ;
#93376 = FACE_OUTER_BOUND ( 'NONE', #72981, .T. ) ;
#93377 = VECTOR ( 'NONE', #87672, 1000.000000000000000 ) ;
#93378 = PLANE ( 'NONE',  #132442 ) ;
#93379 = CARTESIAN_POINT ( 'NONE',  ( -27.79289321881325492, 0.7592924766157086447, 5.000000000000000000 ) ) ;
#93380 = VERTEX_POINT ( 'NONE', #140259 ) ;
#93381 = CARTESIAN_POINT ( 'NONE',  ( 63.48921356237309510, -27.52281430457099631, 5.000000000000000000 ) ) ;
#93382 = ORIENTED_EDGE ( 'NONE', *, *, #55169, .F. ) ;
#93383 = ORIENTED_EDGE ( 'NONE', *, *, #46662, .T. ) ;
#93384 = PRODUCT_DEFINITION_FORMATION_WITH_SPECIFIED_SOURCE ( 'ANY', '', #56020, .NOT_KNOWN. ) ;
#93385 = DIRECTION ( 'NONE',  ( 0.000000000000000000, -5.559056632600921604E-15, 1.000000000000000000 ) ) ;
#93386 = VERTEX_POINT ( 'NONE', #85864 ) ;
#93387 = DIRECTION ( 'NONE',  ( 1.000000000000000000, 0.000000000000000000, 0.000000000000000000 ) ) ;
#93388 = CARTESIAN_POINT ( 'NONE',  ( -0.8518164496185489654, 17.25929247661554200, 8.802941693769200882 ) ) ;
#93389 = CARTESIAN_POINT ( 'NONE',  ( 0.000000000000000000, 0.000000000000000000, 5.000000000000000000 ) ) ;
#93390 = CARTESIAN_POINT ( 'NONE',  ( 31.17183060077625001, 9.759292476615625489, 4.000000000000000000 ) ) ;
#93391 = EDGE_CURVE ( 'NONE', #120276, #52005, #43100, .T. ) ;
#93392 = ORIENTED_EDGE ( 'NONE', *, *, #109562, .T. ) ;
#93393 = SURFACE_STYLE_FILL_AREA ( #49204 ) ;
#93394 = ORIENTED_EDGE ( 'NONE', *, *, #89284, .F. ) ;
#93395 = CARTESIAN_POINT ( 'NONE',  ( -8.999999999999944933, 4.965500833774321165, -4.007596771432636373 ) ) ;
#93396 = EDGE_CURVE ( 'NONE', #66330, #60758, #109031, .T. ) ;
#93397 = EDGE_CURVE ( 'NONE', #55705, #137664, #63445, .T. ) ;
#93398 = VECTOR ( 'NONE', #33396, 1000.000000000000227 ) ;
#93399 = CARTESIAN_POINT ( 'NONE',  ( 25.00456980810188767, 6.871911579029510442, -3.967499999999998916 ) ) ;
#93400 = CARTESIAN_POINT ( 'NONE',  ( 14.51078643762690490, -27.52281430457045275, 5.000000000000000000 ) ) ;
#93401 = EDGE_CURVE ( 'NONE', #52621, #137809, #13994, .T. ) ;
#93402 = CARTESIAN_POINT ( 'NONE',  ( 30.32816939922332011, 5.259292476615665457, 4.000000000000000000 ) ) ;
#93403 = CARTESIAN_POINT ( 'NONE',  ( 6.489213562373093325, -27.52281430457059841, 5.000000000000000000 ) ) ;
#93404 = ORIENTED_EDGE ( 'NONE', *, *, #97551, .F. ) ;
#93405 = ORIENTED_EDGE ( 'NONE', *, *, #14510, .F. ) ;
#93406 = ADVANCED_FACE ( 'NONE', ( #34349 ), #36488, .F. ) ;
#93407 = ORIENTED_EDGE ( 'NONE', *, *, #4452, .T. ) ;
#93408 = DIRECTION ( 'NONE',  ( -1.000000000000000000, -1.369518533665900312E-16, 0.000000000000000000 ) ) ;
#93409 = DIRECTION ( 'NONE',  ( -0.000000000000000000, 0.3543493200069153248, 0.9351131265310292928 ) ) ;
#93410 = LINE ( 'NONE', #2819, #86730 ) ;
#93411 = ADVANCED_FACE ( 'NONE', ( #80728 ), #11853, .T. ) ;
#93412 = PLANE ( 'NONE',  #65828 ) ;
#93413 = CIRCLE ( 'NONE', #132775, 2.500000000000000444 ) ;
#93414 = CARTESIAN_POINT ( 'NONE',  ( 11.15159235450332176, -2.500000000000000000, 3.061616997868384127E-16 ) ) ;
#93415 = LINE ( 'NONE', #27418, #108215 ) ;
#93416 = ADVANCED_FACE ( 'NONE', ( #45264 ), #980, .T. ) ;
#93417 = CARTESIAN_POINT ( 'NONE',  ( -22.00193056682082471, -22.22500000000000142, 4.500000000000000888 ) ) ;
#93418 = EDGE_CURVE ( 'NONE', #34275, #53418, #22956, .T. ) ;
#93419 = LINE ( 'NONE', #37628, #118312 ) ;
#93420 = CARTESIAN_POINT ( 'NONE',  ( 51.48921356237309510, -27.52281430457091460, 5.000000000000000000 ) ) ;
#93421 = ORIENTED_EDGE ( 'NONE', *, *, #139606, .F. ) ;
#93422 = DIRECTION ( 'NONE',  ( -0.000000000000000000, 0.000000000000000000, 1.000000000000000000 ) ) ;
#93423 = ORIENTED_EDGE ( 'NONE', *, *, #73607, .F. ) ;
#93424 = VECTOR ( 'NONE', #94629, 1000.000000000000000 ) ;
#93425 = EDGE_CURVE ( 'NONE', #97256, #56540, #25593, .T. ) ;
#93426 = LINE ( 'NONE', #100904, #41269 ) ;
#93428 = ORIENTED_EDGE ( 'NONE', *, *, #51267, .F. ) ;
#93427 = CARTESIAN_POINT ( 'NONE',  ( 56.45153347184069759, -50.67230138428258357, -37.61253110040615866 ) ) ;
#93429 = ORIENTED_EDGE ( 'NONE', *, *, #86948, .T. ) ;
#93430 = EDGE_CURVE ( 'NONE', #64028, #140629, #56142, .T. ) ;
#93431 = DIRECTION ( 'NONE',  ( 0.000000000000000000, -1.000000000000000000, 0.000000000000000000 ) ) ;
#93432 = DIRECTION ( 'NONE',  ( -0.7071067811865487940, 0.7071067811865463515, -0.000000000000000000 ) ) ;
#93433 = DIRECTION ( 'NONE',  ( -0.7071067811865486830, -0.7071067811865464625, 0.000000000000000000 ) ) ;
#93434 = VERTEX_POINT ( 'NONE', #91583 ) ;
#93435 =( NAMED_UNIT ( * ) PLANE_ANGLE_UNIT ( ) SI_UNIT ( $, .RADIAN. ) );
#93436 = ORIENTED_EDGE ( 'NONE', *, *, #19232, .T. ) ;
#93437 = EDGE_CURVE ( 'NONE', #28467, #84209, #20361, .T. ) ;
#93438 = VECTOR ( 'NONE', #24347, 999.9999999999998863 ) ;
#93439 = LINE ( 'NONE', #50642, #1181 ) ;
#93440 = PLANE ( 'NONE',  #101842 ) ;
#93441 = CARTESIAN_POINT ( 'NONE',  ( 29.80793019189811588, -6.109999999999999432, 1.637169565754158507 ) ) ;
#93443 = VECTOR ( 'NONE', #92833, 1000.000000000000000 ) ;
#93442 = FACE_OUTER_BOUND ( 'NONE', #109466, .T. ) ;
#93444 = LINE ( 'NONE', #39058, #32396 ) ;
#93445 = CARTESIAN_POINT ( 'NONE',  ( -2.510786437626908008, -27.52281430457053446, 5.000000000000000000 ) ) ;
#93446 = CARTESIAN_POINT ( 'NONE',  ( 19.88840764549667384, 3.061616997868380183E-16, -2.500000000000001332 ) ) ;
#93447 = CARTESIAN_POINT ( 'NONE',  ( 53.99451991528749062, 28.92564299267975869, 4.000000000000000000 ) ) ;
#93448 = CARTESIAN_POINT ( 'NONE',  ( 32.93706980810188156, 2.126176841940952134, -7.934999999999993392 ) ) ;
#93449 = CARTESIAN_POINT ( 'NONE',  ( 3.478736474768552078, -5.808823158059033709, 5.808823158059035485 ) ) ;
#93450 = AXIS2_PLACEMENT_3D ( 'NONE', #89039, #57137, #2700 ) ;
#93451 = CARTESIAN_POINT ( 'NONE',  ( 25.39999999999999858, -1.600000000000055600, -28.92500000000001492 ) ) ;
#93452 = DIRECTION ( 'NONE',  ( 0.7071067811865486830, -0.7071067811865464625, -0.000000000000000000 ) ) ;
#93453 = FACE_OUTER_BOUND ( 'NONE', #111932, .T. ) ;
#93454 = EDGE_LOOP ( 'NONE', ( #80601, #40517, #20910, #39502 ) ) ;
#93455 = ORIENTED_EDGE ( 'NONE', *, *, #46116, .T. ) ;
#93456 = CARTESIAN_POINT ( 'NONE',  ( 89.37500000000000000, 7.950000000000000178, 1.460391307983218535E-15 ) ) ;
#93457 = ORIENTED_EDGE ( 'NONE', *, *, #41523, .T. ) ;
#93458 = VERTEX_POINT ( 'NONE', #66985 ) ;
#93459 = EDGE_CURVE ( 'NONE', #139774, #37807, #135804, .T. ) ;
#93460 = FILL_AREA_STYLE ('',( #4228 ) ) ;
#93461 = DIRECTION ( 'NONE',  ( -0.3543493200069162685, -0.000000000000000000, -0.9351131265310288487 ) ) ;
#93462 = VECTOR ( 'NONE', #39574, 1000.000000000000000 ) ;
#93463 = LINE ( 'NONE', #17993, #43151 ) ;
#93464 = ORIENTED_EDGE ( 'NONE', *, *, #29763, .F. ) ;
#93465 = LINE ( 'NONE', #39829, #16198 ) ;
#93466 = CARTESIAN_POINT ( 'NONE',  ( -7.888753617628999938E-63, -6.350000000000004086, -3.888253587292849040E-16 ) ) ;
#93467 = LINE ( 'NONE', #62279, #127445 ) ;
#93468 = CARTESIAN_POINT ( 'NONE',  ( 126.7090635503642062, 5.466269142923943392, 3.952704227923545144 ) ) ;
#93469 = PLANE ( 'NONE',  #12306 ) ;
#93471 = VECTOR ( 'NONE', #53182, 1000.000000000000000 ) ;
#93470 = DIRECTION ( 'NONE',  ( 0.6830127018922181881, 0.6830127018922202975, -0.2588190451025214056 ) ) ;
#93472 = FACE_OUTER_BOUND ( 'NONE', #15638, .T. ) ;
#93473 = CARTESIAN_POINT ( 'NONE',  ( -14.81601139373099585, 28.73617430169776910, 5.000000000000000000 ) ) ;
#93474 = DIRECTION ( 'NONE',  ( 0.7071067811865487940, 0.7071067811865463515, 0.000000000000000000 ) ) ;
#93475 = DIRECTION ( 'NONE',  ( -0.6830127018922180770, 0.6830127018922202975, -0.2588190451025213501 ) ) ;
#93476 = DIRECTION ( 'NONE',  ( -1.000000000000000000, -0.000000000000000000, -0.000000000000000000 ) ) ;
#93477 = EDGE_CURVE ( 'NONE', #121112, #687, #107588, .T. ) ;
#93478 = DIRECTION ( 'NONE',  ( 0.7071067811865487940, 0.7071067811865463515, -0.000000000000000000 ) ) ;
#93479 = VERTEX_POINT ( 'NONE', #57551 ) ;
#93480 = ORIENTED_EDGE ( 'NONE', *, *, #16107, .T. ) ;
#93481 = CARTESIAN_POINT ( 'NONE',  ( 111.8545968585647756, -1.637169565754161615, 6.110000000000000320 ) ) ;
#93482 =( GEOMETRIC_REPRESENTATION_CONTEXT ( 3 ) GLOBAL_UNCERTAINTY_ASSIGNED_CONTEXT ( ( #23146 ) ) GLOBAL_UNIT_ASSIGNED_CONTEXT ( ( #105479, #38120, #93194 ) ) REPRESENTATION_CONTEXT ( 'NONE', 'WORKASPACE' ) );
#93483 = ORIENTED_EDGE ( 'NONE', *, *, #111853, .T. ) ;
#93484 = EDGE_CURVE ( 'NONE', #93151, #141150, #97410, .T. ) ;
#93485 = DIRECTION ( 'NONE',  ( 0.7071067811865486830, -0.7071067811865464625, -0.000000000000000000 ) ) ;
#93486 = CARTESIAN_POINT ( 'NONE',  ( 30.79289321881324781, -11.24070752338416668, 5.000000000000000000 ) ) ;
#93487 = ORIENTED_EDGE ( 'NONE', *, *, #127688, .T. ) ;
#93488 = CARTESIAN_POINT ( 'NONE',  ( 14.09068777029287567, 6.496774105546209377, 4.000000000000000000 ) ) ;
#93490 = VECTOR ( 'NONE', #135450, 999.9999999999998863 ) ;
#93489 = CARTESIAN_POINT ( 'NONE',  ( -2.671830600776449405, -0.7407075233842770334, 4.000000000000000000 ) ) ;
#93491 = CARTESIAN_POINT ( 'NONE',  ( 106.3704301918981230, -3.055000000000001492, 5.291415217122917625 ) ) ;
#93492 = VERTEX_POINT ( 'NONE', #127050 ) ;
#93493 = ADVANCED_FACE ( 'NONE', ( #84307 ), #15406, .T. ) ;
#93494 = DIRECTION ( 'NONE',  ( 1.000000000000000000, 0.000000000000000000, 0.000000000000000000 ) ) ;
#93495 = ORIENTED_EDGE ( 'NONE', *, *, #88681, .F. ) ;
#93496 = CARTESIAN_POINT ( 'NONE',  ( 16.49999999999988276, -16.53360074219757081, 5.000000000000000000 ) ) ;
#93497 = FACE_OUTER_BOUND ( 'NONE', #97658, .T. ) ;
#93498 = ORIENTED_EDGE ( 'NONE', *, *, #47396, .F. ) ;
#93499 = ORIENTED_EDGE ( 'NONE', *, *, #141453, .F. ) ;
#93500 = ADVANCED_FACE ( 'NONE', ( #48805 ), #28483, .T. ) ;
#93501 = EDGE_LOOP ( 'NONE', ( #23137, #141105, #135789, #87595 ) ) ;
#93502 = CARTESIAN_POINT ( 'NONE',  ( -51.18398860626899705, 28.73617430169823095, 5.000000000000000000 ) ) ;
#93503 = DIRECTION ( 'NONE',  ( 0.7071067811865487940, 0.7071067811865463515, 0.000000000000000000 ) ) ;
#93504 = CARTESIAN_POINT ( 'NONE',  ( 9.546236474768553748, -7.934999999999990727, 4.858786175617117713E-16 ) ) ;
#93505 = AXIS2_PLACEMENT_3D ( 'NONE', #141125, #85311, #19363 ) ;
#93506 = CARTESIAN_POINT ( 'NONE',  ( 21.58333333333333570, -5.278424836066144543, 3.047499999999995879 ) ) ;
#93507 = VECTOR ( 'NONE', #106802, 1000.000000000000000 ) ;
#93508 = CARTESIAN_POINT ( 'NONE',  ( 29.99999999999979039, -7.447814304570749222, 5.000000000000000000 ) ) ;
#93509 = ORIENTED_EDGE ( 'NONE', *, *, #103001, .T. ) ;
#93510 = ORIENTED_EDGE ( 'NONE', *, *, #102837, .T. ) ;
#93511 = PLANE ( 'NONE',  #108084 ) ;
#93512 = ORIENTED_EDGE ( 'NONE', *, *, #68300, .T. ) ;
#93513 = ORIENTED_EDGE ( 'NONE', *, *, #98621, .F. ) ;
#93514 = AXIS2_PLACEMENT_3D ( 'NONE', #44399, #58141, #23297 ) ;
#93515 = PLANE ( 'NONE',  #23984 ) ;
#93516 = DIRECTION ( 'NONE',  ( -0.7071067811865486830, -0.7071067811865464625, 0.000000000000000000 ) ) ;
#93518 = EDGE_CURVE ( 'NONE', #13228, #76266, #139404, .T. ) ;
#93517 = DIRECTION ( 'NONE',  ( -0.7071067811865486830, -0.7071067811865464625, 0.000000000000000000 ) ) ;
#93519 = ORIENTED_EDGE ( 'NONE', *, *, #8288, .T. ) ;
#93520 = VECTOR ( 'NONE', #29732, 1000.000000000000227 ) ;
#93521 = DIRECTION ( 'NONE',  ( 0.7071067811865486830, -0.7071067811865464625, -0.000000000000000000 ) ) ;
#93522 = LINE ( 'NONE', #128992, #110323 ) ;
#93523 = CARTESIAN_POINT ( 'NONE',  ( -24.48921356237309510, -27.52281430457072631, 5.000000000000000000 ) ) ;
#93524 = FACE_OUTER_BOUND ( 'NONE', #36075, .T. ) ;
#93525 = ORIENTED_EDGE ( 'NONE', *, *, #45079, .F. ) ;
#93526 = AXIS2_PLACEMENT_3D ( 'NONE', #125709, #26388, #15453 ) ;
#93527 = CARTESIAN_POINT ( 'NONE',  ( 18.48921356237309510, -27.52281430457068367, 5.000000000000000000 ) ) ;
#93528 = FACE_BOUND ( 'NONE', #110123, .T. ) ;
#93530 = ORIENTED_EDGE ( 'NONE', *, *, #127874, .F. ) ;
#93529 = AXIS2_PLACEMENT_3D ( 'NONE', #92132, #71855, #94282 ) ;
#93531 = CARTESIAN_POINT ( 'NONE',  ( 63.07919371712955581, 3.975000000000002753, -6.884901960086283523 ) ) ;
#93532 = DIRECTION ( 'NONE',  ( 0.7071067811865486830, -0.7071067811865464625, -0.000000000000000000 ) ) ;
#93533 = CARTESIAN_POINT ( 'NONE',  ( 20.51078643762690490, -27.52281430457041012, 5.000000000000000000 ) ) ;
#93534 = EDGE_CURVE ( 'NONE', #106612, #75123, #137237, .T. ) ;
#93535 = ORIENTED_EDGE ( 'NONE', *, *, #52881, .F. ) ;
#93536 = DIRECTION ( 'NONE',  ( -0.7071067811865486830, -0.7071067811865464625, -0.000000000000000000 ) ) ;
#93537 = VERTEX_POINT ( 'NONE', #104594 ) ;
#93538 = EDGE_LOOP ( 'NONE', ( #852, #122714, #27316, #23349 ) ) ;
#93539 = ORIENTED_EDGE ( 'NONE', *, *, #108630, .T. ) ;
#93540 = VECTOR ( 'NONE', #28293, 1000.000000000000227 ) ;
#93541 = CARTESIAN_POINT ( 'NONE',  ( 34.03709685856478018, -3.054999999999998828, -5.291415217122919401 ) ) ;
#93543 = ORIENTED_EDGE ( 'NONE', *, *, #107966, .F. ) ;
#93542 = AXIS2_PLACEMENT_3D ( 'NONE', #135833, #77201, #66310 ) ;
#93544 = CARTESIAN_POINT ( 'NONE',  ( 7.828169399223474656, -8.240707523384203981, 4.000000000000000000 ) ) ;
#93545 = FACE_OUTER_BOUND ( 'NONE', #91249, .T. ) ;
#93546 = CARTESIAN_POINT ( 'NONE',  ( 25.49999999999982947, 1.466399257802255329, 5.000000000000000000 ) ) ;
#93547 = EDGE_LOOP ( 'NONE', ( #96787, #27408, #54177, #8197 ) ) ;
#93548 = LINE ( 'NONE', #91417, #106986 ) ;
#93549 = CARTESIAN_POINT ( 'NONE',  ( 75.18398860626899705, 28.73617430169839793, 5.000000000000000000 ) ) ;
#93550 = AXIS2_PLACEMENT_3D ( 'NONE', #138199, #61397, #48330 ) ;
#93551 = ADVANCED_FACE ( 'NONE', ( #59011 ), #48091, .T. ) ;
#93552 = PLANE ( 'NONE',  #60762 ) ;
#93553 = LINE ( 'NONE', #37021, #24772 ) ;
#93554 = FACE_OUTER_BOUND ( 'NONE', #17505, .T. ) ;
#93555 = DIRECTION ( 'NONE',  ( 0.7071067811865487940, 0.7071067811865463515, 0.000000000000000000 ) ) ;
#93556 = LINE ( 'NONE', #17405, #77169 ) ;
#93557 = EDGE_LOOP ( 'NONE', ( #42744, #11512, #108779, #51406 ) ) ;
#93558 = ORIENTED_EDGE ( 'NONE', *, *, #22995, .F. ) ;
#93560 = ORIENTED_EDGE ( 'NONE', *, *, #135461, .T. ) ;
#93559 = VECTOR ( 'NONE', #88434, 1000.000000000000000 ) ;
#93561 = ORIENTED_EDGE ( 'NONE', *, *, #20313, .T. ) ;
#93562 = FACE_OUTER_BOUND ( 'NONE', #51580, .T. ) ;
#93563 = ORIENTED_EDGE ( 'NONE', *, *, #68229, .F. ) ;
#93564 = ADVANCED_FACE ( 'NONE', ( #93010 ), #136500, .F. ) ;
#93565 = ORIENTED_EDGE ( 'NONE', *, *, #24988, .T. ) ;
#93566 = PLANE ( 'NONE',  #63035 ) ;
#93567 = CARTESIAN_POINT ( 'NONE',  ( 81.29974487139159578, -27.71228299555262709, 4.000000000000000000 ) ) ;
#93568 = CARTESIAN_POINT ( 'NONE',  ( -6.005480084712508493, 28.92564299267933947, 4.000000000000000000 ) ) ;
#93569 = VERTEX_POINT ( 'NONE', #70589 ) ;
#93570 = DIRECTION ( 'NONE',  ( -0.7071067811865486830, 0.7071067811865464625, 0.000000000000000000 ) ) ;
#93571 = ORIENTED_EDGE ( 'NONE', *, *, #94131, .T. ) ;
#93572 = CARTESIAN_POINT ( 'NONE',  ( 56.99451991528749062, 28.92564299267978001, 4.000000000000000000 ) ) ;
#93573 = DIRECTION ( 'NONE',  ( 0.7071067811865486830, -0.7071067811865464625, -0.000000000000000000 ) ) ;
#93574 = EDGE_CURVE ( 'NONE', #106170, #96928, #39363, .T. ) ;
#93575 = CARTESIAN_POINT ( 'NONE',  ( 4.004569808101885897, 6.871911579029510442, -3.967499999999998916 ) ) ;
#93576 = ORIENTED_EDGE ( 'NONE', *, *, #98516, .T. ) ;
#93578 = DIRECTION ( 'NONE',  ( -0.000000000000000000, 0.3543493200069153248, 0.9351131265310292928 ) ) ;
#93577 = CARTESIAN_POINT ( 'NONE',  ( 105.7870968585647802, 3.054999999999997939, 5.291415217122920289 ) ) ;
#93579 = EDGE_CURVE ( 'NONE', #2946, #81677, #13, .T. ) ;
#93580 = CARTESIAN_POINT ( 'NONE',  ( 55.45435323442900710, -52.10358567239661198, -40.45860062937833845 ) ) ;
#93581 =( LENGTH_UNIT ( ) NAMED_UNIT ( * ) SI_UNIT ( .MILLI., .METRE. ) );
#93582 = EDGE_LOOP ( 'NONE', ( #31744, #112019, #84911, #61201, #21929, #7590, #81676 ) ) ;
#93583 = ORIENTED_EDGE ( 'NONE', *, *, #22202, .T. ) ;
#93584 = EDGE_CURVE ( 'NONE', #25077, #122713, #81451, .T. ) ;
#93585 = CARTESIAN_POINT ( 'NONE',  ( 48.18398860626899705, 28.73617430169820608, 5.000000000000000000 ) ) ;
#93586 = ORIENTED_EDGE ( 'NONE', *, *, #129540, .F. ) ;
#93587 = CARTESIAN_POINT ( 'NONE',  ( 57.18398860626899705, 28.73617430169827358, 5.000000000000000000 ) ) ;
#93588 = CARTESIAN_POINT ( 'NONE',  ( 68.99451991528748351, 28.92564299267986172, 4.000000000000000000 ) ) ;
#93589 = CARTESIAN_POINT ( 'NONE',  ( 75.18398860626899705, 28.73617430169839793, 5.000000000000000000 ) ) ;
#93590 = DIRECTION ( 'NONE',  ( -0.6830127018922180770, 0.6830127018922202975, -0.2588190451025213501 ) ) ;
#93591 = LINE ( 'NONE', #114602, #116461 ) ;
#93592 = EDGE_CURVE ( 'NONE', #116079, #104350, #26333, .T. ) ;
#93593 = CARTESIAN_POINT ( 'NONE',  ( 181.0498351327038336, -48.63026969829239476, -38.45492102172726590 ) ) ;
#93595 = VERTEX_POINT ( 'NONE', #105302 ) ;
#93594 = VECTOR ( 'NONE', #93720, 1000.000000000000000 ) ;
#93596 = DIRECTION ( 'NONE',  ( 0.7071067811865486830, -0.7071067811865464625, -0.000000000000000000 ) ) ;
#93597 = CARTESIAN_POINT ( 'NONE',  ( 27.70710678118635428, 8.259292476615634371, 5.000000000000000000 ) ) ;
#93598 = DIRECTION ( 'NONE',  ( 0.6830127018922181881, 0.6830127018922202975, -0.2588190451025214056 ) ) ;
#93599 = EDGE_LOOP ( 'NONE', ( #114030, #49581, #1944, #104947, #89065 ) ) ;
#93600 = CARTESIAN_POINT ( 'NONE',  ( 81.18398860626899705, 28.73617430169844056, 5.000000000000000000 ) ) ;
#93601 = DIRECTION ( 'NONE',  ( -1.000000000000000000, -1.224606353822377258E-16, -0.000000000000000000 ) ) ;
#93602 = VERTEX_POINT ( 'NONE', #5958 ) ;
#93603 = EDGE_CURVE ( 'NONE', #138830, #46125, #127944, .T. ) ;
#93605 = ORIENTED_EDGE ( 'NONE', *, *, #83958, .T. ) ;
#93604 = CARTESIAN_POINT ( 'NONE',  ( 10.25398840412855606, 22.22500000000000142, -12.12000758559782554 ) ) ;
#93606 = EDGE_CURVE ( 'NONE', #90217, #87653, #72743, .T. ) ;
#93607 = ORIENTED_EDGE ( 'NONE', *, *, #12180, .F. ) ;
#93608 = CARTESIAN_POINT ( 'NONE',  ( 33.18398860626899705, 28.73617430169810305, 5.000000000000000000 ) ) ;
#93609 = SURFACE_SIDE_STYLE ('',( #16000 ) ) ;
#93610 = CONICAL_SURFACE ( 'NONE', #114490, 2.500000000000000888, 0.9599310885968822538 ) ;
#93611 = ORIENTED_EDGE ( 'NONE', *, *, #142481, .T. ) ;
#93612 = CARTESIAN_POINT ( 'NONE',  ( 28.49999999999981171, -4.216083040037226226, -7.486842126848721968 ) ) ;
#93613 = EDGE_CURVE ( 'NONE', #5098, #115334, #54522, .T. ) ;
#93614 =( NAMED_UNIT ( * ) PLANE_ANGLE_UNIT ( ) SI_UNIT ( $, .RADIAN. ) );
#93615 = AXIS2_PLACEMENT_3D ( 'NONE', #54258, #142661, #22977 ) ;
#93616 = ORIENTED_EDGE ( 'NONE', *, *, #99976, .F. ) ;
#93617 = CARTESIAN_POINT ( 'NONE',  ( -7.171830600776418763, 18.75929247661553489, 4.000000000000000000 ) ) ;
#93619 = CARTESIAN_POINT ( 'NONE',  ( 12.69999999999999574, -22.26999999999999247, -40.00000000000000000 ) ) ;
#93618 = VECTOR ( 'NONE', #24274, 1000.000000000000227 ) ;
#93620 = LINE ( 'NONE', #80097, #60404 ) ;
#93621 = LINE ( 'NONE', #105195, #74535 ) ;
#93622 = EDGE_CURVE ( 'NONE', #66621, #22720, #129919, .T. ) ;
#93623 = DIRECTION ( 'NONE',  ( 0.000000000000000000, -1.000000000000000000, 0.000000000000000000 ) ) ;
#93624 = LINE ( 'NONE', #118189, #127055 ) ;
#93625 = CARTESIAN_POINT ( 'NONE',  ( 29.24586038379621655, 3.974999999999996980, 6.884901960086287964 ) ) ;
#93626 = CARTESIAN_POINT ( 'NONE',  ( 16.83455439249994612, 8.717631302929021331, 5.000000000000000000 ) ) ;
#93627 = ORIENTED_EDGE ( 'NONE', *, *, #114262, .T. ) ;
#93628 = EDGE_LOOP ( 'NONE', ( #111499, #29916, #90699, #86230, #72062, #23090 ) ) ;
#93629 = ORIENTED_EDGE ( 'NONE', *, *, #14210, .T. ) ;
#93630 = CARTESIAN_POINT ( 'NONE',  ( 117.5208333333333428, 7.949999999999999289, 2.130196079827431532 ) ) ;
#93631 = VERTEX_POINT ( 'NONE', #30626 ) ;
#93632 = PRESENTATION_LAYER_ASSIGNMENT (  '', '', ( #91271 ) ) ;
#93633 = ORIENTED_EDGE ( 'NONE', *, *, #30482, .F. ) ;
#93634 = ORIENTED_EDGE ( 'NONE', *, *, #1847, .F. ) ;
#93635 = EDGE_CURVE ( 'NONE', #99005, #37562, #85680, .T. ) ;
#93636 = SURFACE_SIDE_STYLE ('',( #26936 ) ) ;
#93637 = DIRECTION ( 'NONE',  ( -0.7071067811865486830, -0.7071067811865464625, -0.000000000000000000 ) ) ;
#93638 = ORIENTED_EDGE ( 'NONE', *, *, #18175, .T. ) ;
#93639 =( BOUNDED_CURVE ( )  B_SPLINE_CURVE ( 3, ( #118861, #19549, #42764, #29008 ),
 .UNSPECIFIED., .F., .T. ) 
 B_SPLINE_CURVE_WITH_KNOTS ( ( 4, 4 ),
 ( 1.864375635226942718, 1.933014472006551188 ),
 .UNSPECIFIED. ) 
 CURVE ( )  GEOMETRIC_REPRESENTATION_ITEM ( )  RATIONAL_B_SPLINE_CURVE ( ( 1.000000000000000000, 0.9996074310407765395, 0.9996074310407765395, 1.000000000000000000 ) ) 
 REPRESENTATION_ITEM ( '' )  );
#93640 = DIRECTION ( 'NONE',  ( 0.7071067811865487940, 0.7071067811865463515, 0.000000000000000000 ) ) ;
#93641 = PLANE ( 'NONE',  #94980 ) ;
#93643 = AXIS2_PLACEMENT_3D ( 'NONE', #140636, #129768, #30470 ) ;
#93642 = CARTESIAN_POINT ( 'NONE',  ( 12.51280225271498736, 3.821174125832445049E-16, 0.000000000000000000 ) ) ;
#93644 = DIRECTION ( 'NONE',  ( -0.000000000000000000, 0.3543493200069153248, 0.9351131265310292928 ) ) ;
#93645 = CARTESIAN_POINT ( 'NONE',  ( 112.2920968585647756, -5.291415217122921177, 3.054999999999999272 ) ) ;
#93646 = ORIENTED_EDGE ( 'NONE', *, *, #131093, .T. ) ;
#93647 = LINE ( 'NONE', #127710, #81241 ) ;
#93648 = CARTESIAN_POINT ( 'NONE',  ( -6.771599798802371950, -34.64999999999999147, 17.99210858042621908 ) ) ;
#93649 = DIRECTION ( 'NONE',  ( -0.000000000000000000, 0.000000000000000000, 1.000000000000000000 ) ) ;
#93650 = CARTESIAN_POINT ( 'NONE',  ( 82.47502705046287019, -5.819803920172573086, 5.819803920172573086 ) ) ;
#93651 = FILL_AREA_STYLE_COLOUR ( '', #77594 ) ;
#93652 = CARTESIAN_POINT ( 'NONE',  ( -2.999999999999981792, 18.08204922493372635, 0.9627537363044941232 ) ) ;
#93653 = DIRECTION ( 'NONE',  ( -1.000000000000000000, -0.000000000000000000, -0.000000000000000000 ) ) ;
#93654 = AXIS2_PLACEMENT_3D ( 'NONE', #20791, #97642, #98375 ) ;
#93655 = CARTESIAN_POINT ( 'NONE',  ( 33.91252705046289861, -7.949999999999998401, -4.867971026610728450E-16 ) ) ;
#93656 = EDGE_CURVE ( 'NONE', #86264, #23390, #74857, .T. ) ;
#93657 = DIRECTION ( 'NONE',  ( 0.7071067811865487940, 0.7071067811865463515, -0.000000000000000000 ) ) ;
#93658 = AXIS2_PLACEMENT_3D ( 'NONE', #101590, #100885, #33525 ) ;
#93659 = SURFACE_STYLE_USAGE ( .BOTH. , #16041 ) ;
#93660 = ORIENTED_EDGE ( 'NONE', *, *, #108980, .T. ) ;
#93661 = ORIENTED_EDGE ( 'NONE', *, *, #55183, .F. ) ;
#93662 = AXIS2_PLACEMENT_3D ( 'NONE', #90199, #121394, #135173 ) ;
#93663 = CARTESIAN_POINT ( 'NONE',  ( 38.33333333333332860, -6.884901960086287964, 3.974999999999998312 ) ) ;
#93664 = EDGE_LOOP ( 'NONE', ( #141678, #10505, #8815, #103661 ) ) ;
#93665 = CARTESIAN_POINT ( 'NONE',  ( 4.499999999999979572, -14.94781430457068083, 5.000000000000000000 ) ) ;
#93666 = LINE ( 'NONE', #126977, #84879 ) ;
#93667 = ORIENTED_EDGE ( 'NONE', *, *, #77692, .F. ) ;
#93668 = DIRECTION ( 'NONE',  ( -1.000000000000000000, 3.654646145370261567E-15, 0.000000000000000000 ) ) ;
#93669 = LINE ( 'NONE', #27673, #16534 ) ;
#93670 = LINE ( 'NONE', #50169, #76663 ) ;
#93671 = VECTOR ( 'NONE', #93180, 1000.000000000000000 ) ;
#93672 = CARTESIAN_POINT ( 'NONE',  ( 128.5370968585647802, -3.054999999999998828, -5.291415217122919401 ) ) ;
#93673 = ORIENTED_EDGE ( 'NONE', *, *, #86571, .T. ) ;
#93674 = EDGE_CURVE ( 'NONE', #29516, #445, #140771, .T. ) ;
#93675 = CARTESIAN_POINT ( 'NONE',  ( 11.20710678118646619, 6.759292476615645029, 5.000000000000000000 ) ) ;
#93676 = ORIENTED_EDGE ( 'NONE', *, *, #33946, .F. ) ;
#93677 = CARTESIAN_POINT ( 'NONE',  ( -18.48921356237309510, -27.52281430457068367, 5.000000000000000000 ) ) ;
#93678 = SURFACE_STYLE_FILL_AREA ( #40040 ) ;
#93679 = CARTESIAN_POINT ( 'NONE',  ( 63.48921356237309510, -27.52281430457099631, 5.000000000000000000 ) ) ;
#93680 = VERTEX_POINT ( 'NONE', #119033 ) ;
#93681 = CARTESIAN_POINT ( 'NONE',  ( 53.81293019189810423, -1.637169565754159617, -6.110000000000001208 ) ) ;
#93682 = ADVANCED_FACE ( 'NONE', ( #98010 ), #19716, .F. ) ;
#93683 = VERTEX_POINT ( 'NONE', #108128 ) ;
#93684 = CARTESIAN_POINT ( 'NONE',  ( 18.48921356237309510, -27.52281430457068367, 5.000000000000000000 ) ) ;
#93685 = DIRECTION ( 'NONE',  ( 0.6830127018922181881, 0.6830127018922202975, -0.2588190451025214056 ) ) ;
#93686 = CARTESIAN_POINT ( 'NONE',  ( 18.63425672184678916, 4.584330080086930965E-16, 0.000000000000000000 ) ) ;
#93687 = CARTESIAN_POINT ( 'NONE',  ( 0.7307956238753657852, -2.500000000000000000, 0.000000000000000000 ) ) ;
#93688 = CARTESIAN_POINT ( 'NONE',  ( 47.74543019189811588, -5.291415217122918513, -3.055000000000000160 ) ) ;
#93689 = VERTEX_POINT ( 'NONE', #129185 ) ;
#93690 = DIRECTION ( 'NONE',  ( 1.000000000000000000, 0.000000000000000000, 0.000000000000000000 ) ) ;
#93691 = DIRECTION ( 'NONE',  ( -0.7071067811865486830, 0.7071067811865464625, 0.000000000000000000 ) ) ;
#93692 = ORIENTED_EDGE ( 'NONE', *, *, #39811, .F. ) ;
#93693 = EDGE_LOOP ( 'NONE', ( #35456, #49968, #18698, #108105 ) ) ;
#93694 = DIRECTION ( 'NONE',  ( 1.000000000000000000, 0.000000000000000000, 0.000000000000000000 ) ) ;
#93695 = VERTEX_POINT ( 'NONE', #76262 ) ;
#93696 = AXIS2_PLACEMENT_3D ( 'NONE', #17399, #5062, #60968 ) ;
#93697 = CARTESIAN_POINT ( 'NONE',  ( 20.51159235450331764, 9.902892378096218942E-16, 0.000000000000000000 ) ) ;
#93698 = UNCERTAINTY_MEASURE_WITH_UNIT (LENGTH_MEASURE( 1.000000000000000082E-05 ), #43256, 'distance_accuracy_value', 'NONE');
#93699 = ADVANCED_FACE ( 'NONE', ( #106708 ), #42931, .F. ) ;
#93700 = VERTEX_POINT ( 'NONE', #64666 ) ;
#93701 = CARTESIAN_POINT ( 'NONE',  ( -19.49999999999985789, -19.53360074219754239, 5.000000000000000000 ) ) ;
#93702 = DIRECTION ( 'NONE',  ( 0.000000000000000000, 0.000000000000000000, 1.000000000000000000 ) ) ;
#93703 = ADVANCED_FACE ( 'NONE', ( #118306 ), #87838, .T. ) ;
#93704 = FACE_BOUND ( 'NONE', #38260, .T. ) ;
#93705 = FACE_OUTER_BOUND ( 'NONE', #83892, .T. ) ;
#93706 = LINE ( 'NONE', #114713, #123217 ) ;
#93708 = ADVANCED_FACE ( 'NONE', ( #142246 ), #9531, .F. ) ;
#93707 = CARTESIAN_POINT ( 'NONE',  ( -8.999999999999936051, -13.97847968911261241, -0.1324546996127008436 ) ) ;
#93709 = ORIENTED_EDGE ( 'NONE', *, *, #115627, .T. ) ;
#93711 = ORIENTED_EDGE ( 'NONE', *, *, #6001, .F. ) ;
#93710 = CARTESIAN_POINT ( 'NONE',  ( -23.29289321881329755, 8.259292476615625489, 5.000000000000000000 ) ) ;
#93712 = ORIENTED_EDGE ( 'NONE', *, *, #43145, .T. ) ;
#93713 = DIRECTION ( 'NONE',  ( -0.7071067811865486830, 0.7071067811865464625, 0.000000000000000000 ) ) ;
#93714 = ORIENTED_EDGE ( 'NONE', *, *, #131769, .T. ) ;
#93715 = VERTEX_POINT ( 'NONE', #8107 ) ;
#93716 = CARTESIAN_POINT ( 'NONE',  ( 61.45376352523145158, -6.109999999999998543, -3.741295971395162543E-16 ) ) ;
#93717 = ORIENTED_EDGE ( 'NONE', *, *, #132882, .F. ) ;
#93718 = CARTESIAN_POINT ( 'NONE',  ( 46.50000000000000000, 0.000000000000000000, -7.950000000000000178 ) ) ;
#93719 = AXIS2_PLACEMENT_3D ( 'NONE', #50317, #116275, #8872 ) ;
#93720 = DIRECTION ( 'NONE',  ( 0.7071067811865487940, 0.7071067811865463515, -0.000000000000000000 ) ) ;
#93721 = ORIENTED_EDGE ( 'NONE', *, *, #128352, .T. ) ;
#93722 = DIRECTION ( 'NONE',  ( -0.6830127018922180770, -0.6830127018922204085, -0.2588190451025214056 ) ) ;
#93723 = ADVANCED_FACE ( 'NONE', ( #73411 ), #18261, .F. ) ;
#93724 = DIRECTION ( 'NONE',  ( -1.000000000000000000, 0.000000000000000000, 0.000000000000000000 ) ) ;
#93725 = VECTOR ( 'NONE', #138906, 1000.000000000000000 ) ;
#93726 = DIRECTION ( 'NONE',  ( -0.000000000000000000, 0.000000000000000000, 1.000000000000000000 ) ) ;
#93727 = DIRECTION ( 'NONE',  ( -0.3543493200069162685, -0.000000000000000000, -0.9351131265310288487 ) ) ;
#93728 = CARTESIAN_POINT ( 'NONE',  ( 0.000000000000000000, 0.000000000000000000, 5.000000000000000000 ) ) ;
#93729 = ORIENTED_EDGE ( 'NONE', *, *, #138997, .F. ) ;
#93730 = VERTEX_POINT ( 'NONE', #24716 ) ;
#93731 = CARTESIAN_POINT ( 'NONE',  ( 6.852250093007166143, 2.500000000000000888, 0.000000000000000000 ) ) ;
#93732 = DIRECTION ( 'NONE',  ( -0.6830127018922181881, 0.6830127018922202975, -0.2588190451025214056 ) ) ;
#93733 = EDGE_LOOP ( 'NONE', ( #83509, #122757, #114180, #140879 ) ) ;
#93734 = EDGE_LOOP ( 'NONE', ( #117133, #9396, #60237, #57054 ) ) ;
#93735 = ORIENTED_EDGE ( 'NONE', *, *, #10804, .T. ) ;
#93736 = CARTESIAN_POINT ( 'NONE',  ( -5.999999999999960032, 10.21212019023808004, -2.019456568337786972 ) ) ;
#93737 = DIRECTION ( 'NONE',  ( -0.000000000000000000, -1.000000000000000000, -0.000000000000000000 ) ) ;
#93738 = ORIENTED_EDGE ( 'NONE', *, *, #48379, .F. ) ;
#93739 = CARTESIAN_POINT ( 'NONE',  ( 11.72733514412567857, 3.821174125832445049E-16, 0.000000000000000000 ) ) ;
#93740 = CIRCLE ( 'NONE', #28966, 2.500000000000000888 ) ;
#93741 = DIRECTION ( 'NONE',  ( -0.7071067811865486830, -0.7071067811865464625, 0.000000000000000000 ) ) ;
#93742 = VECTOR ( 'NONE', #89460, 1000.000000000000000 ) ;
#93743 = CARTESIAN_POINT ( 'NONE',  ( 5.754569808101886785, -6.871911579029512218, 3.967499999999996252 ) ) ;
#93745 = EDGE_CURVE ( 'NONE', #126076, #88152, #88576, .T. ) ;
#93744 = CONICAL_SURFACE ( 'NONE', #31264, 2.055000000000000604, 0.9599310885968764806 ) ;
#93746 = CARTESIAN_POINT ( 'NONE',  ( 24.18398860626899705, 28.73617430169804265, 5.000000000000000000 ) ) ;
#93747 = EDGE_LOOP ( 'NONE', ( #20154, #13475, #98304, #42976 ) ) ;
#93748 = VECTOR ( 'NONE', #79674, 999.9999999999998863 ) ;
#93749 = CARTESIAN_POINT ( 'NONE',  ( 6.411614905948259668, 22.22500000000000142, 4.777194822843816802 ) ) ;
#93750 = EDGE_CURVE ( 'NONE', #32455, #41056, #45792, .T. ) ;
#93751 = LINE ( 'NONE', #85005, #79061 ) ;
#93752 = CARTESIAN_POINT ( 'NONE',  ( 0.000000000000000000, 0.000000000000000000, 5.000000000000000000 ) ) ;
#93754 = ORIENTED_EDGE ( 'NONE', *, *, #111046, .F. ) ;
#93753 = LINE ( 'NONE', #4523, #37967 ) ;
#93755 = CARTESIAN_POINT ( 'NONE',  ( 13.56687199751249473, -21.74070752338406365, 6.915939825044041811 ) ) ;
#93756 = ORIENTED_EDGE ( 'NONE', *, *, #141158, .T. ) ;
#93757 = CARTESIAN_POINT ( 'NONE',  ( 27.22000000000000242, 9.521314400968980422E-16, 0.000000000000000000 ) ) ;
#93758 = DIRECTION ( 'NONE',  ( 0.000000000000000000, 0.000000000000000000, -1.000000000000000000 ) ) ;
#93759 = EDGE_CURVE ( 'NONE', #83415, #54378, #134212, .T. ) ;
#93760 = EDGE_CURVE ( 'NONE', #36959, #24621, #12406, .T. ) ;
#93761 = DIRECTION ( 'NONE',  ( -0.3543493200069162685, -0.000000000000000000, -0.9351131265310288487 ) ) ;
#93762 = VERTEX_POINT ( 'NONE', #10954 ) ;
#93763 = DIRECTION ( 'NONE',  ( -0.000000000000000000, 0.000000000000000000, 1.000000000000000000 ) ) ;
#93764 = DIRECTION ( 'NONE',  ( -0.7071067811865486830, -0.7071067811865464625, 0.000000000000000000 ) ) ;
#93765 = CARTESIAN_POINT ( 'NONE',  ( 9.489213562373095101, -27.52281430457062328, 5.000000000000000000 ) ) ;
#93766 = ORIENTED_EDGE ( 'NONE', *, *, #18616, .F. ) ;
#93767 = CARTESIAN_POINT ( 'NONE',  ( -34.92500000000001137, -8.671992264596164901, 16.70802535927751364 ) ) ;
#93768 = FACE_OUTER_BOUND ( 'NONE', #119343, .T. ) ;
#93769 = LINE ( 'NONE', #16167, #104862 ) ;
#93770 = CARTESIAN_POINT ( 'NONE',  ( 12.35051985313232237, 4.584330080086930965E-16, 0.000000000000000000 ) ) ;
#93771 = EDGE_CURVE ( 'NONE', #92747, #20850, #34907, .T. ) ;
#93772 = SURFACE_SIDE_STYLE ('',( #49588 ) ) ;
#93773 = VERTEX_POINT ( 'NONE', #22545 ) ;
#93774 = EDGE_CURVE ( 'NONE', #81952, #121450, #78398, .T. ) ;
#93775 = EDGE_LOOP ( 'NONE', ( #90965, #8355, #121020, #47065 ) ) ;
#93776 = LINE ( 'NONE', #6711, #91181 ) ;
#93777 = FACE_OUTER_BOUND ( 'NONE', #57370, .T. ) ;
#93778 = CARTESIAN_POINT ( 'NONE',  ( 4.645403141435220817, -2.126176841940958351, -7.934999999999989839 ) ) ;
#93779 = CARTESIAN_POINT ( 'NONE',  ( 15.79289321881335084, 18.75929247661553489, 5.000000000000000000 ) ) ;
#93780 = CARTESIAN_POINT ( 'NONE',  ( -34.49999999999975842, -5.945670655168998842, 4.994342998332166772 ) ) ;
#93781 = DIRECTION ( 'NONE',  ( 0.3543493200069163240, 0.000000000000000000, 0.9351131265310288487 ) ) ;
#93782 = ADVANCED_FACE ( 'NONE', ( #55953 ), #100155, .F. ) ;
#93783 = DIRECTION ( 'NONE',  ( -0.6830127018922180770, -0.6830127018922204085, -0.2588190451025213501 ) ) ;
#93784 = VERTEX_POINT ( 'NONE', #132809 ) ;
#93785 = DIRECTION ( 'NONE',  ( 1.000000000000000000, 1.224606353822377258E-16, 0.000000000000000000 ) ) ;
#93786 = LINE ( 'NONE', #25664, #74701 ) ;
#93787 = EDGE_CURVE ( 'NONE', #101003, #110282, #123348, .T. ) ;
#93788 = DIRECTION ( 'NONE',  ( 0.000000000000000000, -1.000000000000000000, 0.000000000000000000 ) ) ;
#93789 = CARTESIAN_POINT ( 'NONE',  ( 50.07876352523145158, -7.482591942790327058E-16, 6.109999999999999432 ) ) ;
#93790 = CARTESIAN_POINT ( 'NONE',  ( -5.999999999999952927, -12.41253812416063340, 4.000000000000000000 ) ) ;
#93791 = ORIENTED_EDGE ( 'NONE', *, *, #54549, .F. ) ;
#93792 = CARTESIAN_POINT ( 'NONE',  ( -26.99999999999981526, -5.527737879153217015, -7.983877177622316523 ) ) ;
#93793 = ORIENTED_EDGE ( 'NONE', *, *, #63527, .T. ) ;
#93794 = ORIENTED_EDGE ( 'NONE', *, *, #89638, .T. ) ;
#93795 = EDGE_CURVE ( 'NONE', #117989, #123895, #32401, .T. ) ;
#93796 = CARTESIAN_POINT ( 'NONE',  ( 34.42499999999998295, -21.72500000000000142, 4.500000000000000888 ) ) ;
#93797 = DIRECTION ( 'NONE',  ( 0.7071067811865487940, 0.7071067811865463515, -0.000000000000000000 ) ) ;
#93798 = PLANE ( 'NONE',  #6897 ) ;
#93799 = PLANE ( 'NONE',  #85813 ) ;
#93800 = CARTESIAN_POINT ( 'NONE',  ( 11.22916666666666430, -6.094999999999989093, 1.633150327867691542 ) ) ;
#93801 = VERTEX_POINT ( 'NONE', #35638 ) ;
#93802 = CARTESIAN_POINT ( 'NONE',  ( 30.79289321881324781, 3.759292476615681888, 5.000000000000000000 ) ) ;
#93803 = DIRECTION ( 'NONE',  ( -0.7071067811865487940, 0.7071067811865463515, -0.000000000000000000 ) ) ;
#93804 = UNCERTAINTY_MEASURE_WITH_UNIT (LENGTH_MEASURE( 1.000000000000000082E-05 ), #39029, 'distance_accuracy_value', 'NONE');
#93805 = ADVANCED_FACE ( 'NONE', ( #2214 ), #110278, .F. ) ;
#93806 = CARTESIAN_POINT ( 'NONE',  ( -17.99999999999986500, 11.96639925780213609, 5.000000000000000000 ) ) ;
#93807 = DIRECTION ( 'NONE',  ( 0.6830127018922181881, 0.6830127018922202975, -0.2588190451025214056 ) ) ;
#93808 =( BOUNDED_CURVE ( )  B_SPLINE_CURVE ( 2, ( #32219, #130110, #86613, #98189, #97447, #40266, #109769, #119207, #130841, #41655, #19196, #31504, #76451 ),
 .UNSPECIFIED., .F., .T. ) 
 B_SPLINE_CURVE_WITH_KNOTS ( ( 3, 2, 2, 2, 2, 2, 3 ),
 ( 0.04999999999999305000, 0.05277777777777043627, 0.05555555555554782948, 0.05833333333332522269, 0.06111111111110260896, 0.06388888888888000217, 0.06666666666665739538 ),
 .UNSPECIFIED. ) 
 CURVE ( )  GEOMETRIC_REPRESENTATION_ITEM ( )  RATIONAL_B_SPLINE_CURVE ( ( 1.000000000000085487, 0.9659258262889831581, 1.000000000000000000, 0.9659258262890683122, 1.000000000000000000, 0.9659258262890683122, 1.000000000000000000, 0.9659258262890683122, 1.000000000000000000, 0.9659258262890683122, 1.000000000000000000, 0.9659258262891819991, 0.9999999999998863132 ) ) 
 REPRESENTATION_ITEM ( '' )  );
#93809 = CARTESIAN_POINT ( 'NONE',  ( 104.0583603837961988, -7.949999999999996625, -2.130196079827426203 ) ) ;
#93810 = CARTESIAN_POINT ( 'NONE',  ( 66.28752705046289861, 0.000000000000000000, -7.949999999999998401 ) ) ;
#93811 = EDGE_CURVE ( 'NONE', #20222, #17540, #134225, .T. ) ;
#93812 = VECTOR ( 'NONE', #129648, 999.9999999999998863 ) ;
#93813 = CARTESIAN_POINT ( 'NONE',  ( 7.139999999999955271, -35.56014942880460694, -8.278119684037269721 ) ) ;
#93814 = EDGE_LOOP ( 'NONE', ( #3776, #18670, #102657, #8659 ) ) ;
#93815 = VERTEX_POINT ( 'NONE', #47253 ) ;
#93816 = CARTESIAN_POINT ( 'NONE',  ( 67.79166666666667140, 3.975000000000003642, -6.884901960086285300 ) ) ;
#93817 = CARTESIAN_POINT ( 'NONE',  ( 25.49999999999982592, -16.53360074219757081, 5.000000000000000000 ) ) ;
#93818 = VECTOR ( 'NONE', #102029, 999.9999999999998863 ) ;
#93819 = CARTESIAN_POINT ( 'NONE',  ( 1.320799999999990870, 1.617513492313812843E-16, 0.000000000000000000 ) ) ;
#93820 = CARTESIAN_POINT ( 'NONE',  ( 13.08638746355377158, 2.894607053745207992, 4.324337194087679137 ) ) ;
#93821 = ORIENTED_EDGE ( 'NONE', *, *, #47415, .F. ) ;
#93822 = CARTESIAN_POINT ( 'NONE',  ( -34.92499999999999005, -3.270000000000013340, -37.00000000000000000 ) ) ;
#93823 = VECTOR ( 'NONE', #97894, 999.9999999999998863 ) ;
#93824 = DIRECTION ( 'NONE',  ( -1.000000000000000000, -0.000000000000000000, -0.000000000000000000 ) ) ;
#93825 = CARTESIAN_POINT ( 'NONE',  ( 58.91709685856477563, 3.054999999999998828, 5.291415217122922066 ) ) ;
#93826 = CARTESIAN_POINT ( 'NONE',  ( 0.000000000000000000, 0.000000000000000000, 7.950000000000000178 ) ) ;
#93827 = ORIENTED_EDGE ( 'NONE', *, *, #13442, .T. ) ;
#93828 = EDGE_LOOP ( 'NONE', ( #25727, #1772, #28777, #84738 ) ) ;
#93829 = CARTESIAN_POINT ( 'NONE',  ( 34.42499999999998295, -21.72500000000000142, 0.4999999999999995559 ) ) ;
#93830 = CARTESIAN_POINT ( 'NONE',  ( -8.207106781186485733, 15.75929247661555976, 5.000000000000000000 ) ) ;
#93831 = CARTESIAN_POINT ( 'NONE',  ( -12.69999999999998153, 0.000000000000000000, 2.500000000000000444 ) ) ;
#93832 = LINE ( 'NONE', #72130, #141222 ) ;
#93833 = LINE ( 'NONE', #126448, #48844 ) ;
#93835 = ORIENTED_EDGE ( 'NONE', *, *, #129314, .F. ) ;
#93834 = CARTESIAN_POINT ( 'NONE',  ( -45.18398860626900415, 28.73617430169818832, 5.000000000000000000 ) ) ;
#93836 = LINE ( 'NONE', #125774, #4367 ) ;
#93837 = PLANE ( 'NONE',  #36213 ) ;
#93838 = DIRECTION ( 'NONE',  ( 0.6830127018922180770, -0.6830127018922204085, -0.2588190451025213501 ) ) ;
#93839 = LINE ( 'NONE', #117698, #136446 ) ;
#93840 = VECTOR ( 'NONE', #85600, 1000.000000000000000 ) ;
#93841 = VERTEX_POINT ( 'NONE', #111740 ) ;
#93842 = VECTOR ( 'NONE', #123558, 999.9999999999998863 ) ;
#93843 = AXIS2_PLACEMENT_3D ( 'NONE', #13390, #135911, #69246 ) ;
#93844 = ORIENTED_EDGE ( 'NONE', *, *, #2884, .T. ) ;
#93845 = VECTOR ( 'NONE', #78367, 1000.000000000000114 ) ;
#93846 = FACE_OUTER_BOUND ( 'NONE', #109445, .T. ) ;
#93847 = FACE_OUTER_BOUND ( 'NONE', #125026, .T. ) ;
#93848 = EDGE_CURVE ( 'NONE', #76403, #63322, #124043, .T. ) ;
#93849 = DIRECTION ( 'NONE',  ( -1.000000000000000000, -0.000000000000000000, -0.000000000000000000 ) ) ;
#93850 = CARTESIAN_POINT ( 'NONE',  ( 71.53752705046289861, -9.735942053221456900E-16, 7.949999999999998401 ) ) ;
#93851 = ORIENTED_EDGE ( 'NONE', *, *, #23184, .T. ) ;
#93852 = ORIENTED_EDGE ( 'NONE', *, *, #35989, .T. ) ;
#93853 = CARTESIAN_POINT ( 'NONE',  ( -57.18398860626899705, 28.73617430169827358, 5.000000000000000000 ) ) ;
#93854 = ORIENTED_EDGE ( 'NONE', *, *, #136752, .F. ) ;
#93855 = ORIENTED_EDGE ( 'NONE', *, *, #88009, .F. ) ;
#93856 = PLANE ( 'NONE',  #5002 ) ;
#93857 = ORIENTED_EDGE ( 'NONE', *, *, #4105, .F. ) ;
#93858 = CARTESIAN_POINT ( 'NONE',  ( 0.000000000000000000, 0.000000000000000000, 5.000000000000000000 ) ) ;
#93859 = CARTESIAN_POINT ( 'NONE',  ( 2.292893218813447209, 5.259292476615669010, 5.000000000000000000 ) ) ;
#93860 = EDGE_CURVE ( 'NONE', #45084, #139004, #99396, .T. ) ;
#93861 = FACE_BOUND ( 'NONE', #51009, .T. ) ;
#93862 = PLANE ( 'NONE',  #68793 ) ;
#93863 = DIRECTION ( 'NONE',  ( -0.000000000000000000, 1.000000000000000000, 0.000000000000000000 ) ) ;
#93864 = EDGE_CURVE ( 'NONE', #95628, #136288, #13813, .T. ) ;
#93865 = LINE ( 'NONE', #18988, #34427 ) ;
#93867 = ORIENTED_EDGE ( 'NONE', *, *, #107812, .F. ) ;
#93866 = FACE_OUTER_BOUND ( 'NONE', #86128, .T. ) ;
#93868 = EDGE_CURVE ( 'NONE', #59858, #18661, #68276, .T. ) ;
#93869 = DIRECTION ( 'NONE',  ( 0.5735764363510453823, -0.8191520442889923537, 1.003171929053525486E-16 ) ) ;
#93870 = PRODUCT_CONTEXT ( 'NONE', #53097, 'mechanical' ) ;
#93871 = ORIENTED_EDGE ( 'NONE', *, *, #67597, .F. ) ;
#93872 = ORIENTED_EDGE ( 'NONE', *, *, #35822, .F. ) ;
#93873 = CARTESIAN_POINT ( 'NONE',  ( 97.32876352523145158, 0.000000000000000000, -6.109999999999998543 ) ) ;
#93874 = ORIENTED_EDGE ( 'NONE', *, *, #68231, .F. ) ;
#93875 = EDGE_CURVE ( 'NONE', #125896, #130467, #13828, .T. ) ;
#93876 = CARTESIAN_POINT ( 'NONE',  ( 24.51665438641027350, 22.22500000000000142, 4.500000000000000888 ) ) ;
#93877 = DIRECTION ( 'NONE',  ( 0.000000000000000000, -0.3543493200069153248, -0.9351131265310291818 ) ) ;
#93878 = EDGE_CURVE ( 'NONE', #11057, #50067, #121167, .T. ) ;
#93879 = LINE ( 'NONE', #39531, #58728 ) ;
#93880 = ORIENTED_EDGE ( 'NONE', *, *, #78045, .T. ) ;
#93881 = CARTESIAN_POINT ( 'NONE',  ( 33.70710678118631165, 17.25929247661554200, 5.000000000000000000 ) ) ;
#93882 = DIRECTION ( 'NONE',  ( -0.7071067811865486830, -0.7071067811865464625, 0.000000000000000000 ) ) ;
#93883 = CARTESIAN_POINT ( 'NONE',  ( -6.770042794577893375, 21.73644205237997085, 5.000000000000000888 ) ) ;
#93885 = FACE_OUTER_BOUND ( 'NONE', #111696, .T. ) ;
#93884 = LINE ( 'NONE', #5428, #11039 ) ;
#93886 = PLANE ( 'NONE',  #16914 ) ;
#93887 = DIRECTION ( 'NONE',  ( -1.000000000000000000, -0.000000000000000000, -0.000000000000000000 ) ) ;
#93888 = EDGE_CURVE ( 'NONE', #5968, #44042, #114570, .T. ) ;
#93889 = CARTESIAN_POINT ( 'NONE',  ( 153.6500000000000057, 0.000000000000000000, 0.000000000000000000 ) ) ;
#93890 = ORIENTED_EDGE ( 'NONE', *, *, #141743, .T. ) ;
#93891 = CARTESIAN_POINT ( 'NONE',  ( -32.99451991528749062, 28.92564299267960948, 4.000000000000000000 ) ) ;
#93892 = CARTESIAN_POINT ( 'NONE',  ( 0.005480084712502889671, 28.92564299267938210, 4.000000000000000000 ) ) ;
#93893 = VERTEX_POINT ( 'NONE', #15241 ) ;
#93894 = VERTEX_POINT ( 'NONE', #25416 ) ;
#93895 = ORIENTED_EDGE ( 'NONE', *, *, #118444, .F. ) ;
#93896 = CARTESIAN_POINT ( 'NONE',  ( 43.31293019189811133, -1.637169565754159617, -6.110000000000001208 ) ) ;
#93897 = ADVANCED_FACE ( 'NONE', ( #103676 ), #125476, .F. ) ;
#93898 = ORIENTED_EDGE ( 'NONE', *, *, #19255, .T. ) ;
#93899 = AXIS2_PLACEMENT_3D ( 'NONE', #121294, #109709, #55348 ) ;
#93900 = CARTESIAN_POINT ( 'NONE',  ( 19.73330628287043709, -6.094999999999989981, -1.633150327867689100 ) ) ;
#93901 = CARTESIAN_POINT ( 'NONE',  ( -10.36538675573420676, 9.201169882002593781, -27.40968550208418364 ) ) ;
#93902 = VERTEX_POINT ( 'NONE', #26160 ) ;
#93903 = AXIS2_PLACEMENT_3D ( 'NONE', #99000, #20008, #98320 ) ;
#93904 = CARTESIAN_POINT ( 'NONE',  ( 0.000000000000000000, -0.8619312979532001151, -5.102805207349826233 ) ) ;
#93905 = EDGE_CURVE ( 'NONE', #108114, #18661, #36325, .T. ) ;
#93906 = EDGE_LOOP ( 'NONE', ( #99082, #126187, #37595, #111001 ) ) ;
#93907 = CARTESIAN_POINT ( 'NONE',  ( 23.99999999999984013, 16.93112307739201583, 4.000000000000000000 ) ) ;
#93908 = LINE ( 'NONE', #87335, #33646 ) ;
#93910 = ORIENTED_EDGE ( 'NONE', *, *, #35134, .F. ) ;
#93909 = LINE ( 'NONE', #71461, #95676 ) ;
#93911 = ORIENTED_EDGE ( 'NONE', *, *, #81805, .T. ) ;
#93912 = DIRECTION ( 'NONE',  ( 0.7071067811865487940, -0.7071067811865463515, 0.000000000000000000 ) ) ;
#93913 = FACE_OUTER_BOUND ( 'NONE', #12628, .T. ) ;
#93914 = EDGE_CURVE ( 'NONE', #87047, #128314, #59520, .T. ) ;
#93915 = ADVANCED_FACE ( 'NONE', ( #137057 ), #49367, .F. ) ;
#93916 = ORIENTED_EDGE ( 'NONE', *, *, #57686, .T. ) ;
#93917 = CARTESIAN_POINT ( 'NONE',  ( -2.292893218813438772, -0.7407075233842805861, 5.000000000000000000 ) ) ;
#93918 = ORIENTED_EDGE ( 'NONE', *, *, #85201, .T. ) ;
#93919 = VECTOR ( 'NONE', #107699, 1000.000000000000000 ) ;
#93920 = ORIENTED_EDGE ( 'NONE', *, *, #3122, .F. ) ;
#93921 = ORIENTED_EDGE ( 'NONE', *, *, #38945, .T. ) ;
#93922 = ORIENTED_EDGE ( 'NONE', *, *, #111827, .F. ) ;
#93923 = DIRECTION ( 'NONE',  ( 0.6830127018922181881, 0.6830127018922202975, -0.2588190451025214056 ) ) ;
#93924 = EDGE_CURVE ( 'NONE', #100628, #131755, #14560, .T. ) ;
#93925 = CARTESIAN_POINT ( 'NONE',  ( -21.48921356237309155, -27.52281430457070499, 5.000000000000000000 ) ) ;
#93926 = PLANE ( 'NONE',  #135071 ) ;
#93927 = ADVANCED_FACE ( 'NONE', ( #93554 ), #37022, .F. ) ;
#93928 = VERTEX_POINT ( 'NONE', #26856 ) ;
#93929 = CARTESIAN_POINT ( 'NONE',  ( 0.4892135623730947680, -27.52281430457055578, 5.000000000000000000 ) ) ;
#93930 = EDGE_LOOP ( 'NONE', ( #74569, #19245, #138739, #45499 ) ) ;
#93931 = CARTESIAN_POINT ( 'NONE',  ( -27.48921356237309155, -27.52281430457074762, 5.000000000000000000 ) ) ;
#93932 = AXIS2_PLACEMENT_3D ( 'NONE', #114333, #104139, #4803 ) ;
#93933 = CARTESIAN_POINT ( 'NONE',  ( 0.000000000000000000, 0.000000000000000000, 5.000000000000000000 ) ) ;
#93934 = LINE ( 'NONE', #117105, #117982 ) ;
#93935 = COLOUR_RGB ( '', 0.31764706, 0.68627451, 0.89019608) ;
#93936 = CARTESIAN_POINT ( 'NONE',  ( -30.70710678118632231, 5.259292476615667233, 5.000000000000000000 ) ) ;
#93937 = AXIS2_PLACEMENT_3D ( 'NONE', #125303, #91946, #45626 ) ;
#93938 = EDGE_CURVE ( 'NONE', #110962, #14269, #69690, .T. ) ;
#93939 = CARTESIAN_POINT ( 'NONE',  ( 8.423184310185783730, 4.584330080086930965E-16, 0.000000000000000000 ) ) ;
#93940 = ORIENTED_EDGE ( 'NONE', *, *, #81364, .T. ) ;
#93941 = VERTEX_POINT ( 'NONE', #92103 ) ;
#93942 = ORIENTED_EDGE ( 'NONE', *, *, #116300, .F. ) ;
#93943 = FACE_OUTER_BOUND ( 'NONE', #116260, .T. ) ;
#93944 = CARTESIAN_POINT ( 'NONE',  ( 94.72502705046289861, 5.819803920172573974, -5.819803920172573086 ) ) ;
#93945 = UNCERTAINTY_MEASURE_WITH_UNIT (LENGTH_MEASURE( 1.000000000000000082E-05 ), #44005, 'distance_accuracy_value', 'NONE');
#93946 = CARTESIAN_POINT ( 'NONE',  ( -8.999999999999937828, 10.93112307739207267, 4.000000000000000000 ) ) ;
#93947 = AXIS2_PLACEMENT_3D ( 'NONE', #64364, #53492, #76696 ) ;
#93948 = CARTESIAN_POINT ( 'NONE',  ( -34.42500000000001137, 22.22500000000000142, 0.4999999999999995559 ) ) ;
#93949 = EDGE_CURVE ( 'NONE', #66852, #135458, #58841, .T. ) ;
#93950 = CARTESIAN_POINT ( 'NONE',  ( 0.8183591370940836995, -52.14999999999999147, -41.64500000000001023 ) ) ;
#93951 = CARTESIAN_POINT ( 'NONE',  ( 78.80793019189810877, -6.109999999999999432, 1.637169565754158507 ) ) ;
#93952 = PLANE ( 'NONE',  #52141 ) ;
#93953 = CARTESIAN_POINT ( 'NONE',  ( 74.01669371712955581, 7.950000000000000178, -2.130196079827421318 ) ) ;
#93954 = CARTESIAN_POINT ( 'NONE',  ( -15.48921356237309510, -27.52281430457066236, 5.000000000000000000 ) ) ;
#93955 = CARTESIAN_POINT ( 'NONE',  ( -69.18398860626899705, 28.73617430169835529, 5.000000000000000000 ) ) ;
#93956 = DIRECTION ( 'NONE',  ( -0.000000000000000000, -0.3543493200069152693, 0.9351131265310292928 ) ) ;
#93957 = CARTESIAN_POINT ( 'NONE',  ( -47.99451991528749062, 28.92564299267971251, 4.000000000000000000 ) ) ;
#93958 = ORIENTED_EDGE ( 'NONE', *, *, #98585, .F. ) ;
#93959 = PLANE ( 'NONE',  #1313 ) ;
#93960 = ORIENTED_EDGE ( 'NONE', *, *, #127452, .F. ) ;
#93961 = CARTESIAN_POINT ( 'NONE',  ( -7.140000000000002345, -35.56014942880460694, -11.72188031596274982 ) ) ;
#93963 = VERTEX_POINT ( 'NONE', #103003 ) ;
#93962 = CARTESIAN_POINT ( 'NONE',  ( -51.29974487139158867, -27.71228299555242103, 4.000000000000000000 ) ) ;
#93964 = DIRECTION ( 'NONE',  ( -0.7071067811865486830, -0.7071067811865464625, 0.000000000000000000 ) ) ;
#93965 = CARTESIAN_POINT ( 'NONE',  ( -18.52400138585436551, 22.03583458319438648, 4.979811245910084061 ) ) ;
#93966 = VERTEX_POINT ( 'NONE', #38459 ) ;
#93967 = ORIENTED_EDGE ( 'NONE', *, *, #39427, .T. ) ;
#93968 = CARTESIAN_POINT ( 'NONE',  ( -15.29974487139158867, -27.71228299555216879, 4.000000000000000000 ) ) ;
#93969 = ORIENTED_EDGE ( 'NONE', *, *, #60393, .T. ) ;
#93970 = PLANE ( 'NONE',  #972 ) ;
#93971 = EDGE_CURVE ( 'NONE', #7076, #63600, #82684, .T. ) ;
#93972 = CARTESIAN_POINT ( 'NONE',  ( 91.37086038379622721, 6.884901960086289741, -3.974999999999993427 ) ) ;
#93973 = DIRECTION ( 'NONE',  ( -0.000000000000000000, 0.3543493200069153248, 0.9351131265310292928 ) ) ;
#93974 = PRESENTATION_STYLE_ASSIGNMENT (( #28748 ) ) ;
#93975 = VERTEX_POINT ( 'NONE', #136329 ) ;
#93976 = ADVANCED_FACE ( 'NONE', ( #126866 ), #81269, .F. ) ;
#93977 = DIRECTION ( 'NONE',  ( 0.7071067811865487940, -0.7071067811865463515, 0.000000000000000000 ) ) ;
#93978 = DIRECTION ( 'NONE',  ( -0.7071067811865486830, 0.7071067811865464625, 0.000000000000000000 ) ) ;
#93979 = CARTESIAN_POINT ( 'NONE',  ( 20.56250000000000000, 4.461849672132300881, 4.461849672132299105 ) ) ;
#93980 = CARTESIAN_POINT ( 'NONE',  ( 19.41999999999999815, 9.521314400968980422E-16, 0.000000000000000000 ) ) ;
#93981 = CARTESIAN_POINT ( 'NONE',  ( 24.39999999999999858, -7.600000000000055600, -34.92499999999998295 ) ) ;
#93982 = ORIENTED_EDGE ( 'NONE', *, *, #14047, .F. ) ;
#93983 = DIRECTION ( 'NONE',  ( 0.7071067811865486830, -0.7071067811865464625, -0.000000000000000000 ) ) ;
#93984 = ORIENTED_EDGE ( 'NONE', *, *, #113419, .T. ) ;
#93985 = CARTESIAN_POINT ( 'NONE',  ( 88.37543019189811844, -5.291415217122920289, -3.055000000000001492 ) ) ;
#93986 = DIRECTION ( 'NONE',  ( -0.000000000000000000, 0.000000000000000000, 1.000000000000000000 ) ) ;
#93987 = PLANE ( 'NONE',  #14535 ) ;
#93988 = CARTESIAN_POINT ( 'NONE',  ( 25.55334942336766346, 2.259292476615690770, 14.86850063742348560 ) ) ;
#93989 = ORIENTED_EDGE ( 'NONE', *, *, #25486, .T. ) ;
#93990 = CARTESIAN_POINT ( 'NONE',  ( 11.48334561358946360, 22.22500000000000142, 4.500000000000000888 ) ) ;
#93991 = CARTESIAN_POINT ( 'NONE',  ( 2.613322195557305605, 4.202752102959690472E-16, 0.000000000000000000 ) ) ;
#93992 = DIRECTION ( 'NONE',  ( -1.000000000000000000, -1.224606353822377258E-16, -0.000000000000000000 ) ) ;
#93993 = DIRECTION ( 'NONE',  ( 0.6830127018922180770, -0.6830127018922204085, -0.2588190451025213501 ) ) ;
#93995 = VERTEX_POINT ( 'NONE', #94251 ) ;
#93994 = CARTESIAN_POINT ( 'NONE',  ( -29.48334561358934991, 22.22500000000000142, 4.500000000000000888 ) ) ;
#93996 = CARTESIAN_POINT ( 'NONE',  ( 18.18398860626898994, 28.73617430169800002, 5.000000000000000000 ) ) ;
#93997 = CARTESIAN_POINT ( 'NONE',  ( -34.92500000000001137, 13.70193056682087196, 4.500000000000000888 ) ) ;
#93998 = LINE ( 'NONE', #27310, #114258 ) ;
#93999 = DIRECTION ( 'NONE',  ( 0.7071067811865487940, -0.7071067811865463515, 0.000000000000000000 ) ) ;
#94000 = ORIENTED_EDGE ( 'NONE', *, *, #102761, .F. ) ;
#94001 = AXIS2_PLACEMENT_3D ( 'NONE', #126560, #91799, #82382 ) ;
#94002 = ORIENTED_EDGE ( 'NONE', *, *, #97162, .F. ) ;
#94003 = CARTESIAN_POINT ( 'NONE',  ( 77.29209685856477563, -5.291415217122921177, 3.054999999999999272 ) ) ;
#94004 = VERTEX_POINT ( 'NONE', #138491 ) ;
#94005 = CONICAL_SURFACE ( 'NONE', #19903, 2.055000000000001048, 0.9599310885968758145 ) ;
#94006 = SURFACE_SIDE_STYLE ('',( #49835 ) ) ;
#94007 = CARTESIAN_POINT ( 'NONE',  ( 0.1839886062690032631, 28.73617430169787568, 5.000000000000000000 ) ) ;
#94008 = CARTESIAN_POINT ( 'NONE',  ( -30.48921356237309510, -27.52281430457076894, 5.000000000000000000 ) ) ;
#94009 = DIRECTION ( 'NONE',  ( -0.000000000000000000, 0.3543493200069153248, 0.9351131265310292928 ) ) ;
#94010 = ORIENTED_EDGE ( 'NONE', *, *, #132398, .F. ) ;
#94011 = PLANE ( 'NONE',  #72383 ) ;
#94013 = CARTESIAN_POINT ( 'NONE',  ( -33.32816939922331301, -21.74070752338406010, 4.000000000000000000 ) ) ;
#94012 =( BOUNDED_CURVE ( )  B_SPLINE_CURVE ( 3, ( #76408, #74255, #87979, #54655 ),
 .UNSPECIFIED., .F., .F. ) 
 B_SPLINE_CURVE_WITH_KNOTS ( ( 4, 4 ),
 ( 2.605825008650064500, 2.701628967222372779 ),
 .UNSPECIFIED. ) 
 CURVE ( )  GEOMETRIC_REPRESENTATION_ITEM ( )  RATIONAL_B_SPLINE_CURVE ( ( 1.000000000000000000, 0.9992352797041761381, 0.9992352797041761381, 1.000000000000000000 ) ) 
 REPRESENTATION_ITEM ( '' )  );
#94014 = EDGE_CURVE ( 'NONE', #6381, #136204, #135636, .T. ) ;
#94015 = ORIENTED_EDGE ( 'NONE', *, *, #131889, .F. ) ;
#94016 = VECTOR ( 'NONE', #129268, 1000.000000000000000 ) ;
#94017 = DIRECTION ( 'NONE',  ( -0.7071067811865487940, 0.7071067811865463515, 0.000000000000000000 ) ) ;
#94018 = DIRECTION ( 'NONE',  ( 0.000000000000000000, 0.000000000000000000, -1.000000000000000000 ) ) ;
#94019 = LINE ( 'NONE', #72335, #70124 ) ;
#94020 = ORIENTED_EDGE ( 'NONE', *, *, #23362, .F. ) ;
#94021 = ORIENTED_EDGE ( 'NONE', *, *, #64110, .F. ) ;
#94022 = EDGE_CURVE ( 'NONE', #52416, #118938, #133271, .T. ) ;
#94023 = AXIS2_PLACEMENT_3D ( 'NONE', #40387, #104152, #39672 ) ;
#94024 = PLANE ( 'NONE',  #116351 ) ;
#94025 = EDGE_CURVE ( 'NONE', #14375, #26318, #89737, .T. ) ;
#94026 = EDGE_CURVE ( 'NONE', #141895, #94686, #102773, .T. ) ;
#94027 = DIRECTION ( 'NONE',  ( 0.000000000000000000, 0.000000000000000000, 1.000000000000000000 ) ) ;
#94028 = DIRECTION ( 'NONE',  ( -0.7071067811865487940, 0.7071067811865463515, 0.000000000000000000 ) ) ;
#94029 = LINE ( 'NONE', #139723, #79050 ) ;
#94030 = DIRECTION ( 'NONE',  ( 0.7071067811865487940, 0.7071067811865463515, -0.000000000000000000 ) ) ;
#94031 = CARTESIAN_POINT ( 'NONE',  ( 53.30836038379622721, 7.949999999999996625, 2.130196079827431088 ) ) ;
#94032 = AXIS2_PLACEMENT_3D ( 'NONE', #93686, #115381, #104544 ) ;
#94034 = EDGE_CURVE ( 'NONE', #72846, #43398, #78167, .T. ) ;
#94033 = VECTOR ( 'NONE', #3097, 999.9999999999998863 ) ;
#94035 = ADVANCED_FACE ( 'NONE', ( #1963 ), #112222, .F. ) ;
#94036 = CARTESIAN_POINT ( 'NONE',  ( -29.67183060077626067, -9.740707523384182664, 4.000000000000000000 ) ) ;
#94037 = VERTEX_POINT ( 'NONE', #24479 ) ;
#94038 = VECTOR ( 'NONE', #115168, 1000.000000000000000 ) ;
#94039 = VERTEX_POINT ( 'NONE', #68729 ) ;
#94040 = VERTEX_POINT ( 'NONE', #23779 ) ;
#94041 = PRESENTATION_LAYER_ASSIGNMENT (  '', '', ( #142600 ) ) ;
#94042 = EDGE_CURVE ( 'NONE', #12475, #26153, #34679, .T. ) ;
#94043 = VERTEX_POINT ( 'NONE', #1278 ) ;
#94044 = AXIS2_PLACEMENT_3D ( 'NONE', #92718, #102909, #58741 ) ;
#94045 = SURFACE_SIDE_STYLE ('',( #28813 ) ) ;
#94046 = EDGE_CURVE ( 'NONE', #129574, #121582, #44865, .T. ) ;
#94047 = DIRECTION ( 'NONE',  ( 0.000000000000000000, 0.000000000000000000, 1.000000000000000000 ) ) ;
#94048 = VERTEX_POINT ( 'NONE', #124512 ) ;
#94049 = CARTESIAN_POINT ( 'NONE',  ( 3.707106781186514599, 11.25929247661560062, 5.000000000000000000 ) ) ;
#94050 = CARTESIAN_POINT ( 'NONE',  ( -34.92500000000001137, 21.72500000000000142, 5.000000000000000000 ) ) ;
#94051 = DIRECTION ( 'NONE',  ( 0.6830127018922180770, -0.6830127018922204085, -0.2588190451025213501 ) ) ;
#94052 = DIRECTION ( 'NONE',  ( -0.7071067811865486830, -0.7071067811865464625, 0.000000000000000000 ) ) ;
#94053 = CARTESIAN_POINT ( 'NONE',  ( 33.29974487139158867, -27.71228299555229313, 4.000000000000000000 ) ) ;
#94054 = ORIENTED_EDGE ( 'NONE', *, *, #10006, .T. ) ;
#94055 = LINE ( 'NONE', #28822, #107365 ) ;
#94056 = CARTESIAN_POINT ( 'NONE',  ( -34.92500000000001137, -22.22500000000000142, 4.000000000000000000 ) ) ;
#94057 = EDGE_LOOP ( 'NONE', ( #64497, #712, #94521, #79233 ) ) ;
#94058 = DIRECTION ( 'NONE',  ( 0.3543493200069164351, 2.781805975412904658E-17, -0.9351131265310288487 ) ) ;
#94059 = ORIENTED_EDGE ( 'NONE', *, *, #64502, .F. ) ;
#94060 = ORIENTED_EDGE ( 'NONE', *, *, #48127, .F. ) ;
#94061 = DIRECTION ( 'NONE',  ( -0.7071067811865486830, 0.7071067811865464625, 0.000000000000000000 ) ) ;
#94062 = ORIENTED_EDGE ( 'NONE', *, *, #132595, .F. ) ;
#94063 = ORIENTED_EDGE ( 'NONE', *, *, #11403, .F. ) ;
#94064 = CARTESIAN_POINT ( 'NONE',  ( 69.27126352523144703, 4.472830434245838482, 4.472830434245842035 ) ) ;
#94065 = ADVANCED_FACE ( 'NONE', ( #33952 ), #101825, .T. ) ;
#94066 = ORIENTED_EDGE ( 'NONE', *, *, #133025, .T. ) ;
#94067 = DIRECTION ( 'NONE',  ( -0.000000000000000000, 0.000000000000000000, 1.000000000000000000 ) ) ;
#94068 = PLANE ( 'NONE',  #54351 ) ;
#94069 = CARTESIAN_POINT ( 'NONE',  ( 113.0212635252314044, -4.472830434245838482, -4.472830434245840259 ) ) ;
#94070 = DIRECTION ( 'NONE',  ( -0.3543493200069162685, -0.000000000000000000, -0.9351131265310288487 ) ) ;
#94071 = PLANE ( 'NONE',  #95312 ) ;
#94072 = ADVANCED_FACE ( 'NONE', ( #22304 ), #46275, .F. ) ;
#94073 = CARTESIAN_POINT ( 'NONE',  ( -21.48921356237309155, -27.52281430457070499, 5.000000000000000000 ) ) ;
#94074 = LINE ( 'NONE', #29524, #73080 ) ;
#94075 = PRESENTATION_LAYER_ASSIGNMENT (  '', '', ( #96323 ) ) ;
#94076 = CARTESIAN_POINT ( 'NONE',  ( 15.70710678118643955, -6.740707523384209310, 5.000000000000000000 ) ) ;
#94078 = EDGE_CURVE ( 'NONE', #3326, #118907, #89052, .T. ) ;
#94077 = CARTESIAN_POINT ( 'NONE',  ( 34.47516574401890210, 4.490517612115580981, 4.998110765256833510 ) ) ;
#94079 = VERTEX_POINT ( 'NONE', #12873 ) ;
#94080 = FACE_OUTER_BOUND ( 'NONE', #35098, .T. ) ;
#94081 = ORIENTED_EDGE ( 'NONE', *, *, #27636, .T. ) ;
#94082 = ADVANCED_FACE ( 'NONE', ( #57154 ), #67291, .F. ) ;
#94083 = VERTEX_POINT ( 'NONE', #133959 ) ;
#94084 = CARTESIAN_POINT ( 'NONE',  ( -17.99451991528748351, 28.92564299267950645, 4.000000000000000000 ) ) ;
#94085 = VERTEX_POINT ( 'NONE', #55706 ) ;
#94086 = EDGE_CURVE ( 'NONE', #100760, #36504, #101328, .T. ) ;
#94087 = DIRECTION ( 'NONE',  ( 0.6830127018922181881, 0.6830127018922202975, -0.2588190451025214056 ) ) ;
#94088 = FACE_OUTER_BOUND ( 'NONE', #15557, .T. ) ;
#94089 = LINE ( 'NONE', #115098, #30157 ) ;
#94090 = LINE ( 'NONE', #50605, #74159 ) ;
#94091 = ORIENTED_EDGE ( 'NONE', *, *, #47048, .T. ) ;
#94092 = LINE ( 'NONE', #129575, #111349 ) ;
#94093 = ORIENTED_EDGE ( 'NONE', *, *, #89015, .F. ) ;
#94094 = ADVANCED_FACE ( 'NONE', ( #80324 ), #111487, .F. ) ;
#94095 = CARTESIAN_POINT ( 'NONE',  ( 5.520403141435219929, 7.934999999999989839, -2.126176841940961904 ) ) ;
#94096 = DIRECTION ( 'NONE',  ( 0.7071067811865487940, 0.7071067811865463515, 0.000000000000000000 ) ) ;
#94097 = CARTESIAN_POINT ( 'NONE',  ( -2.999999999999975131, 7.007997736742443529, -8.085015511992120096 ) ) ;
#94098 = EDGE_CURVE ( 'NONE', #20507, #2157, #11426, .T. ) ;
#94099 = DIRECTION ( 'NONE',  ( 0.7071067811865487940, 0.7071067811865463515, 0.000000000000000000 ) ) ;
#94100 = ORIENTED_EDGE ( 'NONE', *, *, #127825, .T. ) ;
#94101 = ORIENTED_EDGE ( 'NONE', *, *, #103071, .T. ) ;
#94102 = ORIENTED_EDGE ( 'NONE', *, *, #37365, .F. ) ;
#94103 = DIRECTION ( 'NONE',  ( -0.7071067811865487940, 0.7071067811865463515, -0.000000000000000000 ) ) ;
#94104 = DIRECTION ( 'NONE',  ( -0.000000000000000000, 0.000000000000000000, 1.000000000000000000 ) ) ;
#94105 = CARTESIAN_POINT ( 'NONE',  ( -42.29974487139158157, -27.71228299555235708, 4.000000000000000000 ) ) ;
#94106 = CARTESIAN_POINT ( 'NONE',  ( -54.29974487139159578, -27.71228299555243879, 4.000000000000000000 ) ) ;
#94107 = LINE ( 'NONE', #14430, #60119 ) ;
#94108 = CARTESIAN_POINT ( 'NONE',  ( 39.18398860626899705, 28.73617430169814568, 5.000000000000000000 ) ) ;
#94109 = CARTESIAN_POINT ( 'NONE',  ( -57.18398860626899705, 28.73617430169827358, 5.000000000000000000 ) ) ;
#94110 = EDGE_CURVE ( 'NONE', #72893, #120409, #36097, .T. ) ;
#94111 = VECTOR ( 'NONE', #25044, 1000.000000000000000 ) ;
#94112 = DIRECTION ( 'NONE',  ( -1.000000000000000000, 0.000000000000000000, 0.000000000000000000 ) ) ;
#94113 = CARTESIAN_POINT ( 'NONE',  ( 10.49999999999993250, 8.319652575858395238, -8.582050562765804358 ) ) ;
#94114 = VERTEX_POINT ( 'NONE', #99901 ) ;
#94115 = DIRECTION ( 'NONE',  ( 0.7071067811865487940, 0.7071067811865463515, 0.000000000000000000 ) ) ;
#94116 = FACE_OUTER_BOUND ( 'NONE', #99184, .T. ) ;
#94117 = EDGE_LOOP ( 'NONE', ( #126819, #91470, #105744, #113222 ) ) ;
#94118 = CARTESIAN_POINT ( 'NONE',  ( 9.328169399223460445, 5.259292476615662792, 4.000000000000000000 ) ) ;
#94120 = ORIENTED_EDGE ( 'NONE', *, *, #1519, .T. ) ;
#94119 = CARTESIAN_POINT ( 'NONE',  ( 55.57593013779389679, -49.04047092357291149, -39.41690992498757140 ) ) ;
#94121 = CARTESIAN_POINT ( 'NONE',  ( 7.251592354503322291, 9.902892378096218942E-16, 0.000000000000000000 ) ) ;
#94122 = CARTESIAN_POINT ( 'NONE',  ( 105.5624999999999858, -5.819803920172573086, -5.819803920172573974 ) ) ;
#94123 = ORIENTED_EDGE ( 'NONE', *, *, #77626, .T. ) ;
#94124 = DIRECTION ( 'NONE',  ( -0.7071067811865486830, 0.7071067811865463515, 0.000000000000000000 ) ) ;
#94125 = UNCERTAINTY_MEASURE_WITH_UNIT (LENGTH_MEASURE( 1.000000000000000082E-05 ), #78129, 'distance_accuracy_value', 'NONE');
#94126 = ORIENTED_EDGE ( 'NONE', *, *, #102441, .F. ) ;
#94127 = VECTOR ( 'NONE', #128796, 1000.000000000000000 ) ;
#94128 = VECTOR ( 'NONE', #134168, 999.9999999999998863 ) ;
#94129 = CARTESIAN_POINT ( 'NONE',  ( 13.49999999999991829, -17.94781430457064531, 5.000000000000000000 ) ) ;
#94130 = PLANE ( 'NONE',  #11464 ) ;
#94131 = EDGE_CURVE ( 'NONE', #5092, #111882, #118027, .T. ) ;
#94133 = CARTESIAN_POINT ( 'NONE',  ( 118.7875270504628986, 0.000000000000000000, -7.949999999999998401 ) ) ;
#94132 = VECTOR ( 'NONE', #82108, 1000.000000000000000 ) ;
#94134 = CARTESIAN_POINT ( 'NONE',  ( 9.370933818357753964, 3.821174125832445049E-16, 0.000000000000000000 ) ) ;
#94135 = DIRECTION ( 'NONE',  ( 0.7071067811865487940, -0.7071067811865463515, 0.000000000000000000 ) ) ;
#94136 = LINE ( 'NONE', #125363, #495 ) ;
#94137 = DIRECTION ( 'NONE',  ( -0.7071067811865487940, 0.7071067811865463515, -0.000000000000000000 ) ) ;
#94138 = DIRECTION ( 'NONE',  ( 0.000000000000000000, 0.000000000000000000, 1.000000000000000000 ) ) ;
#94139 = CARTESIAN_POINT ( 'NONE',  ( 28.12456980810188867, -6.871911579029512218, 3.967499999999996252 ) ) ;
#94140 = CARTESIAN_POINT ( 'NONE',  ( 5.374569808101886892, 6.871911579029510442, -3.967499999999998916 ) ) ;
#94141 = CARTESIAN_POINT ( 'NONE',  ( 22.49999999999984013, -12.08601207473287253, -10.46905243149099540 ) ) ;
#94142 = VECTOR ( 'NONE', #12838, 999.9999999999998863 ) ;
#94143 = CARTESIAN_POINT ( 'NONE',  ( -34.49999999999975842, 16.46425560840032176, 4.994342998332164107 ) ) ;
#94144 = CARTESIAN_POINT ( 'NONE',  ( 34.45011844616451668, 15.00230414159378256, 5.000000000000000888 ) ) ;
#94145 = ORIENTED_EDGE ( 'NONE', *, *, #109895, .F. ) ;
#94146 = EDGE_CURVE ( 'NONE', #106377, #16785, #84005, .T. ) ;
#94147 = EDGE_LOOP ( 'NONE', ( #16659, #104381, #30696, #119166, #1200, #29933 ) ) ;
#94148 = CARTESIAN_POINT ( 'NONE',  ( 81.06249999999998579, -5.819803920172572198, -5.819803920172573086 ) ) ;
#94149 = EDGE_CURVE ( 'NONE', #27138, #49673, #122393, .T. ) ;
#94151 = ORIENTED_EDGE ( 'NONE', *, *, #47539, .F. ) ;
#94150 = PLANE ( 'NONE',  #125384 ) ;
#94152 = EDGE_LOOP ( 'NONE', ( #5776, #116905, #50748, #40341 ) ) ;
#94153 = LINE ( 'NONE', #81910, #57295 ) ;
#94154 = LINE ( 'NONE', #26768, #92672 ) ;
#94155 = CARTESIAN_POINT ( 'NONE',  ( -36.18398860626899705, 28.73617430169812437, 5.000000000000000000 ) ) ;
#94156 = ORIENTED_EDGE ( 'NONE', *, *, #77160, .F. ) ;
#94157 = CARTESIAN_POINT ( 'NONE',  ( -27.18398860626900060, 28.73617430169806042, 5.000000000000000000 ) ) ;
#94158 = DIRECTION ( 'NONE',  ( 0.7071067811865487940, 0.7071067811865463515, 0.000000000000000000 ) ) ;
#94159 = DIRECTION ( 'NONE',  ( -0.7071067811865487940, 0.7071067811865463515, 0.000000000000000000 ) ) ;
#94160 = CARTESIAN_POINT ( 'NONE',  ( 7.499999999999954703, 10.08746187583913922, 4.000000000000000000 ) ) ;
#94161 = EDGE_CURVE ( 'NONE', #34897, #87113, #4925, .T. ) ;
#94162 = PLANE ( 'NONE',  #56348 ) ;
#94163 = DIRECTION ( 'NONE',  ( -1.084202172485504681E-16, 1.000000000000000000, 0.000000000000000000 ) ) ;
#94164 = FACE_OUTER_BOUND ( 'NONE', #21731, .T. ) ;
#94165 = LINE ( 'NONE', #71030, #38279 ) ;
#94166 = LINE ( 'NONE', #72480, #33179 ) ;
#94167 = CARTESIAN_POINT ( 'NONE',  ( -42.18398860626899705, 28.73617430169816700, 5.000000000000000000 ) ) ;
#94168 = DIRECTION ( 'NONE',  ( -0.6830127018922181881, 0.6830127018922202975, -0.2588190451025214056 ) ) ;
#94169 = CARTESIAN_POINT ( 'NONE',  ( 55.47768537940099520, -49.13871568195843764, 40.16438383193126072 ) ) ;
#94170 = ORIENTED_EDGE ( 'NONE', *, *, #42970, .T. ) ;
#94171 = ORIENTED_EDGE ( 'NONE', *, *, #10257, .F. ) ;
#94172 = CARTESIAN_POINT ( 'NONE',  ( 99.16709685856477563, -3.055000000000000160, -5.291415217122921177 ) ) ;
#94173 = AXIS2_PLACEMENT_3D ( 'NONE', #4164, #3491, #6322 ) ;
#94174 =( BOUNDED_CURVE ( )  B_SPLINE_CURVE ( 3, ( #87353, #86652, #130153, #19929 ),
 .UNSPECIFIED., .F., .T. ) 
 B_SPLINE_CURVE_WITH_KNOTS ( ( 4, 4 ),
 ( 5.920967161967927161, 7.341195215986648037 ),
 .UNSPECIFIED. ) 
 CURVE ( )  GEOMETRIC_REPRESENTATION_ITEM ( )  RATIONAL_B_SPLINE_CURVE ( ( 1.000000000000000000, 0.8388583629366591632, 0.8388583629366591632, 1.000000000000000000 ) ) 
 REPRESENTATION_ITEM ( '' )  );
#94175 = ORIENTED_EDGE ( 'NONE', *, *, #19281, .F. ) ;
#94176 = CARTESIAN_POINT ( 'NONE',  ( 21.66240673564756491, -2.337593264352435085, 2.862726108897622684E-16 ) ) ;
#94177 = VECTOR ( 'NONE', #75482, 1000.000000000000000 ) ;
#94178 = CARTESIAN_POINT ( 'NONE',  ( 8.166666666666667851, -5.278424836066145431, -3.047499999999993658 ) ) ;
#94179 = ORIENTED_EDGE ( 'NONE', *, *, #17686, .F. ) ;
#94180 = CARTESIAN_POINT ( 'NONE',  ( 75.66666666666665719, 6.884901960086285300, 3.975000000000003642 ) ) ;
#94181 = FACE_OUTER_BOUND ( 'NONE', #110321, .T. ) ;
#94182 = CARTESIAN_POINT ( 'NONE',  ( 100.9745968585647660, 1.637169565754164058, -6.109999999999996767 ) ) ;
#94183 = VERTEX_POINT ( 'NONE', #60090 ) ;
#94184 = CARTESIAN_POINT ( 'NONE',  ( 9.183988606268997046, 28.73617430169793607, 5.000000000000000000 ) ) ;
#94185 = VERTEX_POINT ( 'NONE', #137653 ) ;
#94186 = LINE ( 'NONE', #26805, #59288 ) ;
#94187 = VECTOR ( 'NONE', #58196, 1000.000000000000000 ) ;
#94188 = LINE ( 'NONE', #140552, #24031 ) ;
#94189 = PLANE ( 'NONE',  #38482 ) ;
#94190 = CARTESIAN_POINT ( 'NONE',  ( -29.99999999999979039, -21.41253812416053393, 4.000000000000000000 ) ) ;
#94191 = ADVANCED_FACE ( 'NONE', ( #17955 ), #126731, .F. ) ;
#94192 = ORIENTED_EDGE ( 'NONE', *, *, #35233, .F. ) ;
#94193 = ORIENTED_EDGE ( 'NONE', *, *, #9618, .T. ) ;
#94194 = VECTOR ( 'NONE', #10066, 1000.000000000000227 ) ;
#94195 = VERTEX_POINT ( 'NONE', #40485 ) ;
#94196 = CARTESIAN_POINT ( 'NONE',  ( -2.700255128608413990, -27.71228299555204089, 4.000000000000000000 ) ) ;
#94197 = EDGE_CURVE ( 'NONE', #55296, #47325, #60835, .T. ) ;
#94198 = DIRECTION ( 'NONE',  ( -0.000000000000000000, -0.3543493200069152693, 0.9351131265310292928 ) ) ;
#94199 = CARTESIAN_POINT ( 'NONE',  ( 6.337903141435219823, -6.871911579029513106, -3.967499999999993587 ) ) ;
#94200 = CARTESIAN_POINT ( 'NONE',  ( 13.49999999999990052, -6.839392718269117211, -8.480912228396118024 ) ) ;
#94201 = VECTOR ( 'NONE', #37198, 999.9999999999998863 ) ;
#94202 = EDGE_CURVE ( 'NONE', #79985, #125649, #104993, .T. ) ;
#94203 = EDGE_CURVE ( 'NONE', #112837, #67571, #17276, .T. ) ;
#94204 = CARTESIAN_POINT ( 'NONE',  ( -5.292893218813416567, -3.740707523384244837, 5.000000000000000000 ) ) ;
#94205 = ADVANCED_FACE ( 'NONE', ( #38328 ), #4582, .T. ) ;
#94206 = ORIENTED_EDGE ( 'NONE', *, *, #131568, .T. ) ;
#94207 = VECTOR ( 'NONE', #66254, 1000.000000000000000 ) ;
#94208 = VERTEX_POINT ( 'NONE', #7072 ) ;
#94210 = ADVANCED_FACE ( 'NONE', ( #82543 ), #71674, .F. ) ;
#94209 = CARTESIAN_POINT ( 'NONE',  ( 8.671830600776420539, 2.259292476615701428, 4.000000000000000000 ) ) ;
#94211 = ORIENTED_EDGE ( 'NONE', *, *, #30221, .F. ) ;
#94212 = EDGE_LOOP ( 'NONE', ( #126236, #13746, #128535, #65757 ) ) ;
#94213 = EDGE_CURVE ( 'NONE', #106218, #18107, #117278, .T. ) ;
#94214 = CARTESIAN_POINT ( 'NONE',  ( 110.8912635252314658, -4.472830434245838482, -4.472830434245838482 ) ) ;
#94215 = EDGE_CURVE ( 'NONE', #127624, #112797, #28163, .T. ) ;
#94216 = DIRECTION ( 'NONE',  ( -0.7071067811865486830, 0.7071067811865464625, 0.000000000000000000 ) ) ;
#94217 = DIRECTION ( 'NONE',  ( -0.000000000000000000, 0.3543493200069153248, 0.9351131265310292928 ) ) ;
#94218 = ORIENTED_EDGE ( 'NONE', *, *, #104414, .T. ) ;
#94219 = CARTESIAN_POINT ( 'NONE',  ( 6.125000000000000000, 6.094999999999989981, -1.119633336120465690E-15 ) ) ;
#94220 = DIRECTION ( 'NONE',  ( 1.000000000000000000, -0.000000000000000000, -0.000000000000000000 ) ) ;
#94221 = DIRECTION ( 'NONE',  ( -1.000000000000000000, 0.000000000000000000, 0.000000000000000000 ) ) ;
#94222 = DIRECTION ( 'NONE',  ( 0.000000000000000000, -1.000000000000000000, 0.000000000000000000 ) ) ;
#94223 = VERTEX_POINT ( 'NONE', #48478 ) ;
#94224 = EDGE_CURVE ( 'NONE', #105583, #19893, #29568, .T. ) ;
#94225 = DIRECTION ( 'NONE',  ( 0.7071067811865487940, 0.7071067811865463515, 0.000000000000000000 ) ) ;
#94227 = FACE_BOUND ( 'NONE', #15574, .T. ) ;
#94226 = VECTOR ( 'NONE', #24497, 1000.000000000000000 ) ;
#94228 = ORIENTED_EDGE ( 'NONE', *, *, #120213, .F. ) ;
#94229 = CARTESIAN_POINT ( 'NONE',  ( 13.96000000000000085, -2.055000000000000160, 2.789133085058098087E-16 ) ) ;
#94230 = LINE ( 'NONE', #71800, #129116 ) ;
#94231 = DIRECTION ( 'NONE',  ( 0.6830127018922181881, 0.6830127018922202975, -0.2588190451025214056 ) ) ;
#94232 = ORIENTED_EDGE ( 'NONE', *, *, #54184, .T. ) ;
#94233 = DIRECTION ( 'NONE',  ( 0.7071067811865487940, 0.7071067811865463515, 0.000000000000000000 ) ) ;
#94234 = ORIENTED_EDGE ( 'NONE', *, *, #6424, .F. ) ;
#94235 = ORIENTED_EDGE ( 'NONE', *, *, #101511, .F. ) ;
#94236 = ADVANCED_FACE ( 'NONE', ( #95545 ), #61539, .T. ) ;
#94237 = CIRCLE ( 'NONE', #66528, 2.500000000000000888 ) ;
#94238 = EDGE_LOOP ( 'NONE', ( #26676, #10145, #85650, #129049 ) ) ;
#94239 = VECTOR ( 'NONE', #110775, 1000.000000000000000 ) ;
#94240 = CIRCLE ( 'NONE', #91965, 5.968999999999998529 ) ;
#94241 = CARTESIAN_POINT ( 'NONE',  ( 30.68293019189811943, -1.637169565754158951, -6.109999999999998543 ) ) ;
#94242 = VERTEX_POINT ( 'NONE', #73806 ) ;
#94243 = DIRECTION ( 'NONE',  ( -0.000000000000000000, 0.3543493200069153248, 0.9351131265310292928 ) ) ;
#94244 =( LENGTH_UNIT ( ) NAMED_UNIT ( * ) SI_UNIT ( .MILLI., .METRE. ) );
#94245 = DIRECTION ( 'NONE',  ( -0.000000000000000000, 0.3543493200069153248, 0.9351131265310292928 ) ) ;
#94246 = CIRCLE ( 'NONE', #64154, 2.500000000000000444 ) ;
#94247 = DIRECTION ( 'NONE',  ( 0.6830127018922180770, -0.6830127018922204085, -0.2588190451025213501 ) ) ;
#94248 =( GEOMETRIC_REPRESENTATION_CONTEXT ( 3 ) GLOBAL_UNCERTAINTY_ASSIGNED_CONTEXT ( ( #59226 ) ) GLOBAL_UNIT_ASSIGNED_CONTEXT ( ( #90075, #56798, #75657 ) ) REPRESENTATION_CONTEXT ( 'NONE', 'WORKASPACE' ) );
#94249 = DIRECTION ( 'NONE',  ( 0.6830127018922180770, -0.6830127018922204085, -0.2588190451025213501 ) ) ;
#94250 =( LENGTH_UNIT ( ) NAMED_UNIT ( * ) SI_UNIT ( .MILLI., .METRE. ) );
#94251 = CARTESIAN_POINT ( 'NONE',  ( 26.29387692260786480, 22.22500000000000142, 4.000000000000000000 ) ) ;
#94252 = PLANE ( 'NONE',  #59899 ) ;
#94253 = DIRECTION ( 'NONE',  ( 0.7071067811865487940, 0.7071067811865463515, 0.000000000000000000 ) ) ;
#94254 = ORIENTED_EDGE ( 'NONE', *, *, #7157, .T. ) ;
#94255 = EDGE_CURVE ( 'NONE', #59374, #34536, #105685, .T. ) ;
#94256 = VERTEX_POINT ( 'NONE', #6348 ) ;
#94257 = EDGE_LOOP ( 'NONE', ( #37711, #36796, #37743, #16419 ) ) ;
#94258 = ORIENTED_EDGE ( 'NONE', *, *, #86785, .F. ) ;
#94259 = DIRECTION ( 'NONE',  ( 1.000000000000000000, 1.224606353822377258E-16, 0.000000000000000000 ) ) ;
#94260 = VERTEX_POINT ( 'NONE', #50626 ) ;
#94261 = EDGE_CURVE ( 'NONE', #111218, #91520, #94808, .T. ) ;
#94262 = ORIENTED_EDGE ( 'NONE', *, *, #86468, .F. ) ;
#94263 = DIRECTION ( 'NONE',  ( 0.000000000000000000, -1.000000000000000000, 0.000000000000000000 ) ) ;
#94264 = CARTESIAN_POINT ( 'NONE',  ( 0.7928932188134510950, -8.240707523384198652, 5.000000000000000000 ) ) ;
#94265 = DIRECTION ( 'NONE',  ( -0.7071067811865486830, -0.7071067811865464625, 0.000000000000000000 ) ) ;
#94266 = EDGE_LOOP ( 'NONE', ( #6153, #18936, #94683, #85849 ) ) ;
#94267 = VECTOR ( 'NONE', #50775, 1000.000000000000000 ) ;
#94268 = LINE ( 'NONE', #138505, #69599 ) ;
#94269 = EDGE_LOOP ( 'NONE', ( #38614, #40744, #12946, #24423 ) ) ;
#94270 = ADVANCED_FACE ( 'NONE', ( #120859 ), #120120, .F. ) ;
#94271 = LINE ( 'NONE', #29027, #120791 ) ;
#94272 = CARTESIAN_POINT ( 'NONE',  ( 5.999999999999963585, 4.384688058510572972, -7.090945410444669861 ) ) ;
#94273 = VECTOR ( 'NONE', #133796, 1000.000000000000000 ) ;
#94274 = CARTESIAN_POINT ( 'NONE',  ( 0.7962364747685526378, 7.934999999999990727, -1.457635852685135314E-15 ) ) ;
#94275 = ORIENTED_EDGE ( 'NONE', *, *, #79518, .T. ) ;
#94277 = CARTESIAN_POINT ( 'NONE',  ( 17.81601139373099940, 28.73617430169775133, 5.000000000000000000 ) ) ;
#94276 = CARTESIAN_POINT ( 'NONE',  ( 101.2662635252314374, 4.472830434245839371, -4.472830434245839371 ) ) ;
#94279 = EDGE_CURVE ( 'NONE', #9868, #6439, #75946, .T. ) ;
#94278 = DIRECTION ( 'NONE',  ( 0.3543493200069162685, -0.000000000000000000, -0.9351131265310288487 ) ) ;
#94280 = EDGE_LOOP ( 'NONE', ( #623, #65756, #64390, #31393 ) ) ;
#94281 = ORIENTED_EDGE ( 'NONE', *, *, #71274, .T. ) ;
#94282 = DIRECTION ( 'NONE',  ( 0.000000000000000000, 1.000000000000000000, 0.000000000000000000 ) ) ;
#94283 = VERTEX_POINT ( 'NONE', #96937 ) ;
#94284 = CIRCLE ( 'NONE', #3990, 2.500000000000000888 ) ;
#94285 = SURFACE_STYLE_FILL_AREA ( #49401 ) ;
#94286 = DIRECTION ( 'NONE',  ( -0.000000000000000000, 0.000000000000000000, 1.000000000000000000 ) ) ;
#94287 = DIRECTION ( 'NONE',  ( -0.7071067811865486830, -0.7071067811865464625, 0.000000000000000000 ) ) ;
#94288 = CARTESIAN_POINT ( 'NONE',  ( 3.792893218813431222, 0.7592924766157120864, 5.000000000000000000 ) ) ;
#94289 = VERTEX_POINT ( 'NONE', #44038 ) ;
#94290 = DIRECTION ( 'NONE',  ( -0.6830127018922181881, 0.6830127018922202975, -0.2588190451025214056 ) ) ;
#94291 = SURFACE_STYLE_FILL_AREA ( #92141 ) ;
#94292 = CARTESIAN_POINT ( 'NONE',  ( 0.000000000000000000, -8.151047557385066256, -8.977947279169798733 ) ) ;
#94293 = VECTOR ( 'NONE', #4969, 999.9999999999998863 ) ;
#94294 = EDGE_LOOP ( 'NONE', ( #61666, #91100, #82289, #119423 ) ) ;
#94295 = LINE ( 'NONE', #93600, #127620 ) ;
#94296 = CARTESIAN_POINT ( 'NONE',  ( -63.18398860626900415, 28.73617430169831621, 5.000000000000000000 ) ) ;
#94297 = EDGE_LOOP ( 'NONE', ( #1528, #95073, #31941, #25970 ) ) ;
#94300 = EDGE_CURVE ( 'NONE', #59468, #114684, #62956, .T. ) ;
#94299 = ORIENTED_EDGE ( 'NONE', *, *, #51693, .T. ) ;
#94298 = DIRECTION ( 'NONE',  ( 1.000000000000000000, -0.000000000000000000, 0.000000000000000000 ) ) ;
#94301 = ADVANCED_FACE ( 'NONE', ( #107133 ), #65092, .F. ) ;
#94302 = EDGE_LOOP ( 'NONE', ( #7252, #11973, #122927, #14508 ) ) ;
#94303 = CARTESIAN_POINT ( 'NONE',  ( 7.499999999999951150, 3.431123077392156162, 4.000000000000000000 ) ) ;
#94304 = CARTESIAN_POINT ( 'NONE',  ( -34.75611968250421313, -19.29434930147574079, 4.955485411084900704 ) ) ;
#94305 = ORIENTED_EDGE ( 'NONE', *, *, #56130, .F. ) ;
#94306 = DIRECTION ( 'NONE',  ( -0.7071067811865486830, 0.7071067811865464625, 0.000000000000000000 ) ) ;
#94307 = UNCERTAINTY_MEASURE_WITH_UNIT (LENGTH_MEASURE( 1.000000000000000082E-05 ), #16617, 'distance_accuracy_value', 'NONE');
#94308 = DIRECTION ( 'NONE',  ( -0.7071067811865487940, 0.7071067811865463515, 0.000000000000000000 ) ) ;
#94309 = EDGE_CURVE ( 'NONE', #142977, #63081, #76687, .T. ) ;
#94310 = DIRECTION ( 'NONE',  ( -0.000000000000000000, -0.3543493200069152693, 0.9351131265310292928 ) ) ;
#94311 = AXIS2_PLACEMENT_3D ( 'NONE', #100131, #11646, #98680 ) ;
#94312 = COLOUR_RGB ( '', 0.08235294, 0.09019608, 0.10196078) ;
#94313 = EDGE_LOOP ( 'NONE', ( #44242, #134402, #130164, #122695 ) ) ;
#94314 = PLANE ( 'NONE',  #67063 ) ;
#94315 = LINE ( 'NONE', #81335, #44313 ) ;
#94316 = LINE ( 'NONE', #50120, #108990 ) ;
#94317 = CARTESIAN_POINT ( 'NONE',  ( 18.43680103220818367, -12.74070752338415247, 9.898150129686332122 ) ) ;
#94318 = CARTESIAN_POINT ( 'NONE',  ( 6.183988606268994381, 28.73617430169791476, 5.000000000000000000 ) ) ;
#94319 = DIRECTION ( 'NONE',  ( -0.000000000000000000, 0.000000000000000000, 1.000000000000000000 ) ) ;
#94320 = CARTESIAN_POINT ( 'NONE',  ( 26.04475813788241112, 1.701477371937655247, -6.349999999999989875 ) ) ;
#94321 = LINE ( 'NONE', #40677, #148 ) ;
#94322 = EDGE_CURVE ( 'NONE', #69532, #112039, #108527, .T. ) ;
#94323 = CARTESIAN_POINT ( 'NONE',  ( -53.99451991528749062, 28.92564299267975869, 4.000000000000000000 ) ) ;
#94324 = ORIENTED_EDGE ( 'NONE', *, *, #82528, .T. ) ;
#94325 = ORIENTED_EDGE ( 'NONE', *, *, #117163, .F. ) ;
#94326 = VERTEX_POINT ( 'NONE', #132509 ) ;
#94327 = CARTESIAN_POINT ( 'NONE',  ( 114.6041666666666572, 2.130196079827422206, 7.950000000000001954 ) ) ;
#94328 = ADVANCED_FACE ( 'NONE', ( #129591 ), #31728, .F. ) ;
#94329 = ORIENTED_EDGE ( 'NONE', *, *, #36306, .T. ) ;
#94330 = ORIENTED_EDGE ( 'NONE', *, *, #129833, .F. ) ;
#94331 = ORIENTED_EDGE ( 'NONE', *, *, #80962, .F. ) ;
#94332 = DIRECTION ( 'NONE',  ( -1.000000000000000000, -0.000000000000000000, -0.000000000000000000 ) ) ;
#94333 = DIRECTION ( 'NONE',  ( 1.000000000000000000, -0.000000000000000000, -0.000000000000000000 ) ) ;
#94334 = VERTEX_POINT ( 'NONE', #87536 ) ;
#94335 = AXIS2_PLACEMENT_3D ( 'NONE', #89801, #12941, #91270 ) ;
#94336 = CARTESIAN_POINT ( 'NONE',  ( -5.994519915287488843, 28.92564299267942118, 4.000000000000000000 ) ) ;
#94337 = FACE_OUTER_BOUND ( 'NONE', #14700, .T. ) ;
#94338 = COLOUR_RGB ( '', 0.40784314, 0.44705882, 0.49803922) ;
#94339 = DIRECTION ( 'NONE',  ( 0.000000000000000000, -1.000000000000000000, 0.000000000000000000 ) ) ;
#94340 = DIRECTION ( 'NONE',  ( -0.000000000000000000, -0.3543493200069152693, 0.9351131265310292928 ) ) ;
#94341 = CARTESIAN_POINT ( 'NONE',  ( 117.2504301918981042, 3.055000000000002824, -5.291415217122919401 ) ) ;
#94342 = ORIENTED_EDGE ( 'NONE', *, *, #26515, .T. ) ;
#94343 = ADVANCED_FACE ( 'NONE', ( #75257 ), #20111, .F. ) ;
#94344 = CARTESIAN_POINT ( 'NONE',  ( -30.52400138585428380, 22.03583458319438293, 4.979811245910084949 ) ) ;
#94345 = SURFACE_STYLE_FILL_AREA ( #29097 ) ;
#94346 = DIRECTION ( 'NONE',  ( 0.3543493200069162685, -0.000000000000000000, -0.9351131265310288487 ) ) ;
#94347 = PLANE ( 'NONE',  #33621 ) ;
#94348 = AXIS2_PLACEMENT_3D ( 'NONE', #86940, #120976, #74653 ) ;
#94349 = PLANE ( 'NONE',  #116337 ) ;
#94350 = CARTESIAN_POINT ( 'NONE',  ( 40.47502705046289861, -5.819803920172572198, 5.819803920172572198 ) ) ;
#94351 = CARTESIAN_POINT ( 'NONE',  ( 18.29974487139159223, -27.71228299555219010, 4.000000000000000000 ) ) ;
#94352 = CARTESIAN_POINT ( 'NONE',  ( 62.99451991528749772, 28.92564299267982264, 4.000000000000000000 ) ) ;
#94353 = ORIENTED_EDGE ( 'NONE', *, *, #138799, .F. ) ;
#94354 = VERTEX_POINT ( 'NONE', #99090 ) ;
#94355 = CARTESIAN_POINT ( 'NONE',  ( 40.81250000000000711, 5.819803920172571310, 5.819803920172575751 ) ) ;
#94356 = ORIENTED_EDGE ( 'NONE', *, *, #49934, .F. ) ;
#94357 = DIRECTION ( 'NONE',  ( 0.6830127018922181881, 0.6830127018922202975, -0.2588190451025214056 ) ) ;
#94358 = FACE_OUTER_BOUND ( 'NONE', #33948, .T. ) ;
#94359 = AXIS2_PLACEMENT_3D ( 'NONE', #122179, #46840, #91026 ) ;
#94360 = DIRECTION ( 'NONE',  ( 1.000000000000000000, 0.000000000000000000, 0.000000000000000000 ) ) ;
#94361 = CARTESIAN_POINT ( 'NONE',  ( 0.03865117921958852176, 0.3999999999999995781, 2.083945894980139268 ) ) ;
#94362 = LINE ( 'NONE', #63901, #14003 ) ;
#94363 = CARTESIAN_POINT ( 'NONE',  ( 28.87543019189810067, -5.291415217122920289, -3.055000000000001492 ) ) ;
#94364 = VERTEX_POINT ( 'NONE', #41900 ) ;
#94365 = CARTESIAN_POINT ( 'NONE',  ( -14.51078643762690490, -27.52281430457045275, 5.000000000000000000 ) ) ;
#94366 = ORIENTED_EDGE ( 'NONE', *, *, #17501, .F. ) ;
#94367 = DIRECTION ( 'NONE',  ( -0.6830127018922180770, -0.6830127018922204085, -0.2588190451025213501 ) ) ;
#94368 = FACE_OUTER_BOUND ( 'NONE', #10939, .T. ) ;
#94369 = LINE ( 'NONE', #81402, #129733 ) ;
#94370 = ORIENTED_EDGE ( 'NONE', *, *, #139829, .F. ) ;
#94371 = CARTESIAN_POINT ( 'NONE',  ( 59.20876352523143993, -7.482591942790329030E-16, 6.110000000000001208 ) ) ;
#94372 = VERTEX_POINT ( 'NONE', #9961 ) ;
#94373 = DIRECTION ( 'NONE',  ( -0.000000000000000000, 0.000000000000000000, 1.000000000000000000 ) ) ;
#94374 = CARTESIAN_POINT ( 'NONE',  ( 12.82439460721831104, 4.202752102959690472E-16, 0.000000000000000000 ) ) ;
#94375 = CARTESIAN_POINT ( 'NONE',  ( 13.49159235450332162, 9.902892378096218942E-16, 0.000000000000000000 ) ) ;
#94376 = VECTOR ( 'NONE', #110618, 1000.000000000000000 ) ;
#94377 = DIRECTION ( 'NONE',  ( 0.7071067811865487940, 0.7071067811865463515, -0.000000000000000000 ) ) ;
#94378 = EDGE_CURVE ( 'NONE', #69087, #39740, #33195, .T. ) ;
#94379 = CARTESIAN_POINT ( 'NONE',  ( 49.78709685856478018, 3.054999999999997495, 5.291415217122919401 ) ) ;
#94380 = EDGE_CURVE ( 'NONE', #108173, #138852, #53485, .T. ) ;
#94382 = EDGE_CURVE ( 'NONE', #68681, #16426, #140927, .T. ) ;
#94381 = ORIENTED_EDGE ( 'NONE', *, *, #93860, .T. ) ;
#94383 = DIRECTION ( 'NONE',  ( -0.000000000000000000, 0.000000000000000000, 1.000000000000000000 ) ) ;
#94385 = ADVANCED_FACE ( 'NONE', ( #98415 ), #18681, .F. ) ;
#94384 = DIRECTION ( 'NONE',  ( 0.000000000000000000, 0.000000000000000000, -1.000000000000000000 ) ) ;
#94386 = ORIENTED_EDGE ( 'NONE', *, *, #88539, .T. ) ;
#94387 = ORIENTED_EDGE ( 'NONE', *, *, #49575, .F. ) ;
#94388 = CARTESIAN_POINT ( 'NONE',  ( 5.292893218813416567, 11.25929247661560595, 5.000000000000000000 ) ) ;
#94389 = ORIENTED_EDGE ( 'NONE', *, *, #48962, .T. ) ;
#94390 = EDGE_CURVE ( 'NONE', #5826, #66103, #80840, .T. ) ;
#94391 = PRODUCT_DEFINITION_SHAPE ( 'NONE', 'NONE',  #143564 ) ;
#94392 = PLANE ( 'NONE',  #141770 ) ;
#94393 = ORIENTED_EDGE ( 'NONE', *, *, #96121, .T. ) ;
#94394 = EDGE_CURVE ( 'NONE', #85293, #76586, #76175, .T. ) ;
#94395 = CARTESIAN_POINT ( 'NONE',  ( 20.99999999999985079, -3.033600742197708477, 5.000000000000000000 ) ) ;
#94396 = ADVANCED_FACE ( 'NONE', ( #96233 ), #131044, .T. ) ;
#94397 = FACE_BOUND ( 'NONE', #36231, .T. ) ;
#94398 = EDGE_CURVE ( 'NONE', #121582, #105496, #45492, .T. ) ;
#94399 = CARTESIAN_POINT ( 'NONE',  ( 0.000000000000000000, 14.87792677143809073, -11.06722581663439975 ) ) ;
#94400 = DIRECTION ( 'NONE',  ( -0.3543493200069162685, -0.000000000000000000, -0.9351131265310288487 ) ) ;
#94401 = DIRECTION ( 'NONE',  ( 0.7071067811865487940, -0.7071067811865463515, 0.000000000000000000 ) ) ;
#94402 = EDGE_LOOP ( 'NONE', ( #116583, #33852, #64835 ) ) ;
#94403 = CARTESIAN_POINT ( 'NONE',  ( 0.000000000000000000, 0.000000000000000000, 5.000000000000000000 ) ) ;
#94405 = ORIENTED_EDGE ( 'NONE', *, *, #108426, .T. ) ;
#94404 = DIRECTION ( 'NONE',  ( 0.7071067811865486830, -0.7071067811865464625, -0.000000000000000000 ) ) ;
#94406 = VERTEX_POINT ( 'NONE', #113551 ) ;
#94407 = CARTESIAN_POINT ( 'NONE',  ( -2.999999999999976463, -9.033600742197648970, 5.000000000000000000 ) ) ;
#94408 = EDGE_CURVE ( 'NONE', #91029, #86782, #90385, .T. ) ;
#94409 = ORIENTED_EDGE ( 'NONE', *, *, #27077, .T. ) ;
#94410 = VERTEX_POINT ( 'NONE', #89669 ) ;
#94411 = CARTESIAN_POINT ( 'NONE',  ( 65.39126352523145158, -4.472830434245838482, -4.472830434245838482 ) ) ;
#94412 = ORIENTED_EDGE ( 'NONE', *, *, #142945, .F. ) ;
#94413 = VECTOR ( 'NONE', #21333, 1000.000000000000000 ) ;
#94414 = DIRECTION ( 'NONE',  ( -1.000000000000000000, -0.000000000000000000, -0.000000000000000000 ) ) ;
#94415 = DIRECTION ( 'NONE',  ( -0.7071067811865486830, -0.7071067811865464625, -0.000000000000000000 ) ) ;
#94416 = ORIENTED_EDGE ( 'NONE', *, *, #21947, .T. ) ;
#94417 =( NAMED_UNIT ( * ) PLANE_ANGLE_UNIT ( ) SI_UNIT ( $, .RADIAN. ) );
#94418 = AXIS2_PLACEMENT_3D ( 'NONE', #90809, #45883, #37860 ) ;
#94419 = DIRECTION ( 'NONE',  ( -0.6830127018922180770, -0.6830127018922204085, -0.2588190451025213501 ) ) ;
#94420 = CARTESIAN_POINT ( 'NONE',  ( 101.3333333333333286, -6.884901960086287964, 3.974999999999998312 ) ) ;
#94421 = CARTESIAN_POINT ( 'NONE',  ( 27.70710678118635073, 17.25929247661554200, 5.000000000000000000 ) ) ;
#94422 = DIRECTION ( 'NONE',  ( -0.000000000000000000, 0.000000000000000000, 1.000000000000000000 ) ) ;
#94423 = CARTESIAN_POINT ( 'NONE',  ( 26.81601139373100651, 28.73617430169768738, 5.000000000000000000 ) ) ;
#94424 = ORIENTED_EDGE ( 'NONE', *, *, #102796, .F. ) ;
#94425 = EDGE_CURVE ( 'NONE', #55296, #108338, #124441, .T. ) ;
#94426 = ORIENTED_EDGE ( 'NONE', *, *, #81693, .F. ) ;
#94427 = CARTESIAN_POINT ( 'NONE',  ( -45.48921356237309510, -27.52281430457087197, 5.000000000000000000 ) ) ;
#94429 = FACE_OUTER_BOUND ( 'NONE', #102254, .T. ) ;
#94428 = AXIS2_PLACEMENT_3D ( 'NONE', #289, #1014, #22058 ) ;
#94430 = VERTEX_POINT ( 'NONE', #134633 ) ;
#94431 = ORIENTED_EDGE ( 'NONE', *, *, #33814, .T. ) ;
#94433 = VERTEX_POINT ( 'NONE', #136028 ) ;
#94432 = VECTOR ( 'NONE', #46694, 1000.000000000000000 ) ;
#94434 = DIRECTION ( 'NONE',  ( -0.7071067811865486830, -0.7071067811865464625, 0.000000000000000000 ) ) ;
#94435 = CARTESIAN_POINT ( 'NONE',  ( 15.29974487139158867, -27.71228299555216879, 4.000000000000000000 ) ) ;
#94436 = ORIENTED_EDGE ( 'NONE', *, *, #40631, .F. ) ;
#94437 = DIRECTION ( 'NONE',  ( -0.7071067811865486830, -0.7071067811865464625, 0.000000000000000000 ) ) ;
#94438 = VECTOR ( 'NONE', #84984, 1000.000000000000000 ) ;
#94439 = VECTOR ( 'NONE', #71258, 999.9999999999998863 ) ;
#94440 = EDGE_CURVE ( 'NONE', #97859, #121120, #67846, .T. ) ;
#94441 = DIRECTION ( 'NONE',  ( -1.000000000000000000, 0.000000000000000000, -0.000000000000000000 ) ) ;
#94442 = CARTESIAN_POINT ( 'NONE',  ( 12.75456980810188767, -6.871911579029512218, 3.967499999999996252 ) ) ;
#94443 = FACE_OUTER_BOUND ( 'NONE', #103750, .T. ) ;
#94444 = ORIENTED_EDGE ( 'NONE', *, *, #49627, .F. ) ;
#94445 = LINE ( 'NONE', #80921, #126144 ) ;
#94447 = ADVANCED_FACE ( 'NONE', ( #123755 ), #11355, .F. ) ;
#94446 = CARTESIAN_POINT ( 'NONE',  ( -8.510786437626906675, -27.52281430457049183, 5.000000000000000000 ) ) ;
#94448 = CARTESIAN_POINT ( 'NONE',  ( 24.64583333333333925, -1.633150327867709528, 6.094999999999979323 ) ) ;
#94450 = ORIENTED_EDGE ( 'NONE', *, *, #108097, .F. ) ;
#94449 = FACE_OUTER_BOUND ( 'NONE', #46107, .T. ) ;
#94451 = CARTESIAN_POINT ( 'NONE',  ( 9.489213562373095101, -27.52281430457062328, 5.000000000000000000 ) ) ;
#94452 = ORIENTED_EDGE ( 'NONE', *, *, #12227, .F. ) ;
#94453 = PLANE ( 'NONE',  #102863 ) ;
#94454 = LINE ( 'NONE', #93041, #39913 ) ;
#94455 = DIRECTION ( 'NONE',  ( -0.7071067811865486830, 0.7071067811865464625, 0.000000000000000000 ) ) ;
#94456 = ORIENTED_EDGE ( 'NONE', *, *, #54646, .F. ) ;
#94457 = EDGE_CURVE ( 'NONE', #96671, #99871, #35328, .T. ) ;
#94458 = FACE_OUTER_BOUND ( 'NONE', #8209, .T. ) ;
#94459 = CARTESIAN_POINT ( 'NONE',  ( 11.51078643762690490, -27.52281430457047406, 5.000000000000000000 ) ) ;
#94460 = DIRECTION ( 'NONE',  ( -0.7071067811865486830, -0.7071067811865464625, 0.000000000000000000 ) ) ;
#94461 = EDGE_LOOP ( 'NONE', ( #49471, #109503, #108376, #122172, #2843 ) ) ;
#94462 = DIRECTION ( 'NONE',  ( -0.6830127018922181881, 0.6830127018922202975, -0.2588190451025214056 ) ) ;
#94463 = LINE ( 'NONE', #27791, #134950 ) ;
#94465 = AXIS2_PLACEMENT_3D ( 'NONE', #6714, #50998, #82919 ) ;
#94464 = DIRECTION ( 'NONE',  ( -1.000000000000000000, -1.224606353822377258E-16, -0.000000000000000000 ) ) ;
#94466 = FACE_OUTER_BOUND ( 'NONE', #68670, .T. ) ;
#94467 = LINE ( 'NONE', #114777, #34584 ) ;
#94469 = EDGE_CURVE ( 'NONE', #134257, #49377, #121573, .T. ) ;
#94468 = ORIENTED_EDGE ( 'NONE', *, *, #29548, .F. ) ;
#94470 = ORIENTED_EDGE ( 'NONE', *, *, #44479, .F. ) ;
#94471 = VECTOR ( 'NONE', #34180, 999.9999999999998863 ) ;
#94472 = PLANE ( 'NONE',  #102753 ) ;
#94473 = CARTESIAN_POINT ( 'NONE',  ( 174.7500000000000000, 7.919999999999947526, -18.97500000000001918 ) ) ;
#94474 = CARTESIAN_POINT ( 'NONE',  ( 0.9995698081018862258, -3.967499999999998028, -6.871911579029511330 ) ) ;
#94475 = CARTESIAN_POINT ( 'NONE',  ( -8.816011393731004731, 28.73617430169781173, 5.000000000000000000 ) ) ;
#94476 = CARTESIAN_POINT ( 'NONE',  ( 10.49999999999992717, -10.91253812416064584, 4.000000000000000000 ) ) ;
#94477 = LINE ( 'NONE', #6012, #122370 ) ;
#94478 = FACE_OUTER_BOUND ( 'NONE', #42918, .T. ) ;
#94479 = ORIENTED_EDGE ( 'NONE', *, *, #136249, .T. ) ;
#94480 = DIRECTION ( 'NONE',  ( 0.7071067811865486830, -0.7071067811865464625, -0.000000000000000000 ) ) ;
#94481 = DIRECTION ( 'NONE',  ( 0.7071067811865487940, 0.7071067811865463515, -0.000000000000000000 ) ) ;
#94482 = DIRECTION ( 'NONE',  ( 3.166071393695993333E-32, -1.016133275908817741E-16, 1.000000000000000000 ) ) ;
#94483 = VECTOR ( 'NONE', #116723, 1000.000000000000000 ) ;
#94484 = CARTESIAN_POINT ( 'NONE',  ( 18.18398860626898994, 28.73617430169800002, 5.000000000000000000 ) ) ;
#94485 = CARTESIAN_POINT ( 'NONE',  ( 45.70376352523145158, 6.109999999999999432, 1.122388791418549108E-15 ) ) ;
#94486 = FACE_OUTER_BOUND ( 'NONE', #111648, .T. ) ;
#94487 = AXIS2_PLACEMENT_3D ( 'NONE', #101084, #92332, #48152 ) ;
#94488 = VERTEX_POINT ( 'NONE', #58537 ) ;
#94489 = EDGE_CURVE ( 'NONE', #110945, #116780, #88981, .T. ) ;
#94490 = VERTEX_POINT ( 'NONE', #133207 ) ;
#94491 = ORIENTED_EDGE ( 'NONE', *, *, #29107, .F. ) ;
#94492 = CARTESIAN_POINT ( 'NONE',  ( 30.70710678118633652, -3.740707523384241728, 5.000000000000000000 ) ) ;
#94493 = CARTESIAN_POINT ( 'NONE',  ( -8.292893218813395251, -9.740707523384186217, 5.000000000000000000 ) ) ;
#94494 = CARTESIAN_POINT ( 'NONE',  ( -15.48921356237309510, -27.52281430457066236, 5.000000000000000000 ) ) ;
#94495 = CARTESIAN_POINT ( 'NONE',  ( 29.99451991528749417, 28.92564299267958816, 4.000000000000000000 ) ) ;
#94496 = EDGE_CURVE ( 'NONE', #107904, #37138, #12809, .T. ) ;
#94497 = CARTESIAN_POINT ( 'NONE',  ( 0.000000000000000000, 0.000000000000000000, 10.00000000000000000 ) ) ;
#94498 = CARTESIAN_POINT ( 'NONE',  ( 12.25000000000000000, -7.464222240803106570E-16, -6.094999999999989981 ) ) ;
#94499 = ORIENTED_EDGE ( 'NONE', *, *, #32440, .F. ) ;
#94500 = ADVANCED_FACE ( 'NONE', ( #102705 ), #24415, .F. ) ;
#94501 = DIRECTION ( 'NONE',  ( -0.7071067811865486830, -0.7071067811865464625, -0.000000000000000000 ) ) ;
#94502 = CARTESIAN_POINT ( 'NONE',  ( 5.671830600776430309, 14.25929247661557397, 4.000000000000000000 ) ) ;
#94503 = DIRECTION ( 'NONE',  ( -0.7071067811865486830, -0.7071067811865464625, 0.000000000000000000 ) ) ;
#94504 = PLANE ( 'NONE',  #21888 ) ;
#94505 = LINE ( 'NONE', #72103, #68910 ) ;
#94506 = CARTESIAN_POINT ( 'NONE',  ( 61.76669371712955581, -7.949999999999999289, 2.130196079827424427 ) ) ;
#94507 = DIRECTION ( 'NONE',  ( 1.000000000000000000, 0.000000000000000000, 0.000000000000000000 ) ) ;
#94508 = ORIENTED_EDGE ( 'NONE', *, *, #36440, .F. ) ;
#94509 = ORIENTED_EDGE ( 'NONE', *, *, #17255, .F. ) ;
#94510 = AXIS2_PLACEMENT_3D ( 'NONE', #62538, #89270, #66805 ) ;
#94511 = CARTESIAN_POINT ( 'NONE',  ( 63.41666666666666430, -6.884901960086287076, -3.975000000000000977 ) ) ;
#94512 = DIRECTION ( 'NONE',  ( -0.6830127018922180770, -0.6830127018922204085, -0.2588190451025213501 ) ) ;
#94513 = FACE_OUTER_BOUND ( 'NONE', #82114, .T. ) ;
#94514 = VERTEX_POINT ( 'NONE', #135349 ) ;
#94515 = EDGE_CURVE ( 'NONE', #87542, #60854, #115438, .T. ) ;
#94516 = FACE_OUTER_BOUND ( 'NONE', #97805, .T. ) ;
#94517 = AXIS2_PLACEMENT_3D ( 'NONE', #122636, #134986, #79186 ) ;
#94518 = DIRECTION ( 'NONE',  ( 0.7071067811865486830, -0.7071067811865464625, -0.000000000000000000 ) ) ;
#94519 = CARTESIAN_POINT ( 'NONE',  ( 56.87543019189809712, -5.291415217122920289, -3.055000000000001492 ) ) ;
#94520 = CARTESIAN_POINT ( 'NONE',  ( 0.4598383894973967490, 18.75929247661552779, 8.305906642995486422 ) ) ;
#94521 = ORIENTED_EDGE ( 'NONE', *, *, #93291, .T. ) ;
#94522 = ORIENTED_EDGE ( 'NONE', *, *, #123216, .F. ) ;
#94523 = CARTESIAN_POINT ( 'NONE',  ( 13.60986171580761805, 2.055000000000001048, 2.516649172247811554E-16 ) ) ;
#94524 = CIRCLE ( 'NONE', #62273, 2.500000000000000444 ) ;
#94525 = AXIS2_PLACEMENT_3D ( 'NONE', #123199, #79730, #15101 ) ;
#94526 = CARTESIAN_POINT ( 'NONE',  ( 2.510786437626908008, -27.52281430457053446, 5.000000000000000000 ) ) ;
#94527 = DIRECTION ( 'NONE',  ( -0.000000000000000000, 0.000000000000000000, 1.000000000000000000 ) ) ;
#94528 = VECTOR ( 'NONE', #114873, 999.9999999999998863 ) ;
#94529 = CARTESIAN_POINT ( 'NONE',  ( -8.999999999999932498, -12.41253812416062985, 4.000000000000000000 ) ) ;
#94530 = DIRECTION ( 'NONE',  ( -0.000000000000000000, -0.000000000000000000, 1.000000000000000000 ) ) ;
#94532 = ORIENTED_EDGE ( 'NONE', *, *, #90760, .T. ) ;
#94531 = CARTESIAN_POINT ( 'NONE',  ( -16.84537971347776875, -0.2749361969536389116, -34.34141757107727244 ) ) ;
#94533 = CARTESIAN_POINT ( 'NONE',  ( 13.60986171580761805, -2.055000000000000160, 2.789133085058097101E-16 ) ) ;
#94534 = DIRECTION ( 'NONE',  ( -0.000000000000000000, -0.3543493200069152693, 0.9351131265310292928 ) ) ;
#94535 = CARTESIAN_POINT ( 'NONE',  ( 66.29974487139159578, -27.71228299555252406, 4.000000000000000000 ) ) ;
#94536 = VECTOR ( 'NONE', #86958, 1000.000000000000000 ) ;
#94537 = LINE ( 'NONE', #129312, #87805 ) ;
#94538 = VERTEX_POINT ( 'NONE', #55632 ) ;
#94539 = EDGE_CURVE ( 'NONE', #474, #12595, #91131, .T. ) ;
#94540 = ORIENTED_EDGE ( 'NONE', *, *, #9687, .T. ) ;
#94541 = CARTESIAN_POINT ( 'NONE',  ( 39.29974487139159578, -27.71228299555233576, 4.000000000000000000 ) ) ;
#94542 = ADVANCED_FACE ( 'NONE', ( #80255 ), #68661, .F. ) ;
#94543 = DIRECTION ( 'NONE',  ( 0.7071067811865487940, 0.7071067811865463515, -0.000000000000000000 ) ) ;
#94544 = CARTESIAN_POINT ( 'NONE',  ( -0.4616035537057042171, -9.740707523384180888, 17.74957260769610556 ) ) ;
#94545 = FACE_OUTER_BOUND ( 'NONE', #115254, .T. ) ;
#94546 = FACE_OUTER_BOUND ( 'NONE', #36517, .T. ) ;
#94547 = ORIENTED_EDGE ( 'NONE', *, *, #103061, .F. ) ;
#94548 = VERTEX_POINT ( 'NONE', #111414 ) ;
#94549 = VECTOR ( 'NONE', #45145, 1000.000000000000000 ) ;
#94550 = FACE_OUTER_BOUND ( 'NONE', #86680, .T. ) ;
#94551 = PRESENTATION_STYLE_ASSIGNMENT (( #39497 ) ) ;
#94552 = ORIENTED_EDGE ( 'NONE', *, *, #103217, .T. ) ;
#94553 = EDGE_CURVE ( 'NONE', #90432, #52479, #112844, .T. ) ;
#94554 = EDGE_CURVE ( 'NONE', #1418, #27121, #12098, .T. ) ;
#94555 = ORIENTED_EDGE ( 'NONE', *, *, #125066, .F. ) ;
#94556 = VECTOR ( 'NONE', #41187, 1000.000000000000000 ) ;
#94557 = DIRECTION ( 'NONE',  ( -0.3543493200069162685, -0.000000000000000000, -0.9351131265310288487 ) ) ;
#94558 = ORIENTED_EDGE ( 'NONE', *, *, #46004, .T. ) ;
#94559 = DIRECTION ( 'NONE',  ( 0.7071067811865486830, -0.7071067811865464625, -0.000000000000000000 ) ) ;
#94560 = CARTESIAN_POINT ( 'NONE',  ( 24.18398860626899705, 28.73617430169804265, 5.000000000000000000 ) ) ;
#94561 = AXIS2_PLACEMENT_3D ( 'NONE', #93253, #46951, #80964 ) ;
#94562 = MECHANICAL_DESIGN_GEOMETRIC_PRESENTATION_REPRESENTATION (  '', ( #83004 ), #62209 ) ;
#94563 = EDGE_CURVE ( 'NONE', #132778, #110801, #133897, .T. ) ;
#94564 = FACE_BOUND ( 'NONE', #109394, .T. ) ;
#94565 = EDGE_CURVE ( 'NONE', #120820, #22653, #61385, .T. ) ;
#94566 = DIRECTION ( 'NONE',  ( 0.3543493200069162685, -0.000000000000000000, -0.9351131265310288487 ) ) ;
#94567 = CARTESIAN_POINT ( 'NONE',  ( 184.1500000000000057, -14.29000000000013593, 12.69999999999954632 ) ) ;
#94569 = ORIENTED_EDGE ( 'NONE', *, *, #78248, .T. ) ;
#94568 = DIRECTION ( 'NONE',  ( 0.000000000000000000, 0.000000000000000000, 1.000000000000000000 ) ) ;
#94570 =( LENGTH_UNIT ( ) NAMED_UNIT ( * ) SI_UNIT ( .MILLI., .METRE. ) );
#94572 = EDGE_CURVE ( 'NONE', #98820, #26598, #27993, .T. ) ;
#94571 = APPLICATION_PROTOCOL_DEFINITION ( 'draft international standard', 'automotive_design', 1998, #65216 ) ;
#94573 = ORIENTED_EDGE ( 'NONE', *, *, #15629, .T. ) ;
#94574 = EDGE_LOOP ( 'NONE', ( #100859, #15500, #68183, #91416 ) ) ;
#94575 = CARTESIAN_POINT ( 'NONE',  ( 94.26626352523143737, 4.472830434245838482, -4.472830434245837594 ) ) ;
#94576 = ORIENTED_EDGE ( 'NONE', *, *, #125526, .F. ) ;
#94577 = DIRECTION ( 'NONE',  ( 0.7071067811865487940, -0.7071067811865463515, 0.000000000000000000 ) ) ;
#94578 = CARTESIAN_POINT ( 'NONE',  ( 53.99451991528749062, 28.92564299267975869, 4.000000000000000000 ) ) ;
#94579 = ADVANCED_FACE ( 'NONE', ( #59234 ), #59921, .F. ) ;
#94580 = AXIS2_PLACEMENT_3D ( 'NONE', #130877, #31544, #10475 ) ;
#94581 = DIRECTION ( 'NONE',  ( 0.7071067811865486830, -0.7071067811865464625, -0.000000000000000000 ) ) ;
#94582 = AXIS2_PLACEMENT_3D ( 'NONE', #142998, #87900, #88637 ) ;
#94583 = CARTESIAN_POINT ( 'NONE',  ( 21.18398860626899349, 28.73617430169802134, 5.000000000000000000 ) ) ;
#94584 = VERTEX_POINT ( 'NONE', #103382 ) ;
#94585 = CARTESIAN_POINT ( 'NONE',  ( 11.81601139373100651, 28.73617430169779041, 5.000000000000000000 ) ) ;
#94586 = CARTESIAN_POINT ( 'NONE',  ( 153.6500000000000057, 0.000000000000000000, 0.000000000000000000 ) ) ;
#94587 = PLANE ( 'NONE',  #115186 ) ;
#94589 = CARTESIAN_POINT ( 'NONE',  ( 25.78501580275793970, -3.740707523384241728, 15.76143240460129924 ) ) ;
#94588 = DIRECTION ( 'NONE',  ( -1.000000000000000000, -0.000000000000000000, -0.000000000000000000 ) ) ;
#94590 = LINE ( 'NONE', #57913, #58574 ) ;
#94591 = CARTESIAN_POINT ( 'NONE',  ( 30.48921356237309510, -27.52281430457076894, 5.000000000000000000 ) ) ;
#94592 = EDGE_CURVE ( 'NONE', #91502, #122835, #48312, .T. ) ;
#94593 = LINE ( 'NONE', #82325, #12176 ) ;
#94594 = ORIENTED_EDGE ( 'NONE', *, *, #78212, .T. ) ;
#94595 = PLANE ( 'NONE',  #51922 ) ;
#94596 = DIRECTION ( 'NONE',  ( 0.6830127018922180770, -0.6830127018922204085, -0.2588190451025213501 ) ) ;
#94597 = VERTEX_POINT ( 'NONE', #50467 ) ;
#94598 = ORIENTED_EDGE ( 'NONE', *, *, #117622, .T. ) ;
#94599 = ORIENTED_EDGE ( 'NONE', *, *, #61517, .T. ) ;
#94600 = EDGE_CURVE ( 'NONE', #53640, #100336, #125892, .T. ) ;
#94601 = CARTESIAN_POINT ( 'NONE',  ( 40.83376352523143993, 6.110000000000001208, 1.122388791418549305E-15 ) ) ;
#94602 = EDGE_CURVE ( 'NONE', #50248, #71285, #83091, .T. ) ;
#94603 = ORIENTED_EDGE ( 'NONE', *, *, #115269, .F. ) ;
#94604 = ADVANCED_FACE ( 'NONE', ( #71506 ), #27503, .T. ) ;
#94605 = CARTESIAN_POINT ( 'NONE',  ( 19.58747294953710849, -6.094999999999989981, 3.732111120401553285E-16 ) ) ;
#94606 = CARTESIAN_POINT ( 'NONE',  ( -7.578096315150903095, 10.89383722895850504, -26.41284878744174947 ) ) ;
#94607 = VERTEX_POINT ( 'NONE', #136736 ) ;
#94608 = FACE_OUTER_BOUND ( 'NONE', #130705, .T. ) ;
#94609 = EDGE_LOOP ( 'NONE', ( #86961, #88628, #103075 ) ) ;
#94610 = LINE ( 'NONE', #129384, #88138 ) ;
#94611 = LINE ( 'NONE', #128688, #121558 ) ;
#94613 = ORIENTED_EDGE ( 'NONE', *, *, #83670, .F. ) ;
#94612 = LINE ( 'NONE', #29360, #10001 ) ;
#94614 = ORIENTED_EDGE ( 'NONE', *, *, #17787, .F. ) ;
#94615 = PLANE ( 'NONE',  #74675 ) ;
#94616 = CARTESIAN_POINT ( 'NONE',  ( 31.49999999999978684, -17.56887692260763956, 4.000000000000000000 ) ) ;
#94617 = VERTEX_POINT ( 'NONE', #6902 ) ;
#94618 = CARTESIAN_POINT ( 'NONE',  ( 31.49999999999977973, -4.533600742197683608, 5.000000000000000000 ) ) ;
#94619 = ORIENTED_EDGE ( 'NONE', *, *, #121990, .F. ) ;
#94620 = EDGE_LOOP ( 'NONE', ( #26652, #120200, #141157, #128896 ) ) ;
#94621 = ORIENTED_EDGE ( 'NONE', *, *, #20545, .T. ) ;
#94622 = ORIENTED_EDGE ( 'NONE', *, *, #20299, .F. ) ;
#94623 = CARTESIAN_POINT ( 'NONE',  ( -6.299744871391586898, -27.71228299555210484, 4.000000000000000000 ) ) ;
#94624 = AXIS2_PLACEMENT_3D ( 'NONE', #103668, #98867, #121340 ) ;
#94625 = VECTOR ( 'NONE', #15616, 1000.000000000000000 ) ;
#94626 = AXIS2_PLACEMENT_3D ( 'NONE', #92073, #13078, #101528 ) ;
#94627 = CARTESIAN_POINT ( 'NONE',  ( 16.27785539607886633, 0.000000000000000000, 2.500000000000000444 ) ) ;
#94628 = VECTOR ( 'NONE', #64458, 1000.000000000000000 ) ;
#94629 = DIRECTION ( 'NONE',  ( 0.7071067811865486830, -0.7071067811865464625, -0.000000000000000000 ) ) ;
#94630 = LINE ( 'NONE', #62048, #143242 ) ;
#94631 = VERTEX_POINT ( 'NONE', #127293 ) ;
#94632 = PLANE ( 'NONE',  #27963 ) ;
#94633 = ORIENTED_EDGE ( 'NONE', *, *, #74970, .F. ) ;
#94634 = PRESENTATION_LAYER_ASSIGNMENT (  '', '', ( #117493 ) ) ;
#94635 = CARTESIAN_POINT ( 'NONE',  ( 1.171830600776465392, 18.75929247661552779, 4.000000000000000000 ) ) ;
#94636 =( BOUNDED_CURVE ( )  B_SPLINE_CURVE ( 2, ( #66029, #42841, #131256, #7305, #120331, #65317, #109501, #95764, #129821, #77613, #24626, #57297, #100769 ),
 .UNSPECIFIED., .F., .T. ) 
 B_SPLINE_CURVE_WITH_KNOTS ( ( 3, 2, 2, 2, 2, 2, 3 ),
 ( 0.3500000000000000333, 0.3527777777777778567, 0.3555555555555556246, 0.3583333333333333925, 0.3611111111111111605, 0.3638888888888889284, 0.3666666666666666963 ),
 .UNSPECIFIED. ) 
 CURVE ( )  GEOMETRIC_REPRESENTATION_ITEM ( )  RATIONAL_B_SPLINE_CURVE ( ( 0.9999999999999993339, 0.9659258262890689783, 1.000000000000000000, 0.9659258262890683122, 1.000000000000000000, 0.9659258262890683122, 1.000000000000000000, 0.9659258262890683122, 1.000000000000000000, 0.9659258262890683122, 1.000000000000000000, 0.9659258262890676461, 1.000000000000000666 ) ) 
 REPRESENTATION_ITEM ( '' )  );
#94637 = CARTESIAN_POINT ( 'NONE',  ( 34.10373647476854586, 5.808823158059036373, 5.808823158059032821 ) ) ;
#94638 = DIRECTION ( 'NONE',  ( -1.000000000000000000, -1.224606353822377258E-16, -0.000000000000000000 ) ) ;
#94639 = DIRECTION ( 'NONE',  ( 0.6830127018922180770, -0.6830127018922204085, -0.2588190451025213501 ) ) ;
#94640 = LINE ( 'NONE', #82375, #74464 ) ;
#94641 = ORIENTED_EDGE ( 'NONE', *, *, #38003, .T. ) ;
#94642 = EDGE_LOOP ( 'NONE', ( #114551, #26339, #47850, #21395 ) ) ;
#94643 = EDGE_LOOP ( 'NONE', ( #33339, #117243, #140464, #7219, #110239 ) ) ;
#94644 = LINE ( 'NONE', #27982, #20881 ) ;
#94645 = DIRECTION ( 'NONE',  ( 0.7071067811865487940, -0.7071067811865463515, 0.000000000000000000 ) ) ;
#94646 = CARTESIAN_POINT ( 'NONE',  ( -26.99451991528749417, 28.92564299267956685, 4.000000000000000000 ) ) ;
#94647 = VECTOR ( 'NONE', #127673, 1000.000000000000000 ) ;
#94648 = DIRECTION ( 'NONE',  ( -1.000000000000000000, -1.224606353822377258E-16, -0.000000000000000000 ) ) ;
#94649 = CARTESIAN_POINT ( 'NONE',  ( 79.24543019189810877, -5.291415217122919401, -3.055000000000000604 ) ) ;
#94650 = CARTESIAN_POINT ( 'NONE',  ( 80.91666666666667140, -6.884901960086287076, -3.975000000000000977 ) ) ;
#94652 = DIRECTION ( 'NONE',  ( 0.000000000000000000, -1.000000000000000000, 0.000000000000000000 ) ) ;
#94651 = VECTOR ( 'NONE', #70830, 999.9999999999998863 ) ;
#94653 = CARTESIAN_POINT ( 'NONE',  ( -51.48921356237309510, -27.52281430457091460, 5.000000000000000000 ) ) ;
#94654 = CARTESIAN_POINT ( 'NONE',  ( 2.924914550060625729, -2.500000000000000000, 3.061616997868383634E-16 ) ) ;
#94655 = CARTESIAN_POINT ( 'NONE',  ( 23.99999999999983302, 19.55218569542896390, 5.000000000000000000 ) ) ;
#94656 = ORIENTED_EDGE ( 'NONE', *, *, #108227, .T. ) ;
#94657 = DIRECTION ( 'NONE',  ( 0.7071067811865487940, 0.7071067811865463515, 0.000000000000000000 ) ) ;
#94658 = ORIENTED_EDGE ( 'NONE', *, *, #80918, .F. ) ;
#94659 = VECTOR ( 'NONE', #13160, 1000.000000000000227 ) ;
#94660 = VECTOR ( 'NONE', #69372, 1000.000000000000000 ) ;
#94661 = CARTESIAN_POINT ( 'NONE',  ( -6.299744871391586898, -27.71228299555210484, 4.000000000000000000 ) ) ;
#94663 = EDGE_LOOP ( 'NONE', ( #42475, #39459, #50836, #36328, #112415, #71968, #3707, #33132, #10071, #3633, #31335, #118713, #143, #132477, #86641 ) ) ;
#94662 = LINE ( 'NONE', #93962, #62682 ) ;
#94664 = EDGE_CURVE ( 'NONE', #127365, #52144, #26564, .T. ) ;
#94665 = CARTESIAN_POINT ( 'NONE',  ( -2.939889289559783681, -9.740707523384180888, 10.89222023123381788 ) ) ;
#94666 = DIRECTION ( 'NONE',  ( 0.6830127018922181881, 0.6830127018922202975, -0.2588190451025214056 ) ) ;
#94667 = ORIENTED_EDGE ( 'NONE', *, *, #66597, .F. ) ;
#94668 = EDGE_CURVE ( 'NONE', #23904, #45259, #38170, .T. ) ;
#94669 = ORIENTED_EDGE ( 'NONE', *, *, #16840, .F. ) ;
#94670 = FILL_AREA_STYLE ('',( #7666 ) ) ;
#94671 = CARTESIAN_POINT ( 'NONE',  ( 121.1208603837962272, -6.884901960086286188, 3.974999999999997424 ) ) ;
#94672 = VECTOR ( 'NONE', #118004, 1000.000000000000227 ) ;
#94673 = CARTESIAN_POINT ( 'NONE',  ( -33.79333936457824450, 21.75929247661549581, 4.998822639870701856 ) ) ;
#94674 = CARTESIAN_POINT ( 'NONE',  ( 91.95419371712957002, 6.884901960086283523, 3.975000000000002753 ) ) ;
#94675 = CARTESIAN_POINT ( 'NONE',  ( -12.87485380690758063, -14.24070752338413648, 9.401115078912688716 ) ) ;
#94676 = VERTEX_POINT ( 'NONE', #116431 ) ;
#94677 = EDGE_CURVE ( 'NONE', #49642, #103979, #104089, .T. ) ;
#94678 = DIRECTION ( 'NONE',  ( 0.3543493200069164351, 2.781805975412904658E-17, -0.9351131265310288487 ) ) ;
#94679 = CARTESIAN_POINT ( 'NONE',  ( 15.48921356237309510, -27.52281430457066236, 5.000000000000000000 ) ) ;
#94680 = CARTESIAN_POINT ( 'NONE',  ( 19.10416666666666430, -1.633150327867691987, -6.094999999999989093 ) ) ;
#94681 = AXIS2_PLACEMENT_3D ( 'NONE', #44147, #76053, #143435 ) ;
#94682 = CARTESIAN_POINT ( 'NONE',  ( -18.00548008471250583, 28.92564299267925776, 4.000000000000000000 ) ) ;
#94683 = ORIENTED_EDGE ( 'NONE', *, *, #22513, .T. ) ;
#94684 = ADVANCED_FACE ( 'NONE', ( #138186 ), #95382, .T. ) ;
#94685 = DIRECTION ( 'NONE',  ( -0.7071067811865487940, 0.7071067811865463515, 0.000000000000000000 ) ) ;
#94686 = VERTEX_POINT ( 'NONE', #15633 ) ;
#94687 = CARTESIAN_POINT ( 'NONE',  ( 82.39626352523143282, 4.472830434245840259, -4.472830434245839371 ) ) ;
#94688 = LINE ( 'NONE', #86712, #59354 ) ;
#94689 = DIRECTION ( 'NONE',  ( -1.000000000000000000, 0.000000000000000000, 0.000000000000000000 ) ) ;
#94690 = LINE ( 'NONE', #20514, #119572 ) ;
#94691 = ORIENTED_EDGE ( 'NONE', *, *, #32857, .T. ) ;
#94692 = EDGE_CURVE ( 'NONE', #108003, #97591, #80956, .T. ) ;
#94693 = DIRECTION ( 'NONE',  ( -1.000000000000000000, -0.000000000000000000, -0.000000000000000000 ) ) ;
#94694 = FACE_OUTER_BOUND ( 'NONE', #81994, .T. ) ;
#94695 = FACE_OUTER_BOUND ( 'NONE', #18496, .T. ) ;
#94697 = EDGE_LOOP ( 'NONE', ( #85245, #8530, #112945, #46781 ) ) ;
#94696 = DIRECTION ( 'NONE',  ( -0.000000000000000000, 1.000000000000000000, -0.000000000000000000 ) ) ;
#94698 = DIRECTION ( 'NONE',  ( -0.6830127018922181881, 0.6830127018922202975, -0.2588190451025214056 ) ) ;
#94699 = CARTESIAN_POINT ( 'NONE',  ( -22.82900182742193351, 7.795401085224272109, 5.000000000000000000 ) ) ;
#94700 =( NAMED_UNIT ( * ) SI_UNIT ( $, .STERADIAN. ) SOLID_ANGLE_UNIT ( ) );
#94701 = SURFACE_SIDE_STYLE ('',( #74424 ) ) ;
#94702 = ORIENTED_EDGE ( 'NONE', *, *, #57413, .T. ) ;
#94703 = EDGE_LOOP ( 'NONE', ( #38148, #78471, #7904, #121428 ) ) ;
#94704 = CARTESIAN_POINT ( 'NONE',  ( 76.27126352523144703, 4.472830434245839371, 4.472830434245842035 ) ) ;
#94705 = ORIENTED_EDGE ( 'NONE', *, *, #82453, .T. ) ;
#94706 = CARTESIAN_POINT ( 'NONE',  ( -24.48921356237309510, -27.52281430457072631, 5.000000000000000000 ) ) ;
#94707 = EDGE_CURVE ( 'NONE', #130915, #97535, #5498, .T. ) ;
#94708 = CARTESIAN_POINT ( 'NONE',  ( -13.49999999999990763, 22.22500000000000142, 4.362957392718799454 ) ) ;
#94709 = DIRECTION ( 'NONE',  ( 0.7071067811865486830, -0.7071067811865464625, -0.000000000000000000 ) ) ;
#94710 = ORIENTED_EDGE ( 'NONE', *, *, #23206, .F. ) ;
#94711 = DIRECTION ( 'NONE',  ( -0.7071067811865487940, 0.7071067811865463515, -0.000000000000000000 ) ) ;
#94712 = CARTESIAN_POINT ( 'NONE',  ( 16.49230000000001084, 3.130000000000008331, -2.396719511207313368E-16 ) ) ;
#94713 = ADVANCED_FACE ( 'NONE', ( #104829 ), #125157, .T. ) ;
#94714 = EDGE_CURVE ( 'NONE', #140579, #72813, #60668, .T. ) ;
#94715 = ORIENTED_EDGE ( 'NONE', *, *, #4622, .T. ) ;
#94716 = LINE ( 'NONE', #83910, #116076 ) ;
#94717 = LINE ( 'NONE', #81771, #94127 ) ;
#94718 = DIRECTION ( 'NONE',  ( 0.6830127018922181881, 0.6830127018922202975, -0.2588190451025214056 ) ) ;
#94719 =( GEOMETRIC_REPRESENTATION_CONTEXT ( 3 ) GLOBAL_UNCERTAINTY_ASSIGNED_CONTEXT ( ( #140341 ) ) GLOBAL_UNIT_ASSIGNED_CONTEXT ( ( #94244, #39905, #127605 ) ) REPRESENTATION_CONTEXT ( 'NONE', 'WORKASPACE' ) );
#94720 = VECTOR ( 'NONE', #39416, 999.9999999999998863 ) ;
#94721 = VECTOR ( 'NONE', #122908, 1000.000000000000000 ) ;
#94722 = ADVANCED_FACE ( 'NONE', ( #72967 ), #117124, .T. ) ;
#94723 = ORIENTED_EDGE ( 'NONE', *, *, #80787, .F. ) ;
#94724 = VERTEX_POINT ( 'NONE', #62783 ) ;
#94725 = AXIS2_PLACEMENT_3D ( 'NONE', #139008, #138290, #38967 ) ;
#94726 = EDGE_CURVE ( 'NONE', #140742, #53886, #96765, .T. ) ;
#94727 = EDGE_CURVE ( 'NONE', #111382, #98928, #85937, .T. ) ;
#94728 = CARTESIAN_POINT ( 'NONE',  ( -60.48921356237309510, -27.52281430457097500, 5.000000000000000000 ) ) ;
#94729 = PLANE ( 'NONE',  #13781 ) ;
#94730 = CARTESIAN_POINT ( 'NONE',  ( 25.39999999999999858, -5.938110122598772023, -4.485947909153642499 ) ) ;
#94731 = CARTESIAN_POINT ( 'NONE',  ( -21.48921356237309155, -27.52281430457070499, 5.000000000000000000 ) ) ;
#94732 = DIRECTION ( 'NONE',  ( -1.000000000000000000, 0.000000000000000000, -0.000000000000000000 ) ) ;
#94733 = CARTESIAN_POINT ( 'NONE',  ( 0.000000000000000000, 0.000000000000000000, 5.000000000000000000 ) ) ;
#94734 = EDGE_LOOP ( 'NONE', ( #131493, #98978, #139881, #42690 ) ) ;
#94735 = ORIENTED_EDGE ( 'NONE', *, *, #93795, .T. ) ;
#94736 = ORIENTED_EDGE ( 'NONE', *, *, #56229, .T. ) ;
#94737 = EDGE_CURVE ( 'NONE', #76243, #81473, #130175, .T. ) ;
#94738 = MANIFOLD_SOLID_BREP ( 'Base-Revolve', #37076 ) ;
#94739 = ORIENTED_EDGE ( 'NONE', *, *, #85299, .T. ) ;
#94740 = AXIS2_PLACEMENT_3D ( 'NONE', #88278, #142648, #132526 ) ;
#94741 = AXIS2_PLACEMENT_3D ( 'NONE', #41570, #30729, #47685 ) ;
#94742 = EDGE_CURVE ( 'NONE', #13302, #22212, #131593, .T. ) ;
#94743 = DIRECTION ( 'NONE',  ( 0.000000000000000000, 0.000000000000000000, 1.000000000000000000 ) ) ;
#94744 = AXIS2_PLACEMENT_3D ( 'NONE', #9633, #19808, #62628 ) ;
#94745 = LINE ( 'NONE', #137572, #126148 ) ;
#94746 = ORIENTED_EDGE ( 'NONE', *, *, #69908, .T. ) ;
#94747 = DIRECTION ( 'NONE',  ( -1.000000000000000000, -0.000000000000000000, -0.000000000000000000 ) ) ;
#94748 = DIRECTION ( 'NONE',  ( 0.6830127018922180770, -0.6830127018922204085, -0.2588190451025213501 ) ) ;
#94749 = DIRECTION ( 'NONE',  ( 0.3543493200069162685, -0.000000000000000000, -0.9351131265310288487 ) ) ;
#94750 = DIRECTION ( 'NONE',  ( -0.7071067811865486830, -0.7071067811865464625, 0.000000000000000000 ) ) ;
#94751 = VECTOR ( 'NONE', #86552, 1000.000000000000000 ) ;
#94752 = CARTESIAN_POINT ( 'NONE',  ( 26.99999999999998934, -5.093796677280518104, -4.382233278760884865 ) ) ;
#94753 = VERTEX_POINT ( 'NONE', #75792 ) ;
#94754 = AXIS2_PLACEMENT_3D ( 'NONE', #111246, #22101, #66358 ) ;
#94755 = CARTESIAN_POINT ( 'NONE',  ( 2.207106781186527478, -5.240707523384232402, 5.000000000000000000 ) ) ;
#94756 = DIRECTION ( 'NONE',  ( 0.7071067811865486830, -0.7071067811865464625, -0.000000000000000000 ) ) ;
#94757 = AXIS2_PLACEMENT_3D ( 'NONE', #21763, #10157, #97896 ) ;
#94758 = VERTEX_POINT ( 'NONE', #109833 ) ;
#94759 = DIRECTION ( 'NONE',  ( 0.7071067811865486830, -0.7071067811865464625, -0.000000000000000000 ) ) ;
#94760 = ORIENTED_EDGE ( 'NONE', *, *, #142429, .F. ) ;
#94762 = VECTOR ( 'NONE', #55897, 1000.000000000000000 ) ;
#94761 = CARTESIAN_POINT ( 'NONE',  ( 17.92867102513379862, 9.037728232668255757, 5.000000000000000000 ) ) ;
#94763 = EDGE_LOOP ( 'NONE', ( #142157, #94555, #137529, #98942 ) ) ;
#94764 = ORIENTED_EDGE ( 'NONE', *, *, #75095, .T. ) ;
#94766 = VECTOR ( 'NONE', #116455, 1000.000000000000000 ) ;
#94765 = CARTESIAN_POINT ( 'NONE',  ( 70.72959685856477563, -6.110000000000000320, -1.637169565754161393 ) ) ;
#94767 = ORIENTED_EDGE ( 'NONE', *, *, #136171, .F. ) ;
#94768 = CIRCLE ( 'NONE', #22933, 1.898649999999994842 ) ;
#94769 = EDGE_CURVE ( 'NONE', #41660, #51304, #76516, .T. ) ;
#94770 = CARTESIAN_POINT ( 'NONE',  ( -34.42500000000001137, -18.02281430457038880, 5.000000000000000000 ) ) ;
#94771 = EDGE_CURVE ( 'NONE', #21869, #119070, #86671, .T. ) ;
#94772 = CARTESIAN_POINT ( 'NONE',  ( 23.29387692260788967, 22.22500000000000142, 4.000000000000000000 ) ) ;
#94773 = CARTESIAN_POINT ( 'NONE',  ( 105.0004301918981184, -3.055000000000002380, 5.291415217122920289 ) ) ;
#94774 = DIRECTION ( 'NONE',  ( -0.000000000000000000, 0.3543493200069152138, -0.9351131265310292928 ) ) ;
#94775 = PLANE ( 'NONE',  #113837 ) ;
#94776 = CARTESIAN_POINT ( 'NONE',  ( 42.48921356237308800, -27.52281430457085065, 5.000000000000000000 ) ) ;
#94777 = PRESENTATION_LAYER_ASSIGNMENT (  '', '', ( #18400 ) ) ;
#94778 = ADVANCED_FACE ( 'NONE', ( #106966 ), #20667, .T. ) ;
#94779 = PLANE ( 'NONE',  #100256 ) ;
#94780 = CARTESIAN_POINT ( 'NONE',  ( 23.67183060077631396, 17.25929247661554555, 4.000000000000000000 ) ) ;
#94781 = EDGE_LOOP ( 'NONE', ( #117050, #4733, #105801, #74886, #132315 ) ) ;
#94782 = CARTESIAN_POINT ( 'NONE',  ( -51.18398860626899705, 28.73617430169823095, 5.000000000000000000 ) ) ;
#94783 = EDGE_LOOP ( 'NONE', ( #9116, #86281, #134170, #45778 ) ) ;
#94784 = ORIENTED_EDGE ( 'NONE', *, *, #96786, .T. ) ;
#94785 = VERTEX_POINT ( 'NONE', #130899 ) ;
#94786 = DIRECTION ( 'NONE',  ( -0.000000000000000000, 0.3543493200069153248, 0.9351131265310292928 ) ) ;
#94787 = CARTESIAN_POINT ( 'NONE',  ( 7.720000000000001528, 9.521314400968980422E-16, 0.000000000000000000 ) ) ;
#94788 = DIRECTION ( 'NONE',  ( 1.000000000000000000, 0.000000000000000000, 0.000000000000000000 ) ) ;
#94789 = DIRECTION ( 'NONE',  ( -1.000000000000000000, 0.000000000000000000, -0.000000000000000000 ) ) ;
#94790 =( REPRESENTATION_RELATIONSHIP ('NONE','NONE', #69070, #103311 ) REPRESENTATION_RELATIONSHIP_WITH_TRANSFORMATION ( #30032 )SHAPE_REPRESENTATION_RELATIONSHIP( ) );
#94791 = VERTEX_POINT ( 'NONE', #7645 ) ;
#94792 = CARTESIAN_POINT ( 'NONE',  ( 0.3818979091348736477, -51.95642703808907470, 39.54367611436850893 ) ) ;
#94793 = ORIENTED_EDGE ( 'NONE', *, *, #110002, .F. ) ;
#94794 = CARTESIAN_POINT ( 'NONE',  ( 3.187069808101886448, -2.126176841940956130, 7.934999999999991616 ) ) ;
#94795 = CARTESIAN_POINT ( 'NONE',  ( 34.92499999999998295, -15.18334561358938650, 4.500000000000000888 ) ) ;
#94796 = DIRECTION ( 'NONE',  ( -0.7071067811865486830, -0.7071067811865464625, 0.000000000000000000 ) ) ;
#94797 = CARTESIAN_POINT ( 'NONE',  ( 22.49999999999984723, -2.947814304570794075, 5.000000000000000000 ) ) ;
#94798 = ORIENTED_EDGE ( 'NONE', *, *, #133295, .F. ) ;
#94799 = ORIENTED_EDGE ( 'NONE', *, *, #137370, .T. ) ;
#94800 = VERTEX_POINT ( 'NONE', #139646 ) ;
#94801 = CARTESIAN_POINT ( 'NONE',  ( 26.99999999999981526, -19.22509904557633931, 1.855685503482240373 ) ) ;
#94802 = DIRECTION ( 'NONE',  ( -0.6830127018922181881, 0.6830127018922202975, -0.2588190451025214056 ) ) ;
#94803 = DIRECTION ( 'NONE',  ( -0.7071067811865487940, 0.7071067811865463515, -0.000000000000000000 ) ) ;
#94804 = DIRECTION ( 'NONE',  ( -0.6830127018922180770, -0.6830127018922204085, -0.2588190451025213501 ) ) ;
#94805 = DIRECTION ( 'NONE',  ( -0.7071067811865486830, 0.7071067811865464625, 0.000000000000000000 ) ) ;
#94806 = DIRECTION ( 'NONE',  ( 0.6830127018922181881, 0.6830127018922202975, -0.2588190451025214056 ) ) ;
#94807 = EDGE_CURVE ( 'NONE', #23195, #23765, #128729, .T. ) ;
#94808 = LINE ( 'NONE', #139073, #2231 ) ;
#94809 = FILL_AREA_STYLE ('',( #52060 ) ) ;
#94810 = ORIENTED_EDGE ( 'NONE', *, *, #76799, .F. ) ;
#94811 = DIRECTION ( 'NONE',  ( -0.5735764363510507113, 0.8191520442889885789, 1.003171929053520926E-16 ) ) ;
#94812 = VECTOR ( 'NONE', #74693, 1000.000000000000227 ) ;
#94813 = VECTOR ( 'NONE', #106951, 1000.000000000000000 ) ;
#94814 = CIRCLE ( 'NONE', #87912, 2.500000000000000444 ) ;
#94815 = CARTESIAN_POINT ( 'NONE',  ( -34.42500000000001137, 21.72500000000000142, 0.4999999999999995559 ) ) ;
#94816 = ORIENTED_EDGE ( 'NONE', *, *, #43473, .T. ) ;
#94818 = ADVANCED_FACE ( 'NONE', ( #85209 ), #9034, .F. ) ;
#94817 = AXIS2_PLACEMENT_3D ( 'NONE', #135808, #67731, #101744 ) ;
#94819 = DIRECTION ( 'NONE',  ( 0.7071067811865487940, 0.7071067811865463515, -0.000000000000000000 ) ) ;
#94821 = ORIENTED_EDGE ( 'NONE', *, *, #110122, .F. ) ;
#94820 = PLANE ( 'NONE',  #34953 ) ;
#94822 = EDGE_CURVE ( 'NONE', #139864, #141891, #52588, .T. ) ;
#94823 = CARTESIAN_POINT ( 'NONE',  ( 8.999999999999944933, 11.96639925780214675, 5.000000000000000000 ) ) ;
#94824 =( LENGTH_UNIT ( ) NAMED_UNIT ( * ) SI_UNIT ( .MILLI., .METRE. ) );
#94825 = ORIENTED_EDGE ( 'NONE', *, *, #43465, .F. ) ;
#94826 = LINE ( 'NONE', #4206, #9540 ) ;
#94827 = VECTOR ( 'NONE', #17975, 999.9999999999998863 ) ;
#94828 = VERTEX_POINT ( 'NONE', #109107 ) ;
#94829 = EDGE_CURVE ( 'NONE', #118847, #38733, #120686, .T. ) ;
#94830 = EDGE_CURVE ( 'NONE', #38833, #80915, #26919, .T. ) ;
#94831 = CARTESIAN_POINT ( 'NONE',  ( 34.92499999999998295, -20.99387692260782501, 4.000000000000000000 ) ) ;
#94832 = CARTESIAN_POINT ( 'NONE',  ( 123.0166937171295416, 7.950000000000001066, -2.130196079827421318 ) ) ;
#94833 = DIRECTION ( 'NONE',  ( 0.000000000000000000, -1.000000000000000000, 0.000000000000000000 ) ) ;
#94834 = AXIS2_PLACEMENT_3D ( 'NONE', #35130, #79373, #123576 ) ;
#94835 = LINE ( 'NONE', #7098, #69133 ) ;
#94836 = EDGE_CURVE ( 'NONE', #90375, #59049, #25477, .T. ) ;
#94837 = CARTESIAN_POINT ( 'NONE',  ( 19.19018167574436262, -18.74070752338409562, 7.910009926591462737 ) ) ;
#94838 = FACE_OUTER_BOUND ( 'NONE', #135600, .T. ) ;
#94839 = LINE ( 'NONE', #60123, #110800 ) ;
#94840 = CARTESIAN_POINT ( 'NONE',  ( 27.54123647476855652, 0.000000000000000000, 7.934999999999990727 ) ) ;
#94842 = VECTOR ( 'NONE', #16025, 1000.000000000000000 ) ;
#94841 = CARTESIAN_POINT ( 'NONE',  ( 12.22873647476855119, 5.808823158059031044, -5.808823158059037262 ) ) ;
#94843 = CARTESIAN_POINT ( 'NONE',  ( 0.000000000000000000, 0.5999999999999987566, -3.054668707061621191 ) ) ;
#94844 = CIRCLE ( 'NONE', #113377, 2.055000000000000604 ) ;
#94845 = DIRECTION ( 'NONE',  ( -0.7071067811865486830, 0.7071067811865464625, 0.000000000000000000 ) ) ;
#94846 = CARTESIAN_POINT ( 'NONE',  ( 6.792893218813414791, -5.240707523384228850, 5.000000000000000000 ) ) ;
#94847 = ORIENTED_EDGE ( 'NONE', *, *, #15070, .T. ) ;
#94848 =( BOUNDED_CURVE ( )  B_SPLINE_CURVE ( 3, ( #77377, #85339, #132479, #31003 ),
 .UNSPECIFIED., .F., .F. ) 
 B_SPLINE_CURVE_WITH_KNOTS ( ( 4, 4 ),
 ( 2.001653308786174090, 3.503810798801451742 ),
 .UNSPECIFIED. ) 
 CURVE ( )  GEOMETRIC_REPRESENTATION_ITEM ( )  RATIONAL_B_SPLINE_CURVE ( ( 1.000000000000000000, 0.8206354192515249446, 0.8206354192515249446, 1.000000000000000000 ) ) 
 REPRESENTATION_ITEM ( '' )  );
#94849 = VERTEX_POINT ( 'NONE', #67055 ) ;
#94851 = EDGE_CURVE ( 'NONE', #133319, #69181, #11188, .T. ) ;
#94850 = CARTESIAN_POINT ( 'NONE',  ( 81.20833333333332860, -3.974999999999999201, -6.884901960086287964 ) ) ;
#94852 = VECTOR ( 'NONE', #54803, 1000.000000000000000 ) ;
#94853 =( NAMED_UNIT ( * ) SI_UNIT ( $, .STERADIAN. ) SOLID_ANGLE_UNIT ( ) );
#94854 = VERTEX_POINT ( 'NONE', #11929 ) ;
#94855 = PLANE ( 'NONE',  #98944 ) ;
#94856 = PLANE ( 'NONE',  #23230 ) ;
#94857 = DIRECTION ( 'NONE',  ( 0.6830127018922180770, -0.6830127018922204085, -0.2588190451025213501 ) ) ;
#94858 = ORIENTED_EDGE ( 'NONE', *, *, #77584, .T. ) ;
#94859 = AXIS2_PLACEMENT_3D ( 'NONE', #52630, #22136, #9844 ) ;
#94860 = EDGE_CURVE ( 'NONE', #96026, #142433, #77244, .T. ) ;
#94861 = CARTESIAN_POINT ( 'NONE',  ( -34.92500000000001137, 22.22500000000000142, 4.000000000000000000 ) ) ;
#94862 = DIRECTION ( 'NONE',  ( 0.7071067811865487940, 0.7071067811865463515, -0.000000000000000000 ) ) ;
#94863 = VECTOR ( 'NONE', #59420, 1000.000000000000000 ) ;
#94864 = DIRECTION ( 'NONE',  ( -1.000000000000000000, -1.224606353822377258E-16, -0.000000000000000000 ) ) ;
#94865 = DIRECTION ( 'NONE',  ( 2.781805975412905274E-17, -0.3543493200069152138, 0.9351131265310292928 ) ) ;
#94866 = AXIS2_PLACEMENT_3D ( 'NONE', #5789, #4319, #92825 ) ;
#94867 = CARTESIAN_POINT ( 'NONE',  ( 21.18398860626899349, 28.73617430169802134, 5.000000000000000000 ) ) ;
#94868 = CARTESIAN_POINT ( 'NONE',  ( -24.25645252394784990, 6.095695649681008632, 4.664440252871067116 ) ) ;
#94869 = CARTESIAN_POINT ( 'NONE',  ( 15.48921356237309510, -27.52281430457066236, 5.000000000000000000 ) ) ;
#94870 = EDGE_CURVE ( 'NONE', #31365, #71785, #88991, .T. ) ;
#94871 = DIRECTION ( 'NONE',  ( 0.7071067811865486830, -0.7071067811865464625, -0.000000000000000000 ) ) ;
#94872 = DIRECTION ( 'NONE',  ( -0.6830127018922180770, -0.6830127018922204085, -0.2588190451025213501 ) ) ;
#94873 = DIRECTION ( 'NONE',  ( 1.000000000000000000, 1.224606353822377258E-16, 0.000000000000000000 ) ) ;
#94874 = CARTESIAN_POINT ( 'NONE',  ( -33.70710678118631165, -3.740707523384248390, 5.000000000000000000 ) ) ;
#94875 = CARTESIAN_POINT ( 'NONE',  ( 59.37656097284888546, -44.54322672567602837, 35.04755940937982217 ) ) ;
#94876 = ORIENTED_EDGE ( 'NONE', *, *, #32331, .T. ) ;
#94877 = ORIENTED_EDGE ( 'NONE', *, *, #88567, .T. ) ;
#94878 = CARTESIAN_POINT ( 'NONE',  ( 100.6254301918981042, 5.291415217122919401, 3.055000000000002824 ) ) ;
#94879 = EDGE_LOOP ( 'NONE', ( #82017, #131706, #48907, #39162 ) ) ;
#94880 = EDGE_CURVE ( 'NONE', #86612, #121778, #89507, .T. ) ;
#94881 = FACE_OUTER_BOUND ( 'NONE', #37824, .T. ) ;
#94882 = AXIS2_PLACEMENT_3D ( 'NONE', #63526, #27439, #96781 ) ;
#94883 = DIRECTION ( 'NONE',  ( -0.7071067811865486830, -0.7071067811865464625, -0.000000000000000000 ) ) ;
#94884 = ORIENTED_EDGE ( 'NONE', *, *, #139592, .T. ) ;
#94885 = FACE_OUTER_BOUND ( 'NONE', #117604, .T. ) ;
#94886 = CARTESIAN_POINT ( 'NONE',  ( 0.000000000000000000, 0.000000000000000000, 5.000000000000000000 ) ) ;
#94887 = ADVANCED_FACE ( 'NONE', ( #103064 ), #71168, .F. ) ;
#94888 = CARTESIAN_POINT ( 'NONE',  ( 98.34959685856479439, 6.109999999999996767, 1.637169565754163836 ) ) ;
#94889 = ORIENTED_EDGE ( 'NONE', *, *, #18942, .T. ) ;
#94890 = EDGE_CURVE ( 'NONE', #17479, #91909, #92889, .T. ) ;
#94891 = LINE ( 'NONE', #52124, #4890 ) ;
#94892 = ORIENTED_EDGE ( 'NONE', *, *, #21743, .T. ) ;
#94893 = LINE ( 'NONE', #72962, #54608 ) ;
#94894 = DIRECTION ( 'NONE',  ( -0.7071067811865487940, 0.7071067811865463515, -0.000000000000000000 ) ) ;
#94895 = VECTOR ( 'NONE', #114059, 1000.000000000000000 ) ;
#94896 = CARTESIAN_POINT ( 'NONE',  ( 11.93159235450332112, 3.061616997868380183E-16, -2.500000000000001332 ) ) ;
#94897 = DIRECTION ( 'NONE',  ( 0.000000000000000000, 0.000000000000000000, 1.000000000000000000 ) ) ;
#94898 = EDGE_CURVE ( 'NONE', #71183, #9868, #9045, .T. ) ;
#94899 = VERTEX_POINT ( 'NONE', #113929 ) ;
#94900 = ORIENTED_EDGE ( 'NONE', *, *, #5322, .T. ) ;
#94901 = VERTEX_POINT ( 'NONE', #44626 ) ;
#94902 = FACE_OUTER_BOUND ( 'NONE', #68643, .T. ) ;
#94903 = DIRECTION ( 'NONE',  ( -0.7071067811865486830, -0.7071067811865464625, 0.000000000000000000 ) ) ;
#94904 = CARTESIAN_POINT ( 'NONE',  ( 6.483736474768551972, -5.808823158059035485, -5.808823158059033709 ) ) ;
#94905 = VECTOR ( 'NONE', #57805, 1000.000000000000227 ) ;
#94906 = VECTOR ( 'NONE', #5822, 999.9999999999998863 ) ;
#94907 = CARTESIAN_POINT ( 'NONE',  ( 10.82816939922345156, -8.240707523384200428, 4.000000000000000000 ) ) ;
#94908 = SURFACE_STYLE_FILL_AREA ( #107911 ) ;
#94909 = ORIENTED_EDGE ( 'NONE', *, *, #117550, .T. ) ;
#94910 = ORIENTED_EDGE ( 'NONE', *, *, #55465, .F. ) ;
#94911 = EDGE_CURVE ( 'NONE', #118679, #111906, #43876, .T. ) ;
#94912 = PLANE ( 'NONE',  #89692 ) ;
#94913 = VERTEX_POINT ( 'NONE', #22093 ) ;
#94914 = ORIENTED_EDGE ( 'NONE', *, *, #108705, .T. ) ;
#94915 = EDGE_CURVE ( 'NONE', #22337, #12371, #36382, .T. ) ;
#94916 = CARTESIAN_POINT ( 'NONE',  ( 110.0162635252314374, -4.472830434245838482, 4.472830434245838482 ) ) ;
#94917 = AXIS2_PLACEMENT_3D ( 'NONE', #40462, #116570, #94788 ) ;
#94918 = LINE ( 'NONE', #104372, #67698 ) ;
#94919 = CARTESIAN_POINT ( 'NONE',  ( 27.99999999999999645, 2.055000000000001492, 2.516649172247811554E-16 ) ) ;
#94920 = VERTEX_POINT ( 'NONE', #133047 ) ;
#94921 = CARTESIAN_POINT ( 'NONE',  ( 5.999999999999960032, -3.485240976185074224, -4.108735105802382215 ) ) ;
#94922 = VECTOR ( 'NONE', #24142, 999.9999999999998863 ) ;
#94923 = DIRECTION ( 'NONE',  ( 0.7071067811865487940, 0.7071067811865463515, 0.000000000000000000 ) ) ;
#94924 = VECTOR ( 'NONE', #81112, 1000.000000000000000 ) ;
#94925 = CIRCLE ( 'NONE', #104232, 5.968999999999998529 ) ;
#94926 = VECTOR ( 'NONE', #90570, 1000.000000000000000 ) ;
#94927 = CARTESIAN_POINT ( 'NONE',  ( 5.281315875828549444, 4.584330080086930965E-16, 0.000000000000000000 ) ) ;
#94928 = ORIENTED_EDGE ( 'NONE', *, *, #100153, .F. ) ;
#94929 = DIRECTION ( 'NONE',  ( 0.3543493200069164351, 2.781805975412904658E-17, -0.9351131265310288487 ) ) ;
#94930 = FACE_BOUND ( 'NONE', #119627, .T. ) ;
#94931 = ORIENTED_EDGE ( 'NONE', *, *, #43077, .F. ) ;
#94932 = CARTESIAN_POINT ( 'NONE',  ( 21.18398860626899349, 28.73617430169802134, 5.000000000000000000 ) ) ;
#94933 = DIRECTION ( 'NONE',  ( 0.7071067811865487940, -0.7071067811865463515, 0.000000000000000000 ) ) ;
#94934 = CARTESIAN_POINT ( 'NONE',  ( 0.1839886062690032631, 28.73617430169787568, 5.000000000000000000 ) ) ;
#94935 = ORIENTED_EDGE ( 'NONE', *, *, #78186, .F. ) ;
#94936 = DIRECTION ( 'NONE',  ( 0.7071067811865486830, -0.7071067811865464625, -0.000000000000000000 ) ) ;
#94937 = VERTEX_POINT ( 'NONE', #55469 ) ;
#94938 = VERTEX_POINT ( 'NONE', #99654 ) ;
#94939 = VERTEX_POINT ( 'NONE', #115312 ) ;
#94940 = EDGE_CURVE ( 'NONE', #61882, #89049, #47992, .T. ) ;
#94941 = CARTESIAN_POINT ( 'NONE',  ( 26.74543019189810877, -5.291415217122918513, -3.055000000000000160 ) ) ;
#94942 = DIRECTION ( 'NONE',  ( 0.7071067811865486830, -0.7071067811865464625, -0.000000000000000000 ) ) ;
#94943 = PLANE ( 'NONE',  #109682 ) ;
#94944 = FACE_OUTER_BOUND ( 'NONE', #55225, .T. ) ;
#94945 = CARTESIAN_POINT ( 'NONE',  ( 11.29289321881338459, 5.259292476615667233, 5.000000000000000000 ) ) ;
#94946 = FACE_OUTER_BOUND ( 'NONE', #12551, .T. ) ;
#94947 = CARTESIAN_POINT ( 'NONE',  ( 4.184256412735922304, -2.055000000000000160, 2.789133085058097101E-16 ) ) ;
#94948 = VECTOR ( 'NONE', #136237, 1000.000000000000000 ) ;
#94949 = DIRECTION ( 'NONE',  ( -0.3543493200069162685, -0.000000000000000000, -0.9351131265310288487 ) ) ;
#94950 = VECTOR ( 'NONE', #68542, 1000.000000000000000 ) ;
#94951 = EDGE_CURVE ( 'NONE', #12119, #11674, #111239, .T. ) ;
#94952 = LINE ( 'NONE', #117409, #138574 ) ;
#94953 = FACE_OUTER_BOUND ( 'NONE', #33979, .T. ) ;
#94954 = CARTESIAN_POINT ( 'NONE',  ( 17.99999999999987566, -15.41253812416059787, 4.000000000000000000 ) ) ;
#94955 = ORIENTED_EDGE ( 'NONE', *, *, #65492, .F. ) ;
#94956 = VECTOR ( 'NONE', #127887, 1000.000000000000000 ) ;
#94957 = EDGE_LOOP ( 'NONE', ( #112995, #6859, #73870, #26111 ) ) ;
#94958 = VERTEX_POINT ( 'NONE', #92162 ) ;
#94959 = VERTEX_POINT ( 'NONE', #100400 ) ;
#94960 = CARTESIAN_POINT ( 'NONE',  ( -23.99999999999983302, -7.068876922607743474, 4.000000000000000000 ) ) ;
#94961 = ORIENTED_EDGE ( 'NONE', *, *, #138854, .T. ) ;
#94962 = VECTOR ( 'NONE', #17116, 1000.000000000000000 ) ;
#94963 = VERTEX_POINT ( 'NONE', #14621 ) ;
#94964 = FACE_OUTER_BOUND ( 'NONE', #142749, .T. ) ;
#94965 = ADVANCED_FACE ( 'NONE', ( #136391 ), #37081, .F. ) ;
#94966 = DIRECTION ( 'NONE',  ( 0.000000000000000000, 0.000000000000000000, -1.000000000000000000 ) ) ;
#94967 = ORIENTED_EDGE ( 'NONE', *, *, #100826, .T. ) ;
#94968 = PLANE ( 'NONE',  #32529 ) ;
#94969 = EDGE_LOOP ( 'NONE', ( #122055, #119829, #3465, #109811 ) ) ;
#94970 = DIRECTION ( 'NONE',  ( 0.7071067811865486830, -0.7071067811865464625, -0.000000000000000000 ) ) ;
#94971 = CARTESIAN_POINT ( 'NONE',  ( 34.75611968250419181, 8.812934254707293746, 4.955485411084883829 ) ) ;
#94972 = CARTESIAN_POINT ( 'NONE',  ( 11.73373647476855197, 5.808823158059036373, 5.808823158059032821 ) ) ;
#94973 = ORIENTED_EDGE ( 'NONE', *, *, #55889, .T. ) ;
#94974 = CARTESIAN_POINT ( 'NONE',  ( 99.66209685856478018, -5.291415217122919401, 3.054999999999998384 ) ) ;
#94975 = CARTESIAN_POINT ( 'NONE',  ( 16.11017322888198677, -22.22500000000000497, 4.785647885939352086 ) ) ;
#94976 = DIRECTION ( 'NONE',  ( 3.469446951953611033E-15, -1.000000000000000000, -6.938893903907222067E-15 ) ) ;
#94977 = VERTEX_POINT ( 'NONE', #59580 ) ;
#94978 = VERTEX_POINT ( 'NONE', #103741 ) ;
#94979 = DIRECTION ( 'NONE',  ( 1.000000000000000000, 1.224606353822377258E-16, 0.000000000000000000 ) ) ;
#94980 = AXIS2_PLACEMENT_3D ( 'NONE', #26244, #112527, #49453 ) ;
#94981 = VERTEX_POINT ( 'NONE', #4384 ) ;
#94982 = DIRECTION ( 'NONE',  ( -0.7071067811865487940, 0.7071067811865463515, 0.000000000000000000 ) ) ;
#94983 = PLANE ( 'NONE',  #104320 ) ;
#94984 = PLANE ( 'NONE',  #33102 ) ;
#94985 = CARTESIAN_POINT ( 'NONE',  ( 180.8518557880187245, -48.98056306480257405, -39.49745726092499609 ) ) ;
#94986 = ORIENTED_EDGE ( 'NONE', *, *, #86127, .T. ) ;
#94987 = CARTESIAN_POINT ( 'NONE',  ( -5.999999999999960920, 19.55218569542897100, 5.000000000000000000 ) ) ;
#94988 = DIRECTION ( 'NONE',  ( -0.6830127018922181881, 0.6830127018922202975, -0.2588190451025214056 ) ) ;
#94989 = LINE ( 'NONE', #139265, #67406 ) ;
#94990 = EDGE_CURVE ( 'NONE', #2478, #22757, #48684, .T. ) ;
#94991 = VERTEX_POINT ( 'NONE', #93617 ) ;
#94992 = CARTESIAN_POINT ( 'NONE',  ( -12.69999999999998153, 0.000000000000000000, 2.500000000000000444 ) ) ;
#94993 = AXIS2_PLACEMENT_3D ( 'NONE', #81287, #2973, #93570 ) ;
#94994 = CARTESIAN_POINT ( 'NONE',  ( 15.48921356237309510, -27.52281430457066236, 5.000000000000000000 ) ) ;
#94995 = VERTEX_POINT ( 'NONE', #39243 ) ;
#94997 = ORIENTED_EDGE ( 'NONE', *, *, #12871, .F. ) ;
#94996 = LINE ( 'NONE', #5837, #115709 ) ;
#94998 = EDGE_CURVE ( 'NONE', #54275, #88406, #126929, .T. ) ;
#94999 = EDGE_CURVE ( 'NONE', #53690, #129512, #11444, .T. ) ;
#95000 = ORIENTED_EDGE ( 'NONE', *, *, #40757, .T. ) ;
#95001 = CARTESIAN_POINT ( 'NONE',  ( 34.75611968250419181, -12.18706574529247710, 4.955485411084880276 ) ) ;
#95002 = LINE ( 'NONE', #82051, #85435 ) ;
#95004 = ORIENTED_EDGE ( 'NONE', *, *, #22815, .F. ) ;
#95003 = AXIS2_PLACEMENT_3D ( 'NONE', #128055, #37467, #93964 ) ;
#95005 = DIRECTION ( 'NONE',  ( -1.000000000000000000, -1.224606353822377258E-16, -0.000000000000000000 ) ) ;
#95006 = EDGE_CURVE ( 'NONE', #57200, #25994, #50117, .T. ) ;
#95007 = EDGE_CURVE ( 'NONE', #139559, #116329, #127681, .T. ) ;
#95008 = LINE ( 'NONE', #71884, #116895 ) ;
#95009 = EDGE_CURVE ( 'NONE', #56334, #22212, #95745, .T. ) ;
#95010 =( BOUNDED_CURVE ( )  B_SPLINE_CURVE ( 3, ( #75712, #73569, #30037, #95301 ),
 .UNSPECIFIED., .F., .T. ) 
 B_SPLINE_CURVE_WITH_KNOTS ( ( 4, 4 ),
 ( 1.964434688349487423, 3.503810798801450854 ),
 .UNSPECIFIED. ) 
 CURVE ( )  GEOMETRIC_REPRESENTATION_ITEM ( )  RATIONAL_B_SPLINE_CURVE ( ( 1.000000000000000000, 0.8120851936182280628, 0.8120851936182280628, 1.000000000000000000 ) ) 
 REPRESENTATION_ITEM ( '' )  );
#95011 = PLANE ( 'NONE',  #18377 ) ;
#95012 = FACE_OUTER_BOUND ( 'NONE', #45321, .T. ) ;
#95013 = EDGE_CURVE ( 'NONE', #106292, #10266, #49427, .T. ) ;
#95014 = DIRECTION ( 'NONE',  ( 1.000000000000000000, 0.000000000000000000, 0.000000000000000000 ) ) ;
#95015 = CARTESIAN_POINT ( 'NONE',  ( -7.809818324255463295, -18.74070752338408852, 7.910009926591528462 ) ) ;
#95016 = DIRECTION ( 'NONE',  ( -0.7071067811865486830, -0.7071067811865464625, -0.000000000000000000 ) ) ;
#95017 = CARTESIAN_POINT ( 'NONE',  ( -9.299744871391588674, -27.71228299555212971, 4.000000000000000000 ) ) ;
#95018 = CARTESIAN_POINT ( 'NONE',  ( 25.89892480454907542, 0.000000000000000000, -6.350000000000003197 ) ) ;
#95019 = ADVANCED_FACE ( 'NONE', ( #140666 ), #83199, .T. ) ;
#95020 = VECTOR ( 'NONE', #39246, 999.9999999999998863 ) ;
#95021 = LINE ( 'NONE', #85578, #28040 ) ;
#95022 = EDGE_LOOP ( 'NONE', ( #73837, #135642, #90614, #29369 ) ) ;
#95023 = ORIENTED_EDGE ( 'NONE', *, *, #95893, .F. ) ;
#95024 = VERTEX_POINT ( 'NONE', #16757 ) ;
#95025 =( GEOMETRIC_REPRESENTATION_CONTEXT ( 3 ) GLOBAL_UNCERTAINTY_ASSIGNED_CONTEXT ( ( #70800 ) ) GLOBAL_UNIT_ASSIGNED_CONTEXT ( ( #102105, #56497, #100674 ) ) REPRESENTATION_CONTEXT ( 'NONE', 'WORKASPACE' ) );
#95027 = EDGE_CURVE ( 'NONE', #116824, #34379, #29992, .T. ) ;
#95026 = CARTESIAN_POINT ( 'NONE',  ( 108.0416666666666714, -3.975000000000002753, 6.884901960086286188 ) ) ;
#95028 = VECTOR ( 'NONE', #139538, 1000.000000000000000 ) ;
#95029 = EDGE_LOOP ( 'NONE', ( #135280, #58310, #132096, #26934 ) ) ;
#95030 = VERTEX_POINT ( 'NONE', #85568 ) ;
#95031 = ORIENTED_EDGE ( 'NONE', *, *, #120959, .F. ) ;
#95032 = LINE ( 'NONE', #136406, #43300 ) ;
#95033 = CARTESIAN_POINT ( 'NONE',  ( 45.29974487139158867, -27.71228299555237840, 4.000000000000000000 ) ) ;
#95034 = VECTOR ( 'NONE', #137629, 1000.000000000000000 ) ;
#95035 = VECTOR ( 'NONE', #17811, 1000.000000000000000 ) ;
#95036 = AXIS2_PLACEMENT_3D ( 'NONE', #18673, #52740, #129586 ) ;
#95037 = CIRCLE ( 'NONE', #74269, 1.000000000000000888 ) ;
#95038 = EDGE_LOOP ( 'NONE', ( #63342, #108174, #92266, #72929 ) ) ;
#95039 = LINE ( 'NONE', #104496, #136475 ) ;
#95040 = VECTOR ( 'NONE', #74323, 999.9999999999998863 ) ;
#95041 = ADVANCED_FACE ( 'NONE', ( #29758 ), #72623, .F. ) ;
#95042 = SURFACE_STYLE_USAGE ( .BOTH. , #28388 ) ;
#95043 = DIRECTION ( 'NONE',  ( 0.000000000000000000, -1.000000000000000000, 0.000000000000000000 ) ) ;
#95044 = DIRECTION ( 'NONE',  ( 0.7071067811865487940, 0.7071067811865463515, 0.000000000000000000 ) ) ;
#95045 = CARTESIAN_POINT ( 'NONE',  ( 100.4795968585647614, 6.109999999999999432, 1.637169565754164280 ) ) ;
#95046 = ORIENTED_EDGE ( 'NONE', *, *, #110496, .T. ) ;
#95047 = DIRECTION ( 'NONE',  ( -1.000000000000000000, -1.224606353822377258E-16, -0.000000000000000000 ) ) ;
#95048 = DIRECTION ( 'NONE',  ( 1.000000000000000000, 0.000000000000000000, 0.000000000000000000 ) ) ;
#95049 = CARTESIAN_POINT ( 'NONE',  ( -34.92500000000001137, 22.22500000000000142, 4.500000000000000888 ) ) ;
#95050 = VECTOR ( 'NONE', #94159, 1000.000000000000000 ) ;
#95051 = CARTESIAN_POINT ( 'NONE',  ( 7.499999999999954703, 16.08746187583908593, 4.000000000000000000 ) ) ;
#95052 = CARTESIAN_POINT ( 'NONE',  ( 16.61159235450331906, 9.902892378096218942E-16, 0.000000000000000000 ) ) ;
#95053 = ADVANCED_FACE ( 'NONE', ( #117472 ), #82745, .T. ) ;
#95054 = CARTESIAN_POINT ( 'NONE',  ( 45.18398860626900415, 28.73617430169818832, 5.000000000000000000 ) ) ;
#95055 = DIRECTION ( 'NONE',  ( 0.6830127018922180770, -0.6830127018922204085, -0.2588190451025213501 ) ) ;
#95056 = CARTESIAN_POINT ( 'NONE',  ( 36.68336038379623432, -2.130196079827426203, 7.949999999999997513 ) ) ;
#95057 = DIRECTION ( 'NONE',  ( 0.000000000000000000, -1.000000000000000000, 0.000000000000000000 ) ) ;
#95058 = CARTESIAN_POINT ( 'NONE',  ( 32.99999999999977263, -0.2811185226894025169, -5.995736974527589247 ) ) ;
#95059 = ORIENTED_EDGE ( 'NONE', *, *, #90630, .F. ) ;
#95060 = ORIENTED_EDGE ( 'NONE', *, *, #95853, .T. ) ;
#95061 = CARTESIAN_POINT ( 'NONE',  ( 25.06249999999998934, -5.819803920172572198, -5.819803920172573086 ) ) ;
#95062 = VERTEX_POINT ( 'NONE', #41353 ) ;
#95063 = LINE ( 'NONE', #84239, #27501 ) ;
#95064 = AXIS2_PLACEMENT_3D ( 'NONE', #80260, #67977, #99840 ) ;
#95065 = DIRECTION ( 'NONE',  ( 0.000000000000000000, -1.000000000000000000, 0.000000000000000000 ) ) ;
#95066 = CARTESIAN_POINT ( 'NONE',  ( -36.18398860626899705, 28.73617430169812437, 5.000000000000000000 ) ) ;
#95067 = CARTESIAN_POINT ( 'NONE',  ( 9.370933818357753964, 2.500000000000000444, 3.061616997868383634E-16 ) ) ;
#95068 = CARTESIAN_POINT ( 'NONE',  ( 57.48921356237308800, -27.52281430457095368, 5.000000000000000000 ) ) ;
#95069 = VECTOR ( 'NONE', #119664, 1000.000000000000227 ) ;
#95070 = EDGE_CURVE ( 'NONE', #88325, #121941, #105190, .T. ) ;
#95071 = VECTOR ( 'NONE', #127788, 1000.000000000000000 ) ;
#95072 = CARTESIAN_POINT ( 'NONE',  ( 25.52126352523142927, -4.472830434245839371, -4.472830434245840259 ) ) ;
#95073 = ORIENTED_EDGE ( 'NONE', *, *, #100281, .T. ) ;
#95074 = ADVANCED_FACE ( 'NONE', ( #5852 ), #63156, .F. ) ;
#95075 = CIRCLE ( 'NONE', #32596, 2.500000000000000888 ) ;
#95076 = DIRECTION ( 'NONE',  ( -0.7071067811865487940, 0.7071067811865463515, 0.000000000000000000 ) ) ;
#95077 = ORIENTED_EDGE ( 'NONE', *, *, #63811, .T. ) ;
#95078 = CARTESIAN_POINT ( 'NONE',  ( 18.48921356237309510, -27.52281430457068367, 5.000000000000000000 ) ) ;
#95079 = AXIS2_PLACEMENT_3D ( 'NONE', #323, #100399, #79400 ) ;
#95080 = FILL_AREA_STYLE_COLOUR ( '', #17556 ) ;
#95082 = ADVANCED_FACE ( 'NONE', ( #83458 ), #94314, .F. ) ;
#95081 = DIRECTION ( 'NONE',  ( -0.7071067811865486830, 0.7071067811865464625, 0.000000000000000000 ) ) ;
#95083 = CARTESIAN_POINT ( 'NONE',  ( 40.04515773336642326, -21.74070752338406365, 21.72585301388593848 ) ) ;
#95084 = ORIENTED_EDGE ( 'NONE', *, *, #132060, .F. ) ;
#95085 = CARTESIAN_POINT ( 'NONE',  ( 42.14626352523143282, -4.472830434245840259, 4.472830434245839371 ) ) ;
#95086 = ORIENTED_EDGE ( 'NONE', *, *, #104739, .F. ) ;
#95087 = FACE_OUTER_BOUND ( 'NONE', #67184, .T. ) ;
#95088 = DIRECTION ( 'NONE',  ( 0.000000000000000000, -1.000000000000000000, 0.000000000000000000 ) ) ;
#95089 = CARTESIAN_POINT ( 'NONE',  ( 12.51280225271498736, 3.821174125832445049E-16, 0.000000000000000000 ) ) ;
#95090 = DIRECTION ( 'NONE',  ( 0.000000000000000000, -1.000000000000000000, 0.000000000000000000 ) ) ;
#95091 =( BOUNDED_CURVE ( )  B_SPLINE_CURVE ( 3, ( #75651, #10360, #121976, #111090 ),
 .UNSPECIFIED., .F., .T. ) 
 B_SPLINE_CURVE_WITH_KNOTS ( ( 4, 4 ),
 ( 5.043186909253407180, 5.074607125596344304 ),
 .UNSPECIFIED. ) 
 CURVE ( )  GEOMETRIC_REPRESENTATION_ITEM ( )  RATIONAL_B_SPLINE_CURVE ( ( 1.000000000000000000, 0.9999177325257868620, 0.9999177325257868620, 1.000000000000000000 ) ) 
 REPRESENTATION_ITEM ( '' )  );
#95092 = VECTOR ( 'NONE', #30120, 1000.000000000000000 ) ;
#95093 = CARTESIAN_POINT ( 'NONE',  ( 48.47459685856478728, 1.637169565754164058, -6.109999999999996767 ) ) ;
#95094 = ORIENTED_EDGE ( 'NONE', *, *, #54570, .T. ) ;
#95095 = DIRECTION ( 'NONE',  ( 1.000000000000000000, 0.000000000000000000, 0.000000000000000000 ) ) ;
#95096 = ADVANCED_FACE ( 'NONE', ( #116782 ), #95011, .F. ) ;
#95097 = LINE ( 'NONE', #73384, #80317 ) ;
#95098 = ORIENTED_EDGE ( 'NONE', *, *, #57252, .F. ) ;
#95099 = VERTEX_POINT ( 'NONE', #52242 ) ;
#95100 = AXIS2_PLACEMENT_3D ( 'NONE', #35559, #71023, #3564 ) ;
#95101 = DIRECTION ( 'NONE',  ( 0.7071067811865487940, 0.7071067811865463515, 0.000000000000000000 ) ) ;
#95102 = ORIENTED_EDGE ( 'NONE', *, *, #104059, .T. ) ;
#95103 = CARTESIAN_POINT ( 'NONE',  ( 45.48921356237309510, -27.52281430457087197, 5.000000000000000000 ) ) ;
#95104 = EDGE_CURVE ( 'NONE', #10011, #121745, #29069, .T. ) ;
#95105 = EDGE_LOOP ( 'NONE', ( #35481, #111673, #77582, #107821 ) ) ;
#95106 = CARTESIAN_POINT ( 'NONE',  ( 44.99586038379622721, -3.974999999999998312, -6.884901960086286188 ) ) ;
#95107 = STYLED_ITEM ( 'NONE', ( #73100 ), #27925 ) ;
#95108 = PLANE ( 'NONE',  #23347 ) ;
#95109 = ADVANCED_FACE ( 'NONE', ( #11558 ), #142825, .F. ) ;
#95110 = FACE_BOUND ( 'NONE', #116372, .T. ) ;
#95111 = DIRECTION ( 'NONE',  ( 0.7071067811865486830, -0.7071067811865464625, -0.000000000000000000 ) ) ;
#95112 = CARTESIAN_POINT ( 'NONE',  ( 31.92500000000001492, 2.730000000000007088, -36.39086428169088094 ) ) ;
#95113 = DIRECTION ( 'NONE',  ( 0.7071067811865486830, -0.7071067811865464625, -0.000000000000000000 ) ) ;
#95114 = ORIENTED_EDGE ( 'NONE', *, *, #63495, .F. ) ;
#95115 =( LENGTH_UNIT ( ) NAMED_UNIT ( * ) SI_UNIT ( .MILLI., .METRE. ) );
#95117 = ORIENTED_EDGE ( 'NONE', *, *, #142380, .T. ) ;
#95116 = LINE ( 'NONE', #105973, #50478 ) ;
#95118 = VERTEX_POINT ( 'NONE', #66699 ) ;
#95119 = VECTOR ( 'NONE', #68356, 1000.000000000000000 ) ;
#95120 = CARTESIAN_POINT ( 'NONE',  ( 39.29974487139159578, -27.71228299555233576, 4.000000000000000000 ) ) ;
#95121 = ORIENTED_EDGE ( 'NONE', *, *, #109265, .F. ) ;
#95122 = ADVANCED_FACE ( 'NONE', ( #89166 ), #131233, .T. ) ;
#95123 = CARTESIAN_POINT ( 'NONE',  ( 52.70376352523144448, 6.109999999999998543, 1.122388791418548911E-15 ) ) ;
#95124 = ORIENTED_EDGE ( 'NONE', *, *, #64442, .F. ) ;
#95125 = CARTESIAN_POINT ( 'NONE',  ( -1.171830600776458509, -11.24070752338416490, 4.000000000000000000 ) ) ;
#95126 = EDGE_LOOP ( 'NONE', ( #6672, #33075, #5399, #138620 ) ) ;
#95127 = PLANE ( 'NONE',  #14378 ) ;
#95128 = VECTOR ( 'NONE', #11524, 1000.000000000000000 ) ;
#95129 = ADVANCED_FACE ( 'NONE', ( #77593 ), #9408, .F. ) ;
#95130 = VECTOR ( 'NONE', #22197, 1000.000000000000227 ) ;
#95131 = VECTOR ( 'NONE', #111510, 999.9999999999998863 ) ;
#95132 = ADVANCED_FACE ( 'NONE', ( #88462 ), #22439, .F. ) ;
#95133 = DIRECTION ( 'NONE',  ( -0.000000000000000000, 0.3543493200069153248, 0.9351131265310292928 ) ) ;
#95134 = CARTESIAN_POINT ( 'NONE',  ( 101.6250000000000000, -7.950000000000000178, -4.867971026610729436E-16 ) ) ;
#95135 = LINE ( 'NONE', #72007, #124567 ) ;
#95136 = CARTESIAN_POINT ( 'NONE',  ( 17.06250000000000000, 4.461849672132300881, 4.461849672132299105 ) ) ;
#95137 = FILL_AREA_STYLE_COLOUR ( '', #122677 ) ;
#95138 = ORIENTED_EDGE ( 'NONE', *, *, #35355, .T. ) ;
#95139 = VECTOR ( 'NONE', #4535, 1000.000000000000000 ) ;
#95140 = VECTOR ( 'NONE', #66359, 1000.000000000000000 ) ;
#95141 = VECTOR ( 'NONE', #82739, 1000.000000000000114 ) ;
#95142 = ORIENTED_EDGE ( 'NONE', *, *, #87454, .T. ) ;
#95143 = AXIS2_PLACEMENT_3D ( 'NONE', #63028, #50697, #105754 ) ;
#95144 = CARTESIAN_POINT ( 'NONE',  ( 20.17080628287043709, -3.047499999999997211, -5.278424836066143655 ) ) ;
#95145 = DIRECTION ( 'NONE',  ( -0.6830127018922180770, -0.6830127018922204085, -0.2588190451025213501 ) ) ;
#95146 = VERTEX_POINT ( 'NONE', #78293 ) ;
#95147 = VECTOR ( 'NONE', #132833, 1000.000000000000000 ) ;
#95148 = ORIENTED_EDGE ( 'NONE', *, *, #98869, .T. ) ;
#95149 = ORIENTED_EDGE ( 'NONE', *, *, #30596, .F. ) ;
#95150 = LINE ( 'NONE', #93736, #97556 ) ;
#95151 = ADVANCED_FACE ( 'NONE', ( #44993 ), #31221, .T. ) ;
#95152 = DIRECTION ( 'NONE',  ( -1.000000000000000000, -3.109656758745491620E-14, 0.000000000000000000 ) ) ;
#95153 = EDGE_LOOP ( 'NONE', ( #82473, #34643, #91713, #134392 ) ) ;
#95154 = AXIS2_PLACEMENT_3D ( 'NONE', #16413, #4074, #48359 ) ;
#95155 = LINE ( 'NONE', #75566, #143553 ) ;
#95156 = CARTESIAN_POINT ( 'NONE',  ( 13.33790314143522160, -6.871911579029513106, -3.967499999999993587 ) ) ;
#95157 = CARTESIAN_POINT ( 'NONE',  ( 11.99999999999992362, 13.55218569542903140, 5.000000000000000000 ) ) ;
#95158 = ORIENTED_EDGE ( 'NONE', *, *, #51564, .F. ) ;
#95159 = CARTESIAN_POINT ( 'NONE',  ( 128.2454301918981230, -5.291415217122919401, -3.055000000000000604 ) ) ;
#95160 = VECTOR ( 'NONE', #50729, 1000.000000000000000 ) ;
#95161 = CARTESIAN_POINT ( 'NONE',  ( 3.995075227788035477, -5.240707523384225297, 12.38332538355495238 ) ) ;
#95162 = DIRECTION ( 'NONE',  ( 0.7071067811865486830, -0.7071067811865464625, -0.000000000000000000 ) ) ;
#95164 = VERTEX_POINT ( 'NONE', #55114 ) ;
#95163 = DIRECTION ( 'NONE',  ( -0.7071067811865486830, -0.7071067811865464625, -0.000000000000000000 ) ) ;
#95165 = CARTESIAN_POINT ( 'NONE',  ( -27.15612307739222331, -22.22500000000000142, 4.000000000000000000 ) ) ;
#95166 = ORIENTED_EDGE ( 'NONE', *, *, #6103, .F. ) ;
#95167 = CARTESIAN_POINT ( 'NONE',  ( -18.18398860626898994, 28.73617430169800002, 5.000000000000000000 ) ) ;
#95168 = CARTESIAN_POINT ( 'NONE',  ( 0.000000000000000000, 0.000000000000000000, 5.000000000000000000 ) ) ;
#95169 = FACE_OUTER_BOUND ( 'NONE', #115997, .T. ) ;
#95170 = EDGE_LOOP ( 'NONE', ( #72959, #72835, #35607, #48263 ) ) ;
#95171 = AXIS2_PLACEMENT_3D ( 'NONE', #41443, #19692, #129891 ) ;
#95172 = VECTOR ( 'NONE', #70693, 1000.000000000000000 ) ;
#95174 = DIRECTION ( 'NONE',  ( -0.3543493200069162685, -0.000000000000000000, -0.9351131265310288487 ) ) ;
#95173 =( GEOMETRIC_REPRESENTATION_CONTEXT ( 3 ) GLOBAL_UNCERTAINTY_ASSIGNED_CONTEXT ( ( #15491 ) ) GLOBAL_UNIT_ASSIGNED_CONTEXT ( ( #83953, #49887, #117227 ) ) REPRESENTATION_CONTEXT ( 'NONE', 'WORKASPACE' ) );
#95175 = CARTESIAN_POINT ( 'NONE',  ( -13.82816939922343380, 6.759292476615643253, 4.000000000000000000 ) ) ;
#95176 = CARTESIAN_POINT ( 'NONE',  ( 9.792893218813395251, 0.7592924766157104211, 5.000000000000000000 ) ) ;
#95177 = ORIENTED_EDGE ( 'NONE', *, *, #24278, .T. ) ;
#95178 = LINE ( 'NONE', #85020, #120275 ) ;
#95179 = LINE ( 'NONE', #18306, #128011 ) ;
#95180 = CYLINDRICAL_SURFACE ( 'NONE', #60936, 7.950000000000000178 ) ;
#95181 = DIRECTION ( 'NONE',  ( -0.7071067811865486830, -0.7071067811865464625, -0.000000000000000000 ) ) ;
#95182 = DIRECTION ( 'NONE',  ( 0.7071067811865486830, -0.7071067811865464625, -0.000000000000000000 ) ) ;
#95183 = ORIENTED_EDGE ( 'NONE', *, *, #18009, .T. ) ;
#95184 = AXIS2_PLACEMENT_3D ( 'NONE', #142305, #19778, #107506 ) ;
#95185 = EDGE_CURVE ( 'NONE', #54925, #109538, #55839, .T. ) ;
#95186 = ORIENTED_EDGE ( 'NONE', *, *, #32465, .T. ) ;
#95187 = DIRECTION ( 'NONE',  ( -1.000000000000000000, -1.224606353822377258E-16, -0.000000000000000000 ) ) ;
#95188 = FACE_OUTER_BOUND ( 'NONE', #96708, .T. ) ;
#95189 = CARTESIAN_POINT ( 'NONE',  ( 11.06206980810188689, -7.934999999999991616, -2.126176841940955242 ) ) ;
#95190 = FACE_OUTER_BOUND ( 'NONE', #130731, .T. ) ;
#95191 = EDGE_CURVE ( 'NONE', #58453, #99164, #19609, .T. ) ;
#95192 = VECTOR ( 'NONE', #141101, 1000.000000000000000 ) ;
#95193 = LINE ( 'NONE', #22601, #71484 ) ;
#95194 = CARTESIAN_POINT ( 'NONE',  ( 34.49999999999976552, 3.653845994658424523, -4.504631822206450309 ) ) ;
#95195 = EDGE_CURVE ( 'NONE', #9261, #99565, #86318, .T. ) ;
#95196 = VERTEX_POINT ( 'NONE', #65293 ) ;
#95197 = PLANE ( 'NONE',  #48857 ) ;
#95198 = EDGE_CURVE ( 'NONE', #19553, #22039, #120312, .T. ) ;
#95199 = DIRECTION ( 'NONE',  ( 0.7071067811865487940, 0.7071067811865463515, 0.000000000000000000 ) ) ;
#95200 = VECTOR ( 'NONE', #43210, 1000.000000000000227 ) ;
#95201 = DIRECTION ( 'NONE',  ( -0.000000000000000000, -0.3543493200069152693, 0.9351131265310292928 ) ) ;
#95202 = VECTOR ( 'NONE', #18683, 1000.000000000000000 ) ;
#95203 = CARTESIAN_POINT ( 'NONE',  ( 13.49159235450332162, -2.500000000000000000, 3.061616997868384127E-16 ) ) ;
#95204 = EDGE_CURVE ( 'NONE', #49880, #99232, #64548, .T. ) ;
#95205 = CARTESIAN_POINT ( 'NONE',  ( 46.72459685856476597, -1.637169565754161171, 6.109999999999998543 ) ) ;
#95206 = DIRECTION ( 'NONE',  ( -1.000000000000000000, -1.224606353822377258E-16, -0.000000000000000000 ) ) ;
#95207 = ORIENTED_EDGE ( 'NONE', *, *, #46108, .T. ) ;
#95208 = CARTESIAN_POINT ( 'NONE',  ( -13.49999999999990408, 22.01701374228154506, 2.453858888625662704 ) ) ;
#95209 = ORIENTED_EDGE ( 'NONE', *, *, #66473, .T. ) ;
#95210 = EDGE_CURVE ( 'NONE', #114819, #43430, #52930, .T. ) ;
#95211 = ORIENTED_EDGE ( 'NONE', *, *, #119713, .F. ) ;
#95212 = CONICAL_SURFACE ( 'NONE', #16550, 2.055000000000000604, 0.9599310885968764806 ) ;
#95213 = DIRECTION ( 'NONE',  ( 0.7071067811865487940, 0.7071067811865463515, 0.000000000000000000 ) ) ;
#95214 = PLANE ( 'NONE',  #143311 ) ;
#95215 = CARTESIAN_POINT ( 'NONE',  ( -32.99999999999977973, -22.06887692260758982, 4.000000000000000000 ) ) ;
#95216 = EDGE_CURVE ( 'NONE', #13538, #124237, #108728, .T. ) ;
#95217 = DIRECTION ( 'NONE',  ( -0.000000000000000000, 0.000000000000000000, 1.000000000000000000 ) ) ;
#95218 = EDGE_CURVE ( 'NONE', #39945, #111361, #99288, .T. ) ;
#95219 = DIRECTION ( 'NONE',  ( -0.6830127018922181881, 0.6830127018922202975, -0.2588190451025214056 ) ) ;
#95220 = ORIENTED_EDGE ( 'NONE', *, *, #88725, .T. ) ;
#95221 = DIRECTION ( 'NONE',  ( 0.7071067811865486830, -0.7071067811865464625, -0.000000000000000000 ) ) ;
#95222 = CARTESIAN_POINT ( 'NONE',  ( 24.39999999999999858, -1.599999999999997202, -17.44999999999996732 ) ) ;
#95224 = AXIS2_PLACEMENT_3D ( 'NONE', #10181, #76177, #46440 ) ;
#95223 = DIRECTION ( 'NONE',  ( -0.6830127018922181881, 0.6830127018922202975, -0.2588190451025214056 ) ) ;
#95225 = SURFACE_STYLE_USAGE ( .BOTH. , #51027 ) ;
#95226 = CARTESIAN_POINT ( 'NONE',  ( -5.483345613589513334, 22.22500000000000142, 4.500000000000000888 ) ) ;
#95227 = EDGE_CURVE ( 'NONE', #68140, #62699, #76147, .T. ) ;
#95228 = PLANE ( 'NONE',  #142965 ) ;
#95229 = CARTESIAN_POINT ( 'NONE',  ( 67.60002705046289861, 5.819803920172570422, 5.819803920172574863 ) ) ;
#95230 = CARTESIAN_POINT ( 'NONE',  ( 127.3989248045490967, 0.000000000000000000, -6.349999999999997868 ) ) ;
#95231 = ORIENTED_EDGE ( 'NONE', *, *, #62219, .T. ) ;
#95232 = ORIENTED_EDGE ( 'NONE', *, *, #46483, .F. ) ;
#95233 = CARTESIAN_POINT ( 'NONE',  ( 52.77083333333332149, -7.949999999999999289, -2.130196079827426203 ) ) ;
#95234 = CARTESIAN_POINT ( 'NONE',  ( -69.29974487139159578, -27.71228299555254537, 4.000000000000000000 ) ) ;
#95235 = CARTESIAN_POINT ( 'NONE',  ( 57.29974487139158157, -27.71228299555246011, 4.000000000000000000 ) ) ;
#95236 = SURFACE_STYLE_FILL_AREA ( #134677 ) ;
#95237 = ORIENTED_EDGE ( 'NONE', *, *, #37435, .T. ) ;
#95238 = CIRCLE ( 'NONE', #99906, 2.500000000000000444 ) ;
#95239 = CARTESIAN_POINT ( 'NONE',  ( 45.29974487139158867, -27.71228299555237840, 4.000000000000000000 ) ) ;
#95240 = VECTOR ( 'NONE', #52357, 1000.000000000000227 ) ;
#95241 = VECTOR ( 'NONE', #34326, 1000.000000000000000 ) ;
#95242 = CARTESIAN_POINT ( 'NONE',  ( 54.68793019189810423, 6.110000000000002984, -1.637169565754156730 ) ) ;
#95243 = ORIENTED_EDGE ( 'NONE', *, *, #112227, .F. ) ;
#95244 = ADVANCED_FACE ( 'NONE', ( #98595 ), #33392, .F. ) ;
#95245 = CARTESIAN_POINT ( 'NONE',  ( 24.29974487139158867, -27.71228299555223273, 4.000000000000000000 ) ) ;
#95246 = EDGE_LOOP ( 'NONE', ( #82183, #88298, #20080, #6027 ) ) ;
#95247 = ORIENTED_EDGE ( 'NONE', *, *, #48479, .F. ) ;
#95248 = VECTOR ( 'NONE', #45870, 1000.000000000000000 ) ;
#95249 = AXIS2_PLACEMENT_3D ( 'NONE', #20851, #131781, #109301 ) ;
#95250 = VECTOR ( 'NONE', #113629, 1000.000000000000000 ) ;
#95251 = DIRECTION ( 'NONE',  ( -0.7071067811865486830, -0.7071067811865464625, 0.000000000000000000 ) ) ;
#95253 = CARTESIAN_POINT ( 'NONE',  ( -14.99451991528749595, 28.92564299267948513, 4.000000000000000000 ) ) ;
#95252 = CIRCLE ( 'NONE', #32783, 5.000000000000000888 ) ;
#95254 = CARTESIAN_POINT ( 'NONE',  ( 21.48921356237309155, -27.52281430457070499, 5.000000000000000000 ) ) ;
#95255 = DIRECTION ( 'NONE',  ( 0.6830127018922181881, 0.6830127018922202975, -0.2588190451025214056 ) ) ;
#95256 = DIRECTION ( 'NONE',  ( -0.3543493200069163240, 0.000000000000000000, 0.9351131265310288487 ) ) ;
#95258 = EDGE_LOOP ( 'NONE', ( #68785, #53092, #72428, #12369 ) ) ;
#95257 = FACE_OUTER_BOUND ( 'NONE', #79270, .T. ) ;
#95259 = DIRECTION ( 'NONE',  ( 0.7071067811865486830, -0.7071067811865464625, -0.000000000000000000 ) ) ;
#95260 = CARTESIAN_POINT ( 'NONE',  ( -29.47599861414530764, 22.03583458319437938, 4.979811245910090278 ) ) ;
#95261 = CARTESIAN_POINT ( 'NONE',  ( -25.49999999999982236, -20.53675388469232743, 2.352720554255833818 ) ) ;
#95262 = VECTOR ( 'NONE', #109705, 1000.000000000000227 ) ;
#95263 = DIRECTION ( 'NONE',  ( 0.7071067811865486830, -0.7071067811865464625, -0.000000000000000000 ) ) ;
#95264 = DIRECTION ( 'NONE',  ( -0.000000000000000000, -0.3543493200069152693, 0.9351131265310292928 ) ) ;
#95265 = ORIENTED_EDGE ( 'NONE', *, *, #126139, .F. ) ;
#95266 = EDGE_LOOP ( 'NONE', ( #50482, #23930, #32514, #36476 ) ) ;
#95267 = AXIS2_PLACEMENT_3D ( 'NONE', #132255, #77165, #41634 ) ;
#95268 = DIRECTION ( 'NONE',  ( -0.000000000000000000, 0.000000000000000000, 1.000000000000000000 ) ) ;
#95269 = CARTESIAN_POINT ( 'NONE',  ( 77.78709685856478018, 3.054999999999997495, 5.291415217122919401 ) ) ;
#95270 = DIRECTION ( 'NONE',  ( -0.7071067811865486830, -0.7071067811865463515, 0.000000000000000000 ) ) ;
#95271 = EDGE_CURVE ( 'NONE', #99346, #98689, #87731, .T. ) ;
#95272 = DIRECTION ( 'NONE',  ( 0.000000000000000000, 0.000000000000000000, -1.000000000000000000 ) ) ;
#95273 = CARTESIAN_POINT ( 'NONE',  ( 72.26669371712955581, -7.949999999999998401, 2.130196079827423983 ) ) ;
#95274 = ORIENTED_EDGE ( 'NONE', *, *, #132629, .F. ) ;
#95275 = EDGE_LOOP ( 'NONE', ( #66491, #127069, #92302, #67426, #70167 ) ) ;
#95276 = CYLINDRICAL_SURFACE ( 'NONE', #58526, 2.500000000000000444 ) ;
#95277 = CARTESIAN_POINT ( 'NONE',  ( 0.000000000000000000, 0.000000000000000000, 0.000000000000000000 ) ) ;
#95278 = ORIENTED_EDGE ( 'NONE', *, *, #79973, .T. ) ;
#95279 = VECTOR ( 'NONE', #21839, 999.9999999999998863 ) ;
#95280 = VERTEX_POINT ( 'NONE', #135534 ) ;
#95281 = VECTOR ( 'NONE', #34670, 999.9999999999998863 ) ;
#95282 = ADVANCED_FACE ( 'NONE', ( #92709 ), #123238, .F. ) ;
#95283 = DIRECTION ( 'NONE',  ( -0.7071067811865486830, -0.7071067811865464625, -0.000000000000000000 ) ) ;
#95284 = VERTEX_POINT ( 'NONE', #103580 ) ;
#95285 = VECTOR ( 'NONE', #88589, 1000.000000000000000 ) ;
#95286 = CARTESIAN_POINT ( 'NONE',  ( 0.000000000000000000, 0.5999999999999987566, 3.054668707061621191 ) ) ;
#95287 = VECTOR ( 'NONE', #20864, 1000.000000000000000 ) ;
#95288 = EDGE_CURVE ( 'NONE', #109290, #7602, #125362, .T. ) ;
#95289 = FACE_BOUND ( 'NONE', #131865, .T. ) ;
#95290 = CARTESIAN_POINT ( 'NONE',  ( -17.24139925780192328, 21.72500000000000142, 5.000000000000000000 ) ) ;
#95291 = CARTESIAN_POINT ( 'NONE',  ( -34.92500000000001137, -22.22500000000000142, 4.500000000000000888 ) ) ;
#95292 = DIRECTION ( 'NONE',  ( -0.5735764363510499342, -0.8191520442889891340, 0.000000000000000000 ) ) ;
#95294 = ORIENTED_EDGE ( 'NONE', *, *, #70403, .T. ) ;
#95293 = LINE ( 'NONE', #127202, #24897 ) ;
#95295 = DIRECTION ( 'NONE',  ( -0.6830127018922181881, 0.6830127018922202975, -0.2588190451025214056 ) ) ;
#95296 = ITEM_DEFINED_TRANSFORMATION ( 'NONE', 'NONE', #42402,  #127880 ) ;
#95297 = ORIENTED_EDGE ( 'NONE', *, *, #80612, .F. ) ;
#95298 = EDGE_LOOP ( 'NONE', ( #120308, #55883, #59950, #84614 ) ) ;
#95299 = CARTESIAN_POINT ( 'NONE',  ( 87.26626352523145158, 4.472830434245838482, -4.472830434245837594 ) ) ;
#95300 = ORIENTED_EDGE ( 'NONE', *, *, #140571, .F. ) ;
#95301 = CARTESIAN_POINT ( 'NONE',  ( -22.99806943317885555, -22.22500000000000142, 4.500000000000000888 ) ) ;
#95302 = CARTESIAN_POINT ( 'NONE',  ( -34.49999999999976552, 6.277155672890240012, -3.510561720658863738 ) ) ;
#95303 = VECTOR ( 'NONE', #88863, 1000.000000000000000 ) ;
#95304 = CARTESIAN_POINT ( 'NONE',  ( 33.18398860626899705, 28.73617430169810305, 5.000000000000000000 ) ) ;
#95305 = VECTOR ( 'NONE', #74178, 1000.000000000000000 ) ;
#95306 = CARTESIAN_POINT ( 'NONE',  ( -39.29974487139159578, -27.71228299555233576, 4.000000000000000000 ) ) ;
#95307 = EDGE_LOOP ( 'NONE', ( #142767, #43156, #43763, #89236, #84593 ) ) ;
#95308 = FACE_OUTER_BOUND ( 'NONE', #86057, .T. ) ;
#95309 = EDGE_CURVE ( 'NONE', #71472, #81871, #112345, .T. ) ;
#95310 = LINE ( 'NONE', #81617, #59377 ) ;
#95311 = LINE ( 'NONE', #81618, #126799 ) ;
#95312 = AXIS2_PLACEMENT_3D ( 'NONE', #84645, #107092, #7767 ) ;
#95313 = DIRECTION ( 'NONE',  ( 0.7071067811865487940, -0.7071067811865463515, 0.000000000000000000 ) ) ;
#95314 = DIRECTION ( 'NONE',  ( -1.000000000000000000, -0.000000000000000000, 0.000000000000000000 ) ) ;
#95315 = LINE ( 'NONE', #140262, #39307 ) ;
#95316 = AXIS2_PLACEMENT_3D ( 'NONE', #99442, #108, #22584 ) ;
#95317 = LINE ( 'NONE', #84475, #123250 ) ;
#95318 = VERTEX_POINT ( 'NONE', #101451 ) ;
#95319 = CARTESIAN_POINT ( 'NONE',  ( 9.850051285410186708, -8.240707523384193323, 17.25253755692241242 ) ) ;
#95320 =( BOUNDED_CURVE ( )  B_SPLINE_CURVE ( 3, ( #123270, #66727, #89197, #12327 ),
 .UNSPECIFIED., .F., .T. ) 
 B_SPLINE_CURVE_WITH_KNOTS ( ( 4, 4 ),
 ( 5.005968288816719181, 5.074607125596323876 ),
 .UNSPECIFIED. ) 
 CURVE ( )  GEOMETRIC_REPRESENTATION_ITEM ( )  RATIONAL_B_SPLINE_CURVE ( ( 1.000000000000000000, 0.9996074310407765395, 0.9996074310407765395, 1.000000000000000000 ) ) 
 REPRESENTATION_ITEM ( '' )  );
#95321 = LINE ( 'NONE', #117062, #58262 ) ;
#95322 = ORIENTED_EDGE ( 'NONE', *, *, #122923, .F. ) ;
#95323 = EDGE_CURVE ( 'NONE', #14445, #102139, #33537, .T. ) ;
#95324 = ORIENTED_EDGE ( 'NONE', *, *, #52904, .T. ) ;
#95325 = EDGE_CURVE ( 'NONE', #95030, #100698, #79033, .T. ) ;
#95326 = VERTEX_POINT ( 'NONE', #124637 ) ;
#95327 = CARTESIAN_POINT ( 'NONE',  ( 43.16709685856477563, -3.055000000000000160, -5.291415217122921177 ) ) ;
#95328 = AXIS2_PLACEMENT_3D ( 'NONE', #34452, #3231, #78676 ) ;
#95329 = ORIENTED_EDGE ( 'NONE', *, *, #49623, .T. ) ;
#95330 = CARTESIAN_POINT ( 'NONE',  ( 18.85830628287044419, -1.633150327867689988, 6.094999999999989981 ) ) ;
#95331 = ORIENTED_EDGE ( 'NONE', *, *, #139230, .T. ) ;
#95332 = CARTESIAN_POINT ( 'NONE',  ( 33.48921356237309510, -27.52281430457078670, 5.000000000000000000 ) ) ;
#95333 = ORIENTED_EDGE ( 'NONE', *, *, #14711, .F. ) ;
#95334 = LINE ( 'NONE', #17075, #95040 ) ;
#95335 = CARTESIAN_POINT ( 'NONE',  ( 10.37159235450332062, 3.061616997868380183E-16, -2.500000000000001332 ) ) ;
#95336 = CIRCLE ( 'NONE', #139372, 1.000000000000000888 ) ;
#95338 = ORIENTED_EDGE ( 'NONE', *, *, #26179, .T. ) ;
#95337 = FACE_OUTER_BOUND ( 'NONE', #35394, .T. ) ;
#95339 = ORIENTED_EDGE ( 'NONE', *, *, #75145, .T. ) ;
#95340 = EDGE_CURVE ( 'NONE', #92930, #123203, #58732, .T. ) ;
#95341 = FACE_OUTER_BOUND ( 'NONE', #5962, .T. ) ;
#95342 = VECTOR ( 'NONE', #137612, 1000.000000000000000 ) ;
#95344 = ORIENTED_EDGE ( 'NONE', *, *, #66320, .F. ) ;
#95343 = VECTOR ( 'NONE', #68255, 1000.000000000000000 ) ;
#95345 = LINE ( 'NONE', #139609, #69007 ) ;
#95346 = ORIENTED_EDGE ( 'NONE', *, *, #35669, .T. ) ;
#95347 = ORIENTED_EDGE ( 'NONE', *, *, #61253, .T. ) ;
#95348 = VERTEX_POINT ( 'NONE', #67431 ) ;
#95349 = ORIENTED_EDGE ( 'NONE', *, *, #85915, .T. ) ;
#95350 = CARTESIAN_POINT ( 'NONE',  ( 14.86920357848291196, 3.821174125832445049E-16, 0.000000000000000000 ) ) ;
#95351 = AXIS2_PLACEMENT_3D ( 'NONE', #109147, #43911, #21439 ) ;
#95352 = AXIS2_PLACEMENT_3D ( 'NONE', #119977, #107698, #8357 ) ;
#95353 = VECTOR ( 'NONE', #37684, 1000.000000000000000 ) ;
#95354 = DIRECTION ( 'NONE',  ( 0.3543493200069162685, -0.000000000000000000, -0.9351131265310288487 ) ) ;
#95355 = LINE ( 'NONE', #4719, #30944 ) ;
#95356 = CARTESIAN_POINT ( 'NONE',  ( -51.48921356237309510, -27.52281430457091460, 5.000000000000000000 ) ) ;
#95357 = VERTEX_POINT ( 'NONE', #69580 ) ;
#95358 = CARTESIAN_POINT ( 'NONE',  ( 67.50000000000000000, 0.000000000000000000, -7.950000000000000178 ) ) ;
#95359 = EDGE_LOOP ( 'NONE', ( #1391, #65928, #109052, #97756 ) ) ;
#95360 = PLANE ( 'NONE',  #72589 ) ;
#95361 = CARTESIAN_POINT ( 'NONE',  ( 28.85373647476855652, -5.808823158059035485, -5.808823158059033709 ) ) ;
#95362 = CARTESIAN_POINT ( 'NONE',  ( 6.489213562373093325, -27.52281430457059841, 5.000000000000000000 ) ) ;
#95363 = EDGE_CURVE ( 'NONE', #85586, #15513, #1400, .T. ) ;
#95364 = ORIENTED_EDGE ( 'NONE', *, *, #11517, .T. ) ;
#95365 = CARTESIAN_POINT ( 'NONE',  ( 23.48334561358938899, 22.22500000000000142, 4.500000000000000888 ) ) ;
#95366 = DIRECTION ( 'NONE',  ( -0.7071067811865487940, 0.7071067811865463515, 0.000000000000000000 ) ) ;
#95367 = ORIENTED_EDGE ( 'NONE', *, *, #108955, .T. ) ;
#95368 = EDGE_CURVE ( 'NONE', #32222, #22382, #3538, .T. ) ;
#95369 = ORIENTED_EDGE ( 'NONE', *, *, #36173, .F. ) ;
#95370 = VERTEX_POINT ( 'NONE', #68861 ) ;
#95371 = DIRECTION ( 'NONE',  ( 1.000000000000000000, 0.000000000000000000, 0.000000000000000000 ) ) ;
#95372 = CARTESIAN_POINT ( 'NONE',  ( -23.54016161050245159, 18.75929247661552424, 8.305906642995433131 ) ) ;
#95373 = CARTESIAN_POINT ( 'NONE',  ( -12.20000000000000284, -40.42999999999999261, -39.50000000000000000 ) ) ;
#95374 = DIRECTION ( 'NONE',  ( -0.7071067811865486830, 0.7071067811865464625, 0.000000000000000000 ) ) ;
#95375 = LINE ( 'NONE', #139643, #38938 ) ;
#95376 = EDGE_CURVE ( 'NONE', #39592, #103460, #34791, .T. ) ;
#95378 = EDGE_CURVE ( 'NONE', #79114, #130423, #90596, .T. ) ;
#95377 = CARTESIAN_POINT ( 'NONE',  ( 79.53709685856478018, -3.054999999999999272, -5.291415217122919401 ) ) ;
#95379 = AXIS2_PLACEMENT_3D ( 'NONE', #10600, #42574, #132455 ) ;
#95380 = CARTESIAN_POINT ( 'NONE',  ( -5.999999999999956479, 15.45873954670184958, -0.03131636524292703144 ) ) ;
#95381 = VECTOR ( 'NONE', #130965, 999.9999999999998863 ) ;
#95382 = CYLINDRICAL_SURFACE ( 'NONE', #11333, 7.950000000000000178 ) ;
#95383 = LINE ( 'NONE', #63514, #134445 ) ;
#95384 = LINE ( 'NONE', #94654, #130032 ) ;
#95385 = AXIS2_PLACEMENT_3D ( 'NONE', #20980, #98547, #35483 ) ;
#95386 = CARTESIAN_POINT ( 'NONE',  ( 41.99451991528749062, 28.92564299267967343, 4.000000000000000000 ) ) ;
#95387 = ORIENTED_EDGE ( 'NONE', *, *, #9920, .T. ) ;
#95389 = VECTOR ( 'NONE', #65506, 1000.000000000000227 ) ;
#95388 = CYLINDRICAL_SURFACE ( 'NONE', #63864, 0.5000000000000004441 ) ;
#95390 = ORIENTED_EDGE ( 'NONE', *, *, #4391, .T. ) ;
#95391 = DIRECTION ( 'NONE',  ( 0.7071067811865487940, -0.7071067811865463515, 0.000000000000000000 ) ) ;
#95393 = ORIENTED_EDGE ( 'NONE', *, *, #7475, .F. ) ;
#95392 = LINE ( 'NONE', #139656, #111 ) ;
#95394 = EDGE_CURVE ( 'NONE', #106218, #131955, #102190, .T. ) ;
#95395 = EDGE_CURVE ( 'NONE', #130550, #45511, #12299, .T. ) ;
#95396 = CARTESIAN_POINT ( 'NONE',  ( 13.49999999999990408, -14.56887692260766443, 4.000000000000000000 ) ) ;
#95397 = EDGE_LOOP ( 'NONE', ( #134816, #83721, #6868, #63745, #87678 ) ) ;
#95398 = ORIENTED_EDGE ( 'NONE', *, *, #74309, .F. ) ;
#95399 = CARTESIAN_POINT ( 'NONE',  ( 15.18398860626900237, 28.73617430169797871, 5.000000000000000000 ) ) ;
#95400 = LINE ( 'NONE', #6920, #67671 ) ;
#95401 = COLOUR_RGB ( '', 0.40784314, 0.44705882, 0.49803922) ;
#95402 = CARTESIAN_POINT ( 'NONE',  ( 24.70710678118637205, -0.7407075233842718154, 5.000000000000000000 ) ) ;
#95403 = EDGE_CURVE ( 'NONE', #104848, #52530, #15138, .T. ) ;
#95404 = CARTESIAN_POINT ( 'NONE',  ( 94.87086038379621300, 6.884901960086289741, -3.974999999999993427 ) ) ;
#95405 = CARTESIAN_POINT ( 'NONE',  ( 2.000000000000011546, 2.638703287232806449, -5.494203305479936184 ) ) ;
#95406 = CARTESIAN_POINT ( 'NONE',  ( -14.99451991528749595, 28.92564299267948513, 4.000000000000000000 ) ) ;
#95407 = ORIENTED_EDGE ( 'NONE', *, *, #29115, .F. ) ;
#95408 = DIRECTION ( 'NONE',  ( 0.7071067811865487940, 0.7071067811865463515, 0.000000000000000000 ) ) ;
#95409 = CARTESIAN_POINT ( 'NONE',  ( 12.69999999999999574, -35.15000000000000568, -39.50000000000000000 ) ) ;
#95411 = VECTOR ( 'NONE', #3424, 1000.000000000000227 ) ;
#95410 = CARTESIAN_POINT ( 'NONE',  ( 31.20833333333333570, 3.047499999999997655, 5.278424836066143655 ) ) ;
#95412 = EDGE_CURVE ( 'NONE', #28959, #137771, #91324, .T. ) ;
#95414 = AXIS2_PLACEMENT_3D ( 'NONE', #16569, #37656, #15825 ) ;
#95413 = CARTESIAN_POINT ( 'NONE',  ( 15.48921356237309510, -27.52281430457066236, 5.000000000000000000 ) ) ;
#95415 = ORIENTED_EDGE ( 'NONE', *, *, #102841, .F. ) ;
#95416 = LINE ( 'NONE', #84566, #137063 ) ;
#95417 = ORIENTED_EDGE ( 'NONE', *, *, #27579, .T. ) ;
#95418 = CARTESIAN_POINT ( 'NONE',  ( 83.70876352523143282, -7.482591942790329030E-16, 6.110000000000001208 ) ) ;
#95419 = LINE ( 'NONE', #140356, #15302 ) ;
#95420 = EDGE_CURVE ( 'NONE', #106925, #102891, #56584, .T. ) ;
#95422 = VECTOR ( 'NONE', #102171, 1000.000000000000000 ) ;
#95421 = DIRECTION ( 'NONE',  ( 1.000000000000000000, 0.000000000000000000, 0.000000000000000000 ) ) ;
#95423 = DIRECTION ( 'NONE',  ( 0.7071067811865487940, 0.7071067811865463515, 0.000000000000000000 ) ) ;
#95424 = ORIENTED_EDGE ( 'NONE', *, *, #38607, .T. ) ;
#95425 = CARTESIAN_POINT ( 'NONE',  ( 22.49999999999984368, 22.01701374228156638, 2.453858888625576995 ) ) ;
#95426 = CARTESIAN_POINT ( 'NONE',  ( 15.79289321881334907, -2.240707523384260824, 5.000000000000000000 ) ) ;
#95427 = DIRECTION ( 'NONE',  ( -0.6830127018922180770, -0.6830127018922204085, -0.2588190451025213501 ) ) ;
#95429 = VERTEX_POINT ( 'NONE', #127493 ) ;
#95428 = DIRECTION ( 'NONE',  ( -1.000000000000000000, 0.000000000000000000, 0.000000000000000000 ) ) ;
#95430 = CARTESIAN_POINT ( 'NONE',  ( -3.183988606268992161, 28.73617430169789699, 5.000000000000000000 ) ) ;
#95431 = DIRECTION ( 'NONE',  ( 0.000000000000000000, -1.000000000000000000, 0.000000000000000000 ) ) ;
#95432 = VECTOR ( 'NONE', #108939, 999.9999999999998863 ) ;
#95433 = CARTESIAN_POINT ( 'NONE',  ( 1.495847097294773720, -1.845811315201534741, 6.347071198332229436 ) ) ;
#95434 =( LENGTH_UNIT ( ) NAMED_UNIT ( * ) SI_UNIT ( .MILLI., .METRE. ) );
#95435 = VERTEX_POINT ( 'NONE', #81893 ) ;
#95436 = EDGE_CURVE ( 'NONE', #126052, #17266, #94835, .T. ) ;
#95437 = ORIENTED_EDGE ( 'NONE', *, *, #62455, .T. ) ;
#95438 = CARTESIAN_POINT ( 'NONE',  ( 70.58376352523143282, -6.110000000000001208, -3.741295971395164515E-16 ) ) ;
#95439 = ORIENTED_EDGE ( 'NONE', *, *, #68285, .F. ) ;
#95440 = DIRECTION ( 'NONE',  ( 0.7071067811865486830, -0.7071067811865464625, -0.000000000000000000 ) ) ;
#95441 = LINE ( 'NONE', #59984, #12986 ) ;
#95442 = ORIENTED_EDGE ( 'NONE', *, *, #69011, .F. ) ;
#95443 = VECTOR ( 'NONE', #86650, 1000.000000000000227 ) ;
#95444 = AXIS2_PLACEMENT_3D ( 'NONE', #45747, #58794, #89919 ) ;
#95445 = CARTESIAN_POINT ( 'NONE',  ( -3.516654386410431599, 22.22500000000000142, 4.500000000000000888 ) ) ;
#95446 = CARTESIAN_POINT ( 'NONE',  ( -1.499999999999990896, 9.431123077392095766, 4.000000000000000000 ) ) ;
#95447 = VECTOR ( 'NONE', #20626, 1000.000000000000000 ) ;
#95448 = AXIS2_PLACEMENT_3D ( 'NONE', #35620, #124024, #24694 ) ;
#95449 = VERTEX_POINT ( 'NONE', #71704 ) ;
#95450 = ADVANCED_FACE ( 'NONE', ( #40505 ), #4950, .F. ) ;
#95451 = CARTESIAN_POINT ( 'NONE',  ( 0.1743335836340011991, -1.312101830529059265, 3.997104009112169010 ) ) ;
#95453 = CARTESIAN_POINT ( 'NONE',  ( 33.91252705046289861, -7.949999999999998401, -4.867971026610728450E-16 ) ) ;
#95452 = CIRCLE ( 'NONE', #132552, 5.968999999999998529 ) ;
#95454 = CARTESIAN_POINT ( 'NONE',  ( -34.92500000000001137, -22.22500000000000142, 4.000000000000000000 ) ) ;
#95455 = VECTOR ( 'NONE', #72098, 1000.000000000000227 ) ;
#95456 =( GEOMETRIC_REPRESENTATION_CONTEXT ( 3 ) GLOBAL_UNCERTAINTY_ASSIGNED_CONTEXT ( ( #77928 ) ) GLOBAL_UNIT_ASSIGNED_CONTEXT ( ( #7896, #63051, #106480 ) ) REPRESENTATION_CONTEXT ( 'NONE', 'WORKASPACE' ) );
#95457 = ORIENTED_EDGE ( 'NONE', *, *, #56656, .F. ) ;
#95458 = EDGE_LOOP ( 'NONE', ( #79065, #130401, #114943, #19348, #124762 ) ) ;
#95459 = EDGE_CURVE ( 'NONE', #115783, #44574, #93444, .T. ) ;
#95460 = PLANE ( 'NONE',  #38561 ) ;
#95461 = CARTESIAN_POINT ( 'NONE',  ( 36.48921356237310221, -27.52281430457080802, 5.000000000000000000 ) ) ;
#95462 = LINE ( 'NONE', #49852, #118304 ) ;
#95463 = LINE ( 'NONE', #116513, #130038 ) ;
#95464 = DIRECTION ( 'NONE',  ( -0.000000000000000000, 0.3543493200069153248, 0.9351131265310292928 ) ) ;
#95465 = ORIENTED_EDGE ( 'NONE', *, *, #131364, .F. ) ;
#95466 = ORIENTED_EDGE ( 'NONE', *, *, #95412, .T. ) ;
#95467 = ORIENTED_EDGE ( 'NONE', *, *, #46465, .F. ) ;
#95468 = ORIENTED_EDGE ( 'NONE', *, *, #20244, .T. ) ;
#95469 = EDGE_CURVE ( 'NONE', #132519, #85530, #139099, .T. ) ;
#95470 = CARTESIAN_POINT ( 'NONE',  ( 184.1383206845090967, -50.55966373067078479, 35.89041033429542438 ) ) ;
#95471 = PRESENTATION_LAYER_ASSIGNMENT (  '', '', ( #49265 ) ) ;
#95472 = DIRECTION ( 'NONE',  ( 0.000000000000000000, 0.000000000000000000, 1.000000000000000000 ) ) ;
#95473 = ORIENTED_EDGE ( 'NONE', *, *, #116679, .T. ) ;
#95474 = DIRECTION ( 'NONE',  ( -0.000000000000000000, -0.3543493200069152693, 0.9351131265310292928 ) ) ;
#95475 = ADVANCED_FACE ( 'NONE', ( #26750 ), #84028, .F. ) ;
#95476 = AXIS2_PLACEMENT_3D ( 'NONE', #76665, #98395, #133874 ) ;
#95477 = DIRECTION ( 'NONE',  ( -0.7071067811865486830, 0.7071067811865464625, 0.000000000000000000 ) ) ;
#95478 = LINE ( 'NONE', #73060, #104029 ) ;
#95479 = VECTOR ( 'NONE', #109344, 1000.000000000000227 ) ;
#95480 = CARTESIAN_POINT ( 'NONE',  ( 29.99999999999979039, -8.731860332648819778, -2.120594902707469309 ) ) ;
#95481 = EDGE_LOOP ( 'NONE', ( #85880, #105537, #43071, #125855 ) ) ;
#95482 = CARTESIAN_POINT ( 'NONE',  ( -32.99999999999976552, -9.033600742197641864, 5.000000000000000000 ) ) ;
#95483 = CARTESIAN_POINT ( 'NONE',  ( 51.31249999999999289, 5.819803920172571310, 5.819803920172576639 ) ) ;
#95484 = ORIENTED_EDGE ( 'NONE', *, *, #121653, .T. ) ;
#95485 = EDGE_CURVE ( 'NONE', #115809, #51152, #84705, .T. ) ;
#95486 = LINE ( 'NONE', #83946, #50381 ) ;
#95487 = ORIENTED_EDGE ( 'NONE', *, *, #13226, .F. ) ;
#95489 = EDGE_CURVE ( 'NONE', #12889, #51279, #83281, .T. ) ;
#95488 = CARTESIAN_POINT ( 'NONE',  ( 13.02497294953710849, -4.461849672132299993, -4.461849672132299105 ) ) ;
#95490 = ORIENTED_EDGE ( 'NONE', *, *, #40328, .T. ) ;
#95491 = CARTESIAN_POINT ( 'NONE',  ( 77.00043019189811844, -3.055000000000002380, 5.291415217122920289 ) ) ;
#95492 = VERTEX_POINT ( 'NONE', #38352 ) ;
#95493 = CARTESIAN_POINT ( 'NONE',  ( 0.000000000000000000, 0.000000000000000000, 5.000000000000000000 ) ) ;
#95494 = DIRECTION ( 'NONE',  ( 0.000000000000000000, 0.000000000000000000, 1.000000000000000000 ) ) ;
#95495 = CARTESIAN_POINT ( 'NONE',  ( 108.2087635252314470, -7.482591942790329030E-16, 6.110000000000001208 ) ) ;
#95496 = FACE_OUTER_BOUND ( 'NONE', #94302, .T. ) ;
#95497 = EDGE_CURVE ( 'NONE', #100985, #139718, #128224, .T. ) ;
#95499 = CARTESIAN_POINT ( 'NONE',  ( -2.816011393730999401, 28.73617430169785436, 5.000000000000000000 ) ) ;
#95498 = VECTOR ( 'NONE', #120764, 999.9999999999998863 ) ;
#95500 = DIRECTION ( 'NONE',  ( -0.6830127018922181881, 0.6830127018922202975, -0.2588190451025214056 ) ) ;
#95501 = CARTESIAN_POINT ( 'NONE',  ( -12.79333936457838661, 21.75929247661549581, 4.998822639870701856 ) ) ;
#95502 = VECTOR ( 'NONE', #130204, 1000.000000000000000 ) ;
#95503 = CYLINDRICAL_SURFACE ( 'NONE', #111851, 4.999999999999998224 ) ;
#95504 = ADVANCED_FACE ( 'NONE', ( #28188 ), #73828, .F. ) ;
#95505 = FACE_OUTER_BOUND ( 'NONE', #124431, .T. ) ;
#95506 = CARTESIAN_POINT ( 'NONE',  ( 11.30840764549667554, 9.139736423841732040E-16, 0.000000000000000000 ) ) ;
#95507 = ORIENTED_EDGE ( 'NONE', *, *, #14169, .T. ) ;
#95508 = DIRECTION ( 'NONE',  ( -0.7071067811865486830, -0.7071067811865464625, 0.000000000000000000 ) ) ;
#95509 = LINE ( 'NONE', #139773, #28970 ) ;
#95510 = ORIENTED_EDGE ( 'NONE', *, *, #128991, .T. ) ;
#95511 = VERTEX_POINT ( 'NONE', #5687 ) ;
#95512 = ORIENTED_EDGE ( 'NONE', *, *, #104573, .T. ) ;
#95514 = ORIENTED_EDGE ( 'NONE', *, *, #18717, .T. ) ;
#95513 = CONICAL_SURFACE ( 'NONE', #7548, 2.500000000000000888, 0.9599310885968822538 ) ;
#95515 = CARTESIAN_POINT ( 'NONE',  ( 42.18398860626899705, 28.73617430169816700, 5.000000000000000000 ) ) ;
#95516 = FACE_OUTER_BOUND ( 'NONE', #131287, .T. ) ;
#95517 = LINE ( 'NONE', #7048, #92642 ) ;
#95518 = CARTESIAN_POINT ( 'NONE',  ( -23.99999999999983302, -12.03360074219761344, 5.000000000000000000 ) ) ;
#95519 = ORIENTED_EDGE ( 'NONE', *, *, #60355, .T. ) ;
#95520 = FILL_AREA_STYLE ('',( #138331 ) ) ;
#95521 = VECTOR ( 'NONE', #13196, 1000.000000000000000 ) ;
#95522 = ORIENTED_EDGE ( 'NONE', *, *, #35829, .T. ) ;
#95523 = CARTESIAN_POINT ( 'NONE',  ( -0.3129301918981140518, -2.126176841940956130, 7.934999999999991616 ) ) ;
#95524 = PLANE ( 'NONE',  #63220 ) ;
#95525 = ADVANCED_FACE ( 'NONE', ( #52080 ), #95571, .F. ) ;
#95526 = LINE ( 'NONE', #26714, #32040 ) ;
#95527 = CARTESIAN_POINT ( 'NONE',  ( 13.79782509673477087, -9.118585253093964837, 2.676058911687216213 ) ) ;
#95528 = ORIENTED_EDGE ( 'NONE', *, *, #627, .F. ) ;
#95529 = EDGE_CURVE ( 'NONE', #14760, #65516, #60120, .T. ) ;
#95530 = ORIENTED_EDGE ( 'NONE', *, *, #47581, .F. ) ;
#95531 = ORIENTED_EDGE ( 'NONE', *, *, #22332, .T. ) ;
#95532 = CARTESIAN_POINT ( 'NONE',  ( -8.207106781186482181, -8.240707523384203981, 5.000000000000000000 ) ) ;
#95533 = DIRECTION ( 'NONE',  ( -0.000000000000000000, -1.000000000000000000, -0.000000000000000000 ) ) ;
#95535 = CARTESIAN_POINT ( 'NONE',  ( -23.99451991528749062, 28.92564299267954908, 4.000000000000000000 ) ) ;
#95534 = AXIS2_PLACEMENT_3D ( 'NONE', #28528, #40139, #108168 ) ;
#95536 = VECTOR ( 'NONE', #56108, 1000.000000000000000 ) ;
#95537 = DIRECTION ( 'NONE',  ( -0.7071067811865486830, -0.7071067811865464625, 0.000000000000000000 ) ) ;
#95538 = CARTESIAN_POINT ( 'NONE',  ( 0.000000000000000000, 0.000000000000000000, 5.000000000000000000 ) ) ;
#95539 = EDGE_CURVE ( 'NONE', #140292, #107648, #82568, .T. ) ;
#95541 = EDGE_CURVE ( 'NONE', #4615, #119637, #138092, .T. ) ;
#95540 = AXIS2_PLACEMENT_3D ( 'NONE', #135673, #48662, #115286 ) ;
#95542 = DIRECTION ( 'NONE',  ( -0.000000000000000000, 0.3543493200069153248, 0.9351131265310292928 ) ) ;
#95544 = VECTOR ( 'NONE', #132269, 1000.000000000000000 ) ;
#95543 = CARTESIAN_POINT ( 'NONE',  ( 10.49999999999993072, 12.05218569542904561, 5.000000000000000000 ) ) ;
#95545 = FACE_OUTER_BOUND ( 'NONE', #55519, .T. ) ;
#95546 = CARTESIAN_POINT ( 'NONE',  ( 51.48921356237309510, -27.52281430457091460, 5.000000000000000000 ) ) ;
#95547 = VERTEX_POINT ( 'NONE', #104286 ) ;
#95548 = CARTESIAN_POINT ( 'NONE',  ( -19.49999999999987210, 10.08746187583915344, 4.000000000000000000 ) ) ;
#95549 = PRESENTATION_LAYER_ASSIGNMENT (  '', '', ( #40037 ) ) ;
#95550 = CIRCLE ( 'NONE', #137281, 2.500000000000000888 ) ;
#95551 =( GEOMETRIC_REPRESENTATION_CONTEXT ( 3 ) GLOBAL_UNCERTAINTY_ASSIGNED_CONTEXT ( ( #89499 ) ) GLOBAL_UNIT_ASSIGNED_CONTEXT ( ( #92601, #125252, #58633 ) ) REPRESENTATION_CONTEXT ( 'NONE', 'WORKASPACE' ) );
#95553 = EDGE_CURVE ( 'NONE', #47748, #69243, #105709, .T. ) ;
#95552 = DIRECTION ( 'NONE',  ( 0.7071067811865487940, 0.7071067811865463515, 0.000000000000000000 ) ) ;
#95554 = ORIENTED_EDGE ( 'NONE', *, *, #26202, .F. ) ;
#95555 = CARTESIAN_POINT ( 'NONE',  ( 15.00548008471250228, 28.92564299267927552, 4.000000000000000000 ) ) ;
#95557 = EDGE_LOOP ( 'NONE', ( #28935, #119398, #48010, #130225 ) ) ;
#95556 = CARTESIAN_POINT ( 'NONE',  ( -2.207106781186521260, -14.24070752338414003, 5.000000000000000000 ) ) ;
#95558 = EDGE_CURVE ( 'NONE', #23935, #90194, #15824, .T. ) ;
#95559 = EDGE_CURVE ( 'NONE', #123136, #48695, #50646, .T. ) ;
#95560 = LINE ( 'NONE', #71692, #100114 ) ;
#95561 = FILL_AREA_STYLE ('',( #141961 ) ) ;
#95562 = ORIENTED_EDGE ( 'NONE', *, *, #30578, .F. ) ;
#95563 = PLANE ( 'NONE',  #127661 ) ;
#95564 = ORIENTED_EDGE ( 'NONE', *, *, #50693, .F. ) ;
#95565 = CARTESIAN_POINT ( 'NONE',  ( 34.92499999999998295, 12.31448516125888126, 8.755464546898146239 ) ) ;
#95566 = CARTESIAN_POINT ( 'NONE',  ( 125.0583603837962272, -7.949999999999997513, -2.130196079827425759 ) ) ;
#95567 = EDGE_CURVE ( 'NONE', #117948, #62641, #57549, .T. ) ;
#95568 = CARTESIAN_POINT ( 'NONE',  ( 0.000000000000000000, 0.000000000000000000, 5.000000000000000000 ) ) ;
#95569 = VECTOR ( 'NONE', #132328, 1000.000000000000000 ) ;
#95570 = ADVANCED_FACE ( 'NONE', ( #110011 ), #31756, .T. ) ;
#95571 = PLANE ( 'NONE',  #115642 ) ;
#95572 = CARTESIAN_POINT ( 'NONE',  ( -31.17183060077625356, 18.75929247661552068, 4.000000000000000000 ) ) ;
#95573 = LINE ( 'NONE', #17979, #17038 ) ;
#95574 = LINE ( 'NONE', #117308, #94672 ) ;
#95575 = CARTESIAN_POINT ( 'NONE',  ( 8.312500000000000000, -4.461849672132299993, -4.461849672132299105 ) ) ;
#95576 = CARTESIAN_POINT ( 'NONE',  ( 11.64540314143521904, -2.126176841940958351, -7.934999999999988951 ) ) ;
#95577 = EDGE_CURVE ( 'NONE', #74437, #35117, #54950, .T. ) ;
#95578 = DIRECTION ( 'NONE',  ( -0.7071067811865486830, 0.7071067811865464625, 0.000000000000000000 ) ) ;
#95579 = CARTESIAN_POINT ( 'NONE',  ( 12.79289321881336683, 9.759292476615623713, 5.000000000000000000 ) ) ;
#95580 = VERTEX_POINT ( 'NONE', #142657 ) ;
#95581 = VECTOR ( 'NONE', #17915, 1000.000000000000227 ) ;
#95582 = ORIENTED_EDGE ( 'NONE', *, *, #54175, .T. ) ;
#95583 = CARTESIAN_POINT ( 'NONE',  ( 79.74999999999998579, -9.735942053221458872E-16, 7.950000000000000178 ) ) ;
#95584 = LINE ( 'NONE', #28204, #44373 ) ;
#95585 = VERTEX_POINT ( 'NONE', #33223 ) ;
#95586 = CIRCLE ( 'NONE', #90962, 2.500000000000000888 ) ;
#95587 = CARTESIAN_POINT ( 'NONE',  ( 91.07919371712955581, 3.975000000000002753, -6.884901960086283523 ) ) ;
#95588 = DIRECTION ( 'NONE',  ( -0.6830127018922180770, -0.6830127018922204085, -0.2588190451025213501 ) ) ;
#95589 = EDGE_CURVE ( 'NONE', #119974, #118230, #121598, .T. ) ;
#95590 = PLANE ( 'NONE',  #1601 ) ;
#95591 = ORIENTED_EDGE ( 'NONE', *, *, #121114, .T. ) ;
#95592 = DIRECTION ( 'NONE',  ( -1.000000000000000000, -0.000000000000000000, -0.000000000000000000 ) ) ;
#95593 = DIRECTION ( 'NONE',  ( -0.7071067811865486830, -0.7071067811865464625, 0.000000000000000000 ) ) ;
#95594 = CARTESIAN_POINT ( 'NONE',  ( 25.49999999999982947, -5.568876922607755908, 4.000000000000000000 ) ) ;
#95595 = CARTESIAN_POINT ( 'NONE',  ( 0.000000000000000000, 0.000000000000000000, 5.000000000000000000 ) ) ;
#95597 = EDGE_LOOP ( 'NONE', ( #52819, #110191, #120946, #108058 ) ) ;
#95596 = CARTESIAN_POINT ( 'NONE',  ( -20.99999999999985434, -11.35517001088073563, -1.126524801160159406 ) ) ;
#95598 = DIRECTION ( 'NONE',  ( -0.000000000000000000, 0.000000000000000000, 1.000000000000000000 ) ) ;
#95599 = EDGE_CURVE ( 'NONE', #101632, #71694, #141968, .T. ) ;
#95600 = LINE ( 'NONE', #83318, #59213 ) ;
#95601 = DIRECTION ( 'NONE',  ( 0.7071067811865487940, -0.7071067811865463515, 0.000000000000000000 ) ) ;
#95602 = PLANE ( 'NONE',  #126246 ) ;
#95603 = CARTESIAN_POINT ( 'NONE',  ( 27.48921356237309155, -27.52281430457074762, 5.000000000000000000 ) ) ;
#95604 = CARTESIAN_POINT ( 'NONE',  ( 57.88343899890263344, -48.52444309369084863, 36.09967824800554581 ) ) ;
#95605 = VECTOR ( 'NONE', #93432, 999.9999999999998863 ) ;
#95606 = EDGE_CURVE ( 'NONE', #108986, #134910, #52767, .T. ) ;
#95607 = VERTEX_POINT ( 'NONE', #77434 ) ;
#95608 = ORIENTED_EDGE ( 'NONE', *, *, #114565, .T. ) ;
#95609 = CARTESIAN_POINT ( 'NONE',  ( 99.31293019189810423, -1.637169565754159617, -6.110000000000001208 ) ) ;
#95610 = VERTEX_POINT ( 'NONE', #21595 ) ;
#95611 = VECTOR ( 'NONE', #80187, 999.9999999999998863 ) ;
#95612 = CARTESIAN_POINT ( 'NONE',  ( 128.1415536296147195, -48.60795469097357113, 38.18754904899810754 ) ) ;
#95613 = VECTOR ( 'NONE', #29266, 999.9999999999998863 ) ;
#95614 = DIRECTION ( 'NONE',  ( -0.7071067811865486830, -0.7071067811865464625, 0.000000000000000000 ) ) ;
#95615 = VERTEX_POINT ( 'NONE', #129620 ) ;
#95616 = EDGE_CURVE ( 'NONE', #78422, #42250, #65856, .T. ) ;
#95617 = DIRECTION ( 'NONE',  ( 0.3543493200069162685, -0.000000000000000000, -0.9351131265310288487 ) ) ;
#95618 = CARTESIAN_POINT ( 'NONE',  ( 10.49999999999992539, -10.04351517176477593, -1.623559851933798814 ) ) ;
#95619 = CARTESIAN_POINT ( 'NONE',  ( 94.99543019189812298, 5.291415217122916737, 3.055000000000001936 ) ) ;
#95620 = ORIENTED_EDGE ( 'NONE', *, *, #47870, .F. ) ;
#95621 = DIRECTION ( 'NONE',  ( 0.000000000000000000, 1.000000000000000000, 0.000000000000000000 ) ) ;
#95622 = EDGE_LOOP ( 'NONE', ( #116963, #41788, #132461, #116201, #129474, #47091, #110474, #43912, #16228 ) ) ;
#95623 = CARTESIAN_POINT ( 'NONE',  ( -30.29974487139158867, -27.71228299555227537, 4.000000000000000000 ) ) ;
#95624 = AXIS2_PLACEMENT_3D ( 'NONE', #72884, #6094, #50371 ) ;
#95625 = CARTESIAN_POINT ( 'NONE',  ( 2.994519915287485734, 28.92564299267940342, 4.000000000000000000 ) ) ;
#95626 = CARTESIAN_POINT ( 'NONE',  ( 34.92499999999998295, 10.70193056682087906, 4.500000000000000888 ) ) ;
#95627 = ORIENTED_EDGE ( 'NONE', *, *, #54998, .F. ) ;
#95628 = VERTEX_POINT ( 'NONE', #20139 ) ;
#95629 = ORIENTED_EDGE ( 'NONE', *, *, #22518, .F. ) ;
#95630 = CARTESIAN_POINT ( 'NONE',  ( 25.39999999999999858, 0.000000000000000000, 6.094999999999989093 ) ) ;
#95631 = LINE ( 'NONE', #139887, #70867 ) ;
#95632 = CARTESIAN_POINT ( 'NONE',  ( 5.754569808101886785, -6.871911579029512218, 3.967499999999996252 ) ) ;
#95633 = VECTOR ( 'NONE', #18738, 999.9999999999998863 ) ;
#95634 = DIRECTION ( 'NONE',  ( 0.000000000000000000, 1.000000000000000000, 0.000000000000000000 ) ) ;
#95635 = ORIENTED_EDGE ( 'NONE', *, *, #57603, .F. ) ;
#95636 = EDGE_LOOP ( 'NONE', ( #56734, #135503, #60674, #9733, #143494 ) ) ;
#95637 = DIRECTION ( 'NONE',  ( 0.000000000000000000, -1.000000000000000000, 0.000000000000000000 ) ) ;
#95639 = EDGE_CURVE ( 'NONE', #34606, #93313, #88287, .T. ) ;
#95638 = EDGE_LOOP ( 'NONE', ( #58233, #15887, #45450, #129538 ) ) ;
#95640 = VERTEX_POINT ( 'NONE', #75973 ) ;
#95641 = AXIS2_PLACEMENT_3D ( 'NONE', #142120, #23131, #20292 ) ;
#95642 = VECTOR ( 'NONE', #117411, 1000.000000000000000 ) ;
#95643 = CARTESIAN_POINT ( 'NONE',  ( -18.18398860626898994, 28.73617430169800002, 5.000000000000000000 ) ) ;
#95644 = ORIENTED_EDGE ( 'NONE', *, *, #136762, .T. ) ;
#95645 = DIRECTION ( 'NONE',  ( -0.3543493200069162685, -0.000000000000000000, -0.9351131265310288487 ) ) ;
#95646 = CARTESIAN_POINT ( 'NONE',  ( -17.29387692260792520, 22.22500000000000142, 4.000000000000000000 ) ) ;
#95647 = AXIS2_PLACEMENT_3D ( 'NONE', #49498, #129149, #7353 ) ;
#95648 = AXIS2_PLACEMENT_3D ( 'NONE', #46118, #57708, #101896 ) ;
#95649 = CARTESIAN_POINT ( 'NONE',  ( 3.299744871391591339, -27.71228299555208352, 4.000000000000000000 ) ) ;
#95650 = CARTESIAN_POINT ( 'NONE',  ( 39.48921356237310221, -27.52281430457082934, 5.000000000000000000 ) ) ;
#95651 = ORIENTED_EDGE ( 'NONE', *, *, #42775, .T. ) ;
#95652 = DIRECTION ( 'NONE',  ( -0.7071067811865486830, -0.7071067811865464625, 0.000000000000000000 ) ) ;
#95653 = CARTESIAN_POINT ( 'NONE',  ( 37.45833333333332860, 3.974999999999997424, 6.884901960086288852 ) ) ;
#95654 = ORIENTED_EDGE ( 'NONE', *, *, #132508, .F. ) ;
#95655 = LINE ( 'NONE', #6461, #71267 ) ;
#95656 = EDGE_CURVE ( 'NONE', #54552, #109346, #99115, .T. ) ;
#95657 = DIRECTION ( 'NONE',  ( -1.000000000000000000, -1.224606353822377258E-16, -0.000000000000000000 ) ) ;
#95658 = CARTESIAN_POINT ( 'NONE',  ( 5.510786437626906675, -27.52281430457051314, 5.000000000000000000 ) ) ;
#95659 = ORIENTED_EDGE ( 'NONE', *, *, #44549, .F. ) ;
#95661 = EDGE_CURVE ( 'NONE', #66820, #57955, #120144, .T. ) ;
#95660 = CARTESIAN_POINT ( 'NONE',  ( 15.07843108771893981, 22.22500000000000142, 23.94816926554818082 ) ) ;
#95662 = ORIENTED_EDGE ( 'NONE', *, *, #108438, .F. ) ;
#95663 = ORIENTED_EDGE ( 'NONE', *, *, #7194, .T. ) ;
#95664 = ORIENTED_EDGE ( 'NONE', *, *, #35700, .T. ) ;
#95665 = EDGE_CURVE ( 'NONE', #3604, #105943, #118748, .T. ) ;
#95666 = EDGE_CURVE ( 'NONE', #45614, #25745, #109307, .T. ) ;
#95667 = CARTESIAN_POINT ( 'NONE',  ( 32.43293019189810877, 1.637169565754156508, 6.110000000000000320 ) ) ;
#95668 = VECTOR ( 'NONE', #3021, 1000.000000000000227 ) ;
#95669 = CARTESIAN_POINT ( 'NONE',  ( -23.99999999999983302, -18.41253812416056945, 4.000000000000000000 ) ) ;
#95670 = CARTESIAN_POINT ( 'NONE',  ( 66.48921356237309510, -27.52281430457101763, 5.000000000000000000 ) ) ;
#95671 = CARTESIAN_POINT ( 'NONE',  ( 2.000000000000000000, 2.375000000000000000, 4.319999999999998508 ) ) ;
#95672 = DIRECTION ( 'NONE',  ( -0.000000000000000000, -0.000000000000000000, -1.000000000000000000 ) ) ;
#95673 = EDGE_CURVE ( 'NONE', #12211, #3321, #74559, .T. ) ;
#95674 = FACE_OUTER_BOUND ( 'NONE', #94609, .T. ) ;
#95675 = DIRECTION ( 'NONE',  ( -0.000000000000000000, -0.3543493200069152693, 0.9351131265310292928 ) ) ;
#95677 = CARTESIAN_POINT ( 'NONE',  ( -15.79289321881334551, -14.24070752338414358, 5.000000000000000000 ) ) ;
#95676 = VECTOR ( 'NONE', #117770, 1000.000000000000000 ) ;
#95678 = EDGE_CURVE ( 'NONE', #49326, #56431, #9991, .T. ) ;
#95679 = CARTESIAN_POINT ( 'NONE',  ( -28.63753812416077693, 22.22499999999999432, 4.000000000000000000 ) ) ;
#95680 = AXIS2_PLACEMENT_3D ( 'NONE', #103193, #4530, #50266 ) ;
#95681 = LINE ( 'NONE', #139937, #54103 ) ;
#95682 = ORIENTED_EDGE ( 'NONE', *, *, #135034, .T. ) ;
#95683 = B_SPLINE_CURVE_WITH_KNOTS ( 'NONE', 3,
 ( #64425, #9283, #53562, #97770, #55001, #86908, #131122, #44119, #31806, #33277 ),
 .UNSPECIFIED., .F., .F.,
 ( 4, 2, 2, 2, 4 ),
 ( 0.008003515366661703712, 0.008517983447693482785, 0.009032451528725263593, 0.009546919609757044400, 0.01006138769078882347 ),
 .UNSPECIFIED. ) ;
#95684 = ORIENTED_EDGE ( 'NONE', *, *, #89518, .F. ) ;
#95685 = ORIENTED_EDGE ( 'NONE', *, *, #135474, .F. ) ;
#95686 = VERTEX_POINT ( 'NONE', #31058 ) ;
#95687 = CARTESIAN_POINT ( 'NONE',  ( 17.99451991528748351, 28.92564299267950645, 4.000000000000000000 ) ) ;
#95688 = ADVANCED_FACE ( 'NONE', ( #22265 ), #131787, .T. ) ;
#95689 = ORIENTED_EDGE ( 'NONE', *, *, #84623, .F. ) ;
#95690 = VECTOR ( 'NONE', #140991, 1000.000000000000000 ) ;
#95691 = VERTEX_POINT ( 'NONE', #102730 ) ;
#95692 = DIRECTION ( 'NONE',  ( 0.000000000000000000, -1.000000000000000000, 0.000000000000000000 ) ) ;
#95693 = LINE ( 'NONE', #119560, #6368 ) ;
#95694 = LINE ( 'NONE', #71837, #17776 ) ;
#95695 = PLANE ( 'NONE',  #71789 ) ;
#95696 = VERTEX_POINT ( 'NONE', #134658 ) ;
#95697 = CARTESIAN_POINT ( 'NONE',  ( -2.671830600776449405, -9.740707523384187994, 4.000000000000000000 ) ) ;
#95698 = EDGE_CURVE ( 'NONE', #140787, #79481, #72506, .T. ) ;
#95699 = VERTEX_POINT ( 'NONE', #79598 ) ;
#95701 = AXIS2_PLACEMENT_3D ( 'NONE', #19183, #51830, #31493 ) ;
#95700 = CARTESIAN_POINT ( 'NONE',  ( -30.29974487139158867, -27.71228299555227537, 4.000000000000000000 ) ) ;
#95702 = LINE ( 'NONE', #142783, #42752 ) ;
#95703 = VECTOR ( 'NONE', #38150, 1000.000000000000000 ) ;
#95704 = CARTESIAN_POINT ( 'NONE',  ( 13.77540314143521982, -2.126176841940958351, -7.934999999999989839 ) ) ;
#95705 = EDGE_LOOP ( 'NONE', ( #38128, #139303, #115649, #93457 ) ) ;
#95706 = CARTESIAN_POINT ( 'NONE',  ( 90.91209685856478018, 5.291415217122922066, -3.054999999999995275 ) ) ;
#95707 = DIRECTION ( 'NONE',  ( 1.000000000000000000, 0.000000000000000000, 0.000000000000000000 ) ) ;
#95708 = CARTESIAN_POINT ( 'NONE',  ( 8.423184310185783730, -2.500000000000000000, 3.061616997868383634E-16 ) ) ;
#95709 = CARTESIAN_POINT ( 'NONE',  ( -42.18398860626899705, 28.73617430169816700, 5.000000000000000000 ) ) ;
#95710 = ORIENTED_EDGE ( 'NONE', *, *, #81530, .F. ) ;
#95711 = ADVANCED_FACE ( 'NONE', ( #123782 ), #90411, .F. ) ;
#95712 = EDGE_LOOP ( 'NONE', ( #119503, #41114, #46611 ) ) ;
#95713 = CARTESIAN_POINT ( 'NONE',  ( -7.499999999999944045, -14.56887692260766087, 4.000000000000000000 ) ) ;
#95714 = ORIENTED_EDGE ( 'NONE', *, *, #51129, .T. ) ;
#95716 =( GEOMETRIC_REPRESENTATION_CONTEXT ( 3 ) GLOBAL_UNCERTAINTY_ASSIGNED_CONTEXT ( ( #72442 ) ) GLOBAL_UNIT_ASSIGNED_CONTEXT ( ( #34641, #12855, #136082 ) ) REPRESENTATION_CONTEXT ( 'NONE', 'WORKASPACE' ) );
#95715 = DIRECTION ( 'NONE',  ( -0.000000000000000000, 0.000000000000000000, 1.000000000000000000 ) ) ;
#95717 = DIRECTION ( 'NONE',  ( 0.6830127018922181881, 0.6830127018922202975, -0.2588190451025214056 ) ) ;
#95718 = CARTESIAN_POINT ( 'NONE',  ( 0.000000000000000000, 7.931123077392108200, 4.000000000000000000 ) ) ;
#95719 = CARTESIAN_POINT ( 'NONE',  ( 184.0776099992117167, -48.13855614192994636, -37.56434003616361395 ) ) ;
#95721 = EDGE_LOOP ( 'NONE', ( #69291, #18311, #29665, #93791 ) ) ;
#95720 =( BOUNDED_CURVE ( )  B_SPLINE_CURVE ( 3, ( #114391, #15061, #126678, #59339 ),
 .UNSPECIFIED., .F., .F. ) 
 B_SPLINE_CURVE_WITH_KNOTS ( ( 4, 4 ),
 ( 1.901594255663637600, 1.933014472006564954 ),
 .UNSPECIFIED. ) 
 CURVE ( )  GEOMETRIC_REPRESENTATION_ITEM ( )  RATIONAL_B_SPLINE_CURVE ( ( 1.000000000000000000, 0.9999177325257868620, 0.9999177325257868620, 1.000000000000000000 ) ) 
 REPRESENTATION_ITEM ( '' )  );
#95722 = ADVANCED_FACE ( 'NONE', ( #100592 ), #123053, .F. ) ;
#95723 = EDGE_CURVE ( 'NONE', #123801, #126581, #12830, .T. ) ;
#95724 = CARTESIAN_POINT ( 'NONE',  ( 20.36747333860806819, 3.061616997868387579E-16, -2.500000000000000444 ) ) ;
#95725 = FACE_OUTER_BOUND ( 'NONE', #81020, .T. ) ;
#95726 = CARTESIAN_POINT ( 'NONE',  ( -45.18398860626900415, 28.73617430169818832, 5.000000000000000000 ) ) ;
#95727 = ORIENTED_EDGE ( 'NONE', *, *, #27445, .F. ) ;
#95728 = LINE ( 'NONE', #120295, #86014 ) ;
#95729 = VECTOR ( 'NONE', #54728, 1000.000000000000000 ) ;
#95731 = EDGE_CURVE ( 'NONE', #123966, #41451, #1233, .T. ) ;
#95730 = DIRECTION ( 'NONE',  ( -0.7071067811865487940, 0.7071067811865463515, 0.000000000000000000 ) ) ;
#95732 = EDGE_LOOP ( 'NONE', ( #80947, #72107, #135133, #41516 ) ) ;
#95734 = EDGE_LOOP ( 'NONE', ( #24762, #137171, #32709, #88225 ) ) ;
#95733 = CARTESIAN_POINT ( 'NONE',  ( 32.99999999999975842, 17.58746187583907528, 4.000000000000000000 ) ) ;
#95735 = EDGE_CURVE ( 'NONE', #13057, #49717, #114303, .T. ) ;
#95736 = VECTOR ( 'NONE', #125038, 1000.000000000000000 ) ;
#95737 = CARTESIAN_POINT ( 'NONE',  ( 63.18398860626900415, 28.73617430169831621, 5.000000000000000000 ) ) ;
#95738 = PLANE ( 'NONE',  #41463 ) ;
#95739 = ORIENTED_EDGE ( 'NONE', *, *, #19743, .F. ) ;
#95740 = DIRECTION ( 'NONE',  ( -0.6830127018922180770, -0.6830127018922204085, -0.2588190451025213501 ) ) ;
#95741 = LINE ( 'NONE', #118917, #42930 ) ;
#95743 = MECHANICAL_DESIGN_GEOMETRIC_PRESENTATION_REPRESENTATION (  '', ( #14724 ), #93482 ) ;
#95742 = LINE ( 'NONE', #71164, #80813 ) ;
#95744 = EDGE_CURVE ( 'NONE', #63240, #21420, #91156, .T. ) ;
#95745 = LINE ( 'NONE', #40668, #113291 ) ;
#95746 = LINE ( 'NONE', #5132, #268 ) ;
#95747 = FACE_OUTER_BOUND ( 'NONE', #58701, .T. ) ;
#95748 = LINE ( 'NONE', #127685, #84233 ) ;
#95749 = CARTESIAN_POINT ( 'NONE',  ( -18.48921356237309510, -27.52281430457068367, 5.000000000000000000 ) ) ;
#95750 = LINE ( 'NONE', #84878, #14306 ) ;
#95751 = CARTESIAN_POINT ( 'NONE',  ( 29.53752705046289151, -9.735942053221456900E-16, 7.949999999999998401 ) ) ;
#95752 = EDGE_CURVE ( 'NONE', #31597, #75508, #68686, .T. ) ;
#95753 = DIRECTION ( 'NONE',  ( -0.000000000000000000, 0.000000000000000000, 1.000000000000000000 ) ) ;
#95754 = DIRECTION ( 'NONE',  ( 0.7071067811865487940, -0.7071067811865463515, 0.000000000000000000 ) ) ;
#95755 = ORIENTED_EDGE ( 'NONE', *, *, #27646, .T. ) ;
#95756 = VECTOR ( 'NONE', #30225, 1000.000000000000227 ) ;
#95757 = ORIENTED_EDGE ( 'NONE', *, *, #50390, .F. ) ;
#95758 = ORIENTED_EDGE ( 'NONE', *, *, #82878, .T. ) ;
#95759 = CARTESIAN_POINT ( 'NONE',  ( 108.4791666666666714, -7.950000000000001066, 2.130196079827424427 ) ) ;
#95760 = VERTEX_POINT ( 'NONE', #112874 ) ;
#95761 = ORIENTED_EDGE ( 'NONE', *, *, #116712, .F. ) ;
#95762 = ORIENTED_EDGE ( 'NONE', *, *, #70203, .T. ) ;
#95763 = DIRECTION ( 'NONE',  ( -0.7071067811865486830, -0.7071067811865464625, 0.000000000000000000 ) ) ;
#95764 = CARTESIAN_POINT ( 'NONE',  ( 89.22916666666667140, 7.950000000000001954, -2.130196079827421762 ) ) ;
#95765 = ORIENTED_EDGE ( 'NONE', *, *, #137581, .T. ) ;
#95766 = CARTESIAN_POINT ( 'NONE',  ( -34.42500000000001137, 0.000000000000000000, 4.500000000000000888 ) ) ;
#95767 = DIRECTION ( 'NONE',  ( -0.6830127018922181881, 0.6830127018922202975, -0.2588190451025214056 ) ) ;
#95768 = CARTESIAN_POINT ( 'NONE',  ( 5.755190629914537226, -2.055000000000000160, 2.789133085058097101E-16 ) ) ;
#95769 = CARTESIAN_POINT ( 'NONE',  ( 5.292893218813423672, -15.74070752338412049, 5.000000000000000000 ) ) ;
#95770 = CARTESIAN_POINT ( 'NONE',  ( 102.5212635252314328, -4.472830434245839371, -4.472830434245840259 ) ) ;
#95771 = ORIENTED_EDGE ( 'NONE', *, *, #103230, .F. ) ;
#95772 = DIRECTION ( 'NONE',  ( -1.000000000000000000, -1.224606353822377258E-16, -0.000000000000000000 ) ) ;
#95773 = LINE ( 'NONE', #116812, #70162 ) ;
#95774 = LINE ( 'NONE', #129836, #56709 ) ;
#95775 = CARTESIAN_POINT ( 'NONE',  ( 82.03752705046288440, -9.735942053221456900E-16, 7.949999999999998401 ) ) ;
#95776 = VECTOR ( 'NONE', #140759, 1000.000000000000000 ) ;
#95777 = PLANE ( 'NONE',  #139556 ) ;
#95778 = CARTESIAN_POINT ( 'NONE',  ( -75.48921356237309510, -27.52281430457107803, 5.000000000000000000 ) ) ;
#95779 = CARTESIAN_POINT ( 'NONE',  ( 28.66252705046289151, 7.949999999999998401, 1.460391307983218338E-15 ) ) ;
#95780 = PLANE ( 'NONE',  #49055 ) ;
#95781 = EDGE_CURVE ( 'NONE', #119711, #48518, #58561, .T. ) ;
#95783 = DIRECTION ( 'NONE',  ( -0.7071067811865486830, -0.7071067811865464625, -0.000000000000000000 ) ) ;
#95782 = VECTOR ( 'NONE', #21766, 1000.000000000000000 ) ;
#95784 = ORIENTED_EDGE ( 'NONE', *, *, #137776, .F. ) ;
#95785 = ORIENTED_EDGE ( 'NONE', *, *, #44495, .F. ) ;
#95786 = CARTESIAN_POINT ( 'NONE',  ( 31.04166666666666075, -3.975000000000002753, 6.884901960086286188 ) ) ;
#95787 = VERTEX_POINT ( 'NONE', #136056 ) ;
#95788 = DIRECTION ( 'NONE',  ( -0.000000000000000000, -1.000000000000000000, -0.000000000000000000 ) ) ;
#95789 = CARTESIAN_POINT ( 'NONE',  ( 57.29974487139158157, -27.71228299555246011, 4.000000000000000000 ) ) ;
#95790 = DIRECTION ( 'NONE',  ( -1.000000000000000000, -1.224606353822377258E-16, -0.000000000000000000 ) ) ;
#95791 = VECTOR ( 'NONE', #22571, 1000.000000000000000 ) ;
#95792 = DIRECTION ( 'NONE',  ( -0.7071067811865486830, -0.7071067811865464625, -0.000000000000000000 ) ) ;
#95793 = DIRECTION ( 'NONE',  ( -0.7071067811865487940, 0.7071067811865463515, 0.000000000000000000 ) ) ;
#95794 = CARTESIAN_POINT ( 'NONE',  ( 85.53752705046288440, -9.735942053221456900E-16, 7.949999999999998401 ) ) ;
#95795 = CARTESIAN_POINT ( 'NONE',  ( 127.8079301918981230, -6.109999999999998543, 1.637169565754158063 ) ) ;
#95796 = VECTOR ( 'NONE', #36361, 1000.000000000000000 ) ;
#95797 = ORIENTED_EDGE ( 'NONE', *, *, #9807, .T. ) ;
#95798 = AXIS2_PLACEMENT_3D ( 'NONE', #19824, #32893, #44487 ) ;
#95799 = CARTESIAN_POINT ( 'NONE',  ( 27.99999999999999645, 9.521314400968980422E-16, 0.000000000000000000 ) ) ;
#95800 = ORIENTED_EDGE ( 'NONE', *, *, #63667, .T. ) ;
#95801 = DIRECTION ( 'NONE',  ( 0.3543493200069162685, -0.000000000000000000, -0.9351131265310288487 ) ) ;
#95802 =( LENGTH_UNIT ( ) NAMED_UNIT ( * ) SI_UNIT ( .MILLI., .METRE. ) );
#95803 = AXIS2_PLACEMENT_3D ( 'NONE', #128300, #5761, #7178 ) ;
#95804 = DIRECTION ( 'NONE',  ( -0.6830127018922181881, 0.6830127018922202975, -0.2588190451025214056 ) ) ;
#95805 = ORIENTED_EDGE ( 'NONE', *, *, #89615, .T. ) ;
#95806 = CARTESIAN_POINT ( 'NONE',  ( 48.56293019189809712, 1.637169565754157174, 6.110000000000002984 ) ) ;
#95807 = ORIENTED_EDGE ( 'NONE', *, *, #80021, .T. ) ;
#95808 = DIRECTION ( 'NONE',  ( -0.7071067811865486830, -0.7071067811865464625, -0.000000000000000000 ) ) ;
#95809 = CARTESIAN_POINT ( 'NONE',  ( 27.48921356237309155, -27.52281430457074762, 5.000000000000000000 ) ) ;
#95810 = FACE_OUTER_BOUND ( 'NONE', #129307, .T. ) ;
#95811 = DIRECTION ( 'NONE',  ( 0.7071067811865487940, 0.7071067811865463515, -0.000000000000000000 ) ) ;
#95812 = AXIS2_PLACEMENT_3D ( 'NONE', #83092, #49777, #49049 ) ;
#95813 = AXIS2_PLACEMENT_3D ( 'NONE', #24188, #101014, #1667 ) ;
#95814 = VECTOR ( 'NONE', #110818, 1000.000000000000227 ) ;
#95815 = CARTESIAN_POINT ( 'NONE',  ( 34.91209685856478018, 5.291415217122921177, -3.054999999999994831 ) ) ;
#95816 = ORIENTED_EDGE ( 'NONE', *, *, #108294, .T. ) ;
#95817 = LINE ( 'NONE', #140065, #24702 ) ;
#95818 = ORIENTED_EDGE ( 'NONE', *, *, #56575, .T. ) ;
#95819 = EDGE_LOOP ( 'NONE', ( #126405, #133027, #68735, #16907 ) ) ;
#95820 = AXIS2_PLACEMENT_3D ( 'NONE', #116445, #114291, #14965 ) ;
#95821 = ORIENTED_EDGE ( 'NONE', *, *, #53395, .T. ) ;
#95822 = CARTESIAN_POINT ( 'NONE',  ( 59.28752705046289151, 0.000000000000000000, -7.949999999999998401 ) ) ;
#95823 = ORIENTED_EDGE ( 'NONE', *, *, #5703, .F. ) ;
#95824 = EDGE_CURVE ( 'NONE', #85885, #106040, #122301, .T. ) ;
#95825 = EDGE_CURVE ( 'NONE', #41816, #36553, #13537, .T. ) ;
#95826 = PLANE ( 'NONE',  #61845 ) ;
#95827 = AXIS2_PLACEMENT_3D ( 'NONE', #65985, #22411, #11528 ) ;
#95828 = DIRECTION ( 'NONE',  ( -0.000000000000000000, 0.000000000000000000, 1.000000000000000000 ) ) ;
#95829 = EDGE_CURVE ( 'NONE', #16704, #64740, #12123, .T. ) ;
#95830 = FACE_BOUND ( 'NONE', #85765, .T. ) ;
#95831 = DIRECTION ( 'NONE',  ( 0.7071067811865487940, 0.7071067811865463515, 0.000000000000000000 ) ) ;
#95832 = EDGE_CURVE ( 'NONE', #78861, #44190, #39337, .T. ) ;
#95833 = EDGE_CURVE ( 'NONE', #9322, #73005, #33908, .T. ) ;
#95834 = DIRECTION ( 'NONE',  ( -0.000000000000000000, -1.000000000000000000, -0.000000000000000000 ) ) ;
#95835 = CARTESIAN_POINT ( 'NONE',  ( -19.17183060077633172, 15.75929247661555976, 4.000000000000000000 ) ) ;
#95836 = EDGE_LOOP ( 'NONE', ( #142875, #101400, #70733, #20746 ) ) ;
#95837 = DIRECTION ( 'NONE',  ( -0.5735764363510499342, -0.8191520442889891340, 0.000000000000000000 ) ) ;
#95838 = ORIENTED_EDGE ( 'NONE', *, *, #14467, .T. ) ;
#95839 = ORIENTED_EDGE ( 'NONE', *, *, #53298, .F. ) ;
#95840 = DIRECTION ( 'NONE',  ( 0.3543493200069162685, -0.000000000000000000, -0.9351131265310288487 ) ) ;
#95841 = ORIENTED_EDGE ( 'NONE', *, *, #15957, .T. ) ;
#95842 = ADVANCED_FACE ( 'NONE', ( #17142 ), #72992, .F. ) ;
#95843 = EDGE_CURVE ( 'NONE', #77610, #44308, #15660, .T. ) ;
#95844 = CARTESIAN_POINT ( 'NONE',  ( 56.20376352523144448, 6.109999999999998543, 1.122388791418548911E-15 ) ) ;
#95846 = ORIENTED_EDGE ( 'NONE', *, *, #74222, .F. ) ;
#95845 = VECTOR ( 'NONE', #99238, 1000.000000000000000 ) ;
#95847 = CARTESIAN_POINT ( 'NONE',  ( -17.81601139373099940, 28.73617430169775133, 5.000000000000000000 ) ) ;
#95848 = PLANE ( 'NONE',  #14828 ) ;
#95849 = ADVANCED_FACE ( 'NONE', ( #71535 ), #105550, .F. ) ;
#95850 = ORIENTED_EDGE ( 'NONE', *, *, #96843, .T. ) ;
#95851 = CARTESIAN_POINT ( 'NONE',  ( -34.92500000000001137, -22.22500000000000142, 4.500000000000000888 ) ) ;
#95852 = MECHANICAL_DESIGN_GEOMETRIC_PRESENTATION_REPRESENTATION (  '', ( #72841 ), #58879 ) ;
#95853 = EDGE_CURVE ( 'NONE', #17670, #136430, #17822, .T. ) ;
#95854 = LINE ( 'NONE', #42217, #34002 ) ;
#95855 = DIRECTION ( 'NONE',  ( -0.6830127018922180770, -0.6830127018922204085, -0.2588190451025213501 ) ) ;
#95856 = LINE ( 'NONE', #40783, #20337 ) ;
#95857 = DIRECTION ( 'NONE',  ( -0.3543493200069162685, -0.000000000000000000, -0.9351131265310288487 ) ) ;
#95858 = SURFACE_SIDE_STYLE ('',( #48808 ) ) ;
#95859 = ORIENTED_EDGE ( 'NONE', *, *, #112509, .F. ) ;
#95860 = VERTEX_POINT ( 'NONE', #62095 ) ;
#95861 = CARTESIAN_POINT ( 'NONE',  ( 31.49999999999977973, -1.533600742197722910, 5.000000000000000000 ) ) ;
#95862 = FACE_OUTER_BOUND ( 'NONE', #87816, .T. ) ;
#95863 = ORIENTED_EDGE ( 'NONE', *, *, #20260, .F. ) ;
#95864 = ORIENTED_EDGE ( 'NONE', *, *, #125081, .F. ) ;
#95865 = VERTEX_POINT ( 'NONE', #125915 ) ;
#95866 = FACE_OUTER_BOUND ( 'NONE', #12454, .T. ) ;
#95867 = LINE ( 'NONE', #120436, #69305 ) ;
#95868 = ORIENTED_EDGE ( 'NONE', *, *, #131598, .F. ) ;
#95869 = LINE ( 'NONE', #18281, #97250 ) ;
#95871 = ADVANCED_FACE ( 'NONE', ( #59949 ), #38894, .F. ) ;
#95870 = CONICAL_SURFACE ( 'NONE', #107459, 2.500000000000000444, 0.9599310885968830309 ) ;
#95872 = PLANE ( 'NONE',  #84009 ) ;
#95873 = VECTOR ( 'NONE', #96617, 1000.000000000000000 ) ;
#95874 = CARTESIAN_POINT ( 'NONE',  ( 14.50456980810188767, 6.871911579029510442, -3.967499999999998916 ) ) ;
#95875 = LINE ( 'NONE', #78252, #119022 ) ;
#95876 = VERTEX_POINT ( 'NONE', #128066 ) ;
#95877 = CARTESIAN_POINT ( 'NONE',  ( 121.2454301918981230, -5.291415217122919401, -3.055000000000000604 ) ) ;
#95878 =( BOUNDED_CURVE ( )  B_SPLINE_CURVE ( 2, ( #140722, #98651, #41417, #30565, #19667, #142878, #87784, #74803, #118979, #97189, #33445, #42164, #132016 ),
 .UNSPECIFIED., .F., .T. ) 
 B_SPLINE_CURVE_WITH_KNOTS ( ( 3, 2, 2, 2, 2, 2, 3 ),
 ( 0.5500000000000000444, 0.5527777777777778123, 0.5555555555555555802, 0.5583333333333333481, 0.5611111111111111160, 0.5638888888888888840, 0.5666666666666666519 ),
 .UNSPECIFIED. ) 
 CURVE ( )  GEOMETRIC_REPRESENTATION_ITEM ( )  RATIONAL_B_SPLINE_CURVE ( ( 1.000000000000000000, 0.9659258262890683122, 1.000000000000000000, 0.9659258262890683122, 1.000000000000000000, 0.9659258262890683122, 1.000000000000000000, 0.9659258262890683122, 1.000000000000000000, 0.9659258262890683122, 1.000000000000000000, 0.9659258262890683122, 1.000000000000000000 ) ) 
 REPRESENTATION_ITEM ( '' )  );
#95879 = PLANE ( 'NONE',  #37323 ) ;
#95880 = ADVANCED_FACE ( 'NONE', ( #104111 ), #4774, .F. ) ;
#95881 = CARTESIAN_POINT ( 'NONE',  ( -34.92500000000001137, -6.048682586364289904, 15.71395525773009538 ) ) ;
#95883 = ORIENTED_EDGE ( 'NONE', *, *, #126778, .T. ) ;
#95882 = DIRECTION ( 'NONE',  ( -0.7071067811865486830, -0.7071067811865464625, 0.000000000000000000 ) ) ;
#95884 = DIRECTION ( 'NONE',  ( 0.6830127018922181881, 0.6830127018922202975, -0.2588190451025214056 ) ) ;
#95885 = ORIENTED_EDGE ( 'NONE', *, *, #12263, .F. ) ;
#95886 = DIRECTION ( 'NONE',  ( 0.7071067811865487940, 0.7071067811865463515, -0.000000000000000000 ) ) ;
#95887 = DIRECTION ( 'NONE',  ( 1.000000000000000000, 0.000000000000000000, 0.000000000000000000 ) ) ;
#95888 = LINE ( 'NONE', #42967, #142185 ) ;
#95889 = VERTEX_POINT ( 'NONE', #51209 ) ;
#95890 = EDGE_CURVE ( 'NONE', #72919, #117423, #134002, .T. ) ;
#95891 = VECTOR ( 'NONE', #129587, 999.9999999999998863 ) ;
#95892 = AXIS2_PLACEMENT_3D ( 'NONE', #5903, #72684, #61097 ) ;
#95893 = EDGE_CURVE ( 'NONE', #36504, #74632, #39634, .T. ) ;
#95894 = CARTESIAN_POINT ( 'NONE',  ( -9.005480084712511157, 28.92564299267931816, 4.000000000000000000 ) ) ;
#95895 = LINE ( 'NONE', #141558, #134497 ) ;
#95896 = CARTESIAN_POINT ( 'NONE',  ( -19.28515664589289003, 1.196650378695325090, -30.59010235425025215 ) ) ;
#95897 = ORIENTED_EDGE ( 'NONE', *, *, #112526, .F. ) ;
#95898 = LINE ( 'NONE', #4542, #4453 ) ;
#95899 = CARTESIAN_POINT ( 'NONE',  ( 2.613322195557305161, 2.055000000000001048, 2.516649172247811554E-16 ) ) ;
#95901 = ADVANCED_FACE ( 'NONE', ( #84558 ), #128750, .F. ) ;
#95900 = CARTESIAN_POINT ( 'NONE',  ( 12.19999999999999574, -40.29840020119763011, 19.55137198191483350 ) ) ;
#95902 = CARTESIAN_POINT ( 'NONE',  ( 42.48921356237308800, -27.52281430457085065, 5.000000000000000000 ) ) ;
#95903 = CARTESIAN_POINT ( 'NONE',  ( -13.49999999999990763, 3.073033219394612825, -6.593910359670999810 ) ) ;
#95904 = VECTOR ( 'NONE', #73438, 1000.000000000000000 ) ;
#95905 = VERTEX_POINT ( 'NONE', #49076 ) ;
#95906 = EDGE_LOOP ( 'NONE', ( #104147, #6129, #74532, #45310 ) ) ;
#95907 = LINE ( 'NONE', #74908, #100475 ) ;
#95908 = CARTESIAN_POINT ( 'NONE',  ( 0.3281693992235254487, -3.740707523384248390, 4.000000000000000000 ) ) ;
#95909 = EDGE_CURVE ( 'NONE', #138815, #16132, #48340, .T. ) ;
#95910 = VECTOR ( 'NONE', #18848, 1000.000000000000000 ) ;
#95911 = CARTESIAN_POINT ( 'NONE',  ( 16.16623647476855652, 7.934999999999990727, -1.457635852685135314E-15 ) ) ;
#95912 = LINE ( 'NONE', #29225, #15771 ) ;
#95913 = STYLED_ITEM ( 'NONE', ( #90173 ), #44362 ) ;
#95914 = DIRECTION ( 'NONE',  ( 0.7071067811865486830, -0.7071067811865464625, -0.000000000000000000 ) ) ;
#95915 = PLANE ( 'NONE',  #141720 ) ;
#95916 = EDGE_LOOP ( 'NONE', ( #63043, #22037, #112403, #77032, #136280, #60801 ) ) ;
#95917 = ADVANCED_FACE ( 'NONE', ( #119982 ), #86699, .F. ) ;
#95918 = CARTESIAN_POINT ( 'NONE',  ( 34.49999999999975842, -6.839392718269096783, -8.480912228396162433 ) ) ;
#95919 = DIRECTION ( 'NONE',  ( -0.7071067811865486830, -0.7071067811865464625, 0.000000000000000000 ) ) ;
#95920 = PLANE ( 'NONE',  #28538 ) ;
#95921 = DIRECTION ( 'NONE',  ( 0.7071067811865487940, 0.7071067811865463515, 0.000000000000000000 ) ) ;
#95922 = CARTESIAN_POINT ( 'NONE',  ( 36.37043019189811588, -3.055000000000001936, 5.291415217122918513 ) ) ;
#95923 = CARTESIAN_POINT ( 'NONE',  ( -13.49999999999990763, 9.431123077392092213, 4.000000000000000000 ) ) ;
#95924 = AXIS2_PLACEMENT_3D ( 'NONE', #101742, #45963, #256 ) ;
#95925 = EDGE_LOOP ( 'NONE', ( #47001, #99588, #136638, #117693, #46819, #113168 ) ) ;
#95926 = CARTESIAN_POINT ( 'NONE',  ( 61.46640106136307935, -1.600000000000094458, 34.92499999999998295 ) ) ;
#95927 = ORIENTED_EDGE ( 'NONE', *, *, #111968, .F. ) ;
#95928 = ORIENTED_EDGE ( 'NONE', *, *, #22503, .F. ) ;
#95929 = DIRECTION ( 'NONE',  ( 0.3543493200069162685, -0.000000000000000000, -0.9351131265310288487 ) ) ;
#95930 = B_SPLINE_CURVE_WITH_KNOTS ( 'NONE', 3,
 ( #128802, #48392, #54147, #54839, #33116, #42548, #129505, #75178, #87461, #131678, #141854, #20751 ),
 .UNSPECIFIED., .F., .F.,
 ( 4, 2, 2, 2, 2, 4 ),
 ( 0.000000000000000000, 0.001108890051515397813, 0.001663335077273096719, 0.002217780103030795626, 0.003326670154546186500, 0.004435560206061577374 ),
 .UNSPECIFIED. ) ;
#95931 = DIRECTION ( 'NONE',  ( -1.000000000000000000, -1.224606353822377258E-16, -0.000000000000000000 ) ) ;
#95932 = FACE_OUTER_BOUND ( 'NONE', #82759, .T. ) ;
#95933 = FACE_OUTER_BOUND ( 'NONE', #112177, .T. ) ;
#95934 = DIRECTION ( 'NONE',  ( 0.6830127018922180770, -0.6830127018922204085, -0.2588190451025213501 ) ) ;
#95935 = EDGE_CURVE ( 'NONE', #127624, #73159, #21430, .T. ) ;
#95936 = FACE_OUTER_BOUND ( 'NONE', #82911, .T. ) ;
#95937 = DIRECTION ( 'NONE',  ( 0.7071067811865487940, 0.7071067811865463515, 0.000000000000000000 ) ) ;
#95938 = EDGE_LOOP ( 'NONE', ( #102493, #68032, #47788, #136151 ) ) ;
#95939 = EDGE_CURVE ( 'NONE', #61026, #15122, #19976, .T. ) ;
#95940 = CARTESIAN_POINT ( 'NONE',  ( -16.25154412867565412, -11.24070752338416845, 10.39518518046013007 ) ) ;
#95941 = DIRECTION ( 'NONE',  ( 0.000000000000000000, -1.000000000000000000, 0.000000000000000000 ) ) ;
#95942 = CARTESIAN_POINT ( 'NONE',  ( 8.999999999999937828, -8.731860332648835765, -2.120594902707516383 ) ) ;
#95943 = CARTESIAN_POINT ( 'NONE',  ( 8.999999999999934275, -16.60178936734447674, 0.8616154019347707083 ) ) ;
#95944 = DIRECTION ( 'NONE',  ( -0.6830127018922181881, 0.6830127018922202975, -0.2588190451025214056 ) ) ;
#95945 = PLANE ( 'NONE',  #119758 ) ;
#95946 = CARTESIAN_POINT ( 'NONE',  ( 69.93336038379619879, 2.130196079827431532, -7.949999999999997513 ) ) ;
#95947 = DIRECTION ( 'NONE',  ( -0.7071067811865486830, -0.7071067811865464625, 0.000000000000000000 ) ) ;
#95948 = ORIENTED_EDGE ( 'NONE', *, *, #132588, .T. ) ;
#95949 = ORIENTED_EDGE ( 'NONE', *, *, #107981, .F. ) ;
#95950 = CARTESIAN_POINT ( 'NONE',  ( 52.47916666666665719, -7.950000000000001066, 2.130196079827424427 ) ) ;
#95951 = DIRECTION ( 'NONE',  ( 0.7071067811865486830, -0.7071067811865464625, -0.000000000000000000 ) ) ;
#95952 = CARTESIAN_POINT ( 'NONE',  ( 45.18398860626900415, 28.73617430169818832, 5.000000000000000000 ) ) ;
#95953 = VERTEX_POINT ( 'NONE', #74396 ) ;
#95955 = EDGE_CURVE ( 'NONE', #55993, #21453, #41033, .T. ) ;
#95954 = CIRCLE ( 'NONE', #133044, 34.93000000000001393 ) ;
#95956 = EDGE_CURVE ( 'NONE', #78104, #7710, #97543, .T. ) ;
#95957 = CARTESIAN_POINT ( 'NONE',  ( 50.31293019189810423, -1.637169565754159617, -6.110000000000001208 ) ) ;
#95958 = VERTEX_POINT ( 'NONE', #109137 ) ;
#95959 = FACE_OUTER_BOUND ( 'NONE', #116453, .T. ) ;
#95960 = ORIENTED_EDGE ( 'NONE', *, *, #15363, .F. ) ;
#95961 = EDGE_LOOP ( 'NONE', ( #4493, #75211, #115765, #18888 ) ) ;
#95962 = CARTESIAN_POINT ( 'NONE',  ( 2.000000000000000000, 2.375000000000000000, 0.000000000000000000 ) ) ;
#95963 = LINE ( 'NONE', #74230, #134613 ) ;
#95964 = ORIENTED_EDGE ( 'NONE', *, *, #42239, .T. ) ;
#95965 = EDGE_CURVE ( 'NONE', #101509, #16508, #41751, .T. ) ;
#95966 = DIRECTION ( 'NONE',  ( -0.3543493200069162685, -0.000000000000000000, -0.9351131265310288487 ) ) ;
#95968 = VERTEX_POINT ( 'NONE', #19282 ) ;
#95967 = CARTESIAN_POINT ( 'NONE',  ( -5.999999999999956479, -8.151047557385073361, -8.977947279169784522 ) ) ;
#95969 = CARTESIAN_POINT ( 'NONE',  ( -14.99999999999988098, 17.58746187583906462, 4.000000000000000000 ) ) ;
#95970 = DIRECTION ( 'NONE',  ( -0.7071067811865487940, 0.7071067811865463515, -0.000000000000000000 ) ) ;
#95971 = LINE ( 'NONE', #51788, #5473 ) ;
#95972 = VECTOR ( 'NONE', #72749, 1000.000000000000000 ) ;
#95973 = CARTESIAN_POINT ( 'NONE',  ( 5.999999999999955591, -21.03360074219752462, 5.000000000000000000 ) ) ;
#95974 = ORIENTED_EDGE ( 'NONE', *, *, #13155, .T. ) ;
#95975 = AXIS2_PLACEMENT_3D ( 'NONE', #63011, #141238, #138403 ) ;
#95976 = ORIENTED_EDGE ( 'NONE', *, *, #57602, .T. ) ;
#95977 = FACE_OUTER_BOUND ( 'NONE', #102255, .T. ) ;
#95978 = CARTESIAN_POINT ( 'NONE',  ( 78.07876352523145158, -7.482591942790325086E-16, 6.109999999999998543 ) ) ;
#95979 = CIRCLE ( 'NONE', #133075, 5.968999999999998529 ) ;
#95980 = DIRECTION ( 'NONE',  ( -1.000000000000000000, -0.000000000000000000, -0.000000000000000000 ) ) ;
#95981 = DIRECTION ( 'NONE',  ( 0.3543493200069162685, -0.000000000000000000, -0.9351131265310288487 ) ) ;
#95982 = DIRECTION ( 'NONE',  ( 0.000000000000000000, -1.000000000000000000, 0.000000000000000000 ) ) ;
#95983 = VERTEX_POINT ( 'NONE', #140345 ) ;
#95984 = VERTEX_POINT ( 'NONE', #30892 ) ;
#95985 = PLANE ( 'NONE',  #30652 ) ;
#95986 = DIRECTION ( 'NONE',  ( -1.000000000000000000, 0.000000000000000000, 0.000000000000000000 ) ) ;
#95987 = ORIENTED_EDGE ( 'NONE', *, *, #793, .T. ) ;
#95988 = ORIENTED_EDGE ( 'NONE', *, *, #91498, .F. ) ;
#95989 = EDGE_CURVE ( 'NONE', #74817, #138852, #118584, .T. ) ;
#95990 = LINE ( 'NONE', #138814, #18908 ) ;
#95991 = ORIENTED_EDGE ( 'NONE', *, *, #111780, .F. ) ;
#95992 = LINE ( 'NONE', #140236, #48021 ) ;
#95993 = EDGE_CURVE ( 'NONE', #58586, #72242, #142738, .T. ) ;
#95994 = CARTESIAN_POINT ( 'NONE',  ( 19.88840764549667384, -3.851859888774471706E-31, 2.500000000000001332 ) ) ;
#95995 = FACE_BOUND ( 'NONE', #75497, .T. ) ;
#95996 = FACE_OUTER_BOUND ( 'NONE', #33479, .T. ) ;
#95997 = EDGE_CURVE ( 'NONE', #127570, #9887, #9823, .T. ) ;
#95998 = CARTESIAN_POINT ( 'NONE',  ( -18.48921356237309510, -27.52281430457068367, 5.000000000000000000 ) ) ;
#95999 = DIRECTION ( 'NONE',  ( -0.000000000000000000, -0.3543493200069152693, 0.9351131265310292928 ) ) ;
#96001 = EDGE_LOOP ( 'NONE', ( #29724, #102804, #26535, #60985 ) ) ;
#96000 = DIRECTION ( 'NONE',  ( -0.000000000000000000, 0.3543493200069153248, 0.9351131265310292928 ) ) ;
#96002 = DIRECTION ( 'NONE',  ( -0.7071067811865486830, -0.7071067811865464625, 0.000000000000000000 ) ) ;
#96003 = VECTOR ( 'NONE', #48906, 1000.000000000000000 ) ;
#96004 = ORIENTED_EDGE ( 'NONE', *, *, #34298, .F. ) ;
#96005 = EDGE_CURVE ( 'NONE', #63804, #65772, #75122, .T. ) ;
#96006 = EDGE_CURVE ( 'NONE', #3259, #89141, #8929, .T. ) ;
#96007 = AXIS2_PLACEMENT_3D ( 'NONE', #78192, #111514, #12194 ) ;
#96009 = ORIENTED_EDGE ( 'NONE', *, *, #140825, .T. ) ;
#96008 = COLOUR_RGB ( '', 0.72549020, 0.75294118, 0.79215686) ;
#96010 = CARTESIAN_POINT ( 'NONE',  ( 84.20376352523145158, 6.109999999999998543, 1.122388791418548911E-15 ) ) ;
#96011 = EDGE_LOOP ( 'NONE', ( #75704, #61003, #13262, #90275, #12529, #30260, #65386, #42866, #71835 ) ) ;
#96012 = EDGE_CURVE ( 'NONE', #20530, #50020, #107704, .T. ) ;
#96013 = CIRCLE ( 'NONE', #114534, 2.500000000000000888 ) ;
#96014 = DIRECTION ( 'NONE',  ( -0.6830127018922180770, -0.6830127018922204085, -0.2588190451025213501 ) ) ;
#96015 = EDGE_CURVE ( 'NONE', #94037, #108205, #54095, .T. ) ;
#96016 = DIRECTION ( 'NONE',  ( 1.000000000000000000, 0.000000000000000000, 0.000000000000000000 ) ) ;
#96017 = EDGE_CURVE ( 'NONE', #14271, #10755, #31596, .T. ) ;
#96018 = CARTESIAN_POINT ( 'NONE',  ( 0.000000000000000000, 0.000000000000000000, 5.000000000000000000 ) ) ;
#96019 = FACE_OUTER_BOUND ( 'NONE', #7295, .T. ) ;
#96020 = EDGE_CURVE ( 'NONE', #63701, #9606, #77269, .T. ) ;
#96021 = PLANE ( 'NONE',  #10673 ) ;
#96022 = CARTESIAN_POINT ( 'NONE',  ( 30.99507522778786850, -5.240707523384228850, 12.38332538355488843 ) ) ;
#96023 = DIRECTION ( 'NONE',  ( 0.7071067811865487940, 0.7071067811865463515, 0.000000000000000000 ) ) ;
#96024 = CARTESIAN_POINT ( 'NONE',  ( -27.70612307739176572, 22.22500000000000142, 4.000000000000000000 ) ) ;
#96025 = DIRECTION ( 'NONE',  ( 0.7071067811865487940, -0.7071067811865463515, 0.000000000000000000 ) ) ;
#96026 = VERTEX_POINT ( 'NONE', #87406 ) ;
#96027 = DIRECTION ( 'NONE',  ( 0.7071067811865486830, -0.7071067811865464625, -0.000000000000000000 ) ) ;
#96028 = CARTESIAN_POINT ( 'NONE',  ( 28.49999999999981171, -1.912538124160733766, 4.000000000000000000 ) ) ;
#96029 = EDGE_CURVE ( 'NONE', #31980, #49135, #85236, .T. ) ;
#96030 = ORIENTED_EDGE ( 'NONE', *, *, #124732, .F. ) ;
#96031 = EDGE_LOOP ( 'NONE', ( #95846, #58479, #36852, #8138 ) ) ;
#96032 = ADVANCED_FACE ( 'NONE', ( #51928 ), #129459, .F. ) ;
#96033 = VERTEX_POINT ( 'NONE', #130925 ) ;
#96034 = CARTESIAN_POINT ( 'NONE',  ( 32.22959685856477563, -6.110000000000000320, -1.637169565754161393 ) ) ;
#96035 = ORIENTED_EDGE ( 'NONE', *, *, #101062, .F. ) ;
#96036 = CARTESIAN_POINT ( 'NONE',  ( -24.70710678118636494, -9.740707523384187994, 5.000000000000000000 ) ) ;
#96037 = EDGE_CURVE ( 'NONE', #114295, #28826, #122141, .T. ) ;
#96038 = CARTESIAN_POINT ( 'NONE',  ( 16.08747294953710849, -6.094999999999989981, 3.732111120401553285E-16 ) ) ;
#96039 = CARTESIAN_POINT ( 'NONE',  ( -3.697064227771988509, 12.20036213366778099, -27.08507981779950313 ) ) ;
#96040 = ORIENTED_EDGE ( 'NONE', *, *, #91288, .F. ) ;
#96041 = CARTESIAN_POINT ( 'NONE',  ( -0.7928932188134442116, -2.240707523384266153, 5.000000000000000000 ) ) ;
#96042 = ORIENTED_EDGE ( 'NONE', *, *, #78847, .T. ) ;
#96043 = DIRECTION ( 'NONE',  ( 0.000000000000000000, 1.000000000000000000, 0.000000000000000000 ) ) ;
#96044 = DIRECTION ( 'NONE',  ( 0.000000000000000000, 0.000000000000000000, -1.000000000000000000 ) ) ;
#96046 = ORIENTED_EDGE ( 'NONE', *, *, #128705, .F. ) ;
#96045 = DIRECTION ( 'NONE',  ( 0.000000000000000000, -0.000000000000000000, 1.000000000000000000 ) ) ;
#96047 = VERTEX_POINT ( 'NONE', #22806 ) ;
#96048 = FACE_OUTER_BOUND ( 'NONE', #111745, .T. ) ;
#96049 = ORIENTED_EDGE ( 'NONE', *, *, #38930, .T. ) ;
#96050 = PLANE ( 'NONE',  #18029 ) ;
#96051 = EDGE_LOOP ( 'NONE', ( #107274, #94262, #107814, #10958 ) ) ;
#96052 = EDGE_LOOP ( 'NONE', ( #81787, #13404, #125739, #82438 ) ) ;
#96053 = ORIENTED_EDGE ( 'NONE', *, *, #104905, .F. ) ;
#96054 = EDGE_CURVE ( 'NONE', #49766, #30783, #115424, .T. ) ;
#96055 = DIRECTION ( 'NONE',  ( -1.504632769052527134E-30, -3.469446951953615372E-15, -1.000000000000000000 ) ) ;
#96056 = DIRECTION ( 'NONE',  ( 1.000000000000000000, 0.000000000000000000, 0.000000000000000000 ) ) ;
#96057 = LINE ( 'NONE', #30844, #123209 ) ;
#96058 = CARTESIAN_POINT ( 'NONE',  ( -21.29974487139158512, -27.71228299555221142, 4.000000000000000000 ) ) ;
#96059 = CARTESIAN_POINT ( 'NONE',  ( 27.68840764549667455, 9.139736423841732040E-16, 0.000000000000000000 ) ) ;
#96060 = VERTEX_POINT ( 'NONE', #88845 ) ;
#96061 = CARTESIAN_POINT ( 'NONE',  ( 34.49999999999976552, 0.4497235411627803492, -5.599840258123462533 ) ) ;
#96062 = ORIENTED_EDGE ( 'NONE', *, *, #130400, .T. ) ;
#96063 = LINE ( 'NONE', #39584, #116518 ) ;
#96064 = ADVANCED_FACE ( 'NONE', ( #100423 ), #78665, .T. ) ;
#96065 = CIRCLE ( 'NONE', #45219, 2.500000000000000888 ) ;
#96066 = CARTESIAN_POINT ( 'NONE',  ( 29.29123647476855652, -9.717572351234235426E-16, -7.934999999999990727 ) ) ;
#96067 = CARTESIAN_POINT ( 'NONE',  ( 0.000000000000000000, 21.72500000000000142, 4.500000000000000888 ) ) ;
#96068 = EDGE_LOOP ( 'NONE', ( #129387, #115092, #28943, #64091 ) ) ;
#96069 = CARTESIAN_POINT ( 'NONE',  ( 36.66846741159834266, -18.74070752338409562, 20.73178291233849890 ) ) ;
#96070 =( LENGTH_UNIT ( ) NAMED_UNIT ( * ) SI_UNIT ( .MILLI., .METRE. ) );
#96071 = VERTEX_POINT ( 'NONE', #112018 ) ;
#96072 = STYLED_ITEM ( 'NONE', ( #131807 ), #90366 ) ;
#96073 = ORIENTED_EDGE ( 'NONE', *, *, #10366, .F. ) ;
#96074 = EDGE_CURVE ( 'NONE', #40937, #11091, #113410, .T. ) ;
#96075 = ORIENTED_EDGE ( 'NONE', *, *, #138957, .T. ) ;
#96076 = PLANE ( 'NONE',  #39447 ) ;
#96077 = DIRECTION ( 'NONE',  ( -0.000000000000000000, 0.000000000000000000, 1.000000000000000000 ) ) ;
#96078 = LINE ( 'NONE', #134452, #23777 ) ;
#96079 = CARTESIAN_POINT ( 'NONE',  ( 8.897059064271770623, 4.202752102959690472E-16, 0.000000000000000000 ) ) ;
#96080 = CARTESIAN_POINT ( 'NONE',  ( 3.596992905804716756, -49.14999999999999147, -40.56450646617317801 ) ) ;
#96081 = CARTESIAN_POINT ( 'NONE',  ( 71.80793019189812298, -6.109999999999999432, 1.637169565754158507 ) ) ;
#96082 = LINE ( 'NONE', #140321, #120500 ) ;
#96083 = DIRECTION ( 'NONE',  ( 0.7071067811865486830, -0.7071067811865464625, -0.000000000000000000 ) ) ;
#96084 = VECTOR ( 'NONE', #137674, 1000.000000000000227 ) ;
#96085 = LINE ( 'NONE', #129433, #7097 ) ;
#96086 = EDGE_CURVE ( 'NONE', #138835, #131561, #133071, .T. ) ;
#96087 = CARTESIAN_POINT ( 'NONE',  ( 66.18398860626901126, 28.73617430169833753, 5.000000000000000000 ) ) ;
#96088 = AXIS2_PLACEMENT_3D ( 'NONE', #95078, #127740, #129142 ) ;
#96089 = ORIENTED_EDGE ( 'NONE', *, *, #47458, .T. ) ;
#96090 = FACE_OUTER_BOUND ( 'NONE', #118386, .T. ) ;
#96091 = EDGE_LOOP ( 'NONE', ( #58507, #102434, #76693, #119429 ) ) ;
#96092 = DIRECTION ( 'NONE',  ( 0.3543493200069162685, -0.000000000000000000, -0.9351131265310288487 ) ) ;
#96093 = DIRECTION ( 'NONE',  ( 1.000000000000000000, 0.000000000000000000, 0.000000000000000000 ) ) ;
#96094 = ORIENTED_EDGE ( 'NONE', *, *, #18257, .F. ) ;
#96095 = DIRECTION ( 'NONE',  ( -0.7071067811865487940, 0.7071067811865463515, 0.000000000000000000 ) ) ;
#96097 = ORIENTED_EDGE ( 'NONE', *, *, #64994, .T. ) ;
#96096 = DIRECTION ( 'NONE',  ( 1.000000000000000000, 1.224606353822377258E-16, 0.000000000000000000 ) ) ;
#96098 = EDGE_CURVE ( 'NONE', #134905, #65308, #64563, .T. ) ;
#96099 = CARTESIAN_POINT ( 'NONE',  ( 24.39999999999999858, -5.520864266206504263E-14, 0.000000000000000000 ) ) ;
#96100 = EDGE_LOOP ( 'NONE', ( #108864, #10579, #15719, #40871 ) ) ;
#96101 = ORIENTED_EDGE ( 'NONE', *, *, #121567, .T. ) ;
#96102 = DIRECTION ( 'NONE',  ( 0.7071067811865487940, 0.7071067811865463515, -0.000000000000000000 ) ) ;
#96103 = DIRECTION ( 'NONE',  ( -0.7071067811865487940, 0.7071067811865463515, 0.000000000000000000 ) ) ;
#96104 = CARTESIAN_POINT ( 'NONE',  ( -34.92500000000001137, 1.077975372831878387, 13.01339814852643606 ) ) ;
#96105 = CARTESIAN_POINT ( 'NONE',  ( 92.82919371712955581, -3.975000000000001865, 6.884901960086284411 ) ) ;
#96107 = CONICAL_SURFACE ( 'NONE', #72990, 2.055000000000000604, 0.9599310885968764806 ) ;
#96106 = DIRECTION ( 'NONE',  ( -1.000000000000000000, -0.000000000000000000, -0.000000000000000000 ) ) ;
#96108 = EDGE_CURVE ( 'NONE', #64975, #32966, #80819, .T. ) ;
#96109 = AXIS2_PLACEMENT_3D ( 'NONE', #58502, #114245, #72766 ) ;
#96110 = CARTESIAN_POINT ( 'NONE',  ( -9.918025652846569784, 22.22500000000000142, -4.476077389926565786 ) ) ;
#96111 = VERTEX_POINT ( 'NONE', #77959 ) ;
#96112 = PRESENTATION_LAYER_ASSIGNMENT (  '', '', ( #105422 ) ) ;
#96113 = LINE ( 'NONE', #41754, #28372 ) ;
#96114 = FACE_OUTER_BOUND ( 'NONE', #33601, .T. ) ;
#96115 = DIRECTION ( 'NONE',  ( -0.3543493200069162685, -0.000000000000000000, -0.9351131265310288487 ) ) ;
#96116 = DIRECTION ( 'NONE',  ( -0.7071067811865486830, -0.7071067811865464625, -0.000000000000000000 ) ) ;
#96117 = ORIENTED_EDGE ( 'NONE', *, *, #62909, .T. ) ;
#96118 = EDGE_CURVE ( 'NONE', #128588, #128930, #25220, .T. ) ;
#96119 = LINE ( 'NONE', #19292, #134817 ) ;
#96120 = VERTEX_POINT ( 'NONE', #135894 ) ;
#96121 = EDGE_CURVE ( 'NONE', #98171, #102894, #56940, .T. ) ;
#96122 = CARTESIAN_POINT ( 'NONE',  ( 74.95876352523143282, 0.000000000000000000, -6.110000000000001208 ) ) ;
#96123 = CARTESIAN_POINT ( 'NONE',  ( 10.49999999999992895, 7.466399257802187606, 5.000000000000000000 ) ) ;
#96124 = PLANE ( 'NONE',  #649 ) ;
#96125 = VERTEX_POINT ( 'NONE', #44652 ) ;
#96126 = CARTESIAN_POINT ( 'NONE',  ( -34.92500000000001137, 22.22500000000000142, 0.4999999999999995559 ) ) ;
#96127 = LINE ( 'NONE', #54112, #132242 ) ;
#96128 = CARTESIAN_POINT ( 'NONE',  ( 118.4958603837962272, -3.974999999999998312, -6.884901960086286188 ) ) ;
#96129 = EDGE_CURVE ( 'NONE', #90375, #132873, #55497, .T. ) ;
#96131 = ORIENTED_EDGE ( 'NONE', *, *, #43257, .T. ) ;
#96130 = LINE ( 'NONE', #41055, #110042 ) ;
#96132 = CARTESIAN_POINT ( 'NONE',  ( 12.68750000000000000, 4.461849672132297329, -4.461849672132302658 ) ) ;
#96133 = DIRECTION ( 'NONE',  ( -0.000000000000000000, 1.000000000000000000, 1.224646799147353207E-16 ) ) ;
#96134 = CARTESIAN_POINT ( 'NONE',  ( 25.39999999999999858, 0.000000000000000000, 0.000000000000000000 ) ) ;
#96135 = DIRECTION ( 'NONE',  ( -0.7071067811865486830, -0.7071067811865464625, -0.000000000000000000 ) ) ;
#96136 = ORIENTED_EDGE ( 'NONE', *, *, #40527, .T. ) ;
#96137 = ORIENTED_EDGE ( 'NONE', *, *, #36159, .T. ) ;
#96138 = CARTESIAN_POINT ( 'NONE',  ( 72.18793019189810423, 6.110000000000002984, -1.637169565754156730 ) ) ;
#96139 = ORIENTED_EDGE ( 'NONE', *, *, #26958, .F. ) ;
#96140 = LINE ( 'NONE', #140377, #110047 ) ;
#96141 = CARTESIAN_POINT ( 'NONE',  ( 5.206660635421493488, 21.75929247661549937, 4.998822639870701856 ) ) ;
#96142 = CARTESIAN_POINT ( 'NONE',  ( 0.000000000000000000, 9.735942053221458872E-16, -7.950000000000000178 ) ) ;
#96143 = DIRECTION ( 'NONE',  ( 0.000000000000000000, 1.000000000000000000, 0.000000000000000000 ) ) ;
#96144 = ORIENTED_EDGE ( 'NONE', *, *, #62882, .T. ) ;
#96145 = FACE_OUTER_BOUND ( 'NONE', #75723, .T. ) ;
#96146 = FILL_AREA_STYLE ('',( #54826 ) ) ;
#96147 = ORIENTED_EDGE ( 'NONE', *, *, #76814, .T. ) ;
#96148 = LINE ( 'NONE', #5573, #25743 ) ;
#96149 = CARTESIAN_POINT ( 'NONE',  ( 34.42499999999998295, 22.22500000000000142, 5.000000000000000000 ) ) ;
#96150 = CARTESIAN_POINT ( 'NONE',  ( -8.671830600776406328, 8.259292476615634371, 4.000000000000000000 ) ) ;
#96151 =( BOUNDED_CURVE ( )  B_SPLINE_CURVE ( 3, ( #44595, #93047, #126378, #103198 ),
 .UNSPECIFIED., .F., .F. ) 
 B_SPLINE_CURVE_WITH_KNOTS ( ( 4, 4 ),
 ( 5.920967161967928050, 7.341195215986584977 ),
 .UNSPECIFIED. ) 
 CURVE ( )  GEOMETRIC_REPRESENTATION_ITEM ( )  RATIONAL_B_SPLINE_CURVE ( ( 1.000000000000000000, 0.8388583629366730410, 0.8388583629366730410, 1.000000000000000000 ) ) 
 REPRESENTATION_ITEM ( '' )  );
#96152 = VERTEX_POINT ( 'NONE', #67080 ) ;
#96153 = ORIENTED_EDGE ( 'NONE', *, *, #138619, .T. ) ;
#96154 = CARTESIAN_POINT ( 'NONE',  ( -31.49999999999976552, 13.46639925780212366, 5.000000000000000000 ) ) ;
#96155 = CARTESIAN_POINT ( 'NONE',  ( 7.637717201596474048, 4.584330080086930965E-16, 0.000000000000000000 ) ) ;
#96156 = CARTESIAN_POINT ( 'NONE',  ( 25.39999999999999147, -6.343664649937126754, -2.773223721129034480 ) ) ;
#96157 = LINE ( 'NONE', #19339, #132348 ) ;
#96158 = CARTESIAN_POINT ( 'NONE',  ( 15.48921356237309510, -27.52281430457066236, 5.000000000000000000 ) ) ;
#96159 = DIRECTION ( 'NONE',  ( -1.000000000000000000, -1.224606353822377258E-16, -0.000000000000000000 ) ) ;
#96160 =( NAMED_UNIT ( * ) PLANE_ANGLE_UNIT ( ) SI_UNIT ( $, .RADIAN. ) );
#96162 = ORIENTED_EDGE ( 'NONE', *, *, #118394, .T. ) ;
#96161 = AXIS2_PLACEMENT_3D ( 'NONE', #65536, #21976, #134893 ) ;
#96163 = EDGE_CURVE ( 'NONE', #107639, #110076, #13371, .T. ) ;
#96164 = ORIENTED_EDGE ( 'NONE', *, *, #104839, .F. ) ;
#96165 = ORIENTED_EDGE ( 'NONE', *, *, #51253, .F. ) ;
#96166 = ADVANCED_FACE ( 'NONE', ( #46803 ), #36813, .T. ) ;
#96167 = AXIS2_PLACEMENT_3D ( 'NONE', #132403, #34480, #56973 ) ;
#96168 = ORIENTED_EDGE ( 'NONE', *, *, #48911, .F. ) ;
#96169 = ADVANCED_FACE ( 'NONE', ( #35902 ), #22117, .F. ) ;
#96170 = CARTESIAN_POINT ( 'NONE',  ( 180.6665599231111230, -49.11775834062249402, 40.20665288736022802 ) ) ;
#96171 = EDGE_CURVE ( 'NONE', #139774, #114801, #80119, .T. ) ;
#96172 = DIRECTION ( 'NONE',  ( -0.7071067811865487940, 0.7071067811865463515, 0.000000000000000000 ) ) ;
#96173 = EDGE_LOOP ( 'NONE', ( #51460, #132015, #30285, #71874 ) ) ;
#96174 = DIRECTION ( 'NONE',  ( -0.7071067811865486830, -0.7071067811865464625, 0.000000000000000000 ) ) ;
#96175 = LINE ( 'NONE', #86770, #28812 ) ;
#96176 = CARTESIAN_POINT ( 'NONE',  ( 31.49999999999977973, 14.14708470758593784, -0.5283514160167287477 ) ) ;
#96177 = DIRECTION ( 'NONE',  ( 0.000000000000000000, 1.000000000000000000, 0.000000000000000000 ) ) ;
#96178 = LINE ( 'NONE', #62894, #30623 ) ;
#96179 = ORIENTED_EDGE ( 'NONE', *, *, #39137, .F. ) ;
#96180 = CARTESIAN_POINT ( 'NONE',  ( -15.48921356237309510, -27.52281430457066236, 5.000000000000000000 ) ) ;
#96181 = DIRECTION ( 'NONE',  ( -0.7071067811865486830, -0.7071067811865464625, 0.000000000000000000 ) ) ;
#96182 = EDGE_CURVE ( 'NONE', #109319, #132339, #124302, .T. ) ;
#96183 = ORIENTED_EDGE ( 'NONE', *, *, #29849, .F. ) ;
#96184 = CARTESIAN_POINT ( 'NONE',  ( -34.92500000000001137, -22.22500000000000142, 4.000000000000000000 ) ) ;
#96185 = ORIENTED_EDGE ( 'NONE', *, *, #92613, .T. ) ;
#96186 = ADVANCED_FACE ( 'NONE', ( #11956 ), #101112, .F. ) ;
#96187 = CARTESIAN_POINT ( 'NONE',  ( -19.05000000000000071, 3.174999999999997158, 5.000000000000000000 ) ) ;
#96188 = ORIENTED_EDGE ( 'NONE', *, *, #63254, .F. ) ;
#96189 = CARTESIAN_POINT ( 'NONE',  ( 62.85459685856477563, -1.637169565754161615, 6.110000000000000320 ) ) ;
#96190 = ORIENTED_EDGE ( 'NONE', *, *, #32992, .T. ) ;
#96191 = EDGE_LOOP ( 'NONE', ( #29216, #80625, #132984 ) ) ;
#96192 = EDGE_CURVE ( 'NONE', #41713, #69496, #79427, .T. ) ;
#96193 = AXIS2_PLACEMENT_3D ( 'NONE', #100619, #36086, #102038 ) ;
#96194 = CARTESIAN_POINT ( 'NONE',  ( -27.18398860626900060, 28.73617430169806042, 5.000000000000000000 ) ) ;
#96195 = VECTOR ( 'NONE', #15516, 999.9999999999998863 ) ;
#96196 = FACE_OUTER_BOUND ( 'NONE', #108568, .T. ) ;
#96197 = CARTESIAN_POINT ( 'NONE',  ( 101.0629301918980900, 1.637169565754157174, 6.110000000000002984 ) ) ;
#96198 = DIRECTION ( 'NONE',  ( -0.7071067811865486830, -0.7071067811865464625, -0.000000000000000000 ) ) ;
#96199 = VECTOR ( 'NONE', #81295, 1000.000000000000227 ) ;
#96200 = CARTESIAN_POINT ( 'NONE',  ( -28.49999999999980460, 12.05218569542904739, 5.000000000000000000 ) ) ;
#96201 = ADVANCED_FACE ( 'NONE', ( #104683 ), #83685, .F. ) ;
#96202 = CARTESIAN_POINT ( 'NONE',  ( -14.99999999999989875, -1.209798855135683748, 4.371887122346860721 ) ) ;
#96203 = VECTOR ( 'NONE', #86120, 1000.000000000000000 ) ;
#96204 = DIRECTION ( 'NONE',  ( -0.7071067811865486830, -0.7071067811865464625, 0.000000000000000000 ) ) ;
#96205 = DIRECTION ( 'NONE',  ( 0.7071067811865487940, 0.7071067811865463515, -0.000000000000000000 ) ) ;
#96206 = DIRECTION ( 'NONE',  ( 0.000000000000000000, 0.000000000000000000, 1.000000000000000000 ) ) ;
#96207 = VERTEX_POINT ( 'NONE', #25693 ) ;
#96208 = ORIENTED_EDGE ( 'NONE', *, *, #122558, .T. ) ;
#96209 = ORIENTED_EDGE ( 'NONE', *, *, #105058, .F. ) ;
#96210 = ORIENTED_EDGE ( 'NONE', *, *, #48553, .T. ) ;
#96211 = EDGE_CURVE ( 'NONE', #113151, #125882, #71361, .T. ) ;
#96212 = EDGE_LOOP ( 'NONE', ( #88490, #64002, #104639, #54181 ) ) ;
#96213 = FACE_OUTER_BOUND ( 'NONE', #38253, .T. ) ;
#96214 = CARTESIAN_POINT ( 'NONE',  ( -0.3281693992235271695, 20.25929247661551003, 4.000000000000000000 ) ) ;
#96215 = DIRECTION ( 'NONE',  ( 1.000000000000000000, 0.000000000000000000, 0.000000000000000000 ) ) ;
#96216 = ORIENTED_EDGE ( 'NONE', *, *, #117251, .F. ) ;
#96217 = CARTESIAN_POINT ( 'NONE',  ( 0.06788206741516134013, -51.13011358081639912, 36.94363806876511802 ) ) ;
#96218 = ORIENTED_EDGE ( 'NONE', *, *, #78013, .T. ) ;
#96219 = CARTESIAN_POINT ( 'NONE',  ( 8.582903141435219041, 3.967499999999992699, -6.871911579029513994 ) ) ;
#96220 = CARTESIAN_POINT ( 'NONE',  ( -5.700255128608413102, -27.71228299555201957, 4.000000000000000000 ) ) ;
#96221 = CARTESIAN_POINT ( 'NONE',  ( 8.673617379884035472E-16, -21.84840872380824450, 2.849755605029608230 ) ) ;
#96222 = CARTESIAN_POINT ( 'NONE',  ( 10.61403459356125190, -8.436352015943745286, -4.367863059733367415 ) ) ;
#96223 = VERTEX_POINT ( 'NONE', #114135 ) ;
#96224 = ORIENTED_EDGE ( 'NONE', *, *, #40086, .F. ) ;
#96225 = EDGE_CURVE ( 'NONE', #113826, #55035, #16213, .T. ) ;
#96226 = ORIENTED_EDGE ( 'NONE', *, *, #113858, .F. ) ;
#96227 = PLANE ( 'NONE',  #7852 ) ;
#96228 = DIRECTION ( 'NONE',  ( 0.000000000000000000, -1.000000000000000000, 0.000000000000000000 ) ) ;
#96229 = DIRECTION ( 'NONE',  ( -0.7071067811865486830, -0.7071067811865464625, 0.000000000000000000 ) ) ;
#96230 = LINE ( 'NONE', #119412, #45040 ) ;
#96231 = DIRECTION ( 'NONE',  ( -0.7071067811865486830, -0.7071067811865464625, 0.000000000000000000 ) ) ;
#96232 = LINE ( 'NONE', #75945, #24849 ) ;
#96233 = FACE_OUTER_BOUND ( 'NONE', #129029, .T. ) ;
#96234 = CARTESIAN_POINT ( 'NONE',  ( 30.62543019189810423, 5.291415217122919401, 3.055000000000002824 ) ) ;
#96235 = ADVANCED_FACE ( 'NONE', ( #115519 ), #72833, .F. ) ;
#96236 = CYLINDRICAL_SURFACE ( 'NONE', #79001, 2.500000000000000000 ) ;
#96237 = EDGE_LOOP ( 'NONE', ( #121650, #17452, #43804, #33498 ) ) ;
#96238 = DIRECTION ( 'NONE',  ( -0.000000000000000000, 0.000000000000000000, 1.000000000000000000 ) ) ;
#96239 = DIRECTION ( 'NONE',  ( -0.3543493200069163240, 0.000000000000000000, 0.9351131265310288487 ) ) ;
#96240 = EDGE_LOOP ( 'NONE', ( #113925, #42336, #5550, #86196 ) ) ;
#96241 = CARTESIAN_POINT ( 'NONE',  ( -28.49999999999979750, -4.912538124160708897, 4.000000000000000000 ) ) ;
#96243 = ORIENTED_EDGE ( 'NONE', *, *, #23829, .T. ) ;
#96242 = CARTESIAN_POINT ( 'NONE',  ( 57.10144406050384447, -49.69743550128772114, -36.79359617903136126 ) ) ;
#96244 = EDGE_CURVE ( 'NONE', #69882, #1156, #48173, .T. ) ;
#96245 = DIRECTION ( 'NONE',  ( 0.7071067811865487940, -0.7071067811865463515, 0.000000000000000000 ) ) ;
#96246 = CARTESIAN_POINT ( 'NONE',  ( 3.872664058232598183, 3.821174125832445049E-16, 0.000000000000000000 ) ) ;
#96247 = ORIENTED_EDGE ( 'NONE', *, *, #8932, .T. ) ;
#96248 = CARTESIAN_POINT ( 'NONE',  ( -12.48921356237309155, -27.52281430457064104, 5.000000000000000000 ) ) ;
#96249 = ORIENTED_EDGE ( 'NONE', *, *, #43491, .T. ) ;
#96250 = CARTESIAN_POINT ( 'NONE',  ( -18.70710678118641468, 20.25929247661551713, 5.000000000000000000 ) ) ;
#96251 = AXIS2_PLACEMENT_3D ( 'NONE', #52125, #85445, #129673 ) ;
#96252 = CARTESIAN_POINT ( 'NONE',  ( 125.3500270504628986, -5.819803920172572198, -5.819803920172572198 ) ) ;
#96253 = CARTESIAN_POINT ( 'NONE',  ( -34.49999999999975131, -4.912538124160707120, 4.000000000000000000 ) ) ;
#96254 = CARTESIAN_POINT ( 'NONE',  ( 35.71998032010574775, 0.7592924766157138627, 14.27032725228017185 ) ) ;
#96256 = EDGE_CURVE ( 'NONE', #37537, #39265, #60504, .T. ) ;
#96255 = DIRECTION ( 'NONE',  ( -0.7071067811865487940, 0.7071067811865463515, -0.000000000000000000 ) ) ;
#96257 = SURFACE_STYLE_USAGE ( .BOTH. , #5689 ) ;
#96258 = CARTESIAN_POINT ( 'NONE',  ( 1.516262732464673579, 3.821174125832445049E-16, 0.000000000000000000 ) ) ;
#96259 = CARTESIAN_POINT ( 'NONE',  ( 3.208333333333333481, 3.047499999999997655, 5.278424836066143655 ) ) ;
#96260 = CARTESIAN_POINT ( 'NONE',  ( 13.54123647476855474, 0.000000000000000000, 7.934999999999990727 ) ) ;
#96261 = DIRECTION ( 'NONE',  ( 0.000000000000000000, 0.000000000000000000, -1.000000000000000000 ) ) ;
#96262 = LINE ( 'NONE', #63700, #3774 ) ;
#96263 = ORIENTED_EDGE ( 'NONE', *, *, #127006, .T. ) ;
#96264 = ORIENTED_EDGE ( 'NONE', *, *, #116362, .T. ) ;
#96265 = VERTEX_POINT ( 'NONE', #17654 ) ;
#96266 = ADVANCED_FACE ( 'NONE', ( #27119 ), #62407, .T. ) ;
#96267 = VECTOR ( 'NONE', #86513, 999.9999999999998863 ) ;
#96268 = CARTESIAN_POINT ( 'NONE',  ( 13.49999999999990585, 16.77039438581780217, 0.4657186855307419160 ) ) ;
#96269 = PLANE ( 'NONE',  #101804 ) ;
#96270 = CARTESIAN_POINT ( 'NONE',  ( 8.343289998337821700, 3.759292476615681888, 13.27625715073267543 ) ) ;
#96271 = CARTESIAN_POINT ( 'NONE',  ( -12.70000000000000462, -25.83999999999998565, 2.999999999999999112 ) ) ;
#96272 = VERTEX_POINT ( 'NONE', #61927 ) ;
#96273 = DIRECTION ( 'NONE',  ( -0.6830127018922180770, -0.6830127018922204085, -0.2588190451025213501 ) ) ;
#96274 = DIRECTION ( 'NONE',  ( -0.6830127018922181881, 0.6830127018922202975, -0.2588190451025214056 ) ) ;
#96275 = LINE ( 'NONE', #40525, #25689 ) ;
#96276 = EDGE_CURVE ( 'NONE', #18833, #78237, #121201, .T. ) ;
#96277 = EDGE_CURVE ( 'NONE', #85340, #50158, #49634, .T. ) ;
#96278 = DIRECTION ( 'NONE',  ( 0.3543493200069163240, -0.000000000000000000, -0.9351131265310288487 ) ) ;
#96280 = EDGE_LOOP ( 'NONE', ( #20909, #121368, #96815, #38815 ) ) ;
#96279 = DIRECTION ( 'NONE',  ( 0.7071067811865487940, -0.7071067811865463515, 0.000000000000000000 ) ) ;
#96281 = LINE ( 'NONE', #140524, #83665 ) ;
#96282 = CARTESIAN_POINT ( 'NONE',  ( -8.999999999999934275, -21.41253812416053748, 4.000000000000000000 ) ) ;
#96283 = DIRECTION ( 'NONE',  ( -0.7071067811865487940, 0.7071067811865463515, 0.000000000000000000 ) ) ;
#96284 = CARTESIAN_POINT ( 'NONE',  ( 2.999999999999988898, 1.552185695429151080, 5.000000000000000000 ) ) ;
#96285 = FACE_OUTER_BOUND ( 'NONE', #124415, .T. ) ;
#96286 = VECTOR ( 'NONE', #34300, 1000.000000000000000 ) ;
#96287 = CARTESIAN_POINT ( 'NONE',  ( 61.46640106136305093, -43.15000000000001990, 34.92499999999998295 ) ) ;
#96288 = EDGE_LOOP ( 'NONE', ( #130082, #23394, #70600, #103829, #71964 ) ) ;
#96289 = ORIENTED_EDGE ( 'NONE', *, *, #78088, .T. ) ;
#96290 = VERTEX_POINT ( 'NONE', #92361 ) ;
#96291 = CONICAL_SURFACE ( 'NONE', #10614, 2.500000000000000888, 0.9599310885968822538 ) ;
#96292 = CARTESIAN_POINT ( 'NONE',  ( 106.0212635252314470, -4.472830434245839371, -4.472830434245840259 ) ) ;
#96293 = ORIENTED_EDGE ( 'NONE', *, *, #71799, .F. ) ;
#96294 = VECTOR ( 'NONE', #35570, 1000.000000000000000 ) ;
#96295 = CARTESIAN_POINT ( 'NONE',  ( 123.7287633665994804, -43.84677628532046612, 34.92499999999998295 ) ) ;
#96296 = VECTOR ( 'NONE', #58007, 1000.000000000000000 ) ;
#96297 = CARTESIAN_POINT ( 'NONE',  ( -2.207106781186529698, 18.75929247661552779, 5.000000000000000000 ) ) ;
#96298 = ORIENTED_EDGE ( 'NONE', *, *, #2876, .T. ) ;
#96299 = ADVANCED_FACE ( 'NONE', ( #38725 ), #26424, .T. ) ;
#96300 = FACE_OUTER_BOUND ( 'NONE', #53766, .T. ) ;
#96301 = DIRECTION ( 'NONE',  ( 0.7071067811865487940, 0.7071067811865463515, 0.000000000000000000 ) ) ;
#96302 = CARTESIAN_POINT ( 'NONE',  ( 97.76626352523143737, 4.472830434245839371, -4.472830434245838482 ) ) ;
#96303 = ORIENTED_EDGE ( 'NONE', *, *, #54310, .F. ) ;
#96304 = DIRECTION ( 'NONE',  ( 0.7071067811865486830, -0.7071067811865464625, -0.000000000000000000 ) ) ;
#96305 = DIRECTION ( 'NONE',  ( -0.7071067811865486830, -0.7071067811865464625, 0.000000000000000000 ) ) ;
#96306 = CARTESIAN_POINT ( 'NONE',  ( 34.92499999999998295, 15.00612307739180551, 4.000000000000000000 ) ) ;
#96307 = PLANE ( 'NONE',  #4438 ) ;
#96308 = VERTEX_POINT ( 'NONE', #95230 ) ;
#96309 = ORIENTED_EDGE ( 'NONE', *, *, #27667, .T. ) ;
#96310 = EDGE_LOOP ( 'NONE', ( #92901, #64855, #9274, #26552 ) ) ;
#96311 = LINE ( 'NONE', #52820, #134809 ) ;
#96312 = DIRECTION ( 'NONE',  ( 0.6830127018922180770, -0.6830127018922204085, -0.2588190451025213501 ) ) ;
#96313 = CARTESIAN_POINT ( 'NONE',  ( 5.025403141435219823, 2.126176841940962348, 7.934999999999988951 ) ) ;
#96314 = DIRECTION ( 'NONE',  ( -0.7071067811865486830, -0.7071067811865464625, -0.000000000000000000 ) ) ;
#96315 = PRESENTATION_STYLE_ASSIGNMENT (( #129685 ) ) ;
#96316 = EDGE_CURVE ( 'NONE', #90677, #74481, #15498, .T. ) ;
#96317 = ORIENTED_EDGE ( 'NONE', *, *, #107411, .F. ) ;
#96318 = VERTEX_POINT ( 'NONE', #40186 ) ;
#96319 = EDGE_CURVE ( 'NONE', #92143, #111424, #125011, .T. ) ;
#96320 = CARTESIAN_POINT ( 'NONE',  ( 12.70710678118645554, -18.74070752338409562, 5.000000000000000000 ) ) ;
#96321 = ORIENTED_EDGE ( 'NONE', *, *, #136588, .T. ) ;
#96322 = EDGE_LOOP ( 'NONE', ( #110414, #33588, #98518, #46927 ) ) ;
#96323 = STYLED_ITEM ( 'NONE', ( #119995 ), #12766 ) ;
#96324 = EDGE_CURVE ( 'NONE', #138495, #108055, #37297, .T. ) ;
#96325 = ADVANCED_FACE ( 'NONE', ( #82252 ), #114817, .T. ) ;
#96326 = FACE_OUTER_BOUND ( 'NONE', #141865, .T. ) ;
#96327 = CARTESIAN_POINT ( 'NONE',  ( -33.48921356237309510, -27.52281430457078670, 5.000000000000000000 ) ) ;
#96328 = ORIENTED_EDGE ( 'NONE', *, *, #60905, .F. ) ;
#96329 = DIRECTION ( 'NONE',  ( 0.000000000000000000, -1.000000000000000000, 0.000000000000000000 ) ) ;
#96330 = DIRECTION ( 'NONE',  ( -1.000000000000000000, -0.000000000000000000, -0.000000000000000000 ) ) ;
#96331 = CARTESIAN_POINT ( 'NONE',  ( 1.499999999999994449, -13.91253812416061564, 4.000000000000000000 ) ) ;
#96332 = CONICAL_SURFACE ( 'NONE', #114869, 2.055000000000001048, 0.9599310885968758145 ) ;
#96333 = DIRECTION ( 'NONE',  ( -1.000000000000000000, -1.224606353822377258E-16, -0.000000000000000000 ) ) ;
#96334 =( NAMED_UNIT ( * ) PLANE_ANGLE_UNIT ( ) SI_UNIT ( $, .RADIAN. ) );
#96335 = ORIENTED_EDGE ( 'NONE', *, *, #80293, .T. ) ;
#96336 = CARTESIAN_POINT ( 'NONE',  ( 16.49999999999988987, -5.947814304570758104, 5.000000000000000000 ) ) ;
#96337 = CARTESIAN_POINT ( 'NONE',  ( 36.14583333333331439, 2.130196079827356037, -7.950000000000043698 ) ) ;
#96338 = EDGE_CURVE ( 'NONE', #22961, #36965, #48899, .T. ) ;
#96339 = EDGE_LOOP ( 'NONE', ( #63978, #137859, #101521, #84236 ) ) ;
#96340 = CARTESIAN_POINT ( 'NONE',  ( 25.39999999999999858, -3.814127886917791255, -7.006053345101936891 ) ) ;
#96341 = DIRECTION ( 'NONE',  ( -1.000000000000000000, -1.224606353822377258E-16, -0.000000000000000000 ) ) ;
#96342 = CARTESIAN_POINT ( 'NONE',  ( -41.99451991528749062, 28.92564299267967343, 4.000000000000000000 ) ) ;
#96343 = EDGE_CURVE ( 'NONE', #125425, #117394, #38029, .T. ) ;
#96344 = EDGE_LOOP ( 'NONE', ( #69389, #55312, #4427, #10076 ) ) ;
#96345 = CARTESIAN_POINT ( 'NONE',  ( -11.99999999999990941, 4.552185695429119328, 5.000000000000000000 ) ) ;
#96346 = ORIENTED_EDGE ( 'NONE', *, *, #112441, .T. ) ;
#96347 = EDGE_LOOP ( 'NONE', ( #45441, #94331, #73724, #101113 ) ) ;
#96348 = ORIENTED_EDGE ( 'NONE', *, *, #54022, .T. ) ;
#96349 = EDGE_CURVE ( 'NONE', #49447, #97071, #76354, .T. ) ;
#96350 = AXIS2_PLACEMENT_3D ( 'NONE', #91065, #3294, #33821 ) ;
#96351 = FACE_OUTER_BOUND ( 'NONE', #142927, .T. ) ;
#96352 = ADVANCED_FACE ( 'NONE', ( #32126 ), #73504, .F. ) ;
#96353 = FILL_AREA_STYLE_COLOUR ( '', #46089 ) ;
#96354 = CARTESIAN_POINT ( 'NONE',  ( 36.18398860626899705, 28.73617430169812437, 5.000000000000000000 ) ) ;
#96355 = COLOUR_RGB ( '', 0.66274510, 0.83137255, 0.94901961) ;
#96356 = CARTESIAN_POINT ( 'NONE',  ( -18.48921356237309510, -27.52281430457068367, 5.000000000000000000 ) ) ;
#96357 = CARTESIAN_POINT ( 'NONE',  ( 34.17183060077623225, -5.240707523384234179, 4.000000000000000000 ) ) ;
#96358 = CARTESIAN_POINT ( 'NONE',  ( 9.183988606268997046, 28.73617430169793607, 5.000000000000000000 ) ) ;
#96360 = CARTESIAN_POINT ( 'NONE',  ( 19.49999999999986500, -4.216083040037233332, -7.486842126848701540 ) ) ;
#96359 = DIRECTION ( 'NONE',  ( -0.7071067811865486830, -0.7071067811865464625, -0.000000000000000000 ) ) ;
#96361 = EDGE_CURVE ( 'NONE', #40163, #72227, #29262, .T. ) ;
#96362 = DIRECTION ( 'NONE',  ( -0.7071067811865487940, 0.7071067811865463515, -0.000000000000000000 ) ) ;
#96363 = CARTESIAN_POINT ( 'NONE',  ( -20.20710678118640402, 12.75929247661558819, 5.000000000000000000 ) ) ;
#96364 = CARTESIAN_POINT ( 'NONE',  ( -34.42500000000001137, -12.02281430457044564, 5.000000000000000000 ) ) ;
#96365 = LINE ( 'NONE', #97834, #35584 ) ;
#96366 = VECTOR ( 'NONE', #126665, 1000.000000000000000 ) ;
#96367 = EDGE_LOOP ( 'NONE', ( #25384, #118839, #17855, #116581 ) ) ;
#96368 = ORIENTED_EDGE ( 'NONE', *, *, #126661, .F. ) ;
#96370 = VERTEX_POINT ( 'NONE', #43018 ) ;
#96369 = EDGE_CURVE ( 'NONE', #90677, #131000, #108216, .T. ) ;
#96371 = ORIENTED_EDGE ( 'NONE', *, *, #9246, .T. ) ;
#96372 = FACE_OUTER_BOUND ( 'NONE', #66883, .T. ) ;
#96373 = ORIENTED_EDGE ( 'NONE', *, *, #64607, .T. ) ;
#96374 = ORIENTED_EDGE ( 'NONE', *, *, #44508, .F. ) ;
#96375 = PLANE ( 'NONE',  #44521 ) ;
#96376 = CARTESIAN_POINT ( 'NONE',  ( 16.49999999999988276, -12.08601207473287964, -10.46905243149098119 ) ) ;
#96377 = VECTOR ( 'NONE', #2533, 1000.000000000000000 ) ;
#96378 = FACE_OUTER_BOUND ( 'NONE', #54457, .T. ) ;
#96379 = ADVANCED_FACE ( 'NONE', ( #117667 ), #119816, .F. ) ;
#96380 = ORIENTED_EDGE ( 'NONE', *, *, #3403, .T. ) ;
#96381 = EDGE_CURVE ( 'NONE', #124489, #18049, #140183, .T. ) ;
#96382 = LINE ( 'NONE', #139952, #81174 ) ;
#96383 = ORIENTED_EDGE ( 'NONE', *, *, #9462, .T. ) ;
#96384 = VECTOR ( 'NONE', #101689, 1000.000000000000000 ) ;
#96386 = CARTESIAN_POINT ( 'NONE',  ( -34.49999999999975842, 15.05432934483078533, 4.994342998332167660 ) ) ;
#96385 = VECTOR ( 'NONE', #32166, 1000.000000000000227 ) ;
#96387 = ADVANCED_FACE ( 'NONE', ( #119126 ), #7498, .F. ) ;
#96388 = CARTESIAN_POINT ( 'NONE',  ( -10.88982677111781427, -22.22500000000000142, 4.785647885939353863 ) ) ;
#96389 = AXIS2_PLACEMENT_3D ( 'NONE', #131290, #96480, #140723 ) ;
#96390 = CARTESIAN_POINT ( 'NONE',  ( 10.27540314143522160, -2.126176841940958351, -7.934999999999989839 ) ) ;
#96391 = ORIENTED_EDGE ( 'NONE', *, *, #96993, .T. ) ;
#96392 = CARTESIAN_POINT ( 'NONE',  ( 90.47459685856479439, 1.637169565754164280, -6.109999999999997655 ) ) ;
#96393 = PLANE ( 'NONE',  #62166 ) ;
#96394 = DIRECTION ( 'NONE',  ( -0.7071067811865486830, -0.7071067811865464625, 0.000000000000000000 ) ) ;
#96395 = DIRECTION ( 'NONE',  ( 0.3543493200069162685, -0.000000000000000000, -0.9351131265310288487 ) ) ;
#96396 = EDGE_LOOP ( 'NONE', ( #72598, #118196, #30011, #23691 ) ) ;
#96397 = ORIENTED_EDGE ( 'NONE', *, *, #24034, .T. ) ;
#96398 = DIRECTION ( 'NONE',  ( 0.7071067811865487940, 0.7071067811865463515, -0.000000000000000000 ) ) ;
#96399 = ORIENTED_EDGE ( 'NONE', *, *, #73097, .F. ) ;
#96400 = DIRECTION ( 'NONE',  ( -1.000000000000000000, -1.224606353822377258E-16, -0.000000000000000000 ) ) ;
#96401 = DIRECTION ( 'NONE',  ( 0.000000000000000000, -1.000000000000000000, 0.000000000000000000 ) ) ;
#96402 = AXIS2_PLACEMENT_3D ( 'NONE', #44830, #9999, #143368 ) ;
#96403 = LINE ( 'NONE', #105166, #21474 ) ;
#96404 = CARTESIAN_POINT ( 'NONE',  ( -34.92500000000001137, 22.22500000000000142, 4.000000000000000000 ) ) ;
#96405 = ORIENTED_EDGE ( 'NONE', *, *, #140335, .F. ) ;
#96406 = DIRECTION ( 'NONE',  ( 1.000000000000000000, 0.000000000000000000, 0.000000000000000000 ) ) ;
#96407 = LINE ( 'NONE', #117453, #129924 ) ;
#96408 = FACE_OUTER_BOUND ( 'NONE', #83950, .T. ) ;
#96409 = ORIENTED_EDGE ( 'NONE', *, *, #118549, .F. ) ;
#96410 = PLANE ( 'NONE',  #104533 ) ;
#96411 = CARTESIAN_POINT ( 'NONE',  ( -2.187538124160505415, -22.22500000000000142, 4.000000000000000000 ) ) ;
#96412 = VERTEX_POINT ( 'NONE', #140863 ) ;
#96414 = ORIENTED_EDGE ( 'NONE', *, *, #127373, .T. ) ;
#96413 = DIRECTION ( 'NONE',  ( 1.000000000000000000, 0.000000000000000000, 0.000000000000000000 ) ) ;
#96415 = ORIENTED_EDGE ( 'NONE', *, *, #18869, .F. ) ;
#96416 = DIRECTION ( 'NONE',  ( 0.7071067811865486830, -0.7071067811865464625, -0.000000000000000000 ) ) ;
#96417 = CARTESIAN_POINT ( 'NONE',  ( -36.18398860626899705, 28.73617430169812437, 5.000000000000000000 ) ) ;
#96418 = EDGE_LOOP ( 'NONE', ( #112595, #19751, #79723, #40295 ) ) ;
#96419 = CARTESIAN_POINT ( 'NONE',  ( 8.999999999999937828, -21.84840872380823740, 2.849755605029629546 ) ) ;
#96420 = PLANE ( 'NONE',  #56828 ) ;
#96421 = CARTESIAN_POINT ( 'NONE',  ( 6.792893218813407685, 18.75929247661553489, 5.000000000000000000 ) ) ;
#96422 = DIRECTION ( 'NONE',  ( -0.7071067811865486830, -0.7071067811865464625, 0.000000000000000000 ) ) ;
#96423 = CARTESIAN_POINT ( 'NONE',  ( 34.49999999999975842, 16.46425560840032531, 4.994342998332160555 ) ) ;
#96424 = DIRECTION ( 'NONE',  ( -0.000000000000000000, 0.3543493200069153248, 0.9351131265310292928 ) ) ;
#96425 = CARTESIAN_POINT ( 'NONE',  ( 34.49999999999975842, 10.46425560840038571, 4.994342998332157890 ) ) ;
#96426 = CARTESIAN_POINT ( 'NONE',  ( 17.99999999999987210, 12.83542986846998524, -1.025386466790412454 ) ) ;
#96427 = LINE ( 'NONE', #10852, #6237 ) ;
#96429 = VECTOR ( 'NONE', #139336, 999.9999999999998863 ) ;
#96428 = FACE_OUTER_BOUND ( 'NONE', #23795, .T. ) ;
#96430 = LINE ( 'NONE', #31230, #8935 ) ;
#96431 = CARTESIAN_POINT ( 'NONE',  ( 34.49999999999975131, 13.46425560840035196, 4.994342998332160555 ) ) ;
#96432 = DIRECTION ( 'NONE',  ( -3.166071393695993333E-32, 1.016133275908817741E-16, -1.000000000000000000 ) ) ;
#96433 = ORIENTED_EDGE ( 'NONE', *, *, #80691, .T. ) ;
#96434 = ORIENTED_EDGE ( 'NONE', *, *, #101844, .F. ) ;
#96435 = EDGE_LOOP ( 'NONE', ( #19346, #114701, #51987, #74937 ) ) ;
#96436 = CARTESIAN_POINT ( 'NONE',  ( 113.7291666666666572, 7.950000000000001954, -2.130196079827421762 ) ) ;
#96437 = ORIENTED_EDGE ( 'NONE', *, *, #54934, .F. ) ;
#96438 = VERTEX_POINT ( 'NONE', #8195 ) ;
#96439 = VERTEX_POINT ( 'NONE', #96625 ) ;
#96440 = VECTOR ( 'NONE', #139308, 1000.000000000000227 ) ;
#96441 = LINE ( 'NONE', #30528, #117455 ) ;
#96442 = FACE_OUTER_BOUND ( 'NONE', #34367, .T. ) ;
#96443 = ORIENTED_EDGE ( 'NONE', *, *, #18195, .T. ) ;
#96444 = FACE_OUTER_BOUND ( 'NONE', #42693, .T. ) ;
#96445 = CARTESIAN_POINT ( 'NONE',  ( 27.29974487139158512, -27.71228299555225405, 4.000000000000000000 ) ) ;
#96447 = VECTOR ( 'NONE', #94220, 1000.000000000000000 ) ;
#96446 = FACE_OUTER_BOUND ( 'NONE', #14997, .T. ) ;
#96448 = DIRECTION ( 'NONE',  ( -0.7071067811865486830, 0.7071067811865464625, 0.000000000000000000 ) ) ;
#96449 = CARTESIAN_POINT ( 'NONE',  ( 105.4379301918981042, -6.110000000000001208, 1.637169565754158951 ) ) ;
#96450 = ADVANCED_FACE ( 'NONE', ( #128587 ), #31422, .T. ) ;
#96451 = ORIENTED_EDGE ( 'NONE', *, *, #130943, .T. ) ;
#96452 = CARTESIAN_POINT ( 'NONE',  ( 10.93876867942899622, 8.767031578203539510, -29.74760889984009182 ) ) ;
#96453 = CARTESIAN_POINT ( 'NONE',  ( 17.87852683662842068, -20.24070752338407075, 7.412974875817750053 ) ) ;
#96454 = ADVANCED_FACE ( 'NONE', ( #53912 ), #18352, .F. ) ;
#96455 = CARTESIAN_POINT ( 'NONE',  ( -15.71462683630238111, 8.126010640810376273, 4.668119888204643075 ) ) ;
#96456 = DIRECTION ( 'NONE',  ( 0.000000000000000000, -1.000000000000000000, 0.000000000000000000 ) ) ;
#96457 = CARTESIAN_POINT ( 'NONE',  ( 22.49999999999985434, -10.53360074219763121, 5.000000000000000000 ) ) ;
#96458 = CARTESIAN_POINT ( 'NONE',  ( 39.18398860626899705, 28.73617430169814568, 5.000000000000000000 ) ) ;
#96459 = CARTESIAN_POINT ( 'NONE',  ( 28.22502705046288440, 5.819803920172573086, -5.819803920172572198 ) ) ;
#96460 = VECTOR ( 'NONE', #102479, 999.9999999999998863 ) ;
#96461 = FACE_OUTER_BOUND ( 'NONE', #86426, .T. ) ;
#96462 = EDGE_LOOP ( 'NONE', ( #125178, #114584, #16962, #71665 ) ) ;
#96463 = ORIENTED_EDGE ( 'NONE', *, *, #118266, .T. ) ;
#96464 = CARTESIAN_POINT ( 'NONE',  ( 26.95833333333332149, 3.974999999999997424, 6.884901960086288852 ) ) ;
#96465 = VECTOR ( 'NONE', #61298, 1000.000000000000000 ) ;
#96466 = ORIENTED_EDGE ( 'NONE', *, *, #9364, .F. ) ;
#96467 = EDGE_CURVE ( 'NONE', #44871, #29293, #42315, .T. ) ;
#96468 = CARTESIAN_POINT ( 'NONE',  ( 34.92499999999998295, -22.22500000000000142, 4.500000000000000888 ) ) ;
#96469 = CARTESIAN_POINT ( 'NONE',  ( 0.000000000000000000, 0.000000000000000000, 0.000000000000000000 ) ) ;
#96470 = CYLINDRICAL_SURFACE ( 'NONE', #75738, 2.500000000000000000 ) ;
#96471 = CARTESIAN_POINT ( 'NONE',  ( -27.79289321881326558, -8.240707523384200428, 5.000000000000000000 ) ) ;
#96472 = ADVANCED_FACE ( 'NONE', ( #64049 ), #29968, .T. ) ;
#96473 = PLANE ( 'NONE',  #99866 ) ;
#96474 = CARTESIAN_POINT ( 'NONE',  ( 120.8079301918980946, -6.109999999999998543, 1.637169565754158063 ) ) ;
#96475 = ORIENTED_EDGE ( 'NONE', *, *, #13061, .T. ) ;
#96476 = FACE_OUTER_BOUND ( 'NONE', #74314, .T. ) ;
#96477 = VERTEX_POINT ( 'NONE', #106809 ) ;
#96478 = FACE_OUTER_BOUND ( 'NONE', #12375, .T. ) ;
#96479 = EDGE_CURVE ( 'NONE', #61213, #45028, #117909, .T. ) ;
#96480 = DIRECTION ( 'NONE',  ( 0.6830127018922180770, -0.6830127018922204085, -0.2588190451025213501 ) ) ;
#96481 = PLANE ( 'NONE',  #64993 ) ;
#96482 = VERTEX_POINT ( 'NONE', #118403 ) ;
#96483 = AXIS2_PLACEMENT_3D ( 'NONE', #39869, #140563, #71773 ) ;
#96484 = CARTESIAN_POINT ( 'NONE',  ( 47.54209685856476852, 5.291415217122923842, -3.054999999999996163 ) ) ;
#96485 = ORIENTED_EDGE ( 'NONE', *, *, #128484, .T. ) ;
#96486 = LINE ( 'NONE', #42888, #746 ) ;
#96487 = DIRECTION ( 'NONE',  ( -0.6830127018922180770, -0.6830127018922204085, -0.2588190451025213501 ) ) ;
#96488 = DIRECTION ( 'NONE',  ( 0.000000000000000000, -1.000000000000000000, 0.000000000000000000 ) ) ;
#96489 = EDGE_CURVE ( 'NONE', #63809, #37645, #87226, .T. ) ;
#96490 = LINE ( 'NONE', #40736, #122780 ) ;
#96491 = AXIS2_PLACEMENT_3D ( 'NONE', #116853, #17527, #62488 ) ;
#96492 = AXIS2_PLACEMENT_3D ( 'NONE', #13771, #104363, #136291 ) ;
#96493 = MECHANICAL_DESIGN_GEOMETRIC_PRESENTATION_REPRESENTATION (  '', ( #40963 ), #128908 ) ;
#96494 = CARTESIAN_POINT ( 'NONE',  ( 39.43293019189811588, 1.637169565754156508, 6.110000000000000320 ) ) ;
#96495 = ORIENTED_EDGE ( 'NONE', *, *, #65353, .F. ) ;
#96496 = EDGE_CURVE ( 'NONE', #6847, #66027, #97348, .T. ) ;
#96497 = VECTOR ( 'NONE', #134634, 999.9999999999998863 ) ;
#96498 = DIRECTION ( 'NONE',  ( 0.7071067811865486830, -0.7071067811865464625, -0.000000000000000000 ) ) ;
#96499 = ORIENTED_EDGE ( 'NONE', *, *, #120889, .F. ) ;
#96500 = ORIENTED_EDGE ( 'NONE', *, *, #67696, .T. ) ;
#96501 = CIRCLE ( 'NONE', #38698, 2.500000000000000444 ) ;
#96502 = ORIENTED_EDGE ( 'NONE', *, *, #130976, .F. ) ;
#96503 = EDGE_CURVE ( 'NONE', #29058, #131561, #75644, .T. ) ;
#96504 = ADVANCED_FACE ( 'NONE', ( #121968 ), #100247, .F. ) ;
#96505 = PLANE ( 'NONE',  #63031 ) ;
#96506 = ORIENTED_EDGE ( 'NONE', *, *, #117221, .F. ) ;
#96507 = CARTESIAN_POINT ( 'NONE',  ( 44.26669371712954870, -7.949999999999998401, 2.130196079827423983 ) ) ;
#96508 = DIRECTION ( 'NONE',  ( -0.7071067811865487940, 0.7071067811865463515, -0.000000000000000000 ) ) ;
#96509 = EDGE_CURVE ( 'NONE', #42250, #98347, #46634, .T. ) ;
#96510 = DIRECTION ( 'NONE',  ( 0.6830127018922181881, 0.6830127018922202975, -0.2588190451025214056 ) ) ;
#96511 = FACE_BOUND ( 'NONE', #15555, .T. ) ;
#96512 = EDGE_CURVE ( 'NONE', #8455, #96941, #133598, .T. ) ;
#96513 = ORIENTED_EDGE ( 'NONE', *, *, #21329, .F. ) ;
#96514 = PLANE ( 'NONE',  #140566 ) ;
#96515 = CARTESIAN_POINT ( 'NONE',  ( -2.292893218813431666, 14.25929247661557220, 5.000000000000000000 ) ) ;
#96516 = DIRECTION ( 'NONE',  ( -0.7071067811865486830, 0.7071067811865464625, 0.000000000000000000 ) ) ;
#96517 = EDGE_CURVE ( 'NONE', #18457, #121677, #135050, .T. ) ;
#96518 = ORIENTED_EDGE ( 'NONE', *, *, #111462, .T. ) ;
#96519 = DIRECTION ( 'NONE',  ( -0.000000000000000000, -0.3543493200069152138, 0.9351131265310292928 ) ) ;
#96520 = ORIENTED_EDGE ( 'NONE', *, *, #129554, .T. ) ;
#96521 = AXIS2_PLACEMENT_3D ( 'NONE', #60614, #92460, #135989 ) ;
#96522 = VERTEX_POINT ( 'NONE', #34274 ) ;
#96523 = CARTESIAN_POINT ( 'NONE',  ( -3.489213562373097322, -27.52281430457057709, 5.000000000000000000 ) ) ;
#96524 = ORIENTED_EDGE ( 'NONE', *, *, #8810, .T. ) ;
#96525 = CARTESIAN_POINT ( 'NONE',  ( 60.28709685856478728, 3.054999999999997495, 5.291415217122919401 ) ) ;
#96526 = VECTOR ( 'NONE', #83562, 1000.000000000000000 ) ;
#96527 = EDGE_LOOP ( 'NONE', ( #45100, #17867, #117075, #87995 ) ) ;
#96528 = ADVANCED_FACE ( 'NONE', ( #79962 ), #134311, .F. ) ;
#96529 = FACE_OUTER_BOUND ( 'NONE', #120827, .T. ) ;
#96530 = CARTESIAN_POINT ( 'NONE',  ( -34.92500000000001137, -17.33753812416083306, 4.000000000000000000 ) ) ;
#96531 = ORIENTED_EDGE ( 'NONE', *, *, #90256, .T. ) ;
#96532 = VECTOR ( 'NONE', #103452, 1000.000000000000000 ) ;
#96533 = ADVANCED_FACE ( 'NONE', ( #13203 ), #121269, .F. ) ;
#96534 =( BOUNDED_CURVE ( )  B_SPLINE_CURVE ( 2, ( #116463, #39645, #18537, #61418, #83871, #126601, #83128, #127326, #62822, #28030, #27292, #128075, #104868 ),
 .UNSPECIFIED., .F., .F. ) 
 B_SPLINE_CURVE_WITH_KNOTS ( ( 3, 2, 2, 2, 2, 2, 3 ),
 ( 0.7833333333333333259, 0.7861111111111110938, 0.7888888888888888618, 0.7916666666666666297, 0.7944444444444443976, 0.7972222222222222765, 0.8000000000000000444 ),
 .UNSPECIFIED. ) 
 CURVE ( )  GEOMETRIC_REPRESENTATION_ITEM ( )  RATIONAL_B_SPLINE_CURVE ( ( 1.000000000000000000, 0.9659258262890683122, 1.000000000000000000, 0.9659258262890683122, 1.000000000000000000, 0.9659258262890683122, 1.000000000000000000, 0.9659258262890683122, 1.000000000000000000, 0.9659258262890683122, 1.000000000000000000, 0.9659258262890683122, 1.000000000000000000 ) ) 
 REPRESENTATION_ITEM ( '' )  );
#96535 = CARTESIAN_POINT ( 'NONE',  ( 30.48921356237309510, -27.52281430457076894, 5.000000000000000000 ) ) ;
#96536 = DIRECTION ( 'NONE',  ( -0.000000000000000000, -0.3543493200069152693, 0.9351131265310292928 ) ) ;
#96537 = LINE ( 'NONE', #39364, #52824 ) ;
#96538 = DIRECTION ( 'NONE',  ( 1.000000000000000000, 0.000000000000000000, 0.000000000000000000 ) ) ;
#96539 = LINE ( 'NONE', #41470, #120369 ) ;
#96540 = ORIENTED_EDGE ( 'NONE', *, *, #94951, .T. ) ;
#96541 = VECTOR ( 'NONE', #7113, 999.9999999999998863 ) ;
#96542 = VERTEX_POINT ( 'NONE', #112544 ) ;
#96543 = DIRECTION ( 'NONE',  ( -0.7071067811865487940, 0.7071067811865463515, 0.000000000000000000 ) ) ;
#96544 = DIRECTION ( 'NONE',  ( 0.7071067811865486830, -0.7071067811865464625, -0.000000000000000000 ) ) ;
#96545 = ORIENTED_EDGE ( 'NONE', *, *, #66831, .T. ) ;
#96546 = EDGE_LOOP ( 'NONE', ( #113318, #47605, #43244, #33272, #59303, #112458 ) ) ;
#96547 = EDGE_LOOP ( 'NONE', ( #101863, #132301, #112465, #7011, #66630, #63997, #100767, #23870, #69671, #37704, #16891, #57622, #2251, #139090, #22736, #49229, #7951, #3607, #12020, #134802, #106716, #30451, #130661, #85281, #89676, #108563, #131475, #128135, #42699, #135640, #136359, #59385, #31113, #8628, #12798, #43175, #50712, #117778 ) ) ;
#96548 = VECTOR ( 'NONE', #11295, 1000.000000000000000 ) ;
#96549 = DIRECTION ( 'NONE',  ( 0.6830127018922180770, -0.6830127018922204085, -0.2588190451025213501 ) ) ;
#96550 = ORIENTED_EDGE ( 'NONE', *, *, #121421, .T. ) ;
#96551 = LINE ( 'NONE', #50959, #101851 ) ;
#96552 = ADVANCED_FACE ( 'NONE', ( #67649 ), #11774, .T. ) ;
#96553 = LINE ( 'NONE', #63296, #135026 ) ;
#96554 = ADVANCED_FACE ( 'NONE', ( #77092 ), #124133, .F. ) ;
#96555 = CARTESIAN_POINT ( 'NONE',  ( 21.21290314143522338, 3.967499999999992699, -6.871911579029513994 ) ) ;
#96556 = LINE ( 'NONE', #133344, #14819 ) ;
#96557 = VERTEX_POINT ( 'NONE', #90061 ) ;
#96558 = CARTESIAN_POINT ( 'NONE',  ( 115.8495968585647802, 6.109999999999997655, 1.637169565754163836 ) ) ;
#96559 = AXIS2_PLACEMENT_3D ( 'NONE', #35790, #110430, #80010 ) ;
#96560 = CARTESIAN_POINT ( 'NONE',  ( 44.99451991528749772, 28.92564299267969474, 4.000000000000000000 ) ) ;
#96561 = DIRECTION ( 'NONE',  ( 0.7071067811865487940, -0.7071067811865463515, 0.000000000000000000 ) ) ;
#96563 = ORIENTED_EDGE ( 'NONE', *, *, #105961, .F. ) ;
#96562 = CARTESIAN_POINT ( 'NONE',  ( 25.39999999999999858, -30.18000000000009564, 15.92499999999935945 ) ) ;
#96564 = PLANE ( 'NONE',  #41538 ) ;
#96565 = ORIENTED_EDGE ( 'NONE', *, *, #96086, .T. ) ;
#96566 = LINE ( 'NONE', #53082, #86729 ) ;
#96567 = DIRECTION ( 'NONE',  ( 0.000000000000000000, 0.000000000000000000, 1.000000000000000000 ) ) ;
#96568 = DIRECTION ( 'NONE',  ( -1.000000000000000000, -1.224606353822377258E-16, -0.000000000000000000 ) ) ;
#96569 = ORIENTED_EDGE ( 'NONE', *, *, #115815, .F. ) ;
#96570 = DIRECTION ( 'NONE',  ( -0.000000000000000000, -0.000000000000000000, 1.000000000000000000 ) ) ;
#96571 = DIRECTION ( 'NONE',  ( -1.000000000000000000, -1.224606353822377258E-16, -0.000000000000000000 ) ) ;
#96572 = CARTESIAN_POINT ( 'NONE',  ( -18.48921356237309510, -27.52281430457068367, 5.000000000000000000 ) ) ;
#96573 = ORIENTED_EDGE ( 'NONE', *, *, #61617, .T. ) ;
#96574 = DIRECTION ( 'NONE',  ( 0.000000000000000000, -1.000000000000000000, 0.000000000000000000 ) ) ;
#96575 = LINE ( 'NONE', #50987, #125679 ) ;
#96576 = CARTESIAN_POINT ( 'NONE',  ( -32.20710678118631165, -17.24070752338410983, 5.000000000000000000 ) ) ;
#96577 = VECTOR ( 'NONE', #87974, 1000.000000000000000 ) ;
#96578 = DIRECTION ( 'NONE',  ( -0.3543493200069162685, -0.000000000000000000, -0.9351131265310288487 ) ) ;
#96579 = EDGE_LOOP ( 'NONE', ( #113184, #87430, #53648, #37841, #64306 ) ) ;
#96580 = VERTEX_POINT ( 'NONE', #12505 ) ;
#96581 = PLANE ( 'NONE',  #86615 ) ;
#96582 = DIRECTION ( 'NONE',  ( -0.000000000000000000, -0.3543493200069152693, 0.9351131265310292928 ) ) ;
#96583 = AXIS2_PLACEMENT_3D ( 'NONE', #108433, #65740, #54831 ) ;
#96584 = AXIS2_PLACEMENT_3D ( 'NONE', #77155, #111142, #23441 ) ;
#96585 = CARTESIAN_POINT ( 'NONE',  ( 11.64540314143521904, -2.126176841940958351, -7.934999999999989839 ) ) ;
#96586 = DIRECTION ( 'NONE',  ( -0.7071067811865486830, -0.7071067811865464625, -0.000000000000000000 ) ) ;
#96587 = CIRCLE ( 'NONE', #36417, 2.500000000000000444 ) ;
#96588 = DIRECTION ( 'NONE',  ( 1.000000000000000000, 0.000000000000000000, 0.000000000000000000 ) ) ;
#96589 = DIRECTION ( 'NONE',  ( 1.000000000000000000, 0.000000000000000000, 0.000000000000000000 ) ) ;
#96590 = ORIENTED_EDGE ( 'NONE', *, *, #55966, .F. ) ;
#96591 = LINE ( 'NONE', #30685, #109043 ) ;
#96592 = DIRECTION ( 'NONE',  ( 1.000000000000000000, 0.000000000000000000, 0.000000000000000000 ) ) ;
#96593 = CARTESIAN_POINT ( 'NONE',  ( 5.441639616203772789, -6.094999999999989093, 1.633150327867691542 ) ) ;
#96594 = VECTOR ( 'NONE', #70185, 1000.000000000000227 ) ;
#96595 = DIRECTION ( 'NONE',  ( 1.000000000000000000, 0.000000000000000000, 0.000000000000000000 ) ) ;
#96596 = CARTESIAN_POINT ( 'NONE',  ( 34.47459685856478018, 1.637169565754164280, -6.109999999999997655 ) ) ;
#96597 = CARTESIAN_POINT ( 'NONE',  ( -0.1214731633714660752, -20.24070752338407075, 7.412974875817792686 ) ) ;
#96598 = EDGE_LOOP ( 'NONE', ( #8703, #32314, #93499, #90643 ) ) ;
#96599 = FILL_AREA_STYLE ('',( #8174 ) ) ;
#96600 = VERTEX_POINT ( 'NONE', #55322 ) ;
#96601 = ORIENTED_EDGE ( 'NONE', *, *, #25620, .T. ) ;
#96602 = CARTESIAN_POINT ( 'NONE',  ( 26.99999999999981526, 7.007997736742471062, -8.085015511992050818 ) ) ;
#96603 = DIRECTION ( 'NONE',  ( -0.7071067811865486830, 0.7071067811865464625, 0.000000000000000000 ) ) ;
#96604 = ORIENTED_EDGE ( 'NONE', *, *, #125721, .T. ) ;
#96605 = CARTESIAN_POINT ( 'NONE',  ( -6.183988606268994381, 28.73617430169791476, 5.000000000000000000 ) ) ;
#96606 = CARTESIAN_POINT ( 'NONE',  ( 38.99451991528749062, 28.92564299267965211, 4.000000000000000000 ) ) ;
#96607 = EDGE_CURVE ( 'NONE', #31098, #93168, #88671, .T. ) ;
#96608 = CARTESIAN_POINT ( 'NONE',  ( 8.031592354503320763, -2.500000000000000444, 3.061616997868384620E-16 ) ) ;
#96609 = DIRECTION ( 'NONE',  ( -0.7071067811865486830, -0.7071067811865464625, 0.000000000000000000 ) ) ;
#96610 = CARTESIAN_POINT ( 'NONE',  ( 128.9683591370937847, -49.14999999999998437, 41.64499999999998181 ) ) ;
#96611 = ADVANCED_FACE ( 'NONE', ( #43716 ), #33586, .T. ) ;
#96612 = EDGE_CURVE ( 'NONE', #133571, #31974, #79252, .T. ) ;
#96613 = ORIENTED_EDGE ( 'NONE', *, *, #79105, .F. ) ;
#96614 = CARTESIAN_POINT ( 'NONE',  ( 2.000000000000011546, 2.638703287232806449, -5.494203305479936184 ) ) ;
#96615 = CARTESIAN_POINT ( 'NONE',  ( 2.538396446294277631, -9.740707523384180888, 17.74957260769611267 ) ) ;
#96616 = AXIS2_PLACEMENT_3D ( 'NONE', #108315, #98892, #10453 ) ;
#96617 = DIRECTION ( 'NONE',  ( 0.7071067811865486830, -0.7071067811865464625, -0.000000000000000000 ) ) ;
#96618 = LINE ( 'NONE', #77085, #8487 ) ;
#96619 = CARTESIAN_POINT ( 'NONE',  ( 0.5685132242927012358, 4.584330080086930965E-16, 0.000000000000000000 ) ) ;
#96620 = FACE_OUTER_BOUND ( 'NONE', #113731, .T. ) ;
#96621 = EDGE_CURVE ( 'NONE', #54679, #33281, #66201, .T. ) ;
#96623 = ADVANCED_FACE ( 'NONE', ( #57476 ), #32870, .T. ) ;
#96622 = CARTESIAN_POINT ( 'NONE',  ( 59.14169371712955581, -2.130196079827424871, -7.949999999999999289 ) ) ;
#96624 = VECTOR ( 'NONE', #96936, 999.9999999999998863 ) ;
#96625 = CARTESIAN_POINT ( 'NONE',  ( -13.49999999999990052, 16.46639925780209168, 5.000000000000000000 ) ) ;
#96626 = EDGE_LOOP ( 'NONE', ( #98207, #47008, #135575 ) ) ;
#96627 = ORIENTED_EDGE ( 'NONE', *, *, #42410, .F. ) ;
#96628 = CARTESIAN_POINT ( 'NONE',  ( 56.70833333333333570, -3.974999999999999201, -6.884901960086287964 ) ) ;
#96629 = DIRECTION ( 'NONE',  ( 0.6830127018922181881, 0.6830127018922202975, -0.2588190451025214056 ) ) ;
#96630 = EDGE_CURVE ( 'NONE', #139000, #101542, #2316, .T. ) ;
#96631 = FACE_OUTER_BOUND ( 'NONE', #16467, .T. ) ;
#96632 = DIRECTION ( 'NONE',  ( -0.7071067811865486830, -0.7071067811865464625, 0.000000000000000000 ) ) ;
#96633 = EDGE_LOOP ( 'NONE', ( #127144, #30658, #13613, #100556, #105189, #130849 ) ) ;
#96634 = CARTESIAN_POINT ( 'NONE',  ( -10.49999999999992006, 0.05218569542917404769, 5.000000000000000000 ) ) ;
#96635 = EDGE_CURVE ( 'NONE', #70864, #22430, #44464, .T. ) ;
#96636 = CARTESIAN_POINT ( 'NONE',  ( 52.06293019189809712, 1.637169565754157174, 6.110000000000002984 ) ) ;
#96637 = EDGE_LOOP ( 'NONE', ( #86335, #131053, #46521, #109995 ) ) ;
#96638 = EDGE_CURVE ( 'NONE', #358, #4623, #103778, .T. ) ;
#96639 = CARTESIAN_POINT ( 'NONE',  ( 15.65467068707222076, 3.821174125832445049E-16, 0.000000000000000000 ) ) ;
#96640 = EDGE_LOOP ( 'NONE', ( #114453, #62973, #35431, #123815 ) ) ;
#96641 = VERTEX_POINT ( 'NONE', #17503 ) ;
#96642 = DIRECTION ( 'NONE',  ( -0.6830127018922181881, 0.6830127018922202975, -0.2588190451025214056 ) ) ;
#96643 = ADVANCED_FACE ( 'NONE', ( #60332 ), #116098, .F. ) ;
#96644 = LINE ( 'NONE', #121289, #56939 ) ;
#96645 = CARTESIAN_POINT ( 'NONE',  ( -6.498163485139524909, -17.24070752338410628, 8.407044977365240257 ) ) ;
#96646 = ORIENTED_EDGE ( 'NONE', *, *, #4882, .F. ) ;
#96647 = DIRECTION ( 'NONE',  ( -0.7071067811865486830, 0.7071067811865464625, 0.000000000000000000 ) ) ;
#96649 = ORIENTED_EDGE ( 'NONE', *, *, #14102, .F. ) ;
#96648 = DIRECTION ( 'NONE',  ( 0.6830127018922181881, 0.6830127018922202975, -0.2588190451025214056 ) ) ;
#96650 = CARTESIAN_POINT ( 'NONE',  ( 85.75043019189810423, 3.055000000000002824, -5.291415217122919401 ) ) ;
#96651 = CARTESIAN_POINT ( 'NONE',  ( 17.39159235450332019, 9.902892378096218942E-16, 0.000000000000000000 ) ) ;
#96652 = CARTESIAN_POINT ( 'NONE',  ( -16.49999999999988987, -12.08601207473291872, -10.46905243149090836 ) ) ;
#96653 =( NAMED_UNIT ( * ) SI_UNIT ( $, .STERADIAN. ) SOLID_ANGLE_UNIT ( ) );
#96654 = EDGE_CURVE ( 'NONE', #42509, #94617, #91518, .T. ) ;
#96655 = CARTESIAN_POINT ( 'NONE',  ( -34.42500000000001137, 21.72500000000000142, 4.000000000000000000 ) ) ;
#96656 = VERTEX_POINT ( 'NONE', #3057 ) ;
#96657 = ORIENTED_EDGE ( 'NONE', *, *, #127022, .T. ) ;
#96658 = VECTOR ( 'NONE', #74652, 1000.000000000000000 ) ;
#96659 = CARTESIAN_POINT ( 'NONE',  ( 27.22000000000000242, -2.055000000000000160, 2.789133085058098087E-16 ) ) ;
#96660 = CARTESIAN_POINT ( 'NONE',  ( 64.37043019189810877, -3.055000000000001492, 5.291415217122917625 ) ) ;
#96661 = DIRECTION ( 'NONE',  ( -0.6830127018922181881, 0.6830127018922202975, -0.2588190451025214056 ) ) ;
#96662 = EDGE_CURVE ( 'NONE', #114524, #100040, #124844, .T. ) ;
#96663 = LINE ( 'NONE', #117705, #47830 ) ;
#96664 = DIRECTION ( 'NONE',  ( -0.7071067811865486830, -0.7071067811865464625, -0.000000000000000000 ) ) ;
#96665 = VERTEX_POINT ( 'NONE', #138590 ) ;
#96666 = EDGE_LOOP ( 'NONE', ( #108679, #38344, #80272, #36854, #136806, #126586 ) ) ;
#96667 = DIRECTION ( 'NONE',  ( 0.000000000000000000, -1.000000000000000000, 0.000000000000000000 ) ) ;
#96668 = LINE ( 'NONE', #41613, #28314 ) ;
#96669 = ORIENTED_EDGE ( 'NONE', *, *, #28965, .F. ) ;
#96670 = EDGE_CURVE ( 'NONE', #8586, #141224, #58941, .T. ) ;
#96671 = VERTEX_POINT ( 'NONE', #5171 ) ;
#96672 = AXIS2_PLACEMENT_3D ( 'NONE', #48895, #112705, #35898 ) ;
#96673 = ADVANCED_BREP_SHAPE_REPRESENTATION ( '', ( #139143, #127880 ), #114185 ) ;
#96674 = DIRECTION ( 'NONE',  ( -0.7071067811865487940, 0.7071067811865463515, 0.000000000000000000 ) ) ;
#96676 = ADVANCED_FACE ( 'NONE', ( #37119 ), #92927, .F. ) ;
#96675 = ORIENTED_EDGE ( 'NONE', *, *, #117021, .T. ) ;
#96677 = FACE_OUTER_BOUND ( 'NONE', #109593, .T. ) ;
#96678 = FACE_OUTER_BOUND ( 'NONE', #44203, .T. ) ;
#96679 = VECTOR ( 'NONE', #120650, 1000.000000000000227 ) ;
#96680 = EDGE_CURVE ( 'NONE', #18415, #37390, #61758, .T. ) ;
#96681 = LINE ( 'NONE', #75003, #44299 ) ;
#96682 = VECTOR ( 'NONE', #129509, 1000.000000000000000 ) ;
#96683 = FACE_BOUND ( 'NONE', #29681, .T. ) ;
#96684 = CARTESIAN_POINT ( 'NONE',  ( 39.29177708983023365, -15.74070752338412760, 19.73771281079106998 ) ) ;
#96685 = CARTESIAN_POINT ( 'NONE',  ( 8.000000000000007105, 1.399551250596199630E-16, -1.142820323027522456 ) ) ;
#96686 = CYLINDRICAL_SURFACE ( 'NONE', #126715, 7.950000000000000178 ) ;
#96688 = EDGE_LOOP ( 'NONE', ( #114579, #27818, #61164, #54469 ) ) ;
#96687 = CARTESIAN_POINT ( 'NONE',  ( -7.499999999999947597, -8.568876922607733704, 4.000000000000000000 ) ) ;
#96689 = VECTOR ( 'NONE', #119523, 999.9999999999998863 ) ;
#96690 = DIRECTION ( 'NONE',  ( 0.000000000000000000, -1.000000000000000000, 0.000000000000000000 ) ) ;
#96691 = ITEM_DEFINED_TRANSFORMATION ( 'NONE', 'NONE', #23855,  #127880 ) ;
#96692 = ORIENTED_EDGE ( 'NONE', *, *, #40297, .F. ) ;
#96693 = ORIENTED_EDGE ( 'NONE', *, *, #138688, .T. ) ;
#96694 = CARTESIAN_POINT ( 'NONE',  ( 84.34959685856478018, 6.109999999999996767, 1.637169565754163836 ) ) ;
#96695 = VERTEX_POINT ( 'NONE', #126277 ) ;
#96696 = EDGE_CURVE ( 'NONE', #123294, #47726, #25519, .T. ) ;
#96697 = DIRECTION ( 'NONE',  ( -0.000000000000000000, 0.000000000000000000, 1.000000000000000000 ) ) ;
#96698 = VERTEX_POINT ( 'NONE', #104513 ) ;
#96699 = CARTESIAN_POINT ( 'NONE',  ( -28.82816939922332011, 3.759292476615681888, 4.000000000000000000 ) ) ;
#96700 = EDGE_CURVE ( 'NONE', #89049, #143240, #47351, .T. ) ;
#96701 = DIRECTION ( 'NONE',  ( 4.681814790819592407E-17, 0.3543493200069153248, 0.9351131265310292928 ) ) ;
#96702 = CARTESIAN_POINT ( 'NONE',  ( -10.00193056682090997, -22.22500000000000142, 4.500000000000000888 ) ) ;
#96703 = DIRECTION ( 'NONE',  ( 0.7071067811865487940, 0.7071067811865463515, 0.000000000000000000 ) ) ;
#96704 = PLANE ( 'NONE',  #34305 ) ;
#96705 = DIRECTION ( 'NONE',  ( -0.7071067811865486830, 0.7071067811865464625, 0.000000000000000000 ) ) ;
#96706 = CARTESIAN_POINT ( 'NONE',  ( 20.99451991528748707, 28.92564299267952777, 4.000000000000000000 ) ) ;
#96707 = CARTESIAN_POINT ( 'NONE',  ( 16.82816939922341248, -11.24070752338416490, 4.000000000000000000 ) ) ;
#96708 = EDGE_LOOP ( 'NONE', ( #18598, #60158, #101093, #116880 ) ) ;
#96709 = CARTESIAN_POINT ( 'NONE',  ( 48.18398860626899705, 28.73617430169820608, 5.000000000000000000 ) ) ;
#96710 = ORIENTED_EDGE ( 'NONE', *, *, #45748, .F. ) ;
#96711 = LINE ( 'NONE', #7583, #98166 ) ;
#96712 = CYLINDRICAL_SURFACE ( 'NONE', #123110, 5.999999999999998224 ) ;
#96713 = ORIENTED_EDGE ( 'NONE', *, *, #142032, .T. ) ;
#96714 = ADVANCED_FACE ( 'NONE', ( #82098 ), #114665, .T. ) ;
#96715 = ORIENTED_EDGE ( 'NONE', *, *, #99424, .T. ) ;
#96716 = ORIENTED_EDGE ( 'NONE', *, *, #103670, .F. ) ;
#96717 = CARTESIAN_POINT ( 'NONE',  ( 39.37543019189809712, -5.291415217122920289, -3.055000000000001492 ) ) ;
#96718 = VECTOR ( 'NONE', #76256, 1000.000000000000000 ) ;
#96719 = ORIENTED_EDGE ( 'NONE', *, *, #46400, .F. ) ;
#96720 = CARTESIAN_POINT ( 'NONE',  ( -51.29974487139158867, -27.71228299555242103, 4.000000000000000000 ) ) ;
#96721 =( BOUNDED_CURVE ( )  B_SPLINE_CURVE ( 3, ( #85928, #64191, #106222, #6896 ),
 .UNSPECIFIED., .F., .T. ) 
 B_SPLINE_CURVE_WITH_KNOTS ( ( 4, 4 ),
 ( 1.248621635838844890, 1.295595743666721811 ),
 .UNSPECIFIED. ) 
 CURVE ( )  GEOMETRIC_REPRESENTATION_ITEM ( )  RATIONAL_B_SPLINE_CURVE ( ( 1.000000000000000000, 0.9998161278856747547, 0.9998161278856747547, 1.000000000000000000 ) ) 
 REPRESENTATION_ITEM ( '' )  );
#96722 = CARTESIAN_POINT ( 'NONE',  ( 23.23330628287043709, -6.094999999999989981, -1.633150327867689100 ) ) ;
#96723 = CARTESIAN_POINT ( 'NONE',  ( 2.438206507620173102, 12.42651081890557307, -25.38545720235088154 ) ) ;
#96724 = ORIENTED_EDGE ( 'NONE', *, *, #64349, .F. ) ;
#96725 = CARTESIAN_POINT ( 'NONE',  ( 18.40295003975137433, -2.759949774800250388, 4.658785122533355860 ) ) ;
#96726 = ORIENTED_EDGE ( 'NONE', *, *, #116712, .T. ) ;
#96727 = CYLINDRICAL_SURFACE ( 'NONE', #35932, 0.5000000000000004441 ) ;
#96729 = ORIENTED_EDGE ( 'NONE', *, *, #93346, .T. ) ;
#96728 = DIRECTION ( 'NONE',  ( -1.000000000000000000, -0.000000000000000000, -0.000000000000000000 ) ) ;
#96730 = EDGE_LOOP ( 'NONE', ( #138474, #122290, #63934, #64498 ) ) ;
#96731 = EDGE_CURVE ( 'NONE', #126491, #97154, #61076, .T. ) ;
#96732 = CARTESIAN_POINT ( 'NONE',  ( 12.48921356237309155, -27.52281430457064104, 5.000000000000000000 ) ) ;
#96733 = AXIS2_PLACEMENT_3D ( 'NONE', #128560, #62598, #27813 ) ;
#96734 = CARTESIAN_POINT ( 'NONE',  ( -29.99451991528749417, 28.92564299267958816, 4.000000000000000000 ) ) ;
#96735 = VERTEX_POINT ( 'NONE', #132559 ) ;
#96736 = EDGE_CURVE ( 'NONE', #137044, #118417, #10700, .T. ) ;
#96737 = CARTESIAN_POINT ( 'NONE',  ( -7.940000000000001279, -33.26999999999999602, -11.89864999999999462 ) ) ;
#96738 = ORIENTED_EDGE ( 'NONE', *, *, #112450, .T. ) ;
#96739 = PRODUCT ( '1.2 Vise Screw', '1.2 Vise Screw', '', ( #17713 ) ) ;
#96740 = ORIENTED_EDGE ( 'NONE', *, *, #15291, .T. ) ;
#96741 = ORIENTED_EDGE ( 'NONE', *, *, #47699, .T. ) ;
#96742 = LINE ( 'NONE', #86647, #37911 ) ;
#96743 = CARTESIAN_POINT ( 'NONE',  ( -2.999999999999976463, -19.22509904557637128, 1.855685503482171983 ) ) ;
#96744 = CARTESIAN_POINT ( 'NONE',  ( -6.280019679894003559, 0.7592924766157138627, 14.27032725228007415 ) ) ;
#96745 = CARTESIAN_POINT ( 'NONE',  ( 15.18398860626900237, 28.73617430169797871, 5.000000000000000000 ) ) ;
#96746 = CARTESIAN_POINT ( 'NONE',  ( 0.000000000000000000, 2.375000000000000000, 4.319999999999998508 ) ) ;
#96747 = CARTESIAN_POINT ( 'NONE',  ( 150.3000000000000114, 7.776507174585691177E-16, -6.349999999999997868 ) ) ;
#96748 = EDGE_CURVE ( 'NONE', #136089, #101203, #110725, .T. ) ;
#96749 = VERTEX_POINT ( 'NONE', #21619 ) ;
#96750 = LINE ( 'NONE', #51161, #16443 ) ;
#96751 = VERTEX_POINT ( 'NONE', #554 ) ;
#96752 = CARTESIAN_POINT ( 'NONE',  ( 48.29974487139158867, -27.71228299555239971, 4.000000000000000000 ) ) ;
#96753 = CARTESIAN_POINT ( 'NONE',  ( 33.37456980810188156, 6.871911579029510442, -3.967499999999998916 ) ) ;
#96754 = EDGE_LOOP ( 'NONE', ( #115969, #48730, #5907, #59544, #93364 ) ) ;
#96755 = LINE ( 'NONE', #143157, #11298 ) ;
#96756 = VECTOR ( 'NONE', #101553, 1000.000000000000000 ) ;
#96757 = LINE ( 'NONE', #21394, #49001 ) ;
#96758 = VERTEX_POINT ( 'NONE', #65145 ) ;
#96759 = ORIENTED_EDGE ( 'NONE', *, *, #130415, .F. ) ;
#96760 = PLANE ( 'NONE',  #58600 ) ;
#96761 = DIRECTION ( 'NONE',  ( 0.6830127018922181881, 0.6830127018922202975, -0.2588190451025214056 ) ) ;
#96762 = CARTESIAN_POINT ( 'NONE',  ( 0.3818979091347701749, -51.95642703809002683, -39.54367611436767760 ) ) ;
#96763 = CARTESIAN_POINT ( 'NONE',  ( 61.45376352523145158, -6.109999999999999432, -3.741295971395163529E-16 ) ) ;
#96764 = CARTESIAN_POINT ( 'NONE',  ( 34.42499999999998295, 22.22500000000000142, 5.000000000000000000 ) ) ;
#96765 = LINE ( 'NONE', #141020, #62313 ) ;
#96766 = CARTESIAN_POINT ( 'NONE',  ( 28.00193056682079273, -22.22500000000000142, 4.500000000000000888 ) ) ;
#96767 = CARTESIAN_POINT ( 'NONE',  ( 8.999999999999937828, -9.412538124160663600, 4.000000000000000000 ) ) ;
#96768 = ORIENTED_EDGE ( 'NONE', *, *, #61772, .F. ) ;
#96769 = CARTESIAN_POINT ( 'NONE',  ( 6.328169399223485314, 2.259292476615697876, 4.000000000000000000 ) ) ;
#96770 = EDGE_CURVE ( 'NONE', #76705, #39505, #89038, .T. ) ;
#96771 = ORIENTED_EDGE ( 'NONE', *, *, #96489, .F. ) ;
#96772 = LINE ( 'NONE', #85946, #80261 ) ;
#96773 = PRESENTATION_STYLE_ASSIGNMENT (( #132347 ) ) ;
#96774 = VERTEX_POINT ( 'NONE', #74041 ) ;
#96775 = AXIS2_PLACEMENT_3D ( 'NONE', #86978, #11522, #22404 ) ;
#96776 = EDGE_CURVE ( 'NONE', #90432, #98765, #55567, .T. ) ;
#96777 = DIRECTION ( 'NONE',  ( -0.6830127018922180770, -0.6830127018922204085, -0.2588190451025213501 ) ) ;
#96779 = ORIENTED_EDGE ( 'NONE', *, *, #30153, .F. ) ;
#96778 = PLANE ( 'NONE',  #30371 ) ;
#96780 = VECTOR ( 'NONE', #30782, 1000.000000000000000 ) ;
#96781 = DIRECTION ( 'NONE',  ( 1.000000000000000000, 0.000000000000000000, 0.000000000000000000 ) ) ;
#96782 = CARTESIAN_POINT ( 'NONE',  ( -60.18398860626900415, 28.73617430169829490, 5.000000000000000000 ) ) ;
#96783 = CARTESIAN_POINT ( 'NONE',  ( 181.1500000000000057, -43.14999999999999147, -40.92499999999998295 ) ) ;
#96785 = EDGE_CURVE ( 'NONE', #107216, #74602, #129124, .T. ) ;
#96784 = EDGE_CURVE ( 'NONE', #29835, #66621, #44561, .T. ) ;
#96786 = EDGE_CURVE ( 'NONE', #77009, #102711, #84909, .T. ) ;
#96787 = ORIENTED_EDGE ( 'NONE', *, *, #59713, .F. ) ;
#96788 = VERTEX_POINT ( 'NONE', #99141 ) ;
#96789 = CARTESIAN_POINT ( 'NONE',  ( 1.353980332882009252, -0.4000000000000004108, 2.467792535850613866 ) ) ;
#96790 = CARTESIAN_POINT ( 'NONE',  ( -14.99999999999989519, -2.904428200921318481, -6.989807076074906256 ) ) ;
#96791 = VECTOR ( 'NONE', #128147, 1000.000000000000227 ) ;
#96792 = VECTOR ( 'NONE', #126003, 1000.000000000000000 ) ;
#96793 = CARTESIAN_POINT ( 'NONE',  ( 32.99999999999977263, 18.08204922493375832, 0.9627537363044108565 ) ) ;
#96794 = ADVANCED_FACE ( 'NONE', ( #29802 ), #32503, .F. ) ;
#96796 = ADVANCED_FACE ( 'NONE', ( #76737 ), #11408, .F. ) ;
#96795 = CARTESIAN_POINT ( 'NONE',  ( 82.47502705046287019, -5.819803920172572198, 5.819803920172572198 ) ) ;
#96797 = LINE ( 'NONE', #8360, #4552 ) ;
#96798 = DIRECTION ( 'NONE',  ( 0.7071067811865487940, 0.7071067811865463515, 0.000000000000000000 ) ) ;
#96800 = EDGE_CURVE ( 'NONE', #115116, #90399, #117512, .T. ) ;
#96799 = ORIENTED_EDGE ( 'NONE', *, *, #137261, .F. ) ;
#96801 = CARTESIAN_POINT ( 'NONE',  ( -25.39999999999996305, 3.061616997868383141E-16, -2.500000000000000000 ) ) ;
#96802 = EDGE_CURVE ( 'NONE', #12209, #14811, #106632, .T. ) ;
#96803 = DIRECTION ( 'NONE',  ( -0.7071067811865487940, 0.7071067811865463515, 0.000000000000000000 ) ) ;
#96804 = CARTESIAN_POINT ( 'NONE',  ( 33.83333333333333570, 5.278424836066143655, -3.047499999999997655 ) ) ;
#96805 = VECTOR ( 'NONE', #21914, 1000.000000000000000 ) ;
#96806 = ADVANCED_FACE ( 'NONE', ( #20880 ), #101313, .F. ) ;
#96807 = ORIENTED_EDGE ( 'NONE', *, *, #19455, .T. ) ;
#96808 = DIRECTION ( 'NONE',  ( 0.7071067811865487940, -0.7071067811865463515, 0.000000000000000000 ) ) ;
#96810 = EDGE_LOOP ( 'NONE', ( #132319, #72849, #118167 ) ) ;
#96809 = EDGE_CURVE ( 'NONE', #70950, #4634, #14300, .T. ) ;
#96811 = CARTESIAN_POINT ( 'NONE',  ( 73.64626352523141861, -4.472830434245840259, 4.472830434245839371 ) ) ;
#96812 = CARTESIAN_POINT ( 'NONE',  ( -39.29974487139159578, -27.71228299555233576, 4.000000000000000000 ) ) ;
#96813 = CARTESIAN_POINT ( 'NONE',  ( 60.48921356237309510, -27.52281430457097500, 5.000000000000000000 ) ) ;
#96815 = ORIENTED_EDGE ( 'NONE', *, *, #98549, .T. ) ;
#96814 = VECTOR ( 'NONE', #97540, 1000.000000000000000 ) ;
#96816 = CARTESIAN_POINT ( 'NONE',  ( 6.722814304570563948, -21.72499999999999432, 5.000000000000000000 ) ) ;
#96817 = AXIS2_PLACEMENT_3D ( 'NONE', #139464, #128553, #63328 ) ;
#96818 = EDGE_CURVE ( 'NONE', #97623, #131861, #36760, .T. ) ;
#96819 = DIRECTION ( 'NONE',  ( -0.000000000000000000, 0.000000000000000000, 1.000000000000000000 ) ) ;
#96820 = AXIS2_PLACEMENT_3D ( 'NONE', #78965, #23083, #34019 ) ;
#96821 = CARTESIAN_POINT ( 'NONE',  ( 3.812461875839446623, -22.22500000000000142, 4.000000000000000000 ) ) ;
#96822 = CARTESIAN_POINT ( 'NONE',  ( 12.35051985313232237, 4.584330080086930965E-16, 0.000000000000000000 ) ) ;
#96824 = VERTEX_POINT ( 'NONE', #3402 ) ;
#96823 = CARTESIAN_POINT ( 'NONE',  ( -30.48921356237309510, -27.52281430457076894, 5.000000000000000000 ) ) ;
#96825 = DIRECTION ( 'NONE',  ( 0.6830127018922180770, -0.6830127018922204085, -0.2588190451025213501 ) ) ;
#96826 = PLANE ( 'NONE',  #105509 ) ;
#96827 = LINE ( 'NONE', #64978, #21658 ) ;
#96828 = EDGE_CURVE ( 'NONE', #21420, #16508, #1261, .T. ) ;
#96829 = DIRECTION ( 'NONE',  ( -0.7071067811865486830, -0.7071067811865464625, 0.000000000000000000 ) ) ;
#96830 = VERTEX_POINT ( 'NONE', #113606 ) ;
#96831 = VERTEX_POINT ( 'NONE', #58587 ) ;
#96832 = CARTESIAN_POINT ( 'NONE',  ( 74.95876352523143282, 0.000000000000000000, -6.110000000000001208 ) ) ;
#96833 = VERTEX_POINT ( 'NONE', #13563 ) ;
#96834 = FACE_OUTER_BOUND ( 'NONE', #66217, .T. ) ;
#96835 = DIRECTION ( 'NONE',  ( 0.000000000000000000, 1.000000000000000000, 0.000000000000000000 ) ) ;
#96836 = CARTESIAN_POINT ( 'NONE',  ( 11.81601139373100651, 28.73617430169779041, 5.000000000000000000 ) ) ;
#96837 = DIRECTION ( 'NONE',  ( 0.5735764363510444941, 0.8191520442889929088, 0.000000000000000000 ) ) ;
#96838 = VERTEX_POINT ( 'NONE', #136795 ) ;
#96839 = VECTOR ( 'NONE', #50757, 1000.000000000000000 ) ;
#96840 = CARTESIAN_POINT ( 'NONE',  ( 22.98012225071438408, -17.24070752338410628, 20.23474786156474892 ) ) ;
#96841 = DIRECTION ( 'NONE',  ( 0.000000000000000000, -1.000000000000000000, 0.000000000000000000 ) ) ;
#96842 = COLOUR_RGB ( '', 0.09019608, 0.27058824, 0.51372549) ;
#96843 = EDGE_CURVE ( 'NONE', #73204, #56643, #83486, .T. ) ;
#96844 = VERTEX_POINT ( 'NONE', #102756 ) ;
#96845 = CARTESIAN_POINT ( 'NONE',  ( -9.489213562373095101, -27.52281430457062328, 5.000000000000000000 ) ) ;
#96846 = ADVANCED_FACE ( 'NONE', ( #103432 ), #47693, .F. ) ;
#96847 = DIRECTION ( 'NONE',  ( -0.7071067811865486830, -0.7071067811865464625, 0.000000000000000000 ) ) ;
#96848 = CARTESIAN_POINT ( 'NONE',  ( -29.29298673570674794, -21.74070752338405299, 4.999753212805210012 ) ) ;
#96849 = EDGE_CURVE ( 'NONE', #12864, #32966, #125936, .T. ) ;
#96850 = ORIENTED_EDGE ( 'NONE', *, *, #51564, .T. ) ;
#96851 = ORIENTED_EDGE ( 'NONE', *, *, #120799, .F. ) ;
#96852 = FACE_BOUND ( 'NONE', #101465, .T. ) ;
#96853 = DIRECTION ( 'NONE',  ( 0.7071067811865486830, -0.7071067811865464625, -0.000000000000000000 ) ) ;
#96854 = CARTESIAN_POINT ( 'NONE',  ( 128.0136022459138303, -6.349999999999999645, -3.888253587292846081E-16 ) ) ;
#96855 = DIRECTION ( 'NONE',  ( -1.000000000000000000, -1.224606353822377258E-16, -0.000000000000000000 ) ) ;
#96856 = FACE_OUTER_BOUND ( 'NONE', #31239, .T. ) ;
#96857 = EDGE_CURVE ( 'NONE', #76475, #41073, #46998, .T. ) ;
#96858 = LINE ( 'NONE', #53392, #41926 ) ;
#96859 = ORIENTED_EDGE ( 'NONE', *, *, #30710, .F. ) ;
#96860 = ORIENTED_EDGE ( 'NONE', *, *, #105798, .F. ) ;
#96861 = ORIENTED_EDGE ( 'NONE', *, *, #109373, .F. ) ;
#96862 = ADVANCED_FACE ( 'NONE', ( #81010 ), #125213, .F. ) ;
#96863 = ORIENTED_EDGE ( 'NONE', *, *, #86610, .T. ) ;
#96864 = SURFACE_SIDE_STYLE ('',( #9888 ) ) ;
#96865 = CARTESIAN_POINT ( 'NONE',  ( -72.18398860626899705, 28.73617430169837661, 5.000000000000000000 ) ) ;
#96866 = DIRECTION ( 'NONE',  ( -0.7071067811865487940, 0.7071067811865463515, -0.000000000000000000 ) ) ;
#96867 = ORIENTED_EDGE ( 'NONE', *, *, #61857, .T. ) ;
#96868 = CARTESIAN_POINT ( 'NONE',  ( 68.32919371712955581, -3.975000000000001865, 6.884901960086284411 ) ) ;
#96869 = CARTESIAN_POINT ( 'NONE',  ( 25.49999999999982947, -7.912538124160678699, 4.000000000000000000 ) ) ;
#96870 = VECTOR ( 'NONE', #843, 1000.000000000000227 ) ;
#96871 = EDGE_CURVE ( 'NONE', #64975, #134832, #37507, .T. ) ;
#96872 = CARTESIAN_POINT ( 'NONE',  ( 58.41252705046289151, -7.949999999999998401, -4.867971026610728450E-16 ) ) ;
#96873 = CARTESIAN_POINT ( 'NONE',  ( -5.816011393731002066, 28.73617430169783304, 5.000000000000000000 ) ) ;
#96874 = VECTOR ( 'NONE', #114381, 1000.000000000000000 ) ;
#96875 = VECTOR ( 'NONE', #80943, 1000.000000000000000 ) ;
#96876 = LINE ( 'NONE', #54867, #39851 ) ;
#96877 = ORIENTED_EDGE ( 'NONE', *, *, #97822, .F. ) ;
#96878 = CARTESIAN_POINT ( 'NONE',  ( 38.91508676806214595, -12.74070752338415247, 18.74364270924363396 ) ) ;
#96879 = PLANE ( 'NONE',  #67445 ) ;
#96880 = AXIS2_PLACEMENT_3D ( 'NONE', #116169, #105286, #5940 ) ;
#96881 = VERTEX_POINT ( 'NONE', #4076 ) ;
#96883 = ADVANCED_FACE ( 'NONE', ( #92554 ), #91185, .T. ) ;
#96882 = CARTESIAN_POINT ( 'NONE',  ( -24.99033360189226372, 3.759292476615678336, 4.478963035907990609 ) ) ;
#96884 = EDGE_LOOP ( 'NONE', ( #123143, #18906, #70452, #92452 ) ) ;
#96885 = VERTEX_POINT ( 'NONE', #100614 ) ;
#96886 = ORIENTED_EDGE ( 'NONE', *, *, #77730, .F. ) ;
#96887 = EDGE_CURVE ( 'NONE', #45259, #129569, #35384, .T. ) ;
#96888 = CARTESIAN_POINT ( 'NONE',  ( 65.33376352523143282, 6.110000000000001208, 1.122388791418549305E-15 ) ) ;
#96889 = AXIS2_PLACEMENT_3D ( 'NONE', #62366, #139221, #6483 ) ;
#96890 = ORIENTED_EDGE ( 'NONE', *, *, #126927, .T. ) ;
#96891 = VERTEX_POINT ( 'NONE', #34638 ) ;
#96892 = AXIS2_PLACEMENT_3D ( 'NONE', #52004, #49879, #94061 ) ;
#96893 = CARTESIAN_POINT ( 'NONE',  ( -34.17183060077622514, -5.240707523384232402, 4.000000000000000000 ) ) ;
#96894 = ADVANCED_FACE ( 'NONE', ( #78875 ), #123083, .F. ) ;
#96895 = CARTESIAN_POINT ( 'NONE',  ( 103.5420968585647756, 5.291415217122923842, -3.054999999999996163 ) ) ;
#96896 = CARTESIAN_POINT ( 'NONE',  ( 19.61351471301484395, 9.118430946277904070, 4.525620927308371400 ) ) ;
#96897 = DIRECTION ( 'NONE',  ( 0.7071067811865487940, 0.7071067811865463515, -0.000000000000000000 ) ) ;
#96898 = EDGE_LOOP ( 'NONE', ( #112410, #122542, #68635, #3878 ) ) ;
#96899 = DIRECTION ( 'NONE',  ( -0.7071067811865486830, -0.7071067811865464625, 0.000000000000000000 ) ) ;
#96900 = DIRECTION ( 'NONE',  ( 0.7071067811865487940, 0.7071067811865463515, 0.000000000000000000 ) ) ;
#96901 = EDGE_CURVE ( 'NONE', #65140, #105391, #46259, .T. ) ;
#96902 = FACE_OUTER_BOUND ( 'NONE', #74054, .T. ) ;
#96903 = DIRECTION ( 'NONE',  ( 0.000000000000000000, -1.000000000000000000, 0.000000000000000000 ) ) ;
#96904 = EDGE_LOOP ( 'NONE', ( #121365, #8013, #73945, #97911, #74821, #136315 ) ) ;
#96905 = AXIS2_PLACEMENT_3D ( 'NONE', #127317, #28019, #37480 ) ;
#96906 = EDGE_CURVE ( 'NONE', #121985, #88187, #36080, .T. ) ;
#96907 = ORIENTED_EDGE ( 'NONE', *, *, #20668, .F. ) ;
#96908 = ORIENTED_EDGE ( 'NONE', *, *, #22179, .F. ) ;
#96909 = ORIENTED_EDGE ( 'NONE', *, *, #42969, .T. ) ;
#96910 = CARTESIAN_POINT ( 'NONE',  ( 125.1829301918981372, -1.637169565754158951, -6.109999999999998543 ) ) ;
#96911 = AXIS2_PLACEMENT_3D ( 'NONE', #120320, #97906, #31930 ) ;
#96912 = ORIENTED_EDGE ( 'NONE', *, *, #112028, .F. ) ;
#96913 = VECTOR ( 'NONE', #8727, 1000.000000000000227 ) ;
#96914 = VECTOR ( 'NONE', #28172, 1000.000000000000000 ) ;
#96915 = DIRECTION ( 'NONE',  ( 1.000000000000000000, 0.000000000000000000, 0.000000000000000000 ) ) ;
#96916 = DIRECTION ( 'NONE',  ( 0.7071067811865487940, 0.7071067811865463515, 0.000000000000000000 ) ) ;
#96917 = VECTOR ( 'NONE', #70119, 1000.000000000000227 ) ;
#96918 = CARTESIAN_POINT ( 'NONE',  ( -36.18398860626899705, 28.73617430169812437, 5.000000000000000000 ) ) ;
#96919 = EDGE_CURVE ( 'NONE', #97698, #88226, #64776, .T. ) ;
#96920 = ORIENTED_EDGE ( 'NONE', *, *, #95368, .T. ) ;
#96921 = CARTESIAN_POINT ( 'NONE',  ( 0.3339215173232504275, -51.89584459748879652, 39.24672819827910786 ) ) ;
#96922 = ORIENTED_EDGE ( 'NONE', *, *, #117154, .F. ) ;
#96923 = AXIS2_PLACEMENT_3D ( 'NONE', #68178, #124641, #79038 ) ;
#96924 = VECTOR ( 'NONE', #91095, 1000.000000000000000 ) ;
#96925 = CARTESIAN_POINT ( 'NONE',  ( 1.145403141435219263, -2.126176841940958351, -7.934999999999989839 ) ) ;
#96926 = LINE ( 'NONE', #76674, #48388 ) ;
#96927 = DIRECTION ( 'NONE',  ( 0.5735764363510451602, 0.8191520442889924647, 0.000000000000000000 ) ) ;
#96928 = VERTEX_POINT ( 'NONE', #15681 ) ;
#96929 = EDGE_LOOP ( 'NONE', ( #69831, #8555, #51723, #29138, #26571 ) ) ;
#96930 = ORIENTED_EDGE ( 'NONE', *, *, #55216, .F. ) ;
#96931 = DIRECTION ( 'NONE',  ( -0.000000000000000000, 0.000000000000000000, 1.000000000000000000 ) ) ;
#96932 = LINE ( 'NONE', #118715, #141299 ) ;
#96933 = VECTOR ( 'NONE', #140992, 999.9999999999998863 ) ;
#96934 = FACE_OUTER_BOUND ( 'NONE', #125120, .T. ) ;
#96935 = DIRECTION ( 'NONE',  ( -1.000000000000000000, -1.224606353822377258E-16, -0.000000000000000000 ) ) ;
#96936 = DIRECTION ( 'NONE',  ( 0.7071067811865487940, 0.7071067811865463515, 0.000000000000000000 ) ) ;
#96937 = CARTESIAN_POINT ( 'NONE',  ( 11.99999999999991296, -19.06887692260762179, 4.000000000000000000 ) ) ;
#96938 = CARTESIAN_POINT ( 'NONE',  ( 34.27126352523143993, 4.472830434245839371, 4.472830434245842035 ) ) ;
#96939 = LINE ( 'NONE', #72426, #115796 ) ;
#96940 = CARTESIAN_POINT ( 'NONE',  ( 0.000000000000000000, 60.00000000000000000, 0.000000000000000000 ) ) ;
#96941 = VERTEX_POINT ( 'NONE', #93294 ) ;
#96942 = DIRECTION ( 'NONE',  ( -0.7071067811865486830, -0.7071067811865464625, -0.000000000000000000 ) ) ;
#96943 = CARTESIAN_POINT ( 'NONE',  ( -21.71238017851530344, 8.518175273744141407, 4.330735335516833651 ) ) ;
#96944 = ORIENTED_EDGE ( 'NONE', *, *, #91628, .F. ) ;
#96945 = LINE ( 'NONE', #129608, #113094 ) ;
#96947 = ORIENTED_EDGE ( 'NONE', *, *, #104560, .F. ) ;
#96946 = DIRECTION ( 'NONE',  ( 0.000000000000000000, 0.000000000000000000, 1.000000000000000000 ) ) ;
#96948 = PLANE ( 'NONE',  #139471 ) ;
#96949 = ORIENTED_EDGE ( 'NONE', *, *, #56688, .F. ) ;
#96950 = DIRECTION ( 'NONE',  ( -0.6830127018922181881, 0.6830127018922202975, -0.2588190451025214056 ) ) ;
#96951 = ORIENTED_EDGE ( 'NONE', *, *, #45348, .T. ) ;
#96952 = LINE ( 'NONE', #29585, #46684 ) ;
#96953 = UNCERTAINTY_MEASURE_WITH_UNIT (LENGTH_MEASURE( 1.000000000000000082E-05 ), #67876, 'distance_accuracy_value', 'NONE');
#96954 = ORIENTED_EDGE ( 'NONE', *, *, #10153, .F. ) ;
#96955 = CARTESIAN_POINT ( 'NONE',  ( 92.68336038379624142, -2.130196079827426203, 7.949999999999996625 ) ) ;
#96957 = EDGE_CURVE ( 'NONE', #8723, #121754, #138229, .T. ) ;
#96956 = CARTESIAN_POINT ( 'NONE',  ( 125.7875270504628986, 0.000000000000000000, -7.949999999999998401 ) ) ;
#96958 = CARTESIAN_POINT ( 'NONE',  ( 0.000000000000000000, 7.007997736742450634, -8.085015511992116544 ) ) ;
#96959 = DIRECTION ( 'NONE',  ( -0.7071067811865486830, -0.7071067811865464625, 0.000000000000000000 ) ) ;
#96960 = EDGE_CURVE ( 'NONE', #34275, #25809, #129521, .T. ) ;
#96961 = PLANE ( 'NONE',  #127830 ) ;
#96962 = CARTESIAN_POINT ( 'NONE',  ( 1.180000000000000826, -6.391994993740215847, 10.00000000000000000 ) ) ;
#96963 = EDGE_CURVE ( 'NONE', #74781, #91404, #5547, .T. ) ;
#96964 = LINE ( 'NONE', #74561, #66968 ) ;
#96965 = CARTESIAN_POINT ( 'NONE',  ( 6.125000000000000000, 6.094999999999989981, -1.119633336120465690E-15 ) ) ;
#96966 = CARTESIAN_POINT ( 'NONE',  ( 15.72873647476855297, 5.808823158059031044, -5.808823158059037262 ) ) ;
#96967 = FACE_OUTER_BOUND ( 'NONE', #45363, .T. ) ;
#96969 = ADVANCED_FACE ( 'NONE', ( #28767 ), #140362, .F. ) ;
#96968 = FACE_OUTER_BOUND ( 'NONE', #78977, .T. ) ;
#96970 = EDGE_LOOP ( 'NONE', ( #24373, #45458, #31485, #65783 ) ) ;
#96971 = ORIENTED_EDGE ( 'NONE', *, *, #130448, .T. ) ;
#96972 = CARTESIAN_POINT ( 'NONE',  ( -12.20000000000000462, -25.33999999999998565, 2.999999999999999112 ) ) ;
#96973 = ORIENTED_EDGE ( 'NONE', *, *, #81629, .F. ) ;
#96974 = EDGE_CURVE ( 'NONE', #20610, #79882, #4652, .T. ) ;
#96975 = LINE ( 'NONE', #141983, #73518 ) ;
#96976 = DIRECTION ( 'NONE',  ( -0.3543493200069162685, -0.000000000000000000, -0.9351131265310288487 ) ) ;
#96977 = CARTESIAN_POINT ( 'NONE',  ( 128.5740698622078071, -49.04047092356724136, -39.41690992498752877 ) ) ;
#96978 = ORIENTED_EDGE ( 'NONE', *, *, #121526, .F. ) ;
#96979 = AXIS2_PLACEMENT_3D ( 'NONE', #73575, #117745, #85145 ) ;
#96980 = VECTOR ( 'NONE', #16179, 1000.000000000000000 ) ;
#96981 = AXIS2_PLACEMENT_3D ( 'NONE', #116308, #127174, #72862 ) ;
#96982 = FACE_OUTER_BOUND ( 'NONE', #81277, .T. ) ;
#96983 = AXIS2_PLACEMENT_3D ( 'NONE', #50735, #117380, #39148 ) ;
#96984 = ADVANCED_FACE ( 'NONE', ( #26609 ), #128773, .F. ) ;
#96985 = CARTESIAN_POINT ( 'NONE',  ( 92.14583333333334281, 2.130196079827431976, -7.949999999999998401 ) ) ;
#96986 = EDGE_CURVE ( 'NONE', #101708, #138040, #38916, .T. ) ;
#96988 = ORIENTED_EDGE ( 'NONE', *, *, #63591, .T. ) ;
#96987 = CARTESIAN_POINT ( 'NONE',  ( 42.18398860626899705, 28.73617430169816700, 5.000000000000000000 ) ) ;
#96989 = CARTESIAN_POINT ( 'NONE',  ( 39.64583333333332149, 2.130196079827356037, -7.950000000000043698 ) ) ;
#96990 = FACE_OUTER_BOUND ( 'NONE', #57557, .T. ) ;
#96991 = DIRECTION ( 'NONE',  ( -0.3543493200069162685, -0.000000000000000000, -0.9351131265310288487 ) ) ;
#96992 = VECTOR ( 'NONE', #129797, 999.9999999999998863 ) ;
#96993 = EDGE_CURVE ( 'NONE', #20187, #68937, #16414, .T. ) ;
#96994 = CARTESIAN_POINT ( 'NONE',  ( 59.70964273383167153, -44.90675832753628782, 35.11767176072511631 ) ) ;
#96995 = EDGE_LOOP ( 'NONE', ( #47751, #114575, #135129, #13459 ) ) ;
#96996 = VERTEX_POINT ( 'NONE', #6947 ) ;
#96997 = ORIENTED_EDGE ( 'NONE', *, *, #132572, .T. ) ;
#96998 = CARTESIAN_POINT ( 'NONE',  ( 101.9379301918980900, -6.110000000000001208, 1.637169565754158951 ) ) ;
#96999 = ORIENTED_EDGE ( 'NONE', *, *, #47476, .T. ) ;
#97000 = CARTESIAN_POINT ( 'NONE',  ( 127.5247579190790219, -47.99115898043997674, 37.22402166429051817 ) ) ;
#97001 = VECTOR ( 'NONE', #100039, 1000.000000000000000 ) ;
#97002 = LINE ( 'NONE', #86898, #47819 ) ;
#97003 = ORIENTED_EDGE ( 'NONE', *, *, #22569, .T. ) ;
#97004 = CARTESIAN_POINT ( 'NONE',  ( 75.37500000000000000, 7.950000000000000178, 1.460391307983218535E-15 ) ) ;
#97005 = PLANE ( 'NONE',  #41983 ) ;
#97006 = AXIS2_PLACEMENT_3D ( 'NONE', #74949, #41561, #30723 ) ;
#97007 = CARTESIAN_POINT ( 'NONE',  ( 95.72459685856476597, -1.637169565754160949, 6.109999999999997655 ) ) ;
#97008 = ORIENTED_EDGE ( 'NONE', *, *, #114929, .T. ) ;
#97009 = CARTESIAN_POINT ( 'NONE',  ( -5.292893218813415679, 14.25929247661557575, 5.000000000000000000 ) ) ;
#97011 = EDGE_CURVE ( 'NONE', #80483, #72728, #83138, .T. ) ;
#97010 = LINE ( 'NONE', #118053, #131063 ) ;
#97012 = DIRECTION ( 'NONE',  ( -0.7071067811865486830, -0.7071067811865464625, -0.000000000000000000 ) ) ;
#97013 = AXIS2_PLACEMENT_3D ( 'NONE', #69251, #135919, #101137 ) ;
#97014 = DIRECTION ( 'NONE',  ( -0.7071067811865486830, -0.7071067811865464625, 0.000000000000000000 ) ) ;
#97015 = STYLED_ITEM ( 'NONE', ( #112691 ), #58768 ) ;
#97016 = VECTOR ( 'NONE', #113031, 1000.000000000000000 ) ;
#97017 = ORIENTED_EDGE ( 'NONE', *, *, #90193, .T. ) ;
#97018 = VERTEX_POINT ( 'NONE', #85255 ) ;
#97019 = ORIENTED_EDGE ( 'NONE', *, *, #18565, .F. ) ;
#97020 = CARTESIAN_POINT ( 'NONE',  ( 28.49999999999981171, 22.22500000000000142, 4.362957392718781691 ) ) ;
#97021 = DIRECTION ( 'NONE',  ( -0.6830127018922180770, -0.6830127018922204085, -0.2588190451025213501 ) ) ;
#97022 = CARTESIAN_POINT ( 'NONE',  ( 16.10873647476855552, -5.808823158059033709, 5.808823158059035485 ) ) ;
#97023 = VECTOR ( 'NONE', #73671, 999.9999999999998863 ) ;
#97024 = AXIS2_PLACEMENT_3D ( 'NONE', #12772, #122987, #23668 ) ;
#97025 = LINE ( 'NONE', #107222, #138228 ) ;
#97026 = ADVANCED_FACE ( 'NONE', ( #94695 ), #17167, .F. ) ;
#97027 = ORIENTED_EDGE ( 'NONE', *, *, #26787, .T. ) ;
#97028 = ORIENTED_EDGE ( 'NONE', *, *, #36449, .T. ) ;
#97029 = CARTESIAN_POINT ( 'NONE',  ( -25.39999999999996305, 3.061616997868383141E-16, -2.500000000000000000 ) ) ;
#97031 = ORIENTED_EDGE ( 'NONE', *, *, #125024, .F. ) ;
#97030 = EDGE_CURVE ( 'NONE', #128836, #10662, #40372, .T. ) ;
#97032 = ORIENTED_EDGE ( 'NONE', *, *, #30398, .F. ) ;
#97033 = VECTOR ( 'NONE', #35693, 1000.000000000000000 ) ;
#97034 = CARTESIAN_POINT ( 'NONE',  ( 0.000000000000000000, 0.000000000000000000, 5.000000000000000000 ) ) ;
#97035 = DIRECTION ( 'NONE',  ( 0.3543493200069162685, -0.000000000000000000, -0.9351131265310288487 ) ) ;
#97036 = ORIENTED_EDGE ( 'NONE', *, *, #86620, .F. ) ;
#97037 = CARTESIAN_POINT ( 'NONE',  ( 1.353980332882009252, -0.3999999999999997446, -2.467792535850613866 ) ) ;
#97038 = EDGE_CURVE ( 'NONE', #57193, #15218, #61430, .T. ) ;
#97039 = CARTESIAN_POINT ( 'NONE',  ( 11.99999999999992006, 10.93112307739207267, 4.000000000000000000 ) ) ;
#97040 = CARTESIAN_POINT ( 'NONE',  ( -29.99999999999979394, 12.83542986846994793, -1.025386466790300544 ) ) ;
#97041 = DIRECTION ( 'NONE',  ( -0.7071067811865486830, -0.7071067811865464625, 0.000000000000000000 ) ) ;
#97042 = ORIENTED_EDGE ( 'NONE', *, *, #104694, .F. ) ;
#97043 = VERTEX_POINT ( 'NONE', #138958 ) ;
#97044 = CARTESIAN_POINT ( 'NONE',  ( 25.40000000000000924, 5.606709230119133025, -5.629648409862730851 ) ) ;
#97046 = EDGE_CURVE ( 'NONE', #9024, #4889, #84575, .T. ) ;
#97045 = CARTESIAN_POINT ( 'NONE',  ( 16.27785539607886633, 4.584330080086930965E-16, 0.000000000000000000 ) ) ;
#97047 = ORIENTED_EDGE ( 'NONE', *, *, #27004, .F. ) ;
#97048 = CARTESIAN_POINT ( 'NONE',  ( -55.65468426143998215, -28.33999999999998565, 13.17925390838734323 ) ) ;
#97049 = ORIENTED_EDGE ( 'NONE', *, *, #61707, .F. ) ;
#97050 = DIRECTION ( 'NONE',  ( -1.000000000000000000, -0.000000000000000000, -0.000000000000000000 ) ) ;
#97051 = ORIENTED_EDGE ( 'NONE', *, *, #142023, .T. ) ;
#97052 = ORIENTED_EDGE ( 'NONE', *, *, #103897, .T. ) ;
#97053 = ORIENTED_EDGE ( 'NONE', *, *, #51233, .T. ) ;
#97054 = CARTESIAN_POINT ( 'NONE',  ( 28.93293019189811943, 1.637169565754156508, 6.110000000000000320 ) ) ;
#97055 = FACE_OUTER_BOUND ( 'NONE', #127919, .T. ) ;
#97056 = CARTESIAN_POINT ( 'NONE',  ( -4.828169399223493308, -5.240707523384230626, 4.000000000000000000 ) ) ;
#97057 =( NAMED_UNIT ( * ) PLANE_ANGLE_UNIT ( ) SI_UNIT ( $, .RADIAN. ) );
#97058 = DIRECTION ( 'NONE',  ( 0.3543493200069162685, -0.000000000000000000, -0.9351131265310288487 ) ) ;
#97059 = DIRECTION ( 'NONE',  ( -0.000000000000000000, 0.3543493200069153248, 0.9351131265310292928 ) ) ;
#97060 = CARTESIAN_POINT ( 'NONE',  ( 4.495848767239241539, 4.584330080086930965E-16, 0.000000000000000000 ) ) ;
#97061 = FACE_OUTER_BOUND ( 'NONE', #125168, .T. ) ;
#97062 = CARTESIAN_POINT ( 'NONE',  ( 5.999999999999956479, 12.25461709320621928, -10.07315571508695839 ) ) ;
#97063 = EDGE_CURVE ( 'NONE', #43532, #37108, #76564, .T. ) ;
#97064 = PLANE ( 'NONE',  #62180 ) ;
#97065 = CARTESIAN_POINT ( 'NONE',  ( 31.49999999999978684, 10.94296225409029510, -9.576120664313185316 ) ) ;
#97066 = EDGE_CURVE ( 'NONE', #25651, #39180, #41775, .T. ) ;
#97067 = ORIENTED_EDGE ( 'NONE', *, *, #4100, .T. ) ;
#97068 = EDGE_LOOP ( 'NONE', ( #119558, #37722, #28493, #42769 ) ) ;
#97069 = AXIS2_PLACEMENT_3D ( 'NONE', #68924, #1462, #100812 ) ;
#97070 = ORIENTED_EDGE ( 'NONE', *, *, #109907, .F. ) ;
#97071 = VERTEX_POINT ( 'NONE', #119308 ) ;
#97072 = CARTESIAN_POINT ( 'NONE',  ( -36.18398860626899705, 28.73617430169812437, 5.000000000000000000 ) ) ;
#97073 = CIRCLE ( 'NONE', #39301, 2.500000000000000444 ) ;
#97074 = VECTOR ( 'NONE', #122264, 1000.000000000000000 ) ;
#97075 = EDGE_LOOP ( 'NONE', ( #113097, #116742, #99207, #10536 ) ) ;
#97076 = AXIS2_PLACEMENT_3D ( 'NONE', #933, #17354, #89393 ) ;
#97078 = ORIENTED_EDGE ( 'NONE', *, *, #36289, .F. ) ;
#97077 = VECTOR ( 'NONE', #50558, 999.9999999999998863 ) ;
#97079 = DIRECTION ( 'NONE',  ( -0.7071067811865486830, -0.7071067811865464625, 0.000000000000000000 ) ) ;
#97080 = DIRECTION ( 'NONE',  ( -1.000000000000000000, -1.224606353822377258E-16, -0.000000000000000000 ) ) ;
#97081 = EDGE_CURVE ( 'NONE', #129291, #42695, #43921, .T. ) ;
#97082 = ADVANCED_FACE ( 'NONE', ( #63559 ), #73982, .T. ) ;
#97083 = DIRECTION ( 'NONE',  ( -0.6830127018922180770, -0.6830127018922204085, -0.2588190451025213501 ) ) ;
#97084 = VERTEX_POINT ( 'NONE', #32330 ) ;
#97085 = CARTESIAN_POINT ( 'NONE',  ( 21.18398860626899349, 28.73617430169802134, 5.000000000000000000 ) ) ;
#97087 = ORIENTED_EDGE ( 'NONE', *, *, #136436, .T. ) ;
#97086 = AXIS2_PLACEMENT_3D ( 'NONE', #19441, #52766, #120884 ) ;
#97088 = SURFACE_STYLE_USAGE ( .BOTH. , #64507 ) ;
#97089 = LINE ( 'NONE', #120273, #70519 ) ;
#97091 = VECTOR ( 'NONE', #93051, 1000.000000000000227 ) ;
#97090 = CARTESIAN_POINT ( 'NONE',  ( 13.62956980810188767, -3.967499999999998028, -6.871911579029511330 ) ) ;
#97092 = ORIENTED_EDGE ( 'NONE', *, *, #64493, .T. ) ;
#97093 = CARTESIAN_POINT ( 'NONE',  ( 94.55793019189810877, 6.110000000000001208, -1.637169565754156286 ) ) ;
#97094 = DIRECTION ( 'NONE',  ( 0.7071067811865487940, -0.7071067811865463515, 0.000000000000000000 ) ) ;
#97095 = CARTESIAN_POINT ( 'NONE',  ( 52.26932219902319332, -49.14999999999999147, -40.92499999999997584 ) ) ;
#97096 = DIRECTION ( 'NONE',  ( 0.000000000000000000, -1.000000000000000000, 0.000000000000000000 ) ) ;
#97097 = EDGE_LOOP ( 'NONE', ( #124625, #74151, #116572, #116078 ) ) ;
#97098 = ORIENTED_EDGE ( 'NONE', *, *, #29222, .F. ) ;
#97099 = FACE_OUTER_BOUND ( 'NONE', #18627, .T. ) ;
#97100 = EDGE_LOOP ( 'NONE', ( #51101, #112818, #124731, #93001 ) ) ;
#97101 = CIRCLE ( 'NONE', #134208, 2.500000000000000444 ) ;
#97102 = CARTESIAN_POINT ( 'NONE',  ( 174.7500000000000000, 7.919999999999947526, -18.97500000000001918 ) ) ;
#97103 = PLANE ( 'NONE',  #139570 ) ;
#97104 = DIRECTION ( 'NONE',  ( -0.3543493200069162685, -0.000000000000000000, -0.9351131265310288487 ) ) ;
#97105 = EDGE_CURVE ( 'NONE', #12477, #48215, #76366, .T. ) ;
#97106 = ORIENTED_EDGE ( 'NONE', *, *, #25554, .T. ) ;
#97107 = CARTESIAN_POINT ( 'NONE',  ( 6.489213562373093325, -27.52281430457059841, 5.000000000000000000 ) ) ;
#97108 = COLOUR_RGB ( '', 0.08235294, 0.09019608, 0.10196078) ;
#97109 = CARTESIAN_POINT ( 'NONE',  ( 30.70710678118633297, 20.25929247661551713, 5.000000000000000000 ) ) ;
#97110 = FACE_OUTER_BOUND ( 'NONE', #93747, .T. ) ;
#97111 = EDGE_LOOP ( 'NONE', ( #30335, #19513, #119574, #68540, #109404 ) ) ;
#97112 = DIRECTION ( 'NONE',  ( -0.7071067811865486830, -0.7071067811865464625, 0.000000000000000000 ) ) ;
#97113 = VECTOR ( 'NONE', #119150, 1000.000000000000227 ) ;
#97115 = PRESENTATION_LAYER_ASSIGNMENT (  '', '', ( #108712 ) ) ;
#97114 = PLANE ( 'NONE',  #3022 ) ;
#97116 = VERTEX_POINT ( 'NONE', #118605 ) ;
#97117 = AXIS2_PLACEMENT_3D ( 'NONE', #42657, #97715, #9229 ) ;
#97119 = ORIENTED_EDGE ( 'NONE', *, *, #30942, .T. ) ;
#97118 = DIRECTION ( 'NONE',  ( -0.7071067811865486830, -0.7071067811865464625, 0.000000000000000000 ) ) ;
#97120 = ORIENTED_EDGE ( 'NONE', *, *, #139423, .T. ) ;
#97121 = VECTOR ( 'NONE', #58111, 1000.000000000000000 ) ;
#97122 = DIRECTION ( 'NONE',  ( -0.000000000000000000, -0.3543493200069152693, 0.9351131265310292928 ) ) ;
#97123 = VECTOR ( 'NONE', #103255, 1000.000000000000000 ) ;
#97124 = DIRECTION ( 'NONE',  ( 1.000000000000000000, 0.000000000000000000, 0.000000000000000000 ) ) ;
#97125 = ORIENTED_EDGE ( 'NONE', *, *, #64689, .F. ) ;
#97126 = FACE_OUTER_BOUND ( 'NONE', #131843, .T. ) ;
#97127 = CARTESIAN_POINT ( 'NONE',  ( -29.20710678118632586, -14.24070752338413648, 5.000000000000000000 ) ) ;
#97128 = EDGE_CURVE ( 'NONE', #124871, #31809, #141066, .T. ) ;
#97129 = FACE_OUTER_BOUND ( 'NONE', #128742, .T. ) ;
#97130 = B_SPLINE_CURVE_WITH_KNOTS ( 'NONE', 3,
 ( #106538, #107959, #42052, #86267, #130487, #61668, #28315, #72574, #39926, #6490, #84143, #29016, #117416, #73250 ),
 .UNSPECIFIED., .F., .F.,
 ( 4, 2, 2, 2, 2, 2, 4 ),
 ( 0.004158817918585050455, 0.004678504169777139392, 0.004938347295373183427, 0.005198190420969228329, 0.005717876672161316398, 0.005977719797757361300, 0.006237562923353405335 ),
 .UNSPECIFIED. ) ;
#97131 = CARTESIAN_POINT ( 'NONE',  ( -21.29974487139158512, -27.71228299555221142, 4.000000000000000000 ) ) ;
#97132 = EDGE_CURVE ( 'NONE', #95686, #18692, #132385, .T. ) ;
#97133 = CARTESIAN_POINT ( 'NONE',  ( 31.91666666666666430, -6.884901960086287076, -3.975000000000000977 ) ) ;
#97134 = CARTESIAN_POINT ( 'NONE',  ( 12.06011071044012439, -9.740707523384180888, 10.89222023123378058 ) ) ;
#97135 = DIRECTION ( 'NONE',  ( -1.000000000000000000, -1.224606353822377258E-16, -0.000000000000000000 ) ) ;
#97136 = PLANE ( 'NONE',  #66866 ) ;
#97138 = AXIS2_PLACEMENT_3D ( 'NONE', #89517, #122861, #131608 ) ;
#97137 = CARTESIAN_POINT ( 'NONE',  ( -24.70710678118637560, 14.25929247661557753, 5.000000000000000000 ) ) ;
#97139 = DIRECTION ( 'NONE',  ( -0.7071067811865487940, 0.7071067811865463515, -0.000000000000000000 ) ) ;
#97140 = DIRECTION ( 'NONE',  ( -0.7071067811865487940, 0.7071067811865463515, 0.000000000000000000 ) ) ;
#97141 = DIRECTION ( 'NONE',  ( -0.7071067811865486830, -0.7071067811865464625, -0.000000000000000000 ) ) ;
#97143 = EDGE_CURVE ( 'NONE', #15589, #106919, #20513, .T. ) ;
#97142 = DIRECTION ( 'NONE',  ( -0.7071067811865486830, -0.7071067811865464625, -0.000000000000000000 ) ) ;
#97145 = EDGE_CURVE ( 'NONE', #36373, #11113, #97563, .T. ) ;
#97144 = VERTEX_POINT ( 'NONE', #9086 ) ;
#97146 = VERTEX_POINT ( 'NONE', #31614 ) ;
#97147 = EDGE_LOOP ( 'NONE', ( #207, #54393, #70391, #116718, #87744 ) ) ;
#97148 = CARTESIAN_POINT ( 'NONE',  ( 106.2916666666666714, 3.975000000000003642, -6.884901960086285300 ) ) ;
#97149 = ORIENTED_EDGE ( 'NONE', *, *, #78454, .F. ) ;
#97150 = ORIENTED_EDGE ( 'NONE', *, *, #138670, .F. ) ;
#97151 = VERTEX_POINT ( 'NONE', #96821 ) ;
#97152 = CARTESIAN_POINT ( 'NONE',  ( 15.79076468313838433, 8.175634574663693144, 5.000000000000000000 ) ) ;
#97153 = DIRECTION ( 'NONE',  ( -0.7071067811865486830, -0.7071067811865464625, -0.000000000000000000 ) ) ;
#97154 = VERTEX_POINT ( 'NONE', #98985 ) ;
#97155 = DIRECTION ( 'NONE',  ( 0.7071067811865487940, 0.7071067811865463515, 0.000000000000000000 ) ) ;
#97156 = CARTESIAN_POINT ( 'NONE',  ( -30.32816939922332367, 11.25929247661560950, 4.000000000000000000 ) ) ;
#97157 = EDGE_CURVE ( 'NONE', #6537, #140758, #8380, .T. ) ;
#97158 = DIRECTION ( 'NONE',  ( -0.000000000000000000, -0.3543493200069152693, 0.9351131265310292928 ) ) ;
#97159 = DIRECTION ( 'NONE',  ( -0.6830127018922180770, -0.6830127018922204085, -0.2588190451025213501 ) ) ;
#97160 = CARTESIAN_POINT ( 'NONE',  ( 107.0420968585647756, 5.291415217122923842, -3.054999999999996163 ) ) ;
#97161 = ORIENTED_EDGE ( 'NONE', *, *, #79908, .T. ) ;
#97162 = EDGE_CURVE ( 'NONE', #107216, #22385, #110563, .T. ) ;
#97163 = CARTESIAN_POINT ( 'NONE',  ( 11.60152521092712341, 8.206876333263409151, -30.11676755377419568 ) ) ;
#97164 = LINE ( 'NONE', #63193, #24176 ) ;
#97165 = LINE ( 'NONE', #121793, #128519 ) ;
#97166 = PLANE ( 'NONE',  #72405 ) ;
#97167 = DIRECTION ( 'NONE',  ( 0.7071067811865487940, 0.7071067811865463515, 0.000000000000000000 ) ) ;
#97168 = CARTESIAN_POINT ( 'NONE',  ( 28.80836038379621655, 7.949999999999997513, 2.130196079827431088 ) ) ;
#97169 = EDGE_CURVE ( 'NONE', #57216, #31488, #86718, .T. ) ;
#97170 = DIRECTION ( 'NONE',  ( -0.7071067811865487940, 0.7071067811865463515, 0.000000000000000000 ) ) ;
#97171 = ORIENTED_EDGE ( 'NONE', *, *, #33163, .F. ) ;
#97172 = ORIENTED_EDGE ( 'NONE', *, *, #32611, .F. ) ;
#97173 = CARTESIAN_POINT ( 'NONE',  ( 29.29166666666666075, 3.975000000000003642, -6.884901960086285300 ) ) ;
#97174 = ORIENTED_EDGE ( 'NONE', *, *, #42781, .F. ) ;
#97175 = DIRECTION ( 'NONE',  ( 0.000000000000000000, -1.000000000000000000, 0.000000000000000000 ) ) ;
#97176 = LINE ( 'NONE', #10198, #40910 ) ;
#97177 = ADVANCED_FACE ( 'NONE', ( #42512 ), #11242, .F. ) ;
#97178 = CARTESIAN_POINT ( 'NONE',  ( 65.99451991528749772, 28.92564299267984396, 4.000000000000000000 ) ) ;
#97179 = DIRECTION ( 'NONE',  ( -0.7071067811865486830, -0.7071067811865464625, 0.000000000000000000 ) ) ;
#97180 = DIRECTION ( 'NONE',  ( -0.6830127018922180770, -0.6830127018922204085, -0.2588190451025214056 ) ) ;
#97181 = DIRECTION ( 'NONE',  ( -0.3543493200069163240, -0.000000000000000000, 0.9351131265310288487 ) ) ;
#97182 = VECTOR ( 'NONE', #79548, 1000.000000000000000 ) ;
#97183 = CARTESIAN_POINT ( 'NONE',  ( 119.6412635252314658, 4.472830434245836706, 4.472830434245840259 ) ) ;
#97184 = ORIENTED_EDGE ( 'NONE', *, *, #82369, .F. ) ;
#97185 = CARTESIAN_POINT ( 'NONE',  ( 16.44013779566152778, 3.821174125832445049E-16, 0.000000000000000000 ) ) ;
#97187 = VERTEX_POINT ( 'NONE', #378 ) ;
#97186 = VECTOR ( 'NONE', #79989, 1000.000000000000000 ) ;
#97188 = EDGE_CURVE ( 'NONE', #47375, #98565, #44671, .T. ) ;
#97189 = CARTESIAN_POINT ( 'NONE',  ( 70.22502705046288440, 5.819803920172573974, -5.819803920172573086 ) ) ;
#97190 = VECTOR ( 'NONE', #82698, 1000.000000000000000 ) ;
#97191 = AXIS2_PLACEMENT_3D ( 'NONE', #36372, #115298, #103728 ) ;
#97192 = CIRCLE ( 'NONE', #83369, 2.500000000000000444 ) ;
#97193 = LINE ( 'NONE', #18958, #89490 ) ;
#97194 = CARTESIAN_POINT ( 'NONE',  ( 33.48921356237309510, -27.52281430457078670, 5.000000000000000000 ) ) ;
#97195 = VECTOR ( 'NONE', #136503, 1000.000000000000000 ) ;
#97196 = DIRECTION ( 'NONE',  ( 0.7071067811865487940, -0.7071067811865463515, 0.000000000000000000 ) ) ;
#97197 = ORIENTED_EDGE ( 'NONE', *, *, #130205, .F. ) ;
#97198 = CARTESIAN_POINT ( 'NONE',  ( 43.31293019189810423, -1.637169565754159617, -6.110000000000001208 ) ) ;
#97199 = ORIENTED_EDGE ( 'NONE', *, *, #32023, .T. ) ;
#97200 = CARTESIAN_POINT ( 'NONE',  ( -34.92500000000001137, -2.240707523384260824, 4.255531930566247567 ) ) ;
#97201 = DIRECTION ( 'NONE',  ( 0.7071067811865487940, -0.7071067811865463515, 0.000000000000000000 ) ) ;
#97202 = DIRECTION ( 'NONE',  ( -1.000000000000000000, 0.000000000000000000, 0.000000000000000000 ) ) ;
#97203 = EDGE_CURVE ( 'NONE', #65062, #47033, #107721, .T. ) ;
#97204 = PLANE ( 'NONE',  #129399 ) ;
#97205 = VECTOR ( 'NONE', #11215, 1000.000000000000227 ) ;
#97206 = EDGE_CURVE ( 'NONE', #43477, #104700, #129477, .T. ) ;
#97207 = CARTESIAN_POINT ( 'NONE',  ( 43.51626352523143737, -4.472830434245839371, 4.472830434245839371 ) ) ;
#97208 = ORIENTED_EDGE ( 'NONE', *, *, #85383, .F. ) ;
#97209 = CARTESIAN_POINT ( 'NONE',  ( 22.07159235450331991, 9.902892378096218942E-16, 0.000000000000000000 ) ) ;
#97210 = ORIENTED_EDGE ( 'NONE', *, *, #129699, .T. ) ;
#97211 = VERTEX_POINT ( 'NONE', #9843 ) ;
#97212 = AXIS2_PLACEMENT_3D ( 'NONE', #77072, #21936, #30705 ) ;
#97213 = ORIENTED_EDGE ( 'NONE', *, *, #130799, .F. ) ;
#97214 = AXIS2_PLACEMENT_3D ( 'NONE', #82970, #105408, #128609 ) ;
#97215 = PLANE ( 'NONE',  #42867 ) ;
#97216 = DIRECTION ( 'NONE',  ( 0.6830127018922180770, -0.6830127018922204085, -0.2588190451025213501 ) ) ;
#97217 = VERTEX_POINT ( 'NONE', #19302 ) ;
#97218 = CARTESIAN_POINT ( 'NONE',  ( 13.17183060077638324, 6.759292476615645917, 4.000000000000000000 ) ) ;
#97219 = CIRCLE ( 'NONE', #92685, 1.142820323027522456 ) ;
#97220 = DIRECTION ( 'NONE',  ( 0.7071067811865487940, 0.7071067811865463515, 0.000000000000000000 ) ) ;
#97221 = VECTOR ( 'NONE', #71022, 1000.000000000000000 ) ;
#97222 = FACE_OUTER_BOUND ( 'NONE', #83643, .T. ) ;
#97223 = FACE_BOUND ( 'NONE', #100664, .T. ) ;
#97224 = VERTEX_POINT ( 'NONE', #64240 ) ;
#97225 =( NAMED_UNIT ( * ) PLANE_ANGLE_UNIT ( ) SI_UNIT ( $, .RADIAN. ) );
#97226 = EDGE_CURVE ( 'NONE', #66880, #11497, #14118, .T. ) ;
#97227 = VECTOR ( 'NONE', #26727, 1000.000000000000000 ) ;
#97228 = CARTESIAN_POINT ( 'NONE',  ( 3.010806948443976339, -48.09618305010691586, 37.50858089739961798 ) ) ;
#97229 = DIRECTION ( 'NONE',  ( -0.7071067811865487940, 0.7071067811865463515, 0.000000000000000000 ) ) ;
#97230 = VERTEX_POINT ( 'NONE', #47530 ) ;
#97231 = DIRECTION ( 'NONE',  ( 0.000000000000000000, 0.000000000000000000, -1.000000000000000000 ) ) ;
#97232 = ORIENTED_EDGE ( 'NONE', *, *, #60436, .T. ) ;
#97233 = AXIS2_PLACEMENT_3D ( 'NONE', #97939, #118232, #21074 ) ;
#97234 = ORIENTED_EDGE ( 'NONE', *, *, #131184, .T. ) ;
#97235 = PLANE ( 'NONE',  #77297 ) ;
#97236 = VERTEX_POINT ( 'NONE', #89549 ) ;
#97237 = CARTESIAN_POINT ( 'NONE',  ( 57.80793019189810877, -6.109999999999998543, 1.637169565754158507 ) ) ;
#97238 = ORIENTED_EDGE ( 'NONE', *, *, #79028, .T. ) ;
#97239 =( GEOMETRIC_REPRESENTATION_CONTEXT ( 3 ) GLOBAL_UNCERTAINTY_ASSIGNED_CONTEXT ( ( #89850 ) ) GLOBAL_UNIT_ASSIGNED_CONTEXT ( ( #3278, #70030, #48227 ) ) REPRESENTATION_CONTEXT ( 'NONE', 'WORKASPACE' ) );
#97240 = DIRECTION ( 'NONE',  ( 0.6830127018922181881, 0.6830127018922202975, -0.2588190451025214056 ) ) ;
#97241 = CARTESIAN_POINT ( 'NONE',  ( -25.49999999999981881, -1.912538124160733766, 4.000000000000000000 ) ) ;
#97242 = ORIENTED_EDGE ( 'NONE', *, *, #121411, .T. ) ;
#97243 = VECTOR ( 'NONE', #64034, 1000.000000000000000 ) ;
#97244 = DIRECTION ( 'NONE',  ( 0.7071067811865487940, -0.7071067811865463515, 0.000000000000000000 ) ) ;
#97245 = DIRECTION ( 'NONE',  ( 0.000000000000000000, 0.000000000000000000, 1.000000000000000000 ) ) ;
#97246 = CARTESIAN_POINT ( 'NONE',  ( 22.74845587132411140, -11.24070752338416845, 10.39518518046004125 ) ) ;
#97247 = DIRECTION ( 'NONE',  ( -0.7071067811865486830, 0.7071067811865464625, 0.000000000000000000 ) ) ;
#97248 = ORIENTED_EDGE ( 'NONE', *, *, #48085, .T. ) ;
#97249 = ORIENTED_EDGE ( 'NONE', *, *, #13486, .F. ) ;
#97250 = VECTOR ( 'NONE', #19030, 999.9999999999998863 ) ;
#97251 = ORIENTED_EDGE ( 'NONE', *, *, #5477, .T. ) ;
#97252 = CARTESIAN_POINT ( 'NONE',  ( -27.78162688292475124, 21.74787736706806740, 4.999607392498048419 ) ) ;
#97253 = DIRECTION ( 'NONE',  ( 0.7071067811865487940, 0.7071067811865463515, 0.000000000000000000 ) ) ;
#97254 = EDGE_LOOP ( 'NONE', ( #72140, #38494, #98432 ) ) ;
#97255 = ORIENTED_EDGE ( 'NONE', *, *, #20239, .T. ) ;
#97256 = VERTEX_POINT ( 'NONE', #35204 ) ;
#97257 = DIRECTION ( 'NONE',  ( 0.7071067811865487940, 0.7071067811865463515, -0.000000000000000000 ) ) ;
#97258 = CARTESIAN_POINT ( 'NONE',  ( 4.499999999999968914, -11.56887692260769995, 4.000000000000000000 ) ) ;
#97259 = EDGE_CURVE ( 'NONE', #47109, #38139, #90255, .T. ) ;
#97260 = EDGE_CURVE ( 'NONE', #66284, #87171, #118603, .T. ) ;
#97261 = DIRECTION ( 'NONE',  ( 0.7071067811865487940, 0.7071067811865463515, 0.000000000000000000 ) ) ;
#97262 = EDGE_LOOP ( 'NONE', ( #49005, #36390, #58470, #78090, #50384 ) ) ;
#97263 = LINE ( 'NONE', #141534, #39367 ) ;
#97264 = VECTOR ( 'NONE', #56230, 1000.000000000000000 ) ;
#97265 = PLANE ( 'NONE',  #74565 ) ;
#97266 = CARTESIAN_POINT ( 'NONE',  ( 17.56706980810188767, 2.126176841940952134, -7.934999999999993392 ) ) ;
#97267 = DIRECTION ( 'NONE',  ( 0.000000000000000000, -1.000000000000000000, 0.000000000000000000 ) ) ;
#97268 = ORIENTED_EDGE ( 'NONE', *, *, #136185, .F. ) ;
#97269 = CARTESIAN_POINT ( 'NONE',  ( 122.7037635252314516, 6.109999999999999432, 1.122388791418549108E-15 ) ) ;
#97270 = EDGE_CURVE ( 'NONE', #61548, #60360, #13929, .T. ) ;
#97271 = DIRECTION ( 'NONE',  ( 0.7071067811865486830, -0.7071067811865464625, -0.000000000000000000 ) ) ;
#97272 = DIRECTION ( 'NONE',  ( 0.7071067811865486830, -0.7071067811865464625, -0.000000000000000000 ) ) ;
#97274 = ORIENTED_EDGE ( 'NONE', *, *, #140656, .T. ) ;
#97273 = LINE ( 'NONE', #99431, #868 ) ;
#97275 = CARTESIAN_POINT ( 'NONE',  ( 66.43336038379622721, 2.130196079827431532, -7.949999999999996625 ) ) ;
#97276 = ORIENTED_EDGE ( 'NONE', *, *, #39444, .F. ) ;
#97277 = CARTESIAN_POINT ( 'NONE',  ( 0.000000000000000000, 0.000000000000000000, 5.000000000000000000 ) ) ;
#97278 = VECTOR ( 'NONE', #1211, 1000.000000000000000 ) ;
#97279 = CARTESIAN_POINT ( 'NONE',  ( 29.99999999999979039, -0.03360074219773898085, 5.000000000000000000 ) ) ;
#97280 = CARTESIAN_POINT ( 'NONE',  ( -47.99451991528749062, 28.92564299267971251, 4.000000000000000000 ) ) ;
#97281 = EDGE_CURVE ( 'NONE', #90791, #60163, #36588, .T. ) ;
#97282 = ORIENTED_EDGE ( 'NONE', *, *, #86189, .T. ) ;
#97283 = STYLED_ITEM ( 'NONE', ( #52846 ), #116793 ) ;
#97284 = VECTOR ( 'NONE', #95980, 1000.000000000000000 ) ;
#97285 = LINE ( 'NONE', #65447, #113665 ) ;
#97286 = DIRECTION ( 'NONE',  ( 0.7071067811865486830, -0.7071067811865464625, -0.000000000000000000 ) ) ;
#97287 = ORIENTED_EDGE ( 'NONE', *, *, #52281, .T. ) ;
#97289 = ADVANCED_FACE ( 'NONE', ( #46080 ), #125032, .F. ) ;
#97288 = VECTOR ( 'NONE', #91958, 999.9999999999998863 ) ;
#97290 = VECTOR ( 'NONE', #3008, 1000.000000000000000 ) ;
#97291 = AXIS2_PLACEMENT_3D ( 'NONE', #21562, #12092, #65823 ) ;
#97292 = PLANE ( 'NONE',  #46273 ) ;
#97293 = AXIS2_PLACEMENT_3D ( 'NONE', #113261, #24837, #137191 ) ;
#97294 = DIRECTION ( 'NONE',  ( 0.000000000000000000, -1.000000000000000000, 0.000000000000000000 ) ) ;
#97296 = VERTEX_POINT ( 'NONE', #133093 ) ;
#97295 = CIRCLE ( 'NONE', #83372, 0.5000000000000004441 ) ;
#97297 = CARTESIAN_POINT ( 'NONE',  ( -20.99999999999984723, -16.06887692260765377, 4.000000000000000000 ) ) ;
#97298 = LINE ( 'NONE', #95903, #83219 ) ;
#97299 = ORIENTED_EDGE ( 'NONE', *, *, #53758, .F. ) ;
#97300 = ORIENTED_EDGE ( 'NONE', *, *, #93397, .F. ) ;
#97301 = PLANE ( 'NONE',  #98191 ) ;
#97302 = AXIS2_PLACEMENT_3D ( 'NONE', #66033, #54444, #110198 ) ;
#97303 = CARTESIAN_POINT ( 'NONE',  ( -3.707106781186512823, -6.740707523384214639, 5.000000000000000000 ) ) ;
#97304 = CARTESIAN_POINT ( 'NONE',  ( 15.72873647476855297, 5.808823158059031044, -5.808823158059038150 ) ) ;
#97305 = DIRECTION ( 'NONE',  ( 0.000000000000000000, 0.000000000000000000, -1.000000000000000000 ) ) ;
#97306 = LINE ( 'NONE', #99457, #43637 ) ;
#97307 = FACE_OUTER_BOUND ( 'NONE', #81171, .T. ) ;
#97308 = VERTEX_POINT ( 'NONE', #14838 ) ;
#97309 = ADVANCED_FACE ( 'NONE', ( #112730 ), #59114, .F. ) ;
#97310 = LINE ( 'NONE', #29935, #88401 ) ;
#97311 = CARTESIAN_POINT ( 'NONE',  ( 6.462472949537106715, -7.464222240803106570E-16, -6.094999999999989981 ) ) ;
#97312 = VECTOR ( 'NONE', #129638, 1000.000000000000227 ) ;
#97313 = DIRECTION ( 'NONE',  ( 0.000000000000000000, 1.000000000000000000, 0.000000000000000000 ) ) ;
#97314 = CARTESIAN_POINT ( 'NONE',  ( 38.12043019189811588, 3.055000000000002380, -5.291415217122917625 ) ) ;
#97315 = LINE ( 'NONE', #141586, #23241 ) ;
#97316 = EDGE_CURVE ( 'NONE', #10400, #100160, #67849, .T. ) ;
#97317 = EDGE_CURVE ( 'NONE', #51470, #49172, #3918, .T. ) ;
#97318 = AXIS2_PLACEMENT_3D ( 'NONE', #123130, #67316, #33973 ) ;
#97319 = EDGE_LOOP ( 'NONE', ( #32822, #117883, #105974, #184, #43106, #118890 ) ) ;
#97320 = LINE ( 'NONE', #108194, #97349 ) ;
#97321 = AXIS2_PLACEMENT_3D ( 'NONE', #78569, #122765, #23452 ) ;
#97322 = EDGE_LOOP ( 'NONE', ( #50837, #111044, #126845, #134992 ) ) ;
#97323 = AXIS2_PLACEMENT_3D ( 'NONE', #91354, #113063, #23941 ) ;
#97324 = ORIENTED_EDGE ( 'NONE', *, *, #120253, .F. ) ;
#97325 = LINE ( 'NONE', #66181, #22347 ) ;
#97326 = CARTESIAN_POINT ( 'NONE',  ( 21.29974487139158512, -27.71228299555221142, 4.000000000000000000 ) ) ;
#97328 = EDGE_CURVE ( 'NONE', #126851, #13117, #111288, .T. ) ;
#97327 = VECTOR ( 'NONE', #54757, 1000.000000000000000 ) ;
#97329 = ORIENTED_EDGE ( 'NONE', *, *, #135510, .T. ) ;
#97330 = FACE_OUTER_BOUND ( 'NONE', #70599, .T. ) ;
#97331 = CARTESIAN_POINT ( 'NONE',  ( -42.29974487139158157, -27.71228299555235708, 4.000000000000000000 ) ) ;
#97332 = LINE ( 'NONE', #40172, #67179 ) ;
#97333 = EDGE_CURVE ( 'NONE', #4583, #22939, #56264, .T. ) ;
#97334 = CARTESIAN_POINT ( 'NONE',  ( 81.64583333333330017, 2.130196079827356037, -7.950000000000043698 ) ) ;
#97335 = DIRECTION ( 'NONE',  ( 0.000000000000000000, -1.000000000000000000, 0.000000000000000000 ) ) ;
#97336 = AXIS2_PLACEMENT_3D ( 'NONE', #19409, #6341, #17269 ) ;
#97337 = ORIENTED_EDGE ( 'NONE', *, *, #51859, .F. ) ;
#97338 = EDGE_CURVE ( 'NONE', #103228, #19198, #101854, .T. ) ;
#97339 = PLANE ( 'NONE',  #20973 ) ;
#97340 = LINE ( 'NONE', #96615, #70054 ) ;
#97341 = PLANE ( 'NONE',  #38057 ) ;
#97342 = CARTESIAN_POINT ( 'NONE',  ( 26.75159235450331963, 9.902892378096218942E-16, 0.000000000000000000 ) ) ;
#97343 = CARTESIAN_POINT ( 'NONE',  ( 5.510786437626906675, -27.52281430457051314, 5.000000000000000000 ) ) ;
#97344 = CARTESIAN_POINT ( 'NONE',  ( -14.99999999999989875, -1.209798855135683748, 4.371887122346860721 ) ) ;
#97345 = CARTESIAN_POINT ( 'NONE',  ( 50.99451991528749062, 28.92564299267973738, 4.000000000000000000 ) ) ;
#97346 = CARTESIAN_POINT ( 'NONE',  ( 56.51669371712956291, 7.950000000000001066, -2.130196079827421318 ) ) ;
#97347 = EDGE_CURVE ( 'NONE', #28576, #25994, #102955, .T. ) ;
#97348 = LINE ( 'NONE', #86525, #106322 ) ;
#97349 = VECTOR ( 'NONE', #128564, 999.9999999999998863 ) ;
#97350 = ORIENTED_EDGE ( 'NONE', *, *, #72885, .F. ) ;
#97351 = EDGE_LOOP ( 'NONE', ( #100667, #138358, #13866, #65599 ) ) ;
#97352 = CARTESIAN_POINT ( 'NONE',  ( 58.31249999999997868, 5.819803920172571310, 5.819803920172575751 ) ) ;
#97353 = EDGE_CURVE ( 'NONE', #72881, #135979, #78682, .T. ) ;
#97354 = CARTESIAN_POINT ( 'NONE',  ( -29.72174548431409136, 8.259292476615641476, 11.78515199841143435 ) ) ;
#97355 = LINE ( 'NONE', #31428, #30002 ) ;
#97356 = VECTOR ( 'NONE', #120915, 999.9999999999998863 ) ;
#97357 = DIRECTION ( 'NONE',  ( 0.000000000000000000, 2.312964634635743450E-15, 1.000000000000000000 ) ) ;
#97358 = VERTEX_POINT ( 'NONE', #125770 ) ;
#97359 = EDGE_CURVE ( 'NONE', #20435, #91284, #138059, .T. ) ;
#97360 = CARTESIAN_POINT ( 'NONE',  ( 23.29289321881330110, -18.74070752338408852, 5.000000000000000000 ) ) ;
#97361 = CARTESIAN_POINT ( 'NONE',  ( 51.91709685856476852, 3.054999999999998828, 5.291415217122922066 ) ) ;
#97362 = ORIENTED_EDGE ( 'NONE', *, *, #50056, .T. ) ;
#97363 = DIRECTION ( 'NONE',  ( 0.000000000000000000, 1.000000000000000000, 0.000000000000000000 ) ) ;
#97364 = VERTEX_POINT ( 'NONE', #82270 ) ;
#97365 = ORIENTED_EDGE ( 'NONE', *, *, #136413, .T. ) ;
#97366 = EDGE_CURVE ( 'NONE', #59073, #117931, #134322, .T. ) ;
#97367 = AXIS2_PLACEMENT_3D ( 'NONE', #122615, #23285, #1523 ) ;
#97368 = CARTESIAN_POINT ( 'NONE',  ( 21.48921356237309155, -27.52281430457070499, 5.000000000000000000 ) ) ;
#97369 = DIRECTION ( 'NONE',  ( 1.000000000000000000, -0.000000000000000000, -0.000000000000000000 ) ) ;
#97370 = DIRECTION ( 'NONE',  ( -0.7071067811865486830, -0.7071067811865464625, 0.000000000000000000 ) ) ;
#97371 = LINE ( 'NONE', #32897, #16191 ) ;
#97372 = ORIENTED_EDGE ( 'NONE', *, *, #96316, .T. ) ;
#97373 = PLANE ( 'NONE',  #45256 ) ;
#97374 = CARTESIAN_POINT ( 'NONE',  ( -7.171830600776425868, 3.759292476615678336, 4.000000000000000000 ) ) ;
#97376 = EDGE_LOOP ( 'NONE', ( #142422, #11840, #35960, #117565 ) ) ;
#97375 = DIRECTION ( 'NONE',  ( 0.000000000000000000, 0.000000000000000000, 1.000000000000000000 ) ) ;
#97377 = CARTESIAN_POINT ( 'NONE',  ( 86.62543019189811844, 5.291415217122919401, 3.055000000000002824 ) ) ;
#97378 = CARTESIAN_POINT ( 'NONE',  ( -23.51078643762690490, -27.52281430457038880, 5.000000000000000000 ) ) ;
#97379 = CARTESIAN_POINT ( 'NONE',  ( -26.67183060077628198, -15.74070752338411694, 4.000000000000000000 ) ) ;
#97380 = CARTESIAN_POINT ( 'NONE',  ( 1.629999999999999893, -0.4000000000000004108, 2.303088455023526215 ) ) ;
#97381 = ADVANCED_FACE ( 'NONE', ( #29283 ), #40206, .F. ) ;
#97382 = VECTOR ( 'NONE', #64746, 1000.000000000000000 ) ;
#97383 = DIRECTION ( 'NONE',  ( 0.7071067811865487940, 0.7071067811865463515, 0.000000000000000000 ) ) ;
#97384 = ADVANCED_FACE ( 'NONE', ( #18378 ), #72853, .F. ) ;
#97385 = ADVANCED_FACE ( 'NONE', ( #73526 ), #28596, .F. ) ;
#97386 = ORIENTED_EDGE ( 'NONE', *, *, #126518, .T. ) ;
#97387 = CARTESIAN_POINT ( 'NONE',  ( 88.30836038379621300, 7.949999999999996625, 2.130196079827431088 ) ) ;
#97388 = CARTESIAN_POINT ( 'NONE',  ( 69.91209685856478018, 5.291415217122921177, -3.054999999999994831 ) ) ;
#97389 = LINE ( 'NONE', #8917, #30258 ) ;
#97390 = LINE ( 'NONE', #83726, #52433 ) ;
#97391 = ORIENTED_EDGE ( 'NONE', *, *, #73034, .F. ) ;
#97392 = VERTEX_POINT ( 'NONE', #117688 ) ;
#97393 = CARTESIAN_POINT ( 'NONE',  ( 11.48334561358946360, 22.22500000000000142, 4.500000000000000888 ) ) ;
#97396 = EDGE_CURVE ( 'NONE', #104452, #5522, #61949, .T. ) ;
#97395 = VECTOR ( 'NONE', #91927, 1000.000000000000000 ) ;
#97394 = DIRECTION ( 'NONE',  ( -0.7071067811865486830, -0.7071067811865464625, 0.000000000000000000 ) ) ;
#97397 = ORIENTED_EDGE ( 'NONE', *, *, #132739, .F. ) ;
#97398 =( BOUNDED_CURVE ( )  B_SPLINE_CURVE ( 3, ( #93997, #59284, #127348, #25903 ),
 .UNSPECIFIED., .F., .F. ) 
 B_SPLINE_CURVE_WITH_KNOTS ( ( 4, 4 ),
 ( 5.920967161967926273, 7.341195215986645373 ),
 .UNSPECIFIED. ) 
 CURVE ( )  GEOMETRIC_REPRESENTATION_ITEM ( )  RATIONAL_B_SPLINE_CURVE ( ( 1.000000000000000000, 0.8388583629366594963, 0.8388583629366594963, 1.000000000000000000 ) ) 
 REPRESENTATION_ITEM ( '' )  );
#97399 = VECTOR ( 'NONE', #10070, 1000.000000000000000 ) ;
#97401 = VERTEX_POINT ( 'NONE', #139522 ) ;
#97400 = VECTOR ( 'NONE', #98491, 999.9999999999998863 ) ;
#97402 = LINE ( 'NONE', #130070, #97656 ) ;
#97403 = EDGE_LOOP ( 'NONE', ( #91624, #26723, #67345, #138565 ) ) ;
#97404 = CARTESIAN_POINT ( 'NONE',  ( -31.82816939922330945, -17.24070752338410628, 4.000000000000000000 ) ) ;
#97405 = CARTESIAN_POINT ( 'NONE',  ( 0.8691243128804486684, 0.5999999999999987566, 4.444585127983390116 ) ) ;
#97406 = VECTOR ( 'NONE', #100890, 1000.000000000000000 ) ;
#97407 = VECTOR ( 'NONE', #9976, 1000.000000000000000 ) ;
#97408 = VECTOR ( 'NONE', #21399, 1000.000000000000000 ) ;
#97409 = VECTOR ( 'NONE', #66341, 1000.000000000000227 ) ;
#97410 =( BOUNDED_CURVE ( )  B_SPLINE_CURVE ( 2, ( #124209, #14733, #50943, #37937, #115426, #83581, #95134, #92272, #94420, #114735, #71276, #59688, #29174 ),
 .UNSPECIFIED., .F., .F. ) 
 B_SPLINE_CURVE_WITH_KNOTS ( ( 3, 2, 2, 2, 2, 2, 3 ),
 ( 0.2333333333333332815, 0.2361111111111110494, 0.2388888888888888451, 0.2416666666666666130, 0.2444444444444443809, 0.2472222222222221766, 0.2499999999999999445 ),
 .UNSPECIFIED. ) 
 CURVE ( )  GEOMETRIC_REPRESENTATION_ITEM ( )  RATIONAL_B_SPLINE_CURVE ( ( 1.000000000000000666, 0.9659258262890676461, 1.000000000000000000, 0.9659258262890683122, 1.000000000000000000, 0.9659258262890683122, 1.000000000000000000, 0.9659258262890683122, 1.000000000000000000, 0.9659258262890683122, 1.000000000000000000, 0.9659258262890689783, 0.9999999999999993339 ) ) 
 REPRESENTATION_ITEM ( '' )  );
#97411 = CIRCLE ( 'NONE', #134501, 2.055000000000001048 ) ;
#97412 = CARTESIAN_POINT ( 'NONE',  ( 84.48921356237309510, -27.52281430457114197, 5.000000000000000000 ) ) ;
#97413 = FACE_BOUND ( 'NONE', #96462, .T. ) ;
#97414 = LINE ( 'NONE', #96684, #89563 ) ;
#97415 = CARTESIAN_POINT ( 'NONE',  ( -12.69999999999998153, 3.061616997868383634E-16, -2.500000000000000444 ) ) ;
#97417 = LINE ( 'NONE', #87287, #91963 ) ;
#97416 = AXIS2_PLACEMENT_3D ( 'NONE', #130220, #51945, #62833 ) ;
#97419 = ORIENTED_EDGE ( 'NONE', *, *, #75699, .F. ) ;
#97418 = PLANE ( 'NONE',  #143082 ) ;
#97420 = CARTESIAN_POINT ( 'NONE',  ( -13.82816939922343380, -20.24070752338408141, 4.000000000000000000 ) ) ;
#97421 = CONTEXT_DEPENDENT_SHAPE_REPRESENTATION ( #133783, #138388 ) ;
#97422 = VERTEX_POINT ( 'NONE', #106101 ) ;
#97423 = ORIENTED_EDGE ( 'NONE', *, *, #7259, .T. ) ;
#97424 = CARTESIAN_POINT ( 'NONE',  ( 83.18293019189810877, -1.637169565754158951, -6.109999999999998543 ) ) ;
#97425 = ORIENTED_EDGE ( 'NONE', *, *, #135286, .F. ) ;
#97426 = DIRECTION ( 'NONE',  ( 0.000000000000000000, 0.000000000000000000, 1.000000000000000000 ) ) ;
#97427 = CIRCLE ( 'NONE', #49150, 3.113037248396092416 ) ;
#97428 = DIRECTION ( 'NONE',  ( -0.000000000000000000, 0.3543493200069153248, 0.9351131265310292928 ) ) ;
#97429 = EDGE_CURVE ( 'NONE', #49762, #24456, #93832, .T. ) ;
#97430 = VECTOR ( 'NONE', #125895, 1000.000000000000000 ) ;
#97431 = VERTEX_POINT ( 'NONE', #38745 ) ;
#97432 = DIRECTION ( 'NONE',  ( 0.6830127018922180770, -0.6830127018922204085, -0.2588190451025213501 ) ) ;
#97433 = AXIS2_PLACEMENT_3D ( 'NONE', #63931, #42193, #31304 ) ;
#97434 = CARTESIAN_POINT ( 'NONE',  ( 2.510786437626908008, -27.52281430457053446, 5.000000000000000000 ) ) ;
#97435 = PLANE ( 'NONE',  #66922 ) ;
#97436 = VECTOR ( 'NONE', #71760, 1000.000000000000227 ) ;
#97437 = DIRECTION ( 'NONE',  ( 0.6830127018922180770, -0.6830127018922204085, -0.2588190451025213501 ) ) ;
#97438 = DIRECTION ( 'NONE',  ( -0.7071067811865487940, 0.7071067811865463515, 0.000000000000000000 ) ) ;
#97439 = CARTESIAN_POINT ( 'NONE',  ( -51.18398860626899705, 28.73617430169823095, 5.000000000000000000 ) ) ;
#97440 = AXIS2_PLACEMENT_3D ( 'NONE', #65221, #22365, #99964 ) ;
#97441 = LINE ( 'NONE', #75721, #56287 ) ;
#97442 = CARTESIAN_POINT ( 'NONE',  ( 15.83159235450332147, 9.902892378096218942E-16, 0.000000000000000000 ) ) ;
#97443 = ORIENTED_EDGE ( 'NONE', *, *, #136802, .F. ) ;
#97444 = CARTESIAN_POINT ( 'NONE',  ( -15.18398860626900237, 28.73617430169797871, 5.000000000000000000 ) ) ;
#97445 = EDGE_LOOP ( 'NONE', ( #23794, #51519, #41123, #21039 ) ) ;
#97446 = VECTOR ( 'NONE', #113209, 1000.000000000000000 ) ;
#97447 = CARTESIAN_POINT ( 'NONE',  ( 123.4541937171295700, 6.884901960086283523, 3.975000000000002753 ) ) ;
#97448 = PLANE ( 'NONE',  #46678 ) ;
#97449 = EDGE_CURVE ( 'NONE', #11291, #57481, #48195, .T. ) ;
#97450 = ORIENTED_EDGE ( 'NONE', *, *, #115020, .T. ) ;
#97451 = EDGE_LOOP ( 'NONE', ( #27368, #42447, #42746, #56727, #102176 ) ) ;
#97452 = EDGE_CURVE ( 'NONE', #104716, #109980, #6775, .T. ) ;
#97453 = AXIS2_PLACEMENT_3D ( 'NONE', #44432, #108906, #110338 ) ;
#97454 = ORIENTED_EDGE ( 'NONE', *, *, #24678, .F. ) ;
#97455 = CARTESIAN_POINT ( 'NONE',  ( 39.52126352523143282, -4.472830434245838482, -4.472830434245840259 ) ) ;
#97456 = EDGE_LOOP ( 'NONE', ( #123114, #86609, #18299, #70287 ) ) ;
#97457 = CARTESIAN_POINT ( 'NONE',  ( -34.92499999999997584, -7.730000000000015525, 3.180000000000000160 ) ) ;
#97458 = EDGE_CURVE ( 'NONE', #58779, #115678, #84413, .T. ) ;
#97459 = EDGE_CURVE ( 'NONE', #132990, #116882, #70692, .T. ) ;
#97460 = CARTESIAN_POINT ( 'NONE',  ( 29.21247294953710494, 0.000000000000000000, 6.094999999999989981 ) ) ;
#97461 = CARTESIAN_POINT ( 'NONE',  ( 5.847033781869541258, 11.58818063635165885, -27.61414687898571430 ) ) ;
#97462 = ORIENTED_EDGE ( 'NONE', *, *, #76868, .T. ) ;
#97463 = EDGE_CURVE ( 'NONE', #61706, #32667, #108809, .T. ) ;
#97464 = EDGE_LOOP ( 'NONE', ( #107230, #64085, #120383, #13053 ) ) ;
#97465 = CARTESIAN_POINT ( 'NONE',  ( -26.20710678118635784, -5.240707523384228850, 5.000000000000000000 ) ) ;
#97466 = AXIS2_PLACEMENT_3D ( 'NONE', #30910, #97561, #30166 ) ;
#97467 = DIRECTION ( 'NONE',  ( -0.3543493200069162685, -0.000000000000000000, -0.9351131265310288487 ) ) ;
#97469 = ORIENTED_EDGE ( 'NONE', *, *, #97030, .F. ) ;
#97468 = DIRECTION ( 'NONE',  ( -0.000000000000000000, 0.3543493200069153248, 0.9351131265310292928 ) ) ;
#97470 = STYLED_ITEM ( 'NONE', ( #118726 ), #29756 ) ;
#97471 = ORIENTED_EDGE ( 'NONE', *, *, #53407, .T. ) ;
#97472 = CARTESIAN_POINT ( 'NONE',  ( -22.82816939922337340, 9.759292476615620160, 4.000000000000000000 ) ) ;
#97473 = DIRECTION ( 'NONE',  ( 0.7071067811865486830, -0.7071067811865464625, -0.000000000000000000 ) ) ;
#97474 = CARTESIAN_POINT ( 'NONE',  ( -9.183988606268997046, 28.73617430169793607, 5.000000000000000000 ) ) ;
#97475 = EDGE_CURVE ( 'NONE', #87517, #94899, #114841, .T. ) ;
#97476 = VERTEX_POINT ( 'NONE', #94529 ) ;
#97477 = CARTESIAN_POINT ( 'NONE',  ( 109.8916937171295558, 2.130196079827421762, 7.950000000000000178 ) ) ;
#97478 = ORIENTED_EDGE ( 'NONE', *, *, #38948, .T. ) ;
#97479 = ORIENTED_EDGE ( 'NONE', *, *, #75626, .F. ) ;
#97480 = ORIENTED_EDGE ( 'NONE', *, *, #136417, .T. ) ;
#97481 = LINE ( 'NONE', #87347, #21747 ) ;
#97482 = VECTOR ( 'NONE', #65809, 1000.000000000000000 ) ;
#97483 = EDGE_CURVE ( 'NONE', #44918, #57148, #106528, .T. ) ;
#97484 = CARTESIAN_POINT ( 'NONE',  ( 30.45983838949721090, 18.75929247661552424, 8.305906642995555700 ) ) ;
#97485 = FACE_OUTER_BOUND ( 'NONE', #48632, .T. ) ;
#97486 = DIRECTION ( 'NONE',  ( 1.000000000000000000, 0.000000000000000000, 0.000000000000000000 ) ) ;
#97487 = CARTESIAN_POINT ( 'NONE',  ( 118.7875270504628986, 0.000000000000000000, -7.949999999999998401 ) ) ;
#97488 = ORIENTED_EDGE ( 'NONE', *, *, #85662, .T. ) ;
#97489 = CARTESIAN_POINT ( 'NONE',  ( 96.62086038379621300, -6.884901960086286188, 3.974999999999997424 ) ) ;
#97490 = ORIENTED_EDGE ( 'NONE', *, *, #8612, .T. ) ;
#97491 = ADVANCED_FACE ( 'NONE', ( #93127 ), #83711, .F. ) ;
#97492 = VECTOR ( 'NONE', #87758, 1000.000000000000000 ) ;
#97493 = DIRECTION ( 'NONE',  ( 0.7071067811865486830, -0.7071067811865464625, -0.000000000000000000 ) ) ;
#97494 = DIRECTION ( 'NONE',  ( 0.3543493200069162685, -0.000000000000000000, -0.9351131265310288487 ) ) ;
#97495 = EDGE_LOOP ( 'NONE', ( #20058, #128108, #44835, #115777, #133280 ) ) ;
#97496 = PLANE ( 'NONE',  #110852 ) ;
#97497 = CARTESIAN_POINT ( 'NONE',  ( 0.000000000000000000, 0.000000000000000000, 5.000000000000000000 ) ) ;
#97498 = ORIENTED_EDGE ( 'NONE', *, *, #138137, .F. ) ;
#97499 = ORIENTED_EDGE ( 'NONE', *, *, #122396, .T. ) ;
#97500 = EDGE_CURVE ( 'NONE', #72776, #126104, #16994, .T. ) ;
#97501 = DIRECTION ( 'NONE',  ( 0.7071067811865487940, 0.7071067811865463515, 0.000000000000000000 ) ) ;
#97502 = DIRECTION ( 'NONE',  ( 0.000000000000000000, 2.312964634635743450E-15, 1.000000000000000000 ) ) ;
#97503 = CARTESIAN_POINT ( 'NONE',  ( 0.2997448713915885632, -27.71228299555206220, 4.000000000000000000 ) ) ;
#97504 = LINE ( 'NONE', #42466, #26565 ) ;
#97505 = VECTOR ( 'NONE', #122624, 1000.000000000000227 ) ;
#97506 = CARTESIAN_POINT ( 'NONE',  ( -21.18398860626899349, 28.73617430169802134, 5.000000000000000000 ) ) ;
#97507 = CARTESIAN_POINT ( 'NONE',  ( 68.01626352523145158, -4.472830434245839371, 4.472830434245839371 ) ) ;
#97508 = DIRECTION ( 'NONE',  ( -0.7071067811865487940, 0.7071067811865463515, 0.000000000000000000 ) ) ;
#97510 = EDGE_CURVE ( 'NONE', #141681, #63322, #71381, .T. ) ;
#97509 = AXIS2_PLACEMENT_3D ( 'NONE', #140423, #41832, #7749 ) ;
#97511 = CIRCLE ( 'NONE', #35056, 2.500000000000000888 ) ;
#97512 = SURFACE_STYLE_FILL_AREA ( #43167 ) ;
#97513 = FACE_OUTER_BOUND ( 'NONE', #54194, .T. ) ;
#97514 = FACE_OUTER_BOUND ( 'NONE', #111830, .T. ) ;
#97515 = EDGE_CURVE ( 'NONE', #126442, #102417, #74971, .T. ) ;
#97516 = ORIENTED_EDGE ( 'NONE', *, *, #64484, .F. ) ;
#97517 = CARTESIAN_POINT ( 'NONE',  ( -29.99999999999977973, 2.587461875839211167, 4.000000000000000000 ) ) ;
#97518 = ORIENTED_EDGE ( 'NONE', *, *, #55538, .T. ) ;
#97519 = AXIS2_PLACEMENT_3D ( 'NONE', #82545, #15799, #113740 ) ;
#97520 = VECTOR ( 'NONE', #51018, 1000.000000000000000 ) ;
#97521 = AXIS2_PLACEMENT_3D ( 'NONE', #26043, #117295, #126077 ) ;
#97522 = CARTESIAN_POINT ( 'NONE',  ( 12.00548008471251293, 28.92564299267929684, 4.000000000000000000 ) ) ;
#97524 = CARTESIAN_POINT ( 'NONE',  ( -29.29289321881324781, -6.740707523384214639, 5.000000000000000000 ) ) ;
#97523 = AXIS2_PLACEMENT_3D ( 'NONE', #15188, #59465, #134887 ) ;
#97525 = ORIENTED_EDGE ( 'NONE', *, *, #14537, .F. ) ;
#97526 = EDGE_CURVE ( 'NONE', #34599, #89628, #86546, .T. ) ;
#97527 = AXIS2_PLACEMENT_3D ( 'NONE', #30650, #10981, #43647 ) ;
#97528 = CARTESIAN_POINT ( 'NONE',  ( 0.000000000000000000, 0.000000000000000000, 5.000000000000000000 ) ) ;
#97530 = ORIENTED_EDGE ( 'NONE', *, *, #108591, .F. ) ;
#97529 = CARTESIAN_POINT ( 'NONE',  ( -5.207106781186502609, -2.240707523384259492, 5.000000000000000000 ) ) ;
#97531 = PLANE ( 'NONE',  #94882 ) ;
#97532 = CARTESIAN_POINT ( 'NONE',  ( 34.75611968250419892, -21.18706574529238651, 4.955485411084882941 ) ) ;
#97533 = DIRECTION ( 'NONE',  ( 0.3543493200069162685, -0.000000000000000000, -0.9351131265310288487 ) ) ;
#97534 = VERTEX_POINT ( 'NONE', #129302 ) ;
#97535 = VERTEX_POINT ( 'NONE', #43737 ) ;
#97536 = LINE ( 'NONE', #78659, #78748 ) ;
#97537 = CARTESIAN_POINT ( 'NONE',  ( -9.874853806907596621, -14.24070752338414003, 9.401115078912679834 ) ) ;
#97538 = AXIS2_PLACEMENT_3D ( 'NONE', #95254, #120544, #21273 ) ;
#97539 = DIRECTION ( 'NONE',  ( -1.000000000000000000, -0.000000000000000000, -0.000000000000000000 ) ) ;
#97540 = DIRECTION ( 'NONE',  ( -0.7071067811865486830, -0.7071067811865464625, -0.000000000000000000 ) ) ;
#97541 = CARTESIAN_POINT ( 'NONE',  ( 86.41252705046289861, -7.949999999999998401, -4.867971026610728450E-16 ) ) ;
#97542 = LINE ( 'NONE', #106989, #6953 ) ;
#97543 = LINE ( 'NONE', #143201, #78440 ) ;
#97544 = VERTEX_POINT ( 'NONE', #75663 ) ;
#97546 = ADVANCED_FACE ( 'NONE', ( #10374 ), #132197, .T. ) ;
#97545 = VECTOR ( 'NONE', #71783, 1000.000000000000000 ) ;
#97547 = DIRECTION ( 'NONE',  ( 0.7071067811865487940, 0.7071067811865463515, -0.000000000000000000 ) ) ;
#97548 = CARTESIAN_POINT ( 'NONE',  ( -34.92500000000001137, 22.22500000000000142, 4.000000000000000000 ) ) ;
#97549 = CARTESIAN_POINT ( 'NONE',  ( 33.10416666666667140, -1.633150327867691987, -6.094999999999989093 ) ) ;
#97550 = ORIENTED_EDGE ( 'NONE', *, *, #7212, .F. ) ;
#97551 = EDGE_CURVE ( 'NONE', #140592, #97230, #130776, .T. ) ;
#97552 = PLANE ( 'NONE',  #132452 ) ;
#97553 = ORIENTED_EDGE ( 'NONE', *, *, #47782, .F. ) ;
#97554 = AXIS2_PLACEMENT_3D ( 'NONE', #36789, #114357, #93320 ) ;
#97555 = CARTESIAN_POINT ( 'NONE',  ( 75.39626352523141861, 4.472830434245840259, -4.472830434245839371 ) ) ;
#97556 = VECTOR ( 'NONE', #39374, 1000.000000000000000 ) ;
#97557 = FILL_AREA_STYLE_COLOUR ( '', #43094 ) ;
#97558 = LINE ( 'NONE', #19297, #26129 ) ;
#97559 = VERTEX_POINT ( 'NONE', #140888 ) ;
#97560 = AXIS2_PLACEMENT_3D ( 'NONE', #13011, #13714, #136228 ) ;
#97561 = DIRECTION ( 'NONE',  ( 0.6830127018922181881, 0.6830127018922202975, -0.2588190451025214056 ) ) ;
#97562 = DIRECTION ( 'NONE',  ( -0.7071067811865486830, -0.7071067811865464625, 0.000000000000000000 ) ) ;
#97563 = LINE ( 'NONE', #10540, #94852 ) ;
#97564 = VECTOR ( 'NONE', #106246, 1000.000000000000000 ) ;
#97565 = CARTESIAN_POINT ( 'NONE',  ( 19.10813147593277250, -2.055000000000000160, 0.000000000000000000 ) ) ;
#97567 = ORIENTED_EDGE ( 'NONE', *, *, #76926, .T. ) ;
#97566 = CARTESIAN_POINT ( 'NONE',  ( 34.45011844616453800, -2.997695858406035363, 5.000000000000001776 ) ) ;
#97568 = CARTESIAN_POINT ( 'NONE',  ( -45.48921356237309510, -27.52281430457087197, 5.000000000000000000 ) ) ;
#97569 = DIRECTION ( 'NONE',  ( -0.7071067811865486830, -0.7071067811865464625, -0.000000000000000000 ) ) ;
#97570 = PLANE ( 'NONE',  #86447 ) ;
#97571 = FILL_AREA_STYLE_COLOUR ( '', #129403 ) ;
#97572 = ORIENTED_EDGE ( 'NONE', *, *, #12573, .T. ) ;
#97573 = EDGE_CURVE ( 'NONE', #121799, #42327, #76378, .T. ) ;
#97574 = VERTEX_POINT ( 'NONE', #9663 ) ;
#97575 = CARTESIAN_POINT ( 'NONE',  ( 62.56293019189811133, 1.637169565754157174, 6.110000000000002984 ) ) ;
#97576 = VERTEX_POINT ( 'NONE', #51776 ) ;
#97577 = LINE ( 'NONE', #85268, #31427 ) ;
#97578 = CARTESIAN_POINT ( 'NONE',  ( -20.70025512860841133, -27.71228299555191654, 4.000000000000000000 ) ) ;
#97579 = AXIS2_PLACEMENT_3D ( 'NONE', #82802, #16813, #61089 ) ;
#97580 = CARTESIAN_POINT ( 'NONE',  ( 8.671830600776411657, 5.259292476615662792, 4.000000000000000000 ) ) ;
#97581 = CARTESIAN_POINT ( 'NONE',  ( 34.92499999999998295, -21.72500000000000142, 5.000000000000000000 ) ) ;
#97582 = VERTEX_POINT ( 'NONE', #119144 ) ;
#97583 = VECTOR ( 'NONE', #12468, 1000.000000000000114 ) ;
#97584 = CARTESIAN_POINT ( 'NONE',  ( -15.29974487139158867, -27.71228299555216879, 4.000000000000000000 ) ) ;
#97585 = EDGE_LOOP ( 'NONE', ( #24855, #75190, #50329, #41459 ) ) ;
#97586 = CARTESIAN_POINT ( 'NONE',  ( 33.48921356237309510, -27.52281430457078670, 5.000000000000000000 ) ) ;
#97587 = CARTESIAN_POINT ( 'NONE',  ( -34.92500000000001137, 22.22500000000000142, 4.000000000000000000 ) ) ;
#97588 = LINE ( 'NONE', #120028, #35445 ) ;
#97589 = VECTOR ( 'NONE', #132314, 1000.000000000000000 ) ;
#97590 = ORIENTED_EDGE ( 'NONE', *, *, #47557, .T. ) ;
#97591 = VERTEX_POINT ( 'NONE', #87955 ) ;
#97592 = FACE_BOUND ( 'NONE', #35689, .T. ) ;
#97593 = LINE ( 'NONE', #30949, #1468 ) ;
#97594 = CARTESIAN_POINT ( 'NONE',  ( 36.18398860626899705, 28.73617430169812437, 5.000000000000000000 ) ) ;
#97595 = PLANE ( 'NONE',  #131607 ) ;
#97596 = VECTOR ( 'NONE', #60515, 1000.000000000000000 ) ;
#97597 =( NAMED_UNIT ( * ) PLANE_ANGLE_UNIT ( ) SI_UNIT ( $, .RADIAN. ) );
#97598 =( BOUNDED_CURVE ( )  B_SPLINE_CURVE ( 3, ( #128562, #53114, #130726, #72807 ),
 .UNSPECIFIED., .F., .T. ) 
 B_SPLINE_CURVE_WITH_KNOTS ( ( 4, 4 ),
 ( 5.005968288816742273, 5.074607125596344304 ),
 .UNSPECIFIED. ) 
 CURVE ( )  GEOMETRIC_REPRESENTATION_ITEM ( )  RATIONAL_B_SPLINE_CURVE ( ( 1.000000000000000000, 0.9996074310407765395, 0.9996074310407765395, 1.000000000000000000 ) ) 
 REPRESENTATION_ITEM ( '' )  );
#97599 = DIRECTION ( 'NONE',  ( 0.7071067811865486830, -0.7071067811865464625, -0.000000000000000000 ) ) ;
#97600 = VERTEX_POINT ( 'NONE', #120545 ) ;
#97601 = ORIENTED_EDGE ( 'NONE', *, *, #66567, .T. ) ;
#97602 = CARTESIAN_POINT ( 'NONE',  ( 114.5370968585647802, -3.054999999999998828, -5.291415217122919401 ) ) ;
#97603 = ORIENTED_EDGE ( 'NONE', *, *, #141252, .T. ) ;
#97604 = EDGE_LOOP ( 'NONE', ( #34264, #19983, #40100, #26363 ) ) ;
#97605 = AXIS2_PLACEMENT_3D ( 'NONE', #83823, #125140, #114940 ) ;
#97606 = AXIS2_PLACEMENT_3D ( 'NONE', #26876, #63114, #6501 ) ;
#97607 = CARTESIAN_POINT ( 'NONE',  ( 15.41161490594821437, 22.22500000000000142, 4.777194822843815913 ) ) ;
#97608 = VECTOR ( 'NONE', #8280, 1000.000000000000000 ) ;
#97609 = CIRCLE ( 'NONE', #65168, 2.256103126841972895 ) ;
#97610 = DIRECTION ( 'NONE',  ( -0.7071067811865486830, -0.7071067811865464625, 0.000000000000000000 ) ) ;
#97611 = ORIENTED_EDGE ( 'NONE', *, *, #14906, .F. ) ;
#97612 = FACE_OUTER_BOUND ( 'NONE', #106861, .T. ) ;
#97613 = CARTESIAN_POINT ( 'NONE',  ( -2.994519915287485734, 28.92564299267940342, 4.000000000000000000 ) ) ;
#97616 = ADVANCED_FACE ( 'NONE', ( #109706 ), #74231, .F. ) ;
#97615 = DIRECTION ( 'NONE',  ( 0.3543493200069162685, -0.000000000000000000, -0.9351131265310288487 ) ) ;
#97614 = DIRECTION ( 'NONE',  ( 0.6830127018922180770, -0.6830127018922204085, -0.2588190451025213501 ) ) ;
#97617 = CARTESIAN_POINT ( 'NONE',  ( 27.53159235450332076, -7.703719777548943412E-31, 2.500000000000001332 ) ) ;
#97618 = VECTOR ( 'NONE', #135352, 1000.000000000000000 ) ;
#97619 = VECTOR ( 'NONE', #111825, 1000.000000000000000 ) ;
#97620 = STYLED_ITEM ( 'NONE', ( #132358 ), #65904 ) ;
#97621 = VECTOR ( 'NONE', #50529, 999.9999999999998863 ) ;
#97622 = LINE ( 'NONE', #11299, #86077 ) ;
#97623 = VERTEX_POINT ( 'NONE', #32150 ) ;
#97624 = AXIS2_PLACEMENT_3D ( 'NONE', #69715, #71851, #15966 ) ;
#97625 = PLANE ( 'NONE',  #132963 ) ;
#97626 = FACE_OUTER_BOUND ( 'NONE', #55851, .T. ) ;
#97627 = EDGE_CURVE ( 'NONE', #37692, #92938, #97371, .T. ) ;
#97628 = ORIENTED_EDGE ( 'NONE', *, *, #32397, .T. ) ;
#97629 = CARTESIAN_POINT ( 'NONE',  ( -0.2997448713915885632, -27.71228299555206220, 4.000000000000000000 ) ) ;
#97630 = ORIENTED_EDGE ( 'NONE', *, *, #16544, .T. ) ;
#97631 = VERTEX_POINT ( 'NONE', #21274 ) ;
#97632 = EDGE_CURVE ( 'NONE', #134215, #43029, #21973, .T. ) ;
#97633 = EDGE_CURVE ( 'NONE', #43477, #139296, #53933, .T. ) ;
#97634 = ORIENTED_EDGE ( 'NONE', *, *, #9256, .F. ) ;
#97635 = COLOUR_RGB ( '', 0.66274510, 0.83137255, 0.94901961) ;
#97636 = CARTESIAN_POINT ( 'NONE',  ( 60.52126352523143282, -4.472830434245838482, -4.472830434245840259 ) ) ;
#97637 = ORIENTED_EDGE ( 'NONE', *, *, #106699, .T. ) ;
#97638 = ORIENTED_EDGE ( 'NONE', *, *, #74422, .T. ) ;
#97639 = ADVANCED_FACE ( 'NONE', ( #20529 ), #119835, .F. ) ;
#97640 = EDGE_CURVE ( 'NONE', #18391, #98793, #122720, .T. ) ;
#97641 = FACE_OUTER_BOUND ( 'NONE', #2342, .T. ) ;
#97642 = DIRECTION ( 'NONE',  ( -0.6830127018922180770, -0.6830127018922204085, -0.2588190451025213501 ) ) ;
#97643 = CARTESIAN_POINT ( 'NONE',  ( 98.29209685856477563, -5.291415217122921177, 3.054999999999999272 ) ) ;
#97644 = CARTESIAN_POINT ( 'NONE',  ( -18.78162688292481874, 21.74787736706806385, 4.999607392498049308 ) ) ;
#97645 = ADVANCED_FACE ( 'NONE', ( #22658 ), #123478, .F. ) ;
#97646 = CARTESIAN_POINT ( 'NONE',  ( -1.499999999999987566, 16.46639925780209168, 5.000000000000000000 ) ) ;
#97647 = ORIENTED_EDGE ( 'NONE', *, *, #88853, .F. ) ;
#97648 = DIRECTION ( 'NONE',  ( 0.7071067811865487940, -0.7071067811865463515, 0.000000000000000000 ) ) ;
#97649 = EDGE_CURVE ( 'NONE', #62399, #51414, #23399, .T. ) ;
#97650 = CARTESIAN_POINT ( 'NONE',  ( 24.99941145866615244, 2.672864951410429679, 4.679979323531649804 ) ) ;
#97651 = CARTESIAN_POINT ( 'NONE',  ( 90.97916666666667140, -7.950000000000000178, 2.130196079827424427 ) ) ;
#97652 = AXIS2_PLACEMENT_3D ( 'NONE', #91746, #1150, #35273 ) ;
#97653 = CARTESIAN_POINT ( 'NONE',  ( 0.000000000000000000, 0.000000000000000000, 5.000000000000000000 ) ) ;
#97654 = EDGE_CURVE ( 'NONE', #102314, #86645, #112262, .T. ) ;
#97655 = VERTEX_POINT ( 'NONE', #13940 ) ;
#97656 = VECTOR ( 'NONE', #43073, 1000.000000000000000 ) ;
#97657 = CARTESIAN_POINT ( 'NONE',  ( -34.92500000000001137, -19.48753812416029874, 4.000000000000000000 ) ) ;
#97658 = EDGE_LOOP ( 'NONE', ( #116797, #134327, #106864, #54338 ) ) ;
#97659 = VECTOR ( 'NONE', #64335, 999.9999999999998863 ) ;
#97660 = ORIENTED_EDGE ( 'NONE', *, *, #101785, .T. ) ;
#97661 = ORIENTED_EDGE ( 'NONE', *, *, #141591, .F. ) ;
#97662 = CARTESIAN_POINT ( 'NONE',  ( 119.0579301918981230, 6.110000000000000320, -1.637169565754156064 ) ) ;
#97663 = ORIENTED_EDGE ( 'NONE', *, *, #112253, .T. ) ;
#97664 = VECTOR ( 'NONE', #5528, 1000.000000000000000 ) ;
#97665 = CARTESIAN_POINT ( 'NONE',  ( 11.99999999999991296, 14.87792677143810316, -11.06722581663437488 ) ) ;
#97666 = DIRECTION ( 'NONE',  ( 0.7071067811865487940, -0.7071067811865463515, 0.000000000000000000 ) ) ;
#97667 = EDGE_CURVE ( 'NONE', #40996, #99872, #34292, .T. ) ;
#97668 = CARTESIAN_POINT ( 'NONE',  ( -27.79289321881325492, 15.75929247661555799, 5.000000000000000000 ) ) ;
#97669 = VERTEX_POINT ( 'NONE', #111105 ) ;
#97670 = CARTESIAN_POINT ( 'NONE',  ( 52.26932219902325727, -49.14999999999999147, 40.92499999999998295 ) ) ;
#97671 = ORIENTED_EDGE ( 'NONE', *, *, #32380, .T. ) ;
#97672 = ADVANCED_FACE ( 'NONE', ( #57495 ), #189, .F. ) ;
#97673 = AXIS2_PLACEMENT_3D ( 'NONE', #60403, #124204, #37193 ) ;
#97674 = CARTESIAN_POINT ( 'NONE',  ( 17.91623647476855652, -7.934999999999990727, 4.858786175617117713E-16 ) ) ;
#97675 = DIRECTION ( 'NONE',  ( 0.7071067811865487940, 0.7071067811865463515, 0.000000000000000000 ) ) ;
#97676 = CARTESIAN_POINT ( 'NONE',  ( -14.99999999999988809, -1.447814304570818500, 5.000000000000000000 ) ) ;
#97677 = CARTESIAN_POINT ( 'NONE',  ( 34.47516574401891631, 3.028067341115785460, 4.998110765256834398 ) ) ;
#97678 = EDGE_LOOP ( 'NONE', ( #15307, #54718, #47797, #106811 ) ) ;
#97679 = ORIENTED_EDGE ( 'NONE', *, *, #82760, .F. ) ;
#97680 = AXIS2_PLACEMENT_3D ( 'NONE', #101333, #58608, #123827 ) ;
#97682 = VERTEX_POINT ( 'NONE', #112565 ) ;
#97681 = ADVANCED_FACE ( 'NONE', ( #45903 ), #58241, .F. ) ;
#97683 = DIRECTION ( 'NONE',  ( -0.7071067811865487940, 0.7071067811865463515, -0.000000000000000000 ) ) ;
#97684 = SURFACE_STYLE_USAGE ( .BOTH. , #64352 ) ;
#97685 = VECTOR ( 'NONE', #10849, 1000.000000000000114 ) ;
#97686 = CARTESIAN_POINT ( 'NONE',  ( -18.18398860626898994, 28.73617430169800002, 5.000000000000000000 ) ) ;
#97687 = PLANE ( 'NONE',  #29750 ) ;
#97688 = CARTESIAN_POINT ( 'NONE',  ( -17.67183060077635304, -12.74070752338415602, 4.000000000000000000 ) ) ;
#97689 = EDGE_CURVE ( 'NONE', #139436, #8017, #92679, .T. ) ;
#97690 = DIRECTION ( 'NONE',  ( 1.000000000000000000, -0.000000000000000000, -0.000000000000000000 ) ) ;
#97691 = CARTESIAN_POINT ( 'NONE',  ( 28.58376352523143993, -6.110000000000001208, -3.741295971395164515E-16 ) ) ;
#97692 =( LENGTH_UNIT ( ) NAMED_UNIT ( * ) SI_UNIT ( .MILLI., .METRE. ) );
#97693 = DIRECTION ( 'NONE',  ( -1.000000000000000000, -0.000000000000000000, -0.000000000000000000 ) ) ;
#97694 = ADVANCED_FACE ( 'NONE', ( #47373 ), #134332, .F. ) ;
#97695 = ORIENTED_EDGE ( 'NONE', *, *, #135745, .T. ) ;
#97696 = CARTESIAN_POINT ( 'NONE',  ( -33.48921356237309510, -27.52281430457078670, 5.000000000000000000 ) ) ;
#97697 = AXIS2_PLACEMENT_3D ( 'NONE', #56731, #100891, #32813 ) ;
#97698 = VERTEX_POINT ( 'NONE', #101682 ) ;
#97699 = LINE ( 'NONE', #121581, #77726 ) ;
#97700 = ORIENTED_EDGE ( 'NONE', *, *, #67089, .T. ) ;
#97701 = EDGE_CURVE ( 'NONE', #51992, #5639, #36438, .T. ) ;
#97702 = ADVANCED_FACE ( 'NONE', ( #46653 ), #2338, .F. ) ;
#97703 = FACE_OUTER_BOUND ( 'NONE', #40530, .T. ) ;
#97705 = EDGE_LOOP ( 'NONE', ( #77467, #85718, #99912, #10899 ) ) ;
#97704 = DIRECTION ( 'NONE',  ( -0.7071067811865486830, -0.7071067811865464625, 0.000000000000000000 ) ) ;
#97706 = DIRECTION ( 'NONE',  ( -0.3543493200069162685, -0.000000000000000000, -0.9351131265310288487 ) ) ;
#97707 = EDGE_LOOP ( 'NONE', ( #131686, #46604, #87141, #34456 ) ) ;
#97708 = LINE ( 'NONE', #86848, #18359 ) ;
#97710 = ORIENTED_EDGE ( 'NONE', *, *, #107183, .T. ) ;
#97709 = STYLED_ITEM ( 'NONE', ( #81721 ), #77853 ) ;
#97711 = DIRECTION ( 'NONE',  ( 0.7071067811865487940, 0.7071067811865463515, 0.000000000000000000 ) ) ;
#97712 = ORIENTED_EDGE ( 'NONE', *, *, #70760, .F. ) ;
#97713 = CARTESIAN_POINT ( 'NONE',  ( 108.8708603837962272, 6.884901960086289741, -3.974999999999993427 ) ) ;
#97714 = CARTESIAN_POINT ( 'NONE',  ( 34.92499999999998295, 2.816654386410421207, 4.500000000000000888 ) ) ;
#97715 = DIRECTION ( 'NONE',  ( -0.000000000000000000, 1.000000000000000000, 0.000000000000000000 ) ) ;
#97716 = EDGE_CURVE ( 'NONE', #11574, #42096, #25546, .T. ) ;
#97717 = CARTESIAN_POINT ( 'NONE',  ( -12.18398860626900060, 28.73617430169795739, 5.000000000000000000 ) ) ;
#97718 = DIRECTION ( 'NONE',  ( -1.000000000000000000, -1.224606353822377258E-16, -0.000000000000000000 ) ) ;
#97719 = CARTESIAN_POINT ( 'NONE',  ( 54.18398860626899705, 28.73617430169825226, 5.000000000000000000 ) ) ;
#97720 = CARTESIAN_POINT ( 'NONE',  ( 7.729166666666666075, -6.094999999999989093, 1.633150327867691765 ) ) ;
#97721 = CARTESIAN_POINT ( 'NONE',  ( 14.12456980810188689, -6.871911579029512218, 3.967499999999996252 ) ) ;
#97722 = VECTOR ( 'NONE', #82226, 999.9999999999998863 ) ;
#97723 = AXIS2_PLACEMENT_3D ( 'NONE', #89478, #78615, #35132 ) ;
#97725 = SURFACE_STYLE_FILL_AREA ( #53518 ) ;
#97724 = VECTOR ( 'NONE', #4275, 1000.000000000000000 ) ;
#97726 = CARTESIAN_POINT ( 'NONE',  ( 21.79289321881331531, 18.75929247661553489, 5.000000000000000000 ) ) ;
#97727 = ORIENTED_EDGE ( 'NONE', *, *, #89679, .F. ) ;
#97728 = ORIENTED_EDGE ( 'NONE', *, *, #120691, .F. ) ;
#97729 = MECHANICAL_DESIGN_GEOMETRIC_PRESENTATION_REPRESENTATION (  '', ( #56070 ), #35259 ) ;
#97730 = AXIS2_PLACEMENT_3D ( 'NONE', #78556, #2369, #122754 ) ;
#97731 = DIRECTION ( 'NONE',  ( -0.7071067811865487940, 0.7071067811865463515, 0.000000000000000000 ) ) ;
#97732 = EDGE_LOOP ( 'NONE', ( #142748, #98929, #43365, #117174 ) ) ;
#97733 = EDGE_CURVE ( 'NONE', #48148, #86443, #91539, .T. ) ;
#97734 = CARTESIAN_POINT ( 'NONE',  ( 90.93336038379622721, 2.130196079827431532, -7.949999999999996625 ) ) ;
#97735 = DIRECTION ( 'NONE',  ( 0.7071067811865487940, 0.7071067811865463515, 0.000000000000000000 ) ) ;
#97736 = CARTESIAN_POINT ( 'NONE',  ( 16.49999999999987921, -20.94781430457061333, 5.000000000000000000 ) ) ;
#97737 = VECTOR ( 'NONE', #73676, 1000.000000000000000 ) ;
#97738 = CIRCLE ( 'NONE', #23754, 4.000000000000000000 ) ;
#97739 = STYLED_ITEM ( 'NONE', ( #40912 ), #18911 ) ;
#97740 = CARTESIAN_POINT ( 'NONE',  ( 127.0485559394951025, -49.69743550128988829, -36.79359617903030966 ) ) ;
#97741 = ORIENTED_EDGE ( 'NONE', *, *, #60544, .T. ) ;
#97742 = LINE ( 'NONE', #73337, #105296 ) ;
#97743 = DIRECTION ( 'NONE',  ( 0.3543493200069162685, -0.000000000000000000, -0.9351131265310288487 ) ) ;
#97744 = CARTESIAN_POINT ( 'NONE',  ( 92.87500000000000000, 7.950000000000000178, 1.460391307983218535E-15 ) ) ;
#97745 = EDGE_CURVE ( 'NONE', #132946, #68806, #924, .T. ) ;
#97746 = FACE_OUTER_BOUND ( 'NONE', #62805, .T. ) ;
#97748 = ORIENTED_EDGE ( 'NONE', *, *, #129132, .F. ) ;
#97747 = LINE ( 'NONE', #31780, #100747 ) ;
#97749 = CARTESIAN_POINT ( 'NONE',  ( -2.510786437626908008, -27.52281430457053446, 5.000000000000000000 ) ) ;
#97750 = LINE ( 'NONE', #141995, #84637 ) ;
#97751 = DIRECTION ( 'NONE',  ( 1.248002500702736137E-15, 1.000000000000000000, 0.000000000000000000 ) ) ;
#97752 = DIRECTION ( 'NONE',  ( 0.000000000000000000, -1.000000000000000000, 0.000000000000000000 ) ) ;
#97753 = CARTESIAN_POINT ( 'NONE',  ( 56.09195796767451014, -46.73296206246043738, 36.09967824800554581 ) ) ;
#97754 = ORIENTED_EDGE ( 'NONE', *, *, #138389, .F. ) ;
#97755 = ORIENTED_EDGE ( 'NONE', *, *, #131248, .T. ) ;
#97756 = ORIENTED_EDGE ( 'NONE', *, *, #66289, .T. ) ;
#97757 = CARTESIAN_POINT ( 'NONE',  ( 92.31293019189811844, -1.637169565754159617, -6.110000000000001208 ) ) ;
#97758 = VERTEX_POINT ( 'NONE', #77806 ) ;
#97759 = CARTESIAN_POINT ( 'NONE',  ( 131.3130295073144396, -48.90295371244932454, 39.18578444878558287 ) ) ;
#97760 = CARTESIAN_POINT ( 'NONE',  ( 42.48921356237308800, -27.52281430457085065, 5.000000000000000000 ) ) ;
#97761 = ORIENTED_EDGE ( 'NONE', *, *, #50413, .T. ) ;
#97762 = PLANE ( 'NONE',  #70005 ) ;
#97764 = EDGE_CURVE ( 'NONE', #99982, #142463, #45207, .T. ) ;
#97763 = LINE ( 'NONE', #20903, #32675 ) ;
#97765 = VECTOR ( 'NONE', #18082, 1000.000000000000000 ) ;
#97766 = CARTESIAN_POINT ( 'NONE',  ( 93.24543019189812298, -5.291415217122918513, -3.055000000000000160 ) ) ;
#97767 = EDGE_CURVE ( 'NONE', #48205, #90138, #69818, .T. ) ;
#97768 = ORIENTED_EDGE ( 'NONE', *, *, #30580, .T. ) ;
#97769 = AXIS2_PLACEMENT_3D ( 'NONE', #88236, #33174, #34565 ) ;
#97770 = CARTESIAN_POINT ( 'NONE',  ( 0.1419055191998411514, 0.5999999999999987566, -3.724211676661871806 ) ) ;
#97771 = CARTESIAN_POINT ( 'NONE',  ( 116.2083333333333286, -3.974999999999999201, -6.884901960086287964 ) ) ;
#97772 = VECTOR ( 'NONE', #11595, 1000.000000000000227 ) ;
#97773 = EDGE_LOOP ( 'NONE', ( #135440, #3907, #97661, #23650 ) ) ;
#97774 = EDGE_LOOP ( 'NONE', ( #36352, #93851, #35517, #109981 ) ) ;
#97775 = EDGE_LOOP ( 'NONE', ( #135240, #72470, #82204, #118511 ) ) ;
#97776 = CARTESIAN_POINT ( 'NONE',  ( 44.99451991528749772, 28.92564299267969474, 4.000000000000000000 ) ) ;
#97777 = EDGE_CURVE ( 'NONE', #143427, #112319, #103761, .T. ) ;
#97778 = DIRECTION ( 'NONE',  ( 0.7071067811865487940, 0.7071067811865463515, -0.000000000000000000 ) ) ;
#97779 = CARTESIAN_POINT ( 'NONE',  ( 16.25456980810188767, -6.871911579029512218, 3.967499999999996252 ) ) ;
#97780 = LINE ( 'NONE', #132593, #76652 ) ;
#97781 = COLOUR_RGB ( '', 0.31764706, 0.68627451, 0.89019608) ;
#97782 = CARTESIAN_POINT ( 'NONE',  ( 164.5367464035145133, 26.96999999999993847, 34.26648380511346659 ) ) ;
#97783 = LINE ( 'NONE', #30387, #2432 ) ;
#97784 =( LENGTH_UNIT ( ) NAMED_UNIT ( * ) SI_UNIT ( .MILLI., .METRE. ) );
#97785 = ORIENTED_EDGE ( 'NONE', *, *, #143104, .F. ) ;
#97786 = VERTEX_POINT ( 'NONE', #92220 ) ;
#97787 = CARTESIAN_POINT ( 'NONE',  ( -21.71715331601274102, -2.164967620583693630, 5.000000000000000000 ) ) ;
#97788 = EDGE_LOOP ( 'NONE', ( #24564, #127582, #31170, #113944, #21225 ) ) ;
#97789 = EDGE_LOOP ( 'NONE', ( #68991, #4930, #12682 ) ) ;
#97790 = AXIS2_PLACEMENT_3D ( 'NONE', #9685, #88716, #98149 ) ;
#97791 = B_SPLINE_CURVE_WITH_KNOTS ( 'NONE', 3,
 ( #40421, #7746, #49158, #17891, #139010, #17217, #128826, #51997, #85308, #94752, #82485, #61479, #29503, #73736 ),
 .UNSPECIFIED., .F., .F.,
 ( 4, 2, 2, 2, 2, 2, 4 ),
 ( 1.498279533920597479E-16, 0.001332397885839088636, 0.001998596828758557493, 0.002664795771678026351, 0.003997193657516964933, 0.004663392600436432923, 0.005329591543355900914 ),
 .UNSPECIFIED. ) ;
#97792 = LINE ( 'NONE', #606, #5754 ) ;
#97793 = EDGE_LOOP ( 'NONE', ( #30519, #136414, #125664, #13697 ) ) ;
#97794 = CARTESIAN_POINT ( 'NONE',  ( 39.18398860626899705, 28.73617430169814568, 5.000000000000000000 ) ) ;
#97795 = DIRECTION ( 'NONE',  ( -0.7071067811865486830, -0.7071067811865464625, -0.000000000000000000 ) ) ;
#97796 = ADVANCED_FACE ( 'NONE', ( #28426 ), #82814, .T. ) ;
#97797 = DIRECTION ( 'NONE',  ( 0.000000000000000000, 0.000000000000000000, 1.000000000000000000 ) ) ;
#97798 = DIRECTION ( 'NONE',  ( -1.000000000000000000, -0.000000000000000000, -0.000000000000000000 ) ) ;
#97799 = VECTOR ( 'NONE', #18765, 1000.000000000000227 ) ;
#97800 = CARTESIAN_POINT ( 'NONE',  ( 120.0000000000000000, 0.000000000000000000, -7.950000000000000178 ) ) ;
#97801 = ORIENTED_EDGE ( 'NONE', *, *, #35498, .F. ) ;
#97802 = VERTEX_POINT ( 'NONE', #136450 ) ;
#97803 = LINE ( 'NONE', #40591, #36572 ) ;
#97804 = PLANE ( 'NONE',  #94348 ) ;
#97805 = EDGE_LOOP ( 'NONE', ( #34251, #13748, #39897, #119408 ) ) ;
#97806 = DIRECTION ( 'NONE',  ( -0.6830127018922181881, 0.6830127018922202975, -0.2588190451025214056 ) ) ;
#97808 = ORIENTED_EDGE ( 'NONE', *, *, #73069, .T. ) ;
#97807 = ADVANCED_FACE ( 'NONE', ( #16064 ), #60356, .F. ) ;
#97809 = PLANE ( 'NONE',  #92156 ) ;
#97810 = EDGE_LOOP ( 'NONE', ( #131404, #60399, #42833, #5045 ) ) ;
#97811 = VERTEX_POINT ( 'NONE', #71228 ) ;
#97812 = AXIS2_PLACEMENT_3D ( 'NONE', #60328, #102404, #36412 ) ;
#97813 = ORIENTED_EDGE ( 'NONE', *, *, #57493, .F. ) ;
#97814 = ADVANCED_FACE ( 'NONE', ( #37147 ), #16826, .F. ) ;
#97815 = EDGE_CURVE ( 'NONE', #17758, #91076, #6603, .T. ) ;
#97816 = CARTESIAN_POINT ( 'NONE',  ( -19.49999999999986144, -20.56887692260760758, 4.000000000000000000 ) ) ;
#97817 = CARTESIAN_POINT ( 'NONE',  ( 24.39999999999999858, -1.600000000000060929, 28.92500000000001847 ) ) ;
#97819 = EDGE_CURVE ( 'NONE', #29477, #69770, #114688, .T. ) ;
#97818 = DIRECTION ( 'NONE',  ( -0.7071067811865487940, 0.7071067811865463515, 0.000000000000000000 ) ) ;
#97820 = FILL_AREA_STYLE ('',( #42034 ) ) ;
#97821 = LINE ( 'NONE', #130472, #1040 ) ;
#97822 = EDGE_CURVE ( 'NONE', #56334, #38475, #94369, .T. ) ;
#97823 = FACE_OUTER_BOUND ( 'NONE', #138361, .T. ) ;
#97824 = CARTESIAN_POINT ( 'NONE',  ( -10.95484226663327654, -21.74070752338406720, 21.72585301388582124 ) ) ;
#97825 = AXIS2_PLACEMENT_3D ( 'NONE', #107146, #39046, #48495 ) ;
#97826 = VECTOR ( 'NONE', #75594, 1000.000000000000000 ) ;
#97827 = VECTOR ( 'NONE', #31473, 1000.000000000000227 ) ;
#97828 = ADVANCED_FACE ( 'NONE', ( #84255 ), #105256, .T. ) ;
#97829 = DIRECTION ( 'NONE',  ( -0.000000000000000000, -0.3543493200069152693, 0.9351131265310292928 ) ) ;
#97830 = VECTOR ( 'NONE', #10074, 1000.000000000000000 ) ;
#97831 = CARTESIAN_POINT ( 'NONE',  ( 20.67183060077633883, 14.25929247661558286, 4.000000000000000000 ) ) ;
#97832 = ADVANCED_FACE ( 'NONE', ( #5203 ), #70543, .F. ) ;
#97833 = CARTESIAN_POINT ( 'NONE',  ( -18.48921356237309510, -27.52281430457068367, 5.000000000000000000 ) ) ;
#97834 = CARTESIAN_POINT ( 'NONE',  ( -36.18398860626899705, 28.73617430169812437, 5.000000000000000000 ) ) ;
#97835 = ADVANCED_FACE ( 'NONE', ( #128453 ), #48752, .F. ) ;
#97836 = VERTEX_POINT ( 'NONE', #137192 ) ;
#97837 = EDGE_LOOP ( 'NONE', ( #25641, #10310, #57204, #121178 ) ) ;
#97838 = AXIS2_PLACEMENT_3D ( 'NONE', #109527, #65347, #43558 ) ;
#97839 = VERTEX_POINT ( 'NONE', #126995 ) ;
#97840 = VECTOR ( 'NONE', #4070, 999.9999999999998863 ) ;
#97841 = ORIENTED_EDGE ( 'NONE', *, *, #21081, .T. ) ;
#97842 =( GEOMETRIC_REPRESENTATION_CONTEXT ( 3 ) GLOBAL_UNCERTAINTY_ASSIGNED_CONTEXT ( ( #53291 ) ) GLOBAL_UNIT_ASSIGNED_CONTEXT ( ( #101351, #34687, #26649 ) ) REPRESENTATION_CONTEXT ( 'NONE', 'WORKASPACE' ) );
#97843 = LINE ( 'NONE', #55784, #95814 ) ;
#97844 = ORIENTED_EDGE ( 'NONE', *, *, #82042, .F. ) ;
#97845 = ORIENTED_EDGE ( 'NONE', *, *, #35017, .T. ) ;
#97846 = CARTESIAN_POINT ( 'NONE',  ( -10.17183060077639922, 6.759292476615645029, 4.000000000000000000 ) ) ;
#97847 =( NAMED_UNIT ( * ) SI_UNIT ( $, .STERADIAN. ) SOLID_ANGLE_UNIT ( ) );
#97848 = ADVANCED_FACE ( 'NONE', ( #17521 ), #61778, .T. ) ;
#97849 = EDGE_CURVE ( 'NONE', #137076, #11057, #31284, .T. ) ;
#97850 = CARTESIAN_POINT ( 'NONE',  ( -35.99451991528749772, 28.92564299267963079, 4.000000000000000000 ) ) ;
#97851 = EDGE_LOOP ( 'NONE', ( #94206, #126410, #38129, #48492 ) ) ;
#97852 = CARTESIAN_POINT ( 'NONE',  ( -29.93988928955962336, -9.740707523384187994, 10.89222023123387828 ) ) ;
#97853 = EDGE_LOOP ( 'NONE', ( #143003, #118361 ) ) ;
#97854 = EDGE_CURVE ( 'NONE', #108587, #77009, #108788, .T. ) ;
#97855 = CARTESIAN_POINT ( 'NONE',  ( 3.850051285410223567, -8.240707523384193323, 17.25253755692239821 ) ) ;
#97856 = CARTESIAN_POINT ( 'NONE',  ( -21.18398860626899349, 28.73617430169802134, 5.000000000000000000 ) ) ;
#97857 = VECTOR ( 'NONE', #7636, 999.9999999999998863 ) ;
#97858 = CARTESIAN_POINT ( 'NONE',  ( 6.337903141435219823, -6.871911579029513106, -3.967499999999993587 ) ) ;
#97859 = VERTEX_POINT ( 'NONE', #64609 ) ;
#97860 = CARTESIAN_POINT ( 'NONE',  ( 96.16209685856478018, -5.291415217122919401, 3.054999999999998384 ) ) ;
#97861 = CARTESIAN_POINT ( 'NONE',  ( -14.51078643762690490, -27.52281430457045275, 5.000000000000000000 ) ) ;
#97862 = CARTESIAN_POINT ( 'NONE',  ( -30.18398860626900060, 28.73617430169808173, 5.000000000000000000 ) ) ;
#97863 = CARTESIAN_POINT ( 'NONE',  ( -75.18398860626899705, 28.73617430169839793, 5.000000000000000000 ) ) ;
#97864 = ORIENTED_EDGE ( 'NONE', *, *, #140890, .T. ) ;
#97865 = ORIENTED_EDGE ( 'NONE', *, *, #8982, .F. ) ;
#97866 = CARTESIAN_POINT ( 'NONE',  ( -57.48921356237308800, -27.52281430457095368, 5.000000000000000000 ) ) ;
#97867 = ORIENTED_EDGE ( 'NONE', *, *, #16833, .T. ) ;
#97868 = DIRECTION ( 'NONE',  ( 0.000000000000000000, -1.000000000000000000, 0.000000000000000000 ) ) ;
#97869 = LINE ( 'NONE', #42795, #55726 ) ;
#97870 = CARTESIAN_POINT ( 'NONE',  ( 3.183988606268992161, 28.73617430169789699, 5.000000000000000000 ) ) ;
#97871 = LINE ( 'NONE', #52217, #68113 ) ;
#97872 = ORIENTED_EDGE ( 'NONE', *, *, #94408, .T. ) ;
#97873 = VECTOR ( 'NONE', #12938, 1000.000000000000000 ) ;
#97874 = LINE ( 'NONE', #98574, #55331 ) ;
#97875 = AXIS2_PLACEMENT_3D ( 'NONE', #44600, #45302, #22064 ) ;
#97876 = CARTESIAN_POINT ( 'NONE',  ( -15.09843580608227143, 11.25929247661560240, 10.79108189686403563 ) ) ;
#97877 = FACE_OUTER_BOUND ( 'NONE', #10370, .T. ) ;
#97878 = EDGE_CURVE ( 'NONE', #56845, #112904, #40728, .T. ) ;
#97879 = ORIENTED_EDGE ( 'NONE', *, *, #68126, .T. ) ;
#97880 = DIRECTION ( 'NONE',  ( -0.6830127018922180770, -0.6830127018922204085, -0.2588190451025213501 ) ) ;
#97881 = VECTOR ( 'NONE', #84410, 1000.000000000000000 ) ;
#97882 = AXIS2_PLACEMENT_3D ( 'NONE', #101321, #70175, #134696 ) ;
#97883 = CARTESIAN_POINT ( 'NONE',  ( 10.37159235450332062, -2.500000000000000000, 3.061616997868384127E-16 ) ) ;
#97884 = ORIENTED_EDGE ( 'NONE', *, *, #48408, .F. ) ;
#97886 = ORIENTED_EDGE ( 'NONE', *, *, #54998, .T. ) ;
#97885 = CARTESIAN_POINT ( 'NONE',  ( 11.12514619309227193, -14.24070752338413648, 9.401115078912631873 ) ) ;
#97887 = ORIENTED_EDGE ( 'NONE', *, *, #77495, .T. ) ;
#97888 = DIRECTION ( 'NONE',  ( 0.3543493200069162685, -0.000000000000000000, -0.9351131265310288487 ) ) ;
#97889 = FACE_OUTER_BOUND ( 'NONE', #104685, .T. ) ;
#97890 = ORIENTED_EDGE ( 'NONE', *, *, #48108, .T. ) ;
#97891 = CARTESIAN_POINT ( 'NONE',  ( -10.17183060077640810, -20.24070752338407786, 4.000000000000000000 ) ) ;
#97892 = ADVANCED_FACE ( 'NONE', ( #75493 ), #96481, .F. ) ;
#97893 = VECTOR ( 'NONE', #96416, 1000.000000000000000 ) ;
#97894 = DIRECTION ( 'NONE',  ( 0.7071067811865487940, 0.7071067811865463515, 0.000000000000000000 ) ) ;
#97895 = DIRECTION ( 'NONE',  ( 3.115803279706882722E-16, -1.000000000000000000, 0.000000000000000000 ) ) ;
#97896 = DIRECTION ( 'NONE',  ( 0.7071067811865487940, 0.7071067811865463515, 0.000000000000000000 ) ) ;
#97897 = CARTESIAN_POINT ( 'NONE',  ( 113.0000000000000000, 0.000000000000000000, -7.950000000000000178 ) ) ;
#97898 = EDGE_CURVE ( 'NONE', #69227, #49314, #127059, .T. ) ;
#97899 = DIRECTION ( 'NONE',  ( -0.7071067811865486830, -0.7071067811865464625, 0.000000000000000000 ) ) ;
#97900 = AXIS2_PLACEMENT_3D ( 'NONE', #65556, #109726, #30764 ) ;
#97901 = CARTESIAN_POINT ( 'NONE',  ( 4.499999999999976019, 13.56627193232215767, -10.57019076586067641 ) ) ;
#97902 = FILL_AREA_STYLE ('',( #9413 ) ) ;
#97903 = CARTESIAN_POINT ( 'NONE',  ( 0.000000000000000000, -30.18000000000009564, -12.70000000000045404 ) ) ;
#97904 = CARTESIAN_POINT ( 'NONE',  ( 74.99451991528749772, 28.92564299267990435, 4.000000000000000000 ) ) ;
#97905 = AXIS2_PLACEMENT_3D ( 'NONE', #105050, #73166, #39833 ) ;
#97906 = DIRECTION ( 'NONE',  ( -0.6830127018922180770, -0.6830127018922204085, -0.2588190451025213501 ) ) ;
#97907 = CARTESIAN_POINT ( 'NONE',  ( -75.18398860626899705, 28.73617430169839793, 5.000000000000000000 ) ) ;
#97908 = CARTESIAN_POINT ( 'NONE',  ( -17.81601139373099940, 28.73617430169775133, 5.000000000000000000 ) ) ;
#97909 = ORIENTED_EDGE ( 'NONE', *, *, #135193, .T. ) ;
#97910 = ORIENTED_EDGE ( 'NONE', *, *, #113116, .F. ) ;
#97911 = ORIENTED_EDGE ( 'NONE', *, *, #122059, .F. ) ;
#97912 = CARTESIAN_POINT ( 'NONE',  ( 104.8333333333333286, -6.884901960086287964, 3.974999999999998312 ) ) ;
#97913 = ORIENTED_EDGE ( 'NONE', *, *, #17068, .T. ) ;
#97914 = ORIENTED_EDGE ( 'NONE', *, *, #26858, .F. ) ;
#97915 = EDGE_CURVE ( 'NONE', #106463, #121849, #9478, .T. ) ;
#97916 = ORIENTED_EDGE ( 'NONE', *, *, #125227, .F. ) ;
#97917 = DIRECTION ( 'NONE',  ( -0.000000000000000000, 0.000000000000000000, 1.000000000000000000 ) ) ;
#97918 = PLANE ( 'NONE',  #111089 ) ;
#97919 = VECTOR ( 'NONE', #8405, 1000.000000000000000 ) ;
#97920 = ORIENTED_EDGE ( 'NONE', *, *, #23391, .T. ) ;
#97921 = CARTESIAN_POINT ( 'NONE',  ( -9.707106781186471522, -6.740707523384216415, 5.000000000000000000 ) ) ;
#97922 = DIRECTION ( 'NONE',  ( 1.000000000000000000, 0.000000000000000000, 0.000000000000000000 ) ) ;
#97923 = PLANE ( 'NONE',  #41782 ) ;
#97924 = FACE_OUTER_BOUND ( 'NONE', #121076, .T. ) ;
#97925 = ADVANCED_FACE ( 'NONE', ( #42884 ), #53755, .F. ) ;
#97926 = ORIENTED_EDGE ( 'NONE', *, *, #28176, .F. ) ;
#97927 = CARTESIAN_POINT ( 'NONE',  ( 5.913250154378581591, 11.56455435889447436, -27.63405961019482149 ) ) ;
#97928 = PLANE ( 'NONE',  #112142 ) ;
#97929 = DIRECTION ( 'NONE',  ( 0.7071067811865487940, -0.7071067811865463515, 0.000000000000000000 ) ) ;
#97930 = CARTESIAN_POINT ( 'NONE',  ( 25.49999999999982236, -1.592773361805348342, -6.492772025301288608 ) ) ;
#97931 = DIRECTION ( 'NONE',  ( 0.7071067811865487940, 0.7071067811865463515, 0.000000000000000000 ) ) ;
#97932 = DIRECTION ( 'NONE',  ( -1.000000000000000000, -0.000000000000000000, -0.000000000000000000 ) ) ;
#97933 = CARTESIAN_POINT ( 'NONE',  ( 30.26669371712955581, -7.949999999999999289, 2.130196079827424427 ) ) ;
#97934 = CARTESIAN_POINT ( 'NONE',  ( 23.18753812416036908, -22.22500000000000142, 4.000000000000000000 ) ) ;
#97935 = ORIENTED_EDGE ( 'NONE', *, *, #52200, .T. ) ;
#97936 = ORIENTED_EDGE ( 'NONE', *, *, #90672, .T. ) ;
#97937 = CARTESIAN_POINT ( 'NONE',  ( 27.97916666666666430, -7.950000000000001066, 2.130196079827424427 ) ) ;
#97938 = VERTEX_POINT ( 'NONE', #129867 ) ;
#97939 = CARTESIAN_POINT ( 'NONE',  ( 13.13598696172163116, 4.584330080086930965E-16, 0.000000000000000000 ) ) ;
#97940 = LINE ( 'NONE', #42870, #124308 ) ;
#97941 = AXIS2_PLACEMENT_3D ( 'NONE', #81873, #12284, #59401 ) ;
#97942 = LINE ( 'NONE', #78335, #52643 ) ;
#97943 = FACE_OUTER_BOUND ( 'NONE', #138284, .T. ) ;
#97944 = VECTOR ( 'NONE', #84848, 1000.000000000000000 ) ;
#97945 = LINE ( 'NONE', #4, #28154 ) ;
#97947 = VECTOR ( 'NONE', #74300, 1000.000000000000114 ) ;
#97946 = PLANE ( 'NONE',  #30374 ) ;
#97948 = CARTESIAN_POINT ( 'NONE',  ( 127.3704301918981088, -3.055000000000001492, 5.291415217122917625 ) ) ;
#97949 = ADVANCED_FACE ( 'NONE', ( #29124 ), #52295, .F. ) ;
#97950 = ORIENTED_EDGE ( 'NONE', *, *, #22063, .T. ) ;
#97951 = ORIENTED_EDGE ( 'NONE', *, *, #112612, .T. ) ;
#97952 = VECTOR ( 'NONE', #98887, 999.9999999999998863 ) ;
#97953 = VECTOR ( 'NONE', #117605, 1000.000000000000000 ) ;
#97954 = DIRECTION ( 'NONE',  ( -0.6830127018922181881, 0.6830127018922202975, -0.2588190451025214056 ) ) ;
#97955 = LINE ( 'NONE', #75491, #59417 ) ;
#97956 = CARTESIAN_POINT ( 'NONE',  ( -12.54133533107846432, 22.22500000000000142, -3.482007288379135979 ) ) ;
#97957 = DIRECTION ( 'NONE',  ( 0.7071067811865487940, -0.7071067811865463515, 0.000000000000000000 ) ) ;
#97958 = ORIENTED_EDGE ( 'NONE', *, *, #40865, .F. ) ;
#97959 = CARTESIAN_POINT ( 'NONE',  ( 44.33376352523143993, 6.110000000000001208, 1.122388791418549305E-15 ) ) ;
#97960 = ORIENTED_EDGE ( 'NONE', *, *, #81111, .F. ) ;
#97961 = CARTESIAN_POINT ( 'NONE',  ( 3.469446951953614189E-15, -13.44781430457069327, 5.000000000000000000 ) ) ;
#97962 = EDGE_CURVE ( 'NONE', #131602, #18734, #142192, .T. ) ;
#97963 = DIRECTION ( 'NONE',  ( 0.7071067811865487940, 0.7071067811865463515, -0.000000000000000000 ) ) ;
#97964 = LINE ( 'NONE', #76952, #3861 ) ;
#97965 = FILL_AREA_STYLE_COLOUR ( '', #4324 ) ;
#97966 = PRODUCT_RELATED_PRODUCT_CATEGORY ( 'part', '', ( #120757 ) ) ;
#97967 = VECTOR ( 'NONE', #20479, 1000.000000000000000 ) ;
#97968 = CARTESIAN_POINT ( 'NONE',  ( 43.07876352523144448, -7.482591942790325086E-16, 6.109999999999998543 ) ) ;
#97969 = EDGE_LOOP ( 'NONE', ( #126943, #138611, #83331 ) ) ;
#97970 = DIRECTION ( 'NONE',  ( -0.7071067811865487940, 0.7071067811865463515, 0.000000000000000000 ) ) ;
#97971 = EDGE_LOOP ( 'NONE', ( #27344, #11684, #33577, #71780 ) ) ;
#97972 = ORIENTED_EDGE ( 'NONE', *, *, #5130, .T. ) ;
#97973 = EDGE_LOOP ( 'NONE', ( #68010, #122601, #81932, #33481 ) ) ;
#97974 = AXIS2_PLACEMENT_3D ( 'NONE', #34551, #3314, #124406 ) ;
#97975 = LINE ( 'NONE', #74085, #130927 ) ;
#97976 = CARTESIAN_POINT ( 'NONE',  ( 78.97502705046288440, -5.819803920172573086, 5.819803920172573086 ) ) ;
#97977 = ORIENTED_EDGE ( 'NONE', *, *, #116268, .F. ) ;
#97978 = VECTOR ( 'NONE', #31530, 1000.000000000000000 ) ;
#97979 = DIRECTION ( 'NONE',  ( -0.7071067811865487940, 0.7071067811865463515, -0.000000000000000000 ) ) ;
#97980 = LINE ( 'NONE', #120394, #43626 ) ;
#97981 = CARTESIAN_POINT ( 'NONE',  ( 6.707106781186496391, -3.740707523384244837, 5.000000000000000000 ) ) ;
#97982 = VECTOR ( 'NONE', #50444, 1000.000000000000000 ) ;
#97983 = FACE_BOUND ( 'NONE', #88609, .T. ) ;
#97984 = EDGE_LOOP ( 'NONE', ( #19822, #40311, #95689, #5630 ) ) ;
#97985 = FACE_OUTER_BOUND ( 'NONE', #120665, .T. ) ;
#97986 = DIRECTION ( 'NONE',  ( 1.000000000000000000, 0.000000000000000000, 0.000000000000000000 ) ) ;
#97987 = CARTESIAN_POINT ( 'NONE',  ( 36.48921356237310221, -27.52281430457080802, 5.000000000000000000 ) ) ;
#97988 = ORIENTED_EDGE ( 'NONE', *, *, #122637, .F. ) ;
#97989 = VERTEX_POINT ( 'NONE', #87079 ) ;
#97990 = ORIENTED_EDGE ( 'NONE', *, *, #138240, .F. ) ;
#97991 = ORIENTED_EDGE ( 'NONE', *, *, #41950, .T. ) ;
#97992 = VECTOR ( 'NONE', #116050, 1000.000000000000000 ) ;
#97993 = EDGE_CURVE ( 'NONE', #48713, #135328, #18961, .T. ) ;
#97994 = CARTESIAN_POINT ( 'NONE',  ( 58.97459685856478018, 1.637169565754164280, -6.109999999999996767 ) ) ;
#97996 = VERTEX_POINT ( 'NONE', #31977 ) ;
#97995 = VECTOR ( 'NONE', #56900, 999.9999999999998863 ) ;
#97997 =( BOUNDED_CURVE ( )  B_SPLINE_CURVE ( 2, ( #82565, #54079, #119970, #115146, #98267, #126755, #141783, #41739, #130189, #119277, #15819, #37651, #71699 ),
 .UNSPECIFIED., .F., .T. ) 
 B_SPLINE_CURVE_WITH_KNOTS ( ( 3, 2, 2, 2, 2, 2, 3 ),
 ( 0.1833333333333333481, 0.1861111111111111438, 0.1888888888888889117, 0.1916666666666667074, 0.1944444444444444753, 0.1972222222222222432, 0.2000000000000000389 ),
 .UNSPECIFIED. ) 
 CURVE ( )  GEOMETRIC_REPRESENTATION_ITEM ( )  RATIONAL_B_SPLINE_CURVE ( ( 0.9999999999999996669, 0.9659258262890686453, 1.000000000000000000, 0.9659258262890683122, 1.000000000000000000, 0.9659258262890683122, 1.000000000000000000, 0.9659258262890683122, 1.000000000000000000, 0.9659258262890683122, 1.000000000000000000, 0.9659258262890679791, 1.000000000000000444 ) ) 
 REPRESENTATION_ITEM ( '' )  );
#97998 = PLANE ( 'NONE',  #134426 ) ;
#98000 = EDGE_LOOP ( 'NONE', ( #40078, #141539, #39941, #109402 ) ) ;
#97999 = EDGE_CURVE ( 'NONE', #116750, #54134, #18208, .T. ) ;
#98001 = LINE ( 'NONE', #99387, #116758 ) ;
#98002 = CARTESIAN_POINT ( 'NONE',  ( -18.29974487139159223, -27.71228299555219010, 4.000000000000000000 ) ) ;
#98003 = VERTEX_POINT ( 'NONE', #7349 ) ;
#98004 = ADVANCED_FACE ( 'NONE', ( #107393 ), #8742, .F. ) ;
#98005 = CARTESIAN_POINT ( 'NONE',  ( 34.92499999999998295, 15.85612307739225280, 4.000000000000000000 ) ) ;
#98006 = DIRECTION ( 'NONE',  ( -0.7071067811865487940, 0.7071067811865463515, -0.000000000000000000 ) ) ;
#98007 = AXIS2_PLACEMENT_3D ( 'NONE', #120528, #76359, #36246 ) ;
#98008 = EDGE_CURVE ( 'NONE', #95760, #113826, #97783, .T. ) ;
#98009 = DIRECTION ( 'NONE',  ( 0.7071067811865487940, -0.7071067811865463515, 0.000000000000000000 ) ) ;
#98010 = FACE_OUTER_BOUND ( 'NONE', #44158, .T. ) ;
#98011 = DIRECTION ( 'NONE',  ( 0.3543493200069163240, -0.000000000000000000, 0.9351131265310288487 ) ) ;
#98012 = DIRECTION ( 'NONE',  ( 0.7071067811865487940, -0.7071067811865463515, -0.000000000000000000 ) ) ;
#98013 = PLANE ( 'NONE',  #132021 ) ;
#98014 = ORIENTED_EDGE ( 'NONE', *, *, #141059, .T. ) ;
#98016 = EDGE_LOOP ( 'NONE', ( #110735, #15013, #136883, #103641 ) ) ;
#98015 = VECTOR ( 'NONE', #17024, 1000.000000000000000 ) ;
#98017 = ORIENTED_EDGE ( 'NONE', *, *, #110234, .T. ) ;
#98018 = CARTESIAN_POINT ( 'NONE',  ( 33.81246187583924723, -22.22500000000000142, 4.000000000000000000 ) ) ;
#98019 = LINE ( 'NONE', #43624, #60737 ) ;
#98020 = VERTEX_POINT ( 'NONE', #63751 ) ;
#98021 = ORIENTED_EDGE ( 'NONE', *, *, #80512, .F. ) ;
#98022 = LINE ( 'NONE', #140114, #123030 ) ;
#98024 = ADVANCED_FACE ( 'NONE', ( #142030 ), #53580, .F. ) ;
#98023 = LINE ( 'NONE', #20433, #115042 ) ;
#98025 = ADVANCED_FACE ( 'NONE', ( #76783 ), #99931, .F. ) ;
#98026 = DIRECTION ( 'NONE',  ( -1.000000000000000000, -1.224606353822377258E-16, -0.000000000000000000 ) ) ;
#98027 = VECTOR ( 'NONE', #46828, 999.9999999999998863 ) ;
#98028 = ORIENTED_EDGE ( 'NONE', *, *, #62976, .T. ) ;
#98029 = CARTESIAN_POINT ( 'NONE',  ( 0.000000000000000000, 0.000000000000000000, 5.000000000000000000 ) ) ;
#98030 = EDGE_CURVE ( 'NONE', #139938, #131028, #109371, .T. ) ;
#98031 = DIRECTION ( 'NONE',  ( -1.000000000000000000, -1.224606353822377258E-16, -0.000000000000000000 ) ) ;
#98032 = CARTESIAN_POINT ( 'NONE',  ( 17.27540314143521627, -2.126176841940958351, -7.934999999999989839 ) ) ;
#98033 = VECTOR ( 'NONE', #140437, 1000.000000000000000 ) ;
#98034 = DIRECTION ( 'NONE',  ( -0.000000000000000000, -0.3543493200069152693, 0.9351131265310292928 ) ) ;
#98035 = ORIENTED_EDGE ( 'NONE', *, *, #93280, .T. ) ;
#98036 = CARTESIAN_POINT ( 'NONE',  ( 120.8079301918980946, -6.109999999999999432, 1.637169565754158507 ) ) ;
#98037 = CARTESIAN_POINT ( 'NONE',  ( -63.48921356237309510, -27.52281430457099631, 5.000000000000000000 ) ) ;
#98038 = CARTESIAN_POINT ( 'NONE',  ( 14.99999999999990230, -0.2811185226894094558, -5.995736974527545726 ) ) ;
#98039 = EDGE_CURVE ( 'NONE', #2079, #79854, #98298, .T. ) ;
#98041 = VERTEX_POINT ( 'NONE', #64440 ) ;
#98040 = CARTESIAN_POINT ( 'NONE',  ( 9.793339364578407924, 21.75929247661549937, 4.998822639870711626 ) ) ;
#98042 = CARTESIAN_POINT ( 'NONE',  ( -32.99451991528749062, 28.92564299267960948, 4.000000000000000000 ) ) ;
#98043 = VERTEX_POINT ( 'NONE', #74627 ) ;
#98044 = CARTESIAN_POINT ( 'NONE',  ( -25.49999999999982236, -4.533600742197692490, 5.000000000000000000 ) ) ;
#98045 = DIRECTION ( 'NONE',  ( -8.817971600062198362E-18, -0.3543493200069152693, 0.9351131265310292928 ) ) ;
#98046 = LINE ( 'NONE', #87162, #139806 ) ;
#98048 = VERTEX_POINT ( 'NONE', #20921 ) ;
#98047 = VECTOR ( 'NONE', #20248, 1000.000000000000000 ) ;
#98049 = CARTESIAN_POINT ( 'NONE',  ( 23.99451991528749062, 28.92564299267954908, 4.000000000000000000 ) ) ;
#98050 = DIRECTION ( 'NONE',  ( -1.000000000000000000, -1.224606353822377258E-16, -0.000000000000000000 ) ) ;
#98051 = EDGE_CURVE ( 'NONE', #79346, #98685, #52956, .T. ) ;
#98052 = VECTOR ( 'NONE', #28512, 999.9999999999998863 ) ;
#98053 = ORIENTED_EDGE ( 'NONE', *, *, #2673, .T. ) ;
#98054 = CARTESIAN_POINT ( 'NONE',  ( -24.48921356237309510, -27.52281430457072631, 5.000000000000000000 ) ) ;
#98055 = CARTESIAN_POINT ( 'NONE',  ( 21.18398860626899349, 28.73617430169802134, 5.000000000000000000 ) ) ;
#98056 = ORIENTED_EDGE ( 'NONE', *, *, #37958, .T. ) ;
#98057 = DIRECTION ( 'NONE',  ( -0.7071067811865486830, -0.7071067811865464625, -0.000000000000000000 ) ) ;
#98058 = DIRECTION ( 'NONE',  ( 0.7071067811865486830, -0.7071067811865464625, -0.000000000000000000 ) ) ;
#98059 = ORIENTED_EDGE ( 'NONE', *, *, #10048, .T. ) ;
#98060 = VERTEX_POINT ( 'NONE', #120209 ) ;
#98061 = DIRECTION ( 'NONE',  ( -0.3543493200069162685, -0.000000000000000000, -0.9351131265310288487 ) ) ;
#98062 = LINE ( 'NONE', #10313, #76047 ) ;
#98063 = VECTOR ( 'NONE', #64650, 1000.000000000000227 ) ;
#98064 = ADVANCED_FACE ( 'NONE', ( #10053 ), #131854, .F. ) ;
#98065 = DIRECTION ( 'NONE',  ( 0.000000000000000000, -1.000000000000000000, 0.000000000000000000 ) ) ;
#98066 = PRESENTATION_LAYER_ASSIGNMENT (  '', '', ( #858 ) ) ;
#98067 = FACE_OUTER_BOUND ( 'NONE', #16215, .T. ) ;
#98068 = DIRECTION ( 'NONE',  ( -0.6830127018922181881, 0.6830127018922202975, -0.2588190451025214056 ) ) ;
#98069 = ORIENTED_EDGE ( 'NONE', *, *, #138255, .T. ) ;
#98070 = DIRECTION ( 'NONE',  ( -0.000000000000000000, -0.000000000000000000, 1.000000000000000000 ) ) ;
#98071 = DIRECTION ( 'NONE',  ( 0.3543493200069162685, -0.000000000000000000, -0.9351131265310288487 ) ) ;
#98072 = CARTESIAN_POINT ( 'NONE',  ( -14.99999999999990230, 7.559798855135676732, 4.979909187984716823 ) ) ;
#98073 = CARTESIAN_POINT ( 'NONE',  ( -34.92500000000001137, 22.22500000000000142, 4.000000000000000000 ) ) ;
#98074 = CARTESIAN_POINT ( 'NONE',  ( 34.62043019189811588, 3.055000000000002380, -5.291415217122917625 ) ) ;
#98075 = VECTOR ( 'NONE', #42249, 1000.000000000000000 ) ;
#98076 = VERTEX_POINT ( 'NONE', #20196 ) ;
#98077 = ORIENTED_EDGE ( 'NONE', *, *, #5232, .F. ) ;
#98078 = DIRECTION ( 'NONE',  ( -0.7071067811865487940, 0.7071067811865463515, -0.000000000000000000 ) ) ;
#98079 = VECTOR ( 'NONE', #62569, 999.9999999999998863 ) ;
#98080 = ORIENTED_EDGE ( 'NONE', *, *, #5215, .T. ) ;
#98081 = EDGE_CURVE ( 'NONE', #135356, #79591, #88357, .T. ) ;
#98083 = VERTEX_POINT ( 'NONE', #8577 ) ;
#98082 = B_SPLINE_CURVE_WITH_KNOTS ( 'NONE', 3,
 ( #50041, #138473, #75363, #61646 ),
 .UNSPECIFIED., .F., .F.,
 ( 4, 4 ),
 ( 0.009196836153558695173, 0.009397116448368620506 ),
 .UNSPECIFIED. ) ;
#98084 = CARTESIAN_POINT ( 'NONE',  ( 25.17183060077629264, 3.759292476615674783, 4.000000000000000000 ) ) ;
#98085 = FACE_OUTER_BOUND ( 'NONE', #91633, .T. ) ;
#98086 = VERTEX_POINT ( 'NONE', #99180 ) ;
#98087 = CARTESIAN_POINT ( 'NONE',  ( 45.29974487139158867, -27.71228299555237840, 4.000000000000000000 ) ) ;
#98089 = CIRCLE ( 'NONE', #95803, 2.500000000000000444 ) ;
#98088 = LINE ( 'NONE', #97331, #132234 ) ;
#98090 = CARTESIAN_POINT ( 'NONE',  ( -33.70710678118629744, -15.74070752338412760, 5.000000000000000000 ) ) ;
#98091 = PLANE ( 'NONE',  #58128 ) ;
#98092 = DIRECTION ( 'NONE',  ( -0.7071067811865486830, -0.7071067811865464625, -0.000000000000000000 ) ) ;
#98093 = EDGE_CURVE ( 'NONE', #76846, #77009, #44133, .T. ) ;
#98094 = ORIENTED_EDGE ( 'NONE', *, *, #122647, .T. ) ;
#98095 = CARTESIAN_POINT ( 'NONE',  ( -10.49999999999992539, -4.216083040037264418, -7.486842126848634038 ) ) ;
#98096 = CARTESIAN_POINT ( 'NONE',  ( 17.51078643762690845, -27.52281430457043143, 5.000000000000000000 ) ) ;
#98097 = CARTESIAN_POINT ( 'NONE',  ( -15.48921356237309510, -27.52281430457066236, 5.000000000000000000 ) ) ;
#98098 = CARTESIAN_POINT ( 'NONE',  ( 0.2069207719830578884, 4.031931619714366200, -6.831241579940219744 ) ) ;
#98099 = FACE_OUTER_BOUND ( 'NONE', #50800, .T. ) ;
#98100 = DIRECTION ( 'NONE',  ( -0.6830127018922181881, 0.6830127018922202975, -0.2588190451025214056 ) ) ;
#98101 = PLANE ( 'NONE',  #24980 ) ;
#98102 = AXIS2_PLACEMENT_3D ( 'NONE', #91738, #100497, #44728 ) ;
#98103 = CARTESIAN_POINT ( 'NONE',  ( 55.78752705046288440, 0.000000000000000000, -7.949999999999998401 ) ) ;
#98104 = VECTOR ( 'NONE', #86963, 1000.000000000000000 ) ;
#98105 = CARTESIAN_POINT ( 'NONE',  ( 29.99451991528749417, 28.92564299267958816, 4.000000000000000000 ) ) ;
#98106 = ORIENTED_EDGE ( 'NONE', *, *, #75237, .F. ) ;
#98107 = ORIENTED_EDGE ( 'NONE', *, *, #3894, .F. ) ;
#98108 = CARTESIAN_POINT ( 'NONE',  ( 52.91666666666666430, -6.884901960086287076, -3.975000000000000977 ) ) ;
#98109 = CARTESIAN_POINT ( 'NONE',  ( 27.29974487139158512, -27.71228299555225405, 4.000000000000000000 ) ) ;
#98110 = CARTESIAN_POINT ( 'NONE',  ( -29.38161509397986038, -2.240707523384260824, 13.37739548510246124 ) ) ;
#98111 = COLOUR_RGB ( '', 0.31764706, 0.68627451, 0.89019608) ;
#98112 = DIRECTION ( 'NONE',  ( 0.3543493200069162685, -0.000000000000000000, -0.9351131265310288487 ) ) ;
#98113 = VERTEX_POINT ( 'NONE', #21661 ) ;
#98114 = LINE ( 'NONE', #143038, #36311 ) ;
#98115 = CARTESIAN_POINT ( 'NONE',  ( -25.22850677138649189, 20.25929247661551003, 7.808871592221711566 ) ) ;
#98116 = CARTESIAN_POINT ( 'NONE',  ( 47.39626352523143282, 4.472830434245840259, -4.472830434245839371 ) ) ;
#98117 = EDGE_CURVE ( 'NONE', #103874, #59558, #111313, .T. ) ;
#98118 = ORIENTED_EDGE ( 'NONE', *, *, #96630, .F. ) ;
#98119 = CARTESIAN_POINT ( 'NONE',  ( -34.49999999999975131, -4.535744391599457082, 4.994342998332168548 ) ) ;
#98120 = ORIENTED_EDGE ( 'NONE', *, *, #32298, .T. ) ;
#98121 = ORIENTED_EDGE ( 'NONE', *, *, #68574, .T. ) ;
#98122 = AXIS2_PLACEMENT_3D ( 'NONE', #128539, #18300, #137989 ) ;
#98123 = CARTESIAN_POINT ( 'NONE',  ( 54.18398860626899705, 28.73617430169825226, 5.000000000000000000 ) ) ;
#98124 = CARTESIAN_POINT ( 'NONE',  ( 15.75000000000000000, -7.464222240803106570E-16, -6.094999999999989981 ) ) ;
#98125 = DIRECTION ( 'NONE',  ( -0.7071067811865486830, -0.7071067811865464625, 0.000000000000000000 ) ) ;
#98126 = CARTESIAN_POINT ( 'NONE',  ( 20.99451991528748707, 28.92564299267952777, 4.000000000000000000 ) ) ;
#98128 = ADVANCED_FACE ( 'NONE', ( #86205 ), #75337, .F. ) ;
#98127 = ORIENTED_EDGE ( 'NONE', *, *, #11279, .F. ) ;
#98129 = DIRECTION ( 'NONE',  ( 0.6830127018922180770, -0.6830127018922204085, -0.2588190451025213501 ) ) ;
#98130 = DIRECTION ( 'NONE',  ( -0.7071067811865486830, 0.7071067811865464625, 0.000000000000000000 ) ) ;
#98132 = ORIENTED_EDGE ( 'NONE', *, *, #46303, .F. ) ;
#98131 = PLANE ( 'NONE',  #31421 ) ;
#98133 = CARTESIAN_POINT ( 'NONE',  ( 80.35459685856476142, -1.637169565754161615, 6.110000000000000320 ) ) ;
#98134 = EDGE_CURVE ( 'NONE', #71727, #48744, #108623, .T. ) ;
#98135 = LINE ( 'NONE', #43050, #71728 ) ;
#98136 = LINE ( 'NONE', #53181, #29257 ) ;
#98137 = VECTOR ( 'NONE', #26107, 1000.000000000000000 ) ;
#98138 = CARTESIAN_POINT ( 'NONE',  ( 1.592112669765240796, -0.4000000000000004108, 2.358007193124715073 ) ) ;
#98139 = CARTESIAN_POINT ( 'NONE',  ( -13.49999999999990408, 19.39370406404965763, 1.459788787078232897 ) ) ;
#98140 = CARTESIAN_POINT ( 'NONE',  ( 30.18398860626900060, 28.73617430169808173, 5.000000000000000000 ) ) ;
#98141 = ORIENTED_EDGE ( 'NONE', *, *, #136752, .T. ) ;
#98142 = VECTOR ( 'NONE', #36509, 1000.000000000000227 ) ;
#98143 = CARTESIAN_POINT ( 'NONE',  ( -11.99999999999991296, 14.96639925780211478, 5.000000000000000000 ) ) ;
#98144 = CARTESIAN_POINT ( 'NONE',  ( 68.59959685856476597, -6.109999999999997655, -1.637169565754160283 ) ) ;
#98145 = PLANE ( 'NONE',  #60308 ) ;
#98146 = DIRECTION ( 'NONE',  ( 0.000000000000000000, 1.000000000000000000, 0.000000000000000000 ) ) ;
#98147 = ORIENTED_EDGE ( 'NONE', *, *, #25210, .T. ) ;
#98148 = ORIENTED_EDGE ( 'NONE', *, *, #61510, .F. ) ;
#98149 = DIRECTION ( 'NONE',  ( -0.7071067811865486830, 0.7071067811865464625, 0.000000000000000000 ) ) ;
#98150 = PLANE ( 'NONE',  #46891 ) ;
#98151 = VERTEX_POINT ( 'NONE', #143425 ) ;
#98152 = EDGE_CURVE ( 'NONE', #44496, #44686, #132596, .T. ) ;
#98153 = AXIS2_PLACEMENT_3D ( 'NONE', #108661, #118120, #131172 ) ;
#98154 = ORIENTED_EDGE ( 'NONE', *, *, #40918, .T. ) ;
#98155 = CARTESIAN_POINT ( 'NONE',  ( 24.18398860626899705, 28.73617430169804265, 5.000000000000000000 ) ) ;
#98156 = ORIENTED_EDGE ( 'NONE', *, *, #45813, .F. ) ;
#98157 = DIRECTION ( 'NONE',  ( 0.7071067811865486830, -0.7071067811865464625, -0.000000000000000000 ) ) ;
#98158 = CARTESIAN_POINT ( 'NONE',  ( 10.49999999999992539, 6.431123077392117082, 4.000000000000000000 ) ) ;
#98159 = CARTESIAN_POINT ( 'NONE',  ( -7.140000000000001457, -35.62921248010920294, -8.151379605006853879 ) ) ;
#98160 = FACE_BOUND ( 'NONE', #76946, .T. ) ;
#98161 = CARTESIAN_POINT ( 'NONE',  ( -34.42500000000001137, -21.72500000000000142, 4.500000000000000888 ) ) ;
#98162 = LINE ( 'NONE', #76421, #72115 ) ;
#98163 = CARTESIAN_POINT ( 'NONE',  ( 15.98840764549667703, -3.851859888774471706E-31, 2.500000000000001332 ) ) ;
#98165 = ORIENTED_EDGE ( 'NONE', *, *, #122164, .T. ) ;
#98164 = CARTESIAN_POINT ( 'NONE',  ( -31.92499999999997584, -22.26999999999999247, -39.50000000000000000 ) ) ;
#98166 = VECTOR ( 'NONE', #131529, 999.9999999999998863 ) ;
#98167 = CARTESIAN_POINT ( 'NONE',  ( 31.74845587132405811, -11.24070752338416135, 10.39518518046001994 ) ) ;
#98168 = ORIENTED_EDGE ( 'NONE', *, *, #107260, .T. ) ;
#98169 = VECTOR ( 'NONE', #129273, 1000.000000000000000 ) ;
#98171 = VERTEX_POINT ( 'NONE', #24499 ) ;
#98170 = EDGE_CURVE ( 'NONE', #89800, #56401, #66599, .T. ) ;
#98172 = CARTESIAN_POINT ( 'NONE',  ( 80.41209685856479439, 5.291415217122921177, -3.054999999999994831 ) ) ;
#98173 = VERTEX_POINT ( 'NONE', #113647 ) ;
#98174 = PLANE ( 'NONE',  #81443 ) ;
#98175 = EDGE_CURVE ( 'NONE', #96223, #135001, #74292, .T. ) ;
#98176 = VERTEX_POINT ( 'NONE', #45584 ) ;
#98177 = DIRECTION ( 'NONE',  ( -0.000000000000000000, 0.000000000000000000, 1.000000000000000000 ) ) ;
#98178 = EDGE_CURVE ( 'NONE', #122443, #81871, #47731, .T. ) ;
#98179 = ADVANCED_FACE ( 'NONE', ( #36806 ), #34685, .F. ) ;
#98180 = CARTESIAN_POINT ( 'NONE',  ( 0.000000000000000000, 9.735942053221458872E-16, -7.950000000000000178 ) ) ;
#98181 = LINE ( 'NONE', #141691, #36792 ) ;
#98182 = FACE_OUTER_BOUND ( 'NONE', #101044, .T. ) ;
#98183 = VECTOR ( 'NONE', #121204, 1000.000000000000227 ) ;
#98184 = CARTESIAN_POINT ( 'NONE',  ( 28.37176554955598462, -8.240707523384193323, 11.38925528200746129 ) ) ;
#98185 = PLANE ( 'NONE',  #5292 ) ;
#98186 = DIRECTION ( 'NONE',  ( -1.000000000000000000, -1.224606353822377258E-16, -0.000000000000000000 ) ) ;
#98187 = ORIENTED_EDGE ( 'NONE', *, *, #53650, .T. ) ;
#98188 = ORIENTED_EDGE ( 'NONE', *, *, #30583, .F. ) ;
#98189 = CARTESIAN_POINT ( 'NONE',  ( 123.6000270504628844, 5.819803920172570422, 5.819803920172575751 ) ) ;
#98190 = DIRECTION ( 'NONE',  ( 0.6830127018922180770, -0.6830127018922204085, -0.2588190451025213501 ) ) ;
#98191 = AXIS2_PLACEMENT_3D ( 'NONE', #40825, #77047, #107495 ) ;
#98192 = VERTEX_POINT ( 'NONE', #78918 ) ;
#98193 = VERTEX_POINT ( 'NONE', #134734 ) ;
#98195 = EDGE_CURVE ( 'NONE', #119529, #120251, #12193, .T. ) ;
#98194 = LINE ( 'NONE', #43811, #56852 ) ;
#98196 = CONICAL_SURFACE ( 'NONE', #126036, 2.500000000000000888, 0.9599310885968822538 ) ;
#98197 = EDGE_CURVE ( 'NONE', #50863, #103304, #36120, .T. ) ;
#98198 = CARTESIAN_POINT ( 'NONE',  ( 32.52126352523143282, -4.472830434245838482, -4.472830434245840259 ) ) ;
#98199 = EDGE_LOOP ( 'NONE', ( #123979, #35100, #93289, #119798 ) ) ;
#98200 = CARTESIAN_POINT ( 'NONE',  ( -20.90332935812582349, -2.240707523384260824, 15.26439735382747642 ) ) ;
#98201 = VECTOR ( 'NONE', #12576, 1000.000000000000000 ) ;
#98202 = LINE ( 'NONE', #77876, #74801 ) ;
#98203 = VECTOR ( 'NONE', #122810, 1000.000000000000227 ) ;
#98204 = CARTESIAN_POINT ( 'NONE',  ( 27.46247294953710849, -7.464222240803106570E-16, -6.094999999999989981 ) ) ;
#98205 = CARTESIAN_POINT ( 'NONE',  ( 1.945313545083072748, 12.48888505241799152, -25.34115511373076046 ) ) ;
#98206 = ADVANCED_FACE ( 'NONE', ( #136116 ), #68755, .T. ) ;
#98207 = ORIENTED_EDGE ( 'NONE', *, *, #136004, .T. ) ;
#98208 = VERTEX_POINT ( 'NONE', #101349 ) ;
#98209 = FACE_OUTER_BOUND ( 'NONE', #101729, .T. ) ;
#98210 = CARTESIAN_POINT ( 'NONE',  ( -36.18398860626899705, 28.73617430169812437, 5.000000000000000000 ) ) ;
#98211 = EDGE_CURVE ( 'NONE', #76142, #132249, #68068, .T. ) ;
#98213 = ORIENTED_EDGE ( 'NONE', *, *, #55183, .T. ) ;
#98212 = LINE ( 'NONE', #22049, #16945 ) ;
#98214 = ORIENTED_EDGE ( 'NONE', *, *, #91810, .F. ) ;
#98215 = DIRECTION ( 'NONE',  ( -0.7071067811865486830, -0.7071067811865464625, 0.000000000000000000 ) ) ;
#98216 = CARTESIAN_POINT ( 'NONE',  ( -25.39999999999996305, 0.000000000000000000, 0.000000000000000000 ) ) ;
#98217 = PLANE ( 'NONE',  #86502 ) ;
#98218 = ORIENTED_EDGE ( 'NONE', *, *, #141379, .T. ) ;
#98219 = DIRECTION ( 'NONE',  ( 0.7071067811865487940, 0.7071067811865463515, 0.000000000000000000 ) ) ;
#98220 = ORIENTED_EDGE ( 'NONE', *, *, #109766, .T. ) ;
#98221 = VERTEX_POINT ( 'NONE', #47042 ) ;
#98222 = ORIENTED_EDGE ( 'NONE', *, *, #111138, .F. ) ;
#98223 = FACE_OUTER_BOUND ( 'NONE', #13720, .T. ) ;
#98224 = CARTESIAN_POINT ( 'NONE',  ( 34.75611968250419181, 11.81293425470726710, 4.955485411084880276 ) ) ;
#98226 = EDGE_CURVE ( 'NONE', #22380, #27557, #70209, .T. ) ;
#98225 = AXIS2_PLACEMENT_3D ( 'NONE', #67402, #140139, #23115 ) ;
#98227 = DIRECTION ( 'NONE',  ( 0.6830127018922181881, 0.6830127018922202975, -0.2588190451025214056 ) ) ;
#98228 = FACE_OUTER_BOUND ( 'NONE', #33770, .T. ) ;
#98229 = DIRECTION ( 'NONE',  ( -0.7071067811865487940, 0.7071067811865463515, -0.000000000000000000 ) ) ;
#98230 = CARTESIAN_POINT ( 'NONE',  ( 10.49999999999992539, -16.53360074219757081, 5.000000000000000000 ) ) ;
#98231 = CARTESIAN_POINT ( 'NONE',  ( -11.29289321881337393, 20.25929247661551003, 5.000000000000000000 ) ) ;
#98232 = ORIENTED_EDGE ( 'NONE', *, *, #70512, .F. ) ;
#98233 = DIRECTION ( 'NONE',  ( 0.7071067811865487940, -0.7071067811865463515, 0.000000000000000000 ) ) ;
#98234 = EDGE_CURVE ( 'NONE', #85558, #132912, #112242, .T. ) ;
#98235 = ORIENTED_EDGE ( 'NONE', *, *, #124054, .T. ) ;
#98236 = ADVANCED_FACE ( 'NONE', ( #13605 ), #125250, .T. ) ;
#98237 = CARTESIAN_POINT ( 'NONE',  ( -33.79289321881321939, -11.24070752338416668, 5.000000000000000000 ) ) ;
#98238 = EDGE_CURVE ( 'NONE', #86975, #39389, #114369, .T. ) ;
#98239 = DIRECTION ( 'NONE',  ( -0.000000000000000000, 0.000000000000000000, 1.000000000000000000 ) ) ;
#98240 = EDGE_LOOP ( 'NONE', ( #42360, #70776, #47448, #25750 ) ) ;
#98241 = DIRECTION ( 'NONE',  ( 0.7071067811865487940, 0.7071067811865463515, 0.000000000000000000 ) ) ;
#98242 = CARTESIAN_POINT ( 'NONE',  ( 12.19999999999999574, -40.43000000000000682, -40.00000000000000000 ) ) ;
#98243 = SURFACE_SIDE_STYLE ('',( #29393 ) ) ;
#98244 = ORIENTED_EDGE ( 'NONE', *, *, #18097, .T. ) ;
#98245 = ORIENTED_EDGE ( 'NONE', *, *, #78454, .T. ) ;
#98246 = SURFACE_SIDE_STYLE ('',( #66344 ) ) ;
#98247 = CARTESIAN_POINT ( 'NONE',  ( -20.20710678118640402, -11.24070752338416312, 5.000000000000000000 ) ) ;
#98248 = DIRECTION ( 'NONE',  ( 0.000000000000000000, 0.000000000000000000, 1.000000000000000000 ) ) ;
#98249 = FILL_AREA_STYLE ('',( #142473 ) ) ;
#98250 = ADVANCED_FACE ( 'NONE', ( #14345 ), #133293, .F. ) ;
#98251 = PLANE ( 'NONE',  #103790 ) ;
#98252 = CARTESIAN_POINT ( 'NONE',  ( 69.32876352523145158, 0.000000000000000000, -6.109999999999999432 ) ) ;
#98253 = VECTOR ( 'NONE', #66450, 1000.000000000000000 ) ;
#98254 = DIRECTION ( 'NONE',  ( -0.000000000000000000, -0.3543493200069152693, 0.9351131265310292928 ) ) ;
#98255 =( NAMED_UNIT ( * ) SI_UNIT ( $, .STERADIAN. ) SOLID_ANGLE_UNIT ( ) );
#98256 = DIRECTION ( 'NONE',  ( -0.5735764363510507113, 0.8191520442889885789, 1.003171929053520926E-16 ) ) ;
#98257 = CARTESIAN_POINT ( 'NONE',  ( 83.83333333333332860, -6.884901960086287964, 3.974999999999998312 ) ) ;
#98258 = ORIENTED_EDGE ( 'NONE', *, *, #71358, .F. ) ;
#98259 = CARTESIAN_POINT ( 'NONE',  ( -17.72082203615853047, 8.995094813919580545, 4.338987337627234098 ) ) ;
#98260 = VERTEX_POINT ( 'NONE', #23801 ) ;
#98261 = DIRECTION ( 'NONE',  ( -0.7071067811865486830, -0.7071067811865464625, 0.000000000000000000 ) ) ;
#98262 = CARTESIAN_POINT ( 'NONE',  ( -26.99999999999981526, 19.93112307739197675, 4.000000000000000000 ) ) ;
#98263 = EDGE_LOOP ( 'NONE', ( #23255, #4104 ) ) ;
#98264 = PLANE ( 'NONE',  #18271 ) ;
#98266 = EDGE_LOOP ( 'NONE', ( #107119, #23974, #31720, #25769 ) ) ;
#98265 = DIRECTION ( 'NONE',  ( -0.3543493200069162685, -0.000000000000000000, -0.9351131265310288487 ) ) ;
#98267 = CARTESIAN_POINT ( 'NONE',  ( 107.1666666666666572, 6.884901960086285300, 3.975000000000003642 ) ) ;
#98268 = CARTESIAN_POINT ( 'NONE',  ( 30.75860074219774631, 21.72500000000000142, 5.000000000000000000 ) ) ;
#98269 = CARTESIAN_POINT ( 'NONE',  ( -11.20710678118646619, -2.240707523384255939, 5.000000000000000000 ) ) ;
#98270 = ORIENTED_EDGE ( 'NONE', *, *, #70258, .T. ) ;
#98271 = EDGE_LOOP ( 'NONE', ( #34580, #27014, #11842, #112751 ) ) ;
#98272 = CARTESIAN_POINT ( 'NONE',  ( 127.1386022459138019, -7.776507174585692163E-16, 6.349999999999999645 ) ) ;
#98273 = DIRECTION ( 'NONE',  ( 0.7071067811865486830, -0.7071067811865464625, -0.000000000000000000 ) ) ;
#98274 = UNCERTAINTY_MEASURE_WITH_UNIT (LENGTH_MEASURE( 1.000000000000000082E-05 ), #2621, 'distance_accuracy_value', 'NONE');
#98275 = VECTOR ( 'NONE', #32038, 1000.000000000000000 ) ;
#98276 = FACE_OUTER_BOUND ( 'NONE', #100263, .T. ) ;
#98277 = LINE ( 'NONE', #43188, #64231 ) ;
#98278 = CARTESIAN_POINT ( 'NONE',  ( 83.64169371712955581, -2.130196079827424871, -7.949999999999999289 ) ) ;
#98279 = CARTESIAN_POINT ( 'NONE',  ( -63.18398860626900415, 28.73617430169831621, 5.000000000000000000 ) ) ;
#98280 = VECTOR ( 'NONE', #136251, 1000.000000000000000 ) ;
#98281 = CARTESIAN_POINT ( 'NONE',  ( 34.92499999999998295, -10.29806943317891310, 4.500000000000000888 ) ) ;
#98282 = ORIENTED_EDGE ( 'NONE', *, *, #23042, .F. ) ;
#98283 = CARTESIAN_POINT ( 'NONE',  ( 86.45833333333332860, 3.974999999999997424, 6.884901960086288852 ) ) ;
#98284 = CARTESIAN_POINT ( 'NONE',  ( -20.24139925780189841, 21.72500000000000853, 5.000000000000000000 ) ) ;
#98285 = AXIS2_PLACEMENT_3D ( 'NONE', #96619, #61922, #140859 ) ;
#98286 = EDGE_CURVE ( 'NONE', #139251, #114615, #56476, .T. ) ;
#98287 = CARTESIAN_POINT ( 'NONE',  ( 156.1500000000000057, -49.14999999999999147, -49.92499999999968452 ) ) ;
#98288 = CARTESIAN_POINT ( 'NONE',  ( 32.66666666666667140, -5.278424836066145431, -3.047499999999993658 ) ) ;
#98289 = ORIENTED_EDGE ( 'NONE', *, *, #124570, .T. ) ;
#98290 =( BOUNDED_CURVE ( )  B_SPLINE_CURVE ( 3, ( #138267, #127378, #50541, #39690 ),
 .UNSPECIFIED., .F., .F. ) 
 B_SPLINE_CURVE_WITH_KNOTS ( ( 4, 4 ),
 ( 2.001653308786170982, 3.503810798801451742 ),
 .UNSPECIFIED. ) 
 CURVE ( )  GEOMETRIC_REPRESENTATION_ITEM ( )  RATIONAL_B_SPLINE_CURVE ( ( 1.000000000000000000, 0.8206354192515243895, 0.8206354192515243895, 1.000000000000000000 ) ) 
 REPRESENTATION_ITEM ( '' )  );
#98291 = DIRECTION ( 'NONE',  ( -0.7071067811865487940, 0.7071067811865463515, -0.000000000000000000 ) ) ;
#98292 = ORIENTED_EDGE ( 'NONE', *, *, #120707, .T. ) ;
#98293 = VECTOR ( 'NONE', #81128, 999.9999999999998863 ) ;
#98294 = CARTESIAN_POINT ( 'NONE',  ( 71.45876352523143282, 0.000000000000000000, -6.110000000000001208 ) ) ;
#98295 = CARTESIAN_POINT ( 'NONE',  ( 0.000000000000000000, 0.000000000000000000, 5.000000000000000000 ) ) ;
#98296 = VERTEX_POINT ( 'NONE', #89756 ) ;
#98297 = PLANE ( 'NONE',  #51249 ) ;
#98298 =( BOUNDED_CURVE ( )  B_SPLINE_CURVE ( 3, ( #77492, #118815, #54316, #130432 ),
 .UNSPECIFIED., .F., .T. ) 
 B_SPLINE_CURVE_WITH_KNOTS ( ( 4, 4 ),
 ( 1.208578181583235267, 1.359146454359470901 ),
 .UNSPECIFIED. ) 
 CURVE ( )  GEOMETRIC_REPRESENTATION_ITEM ( )  RATIONAL_B_SPLINE_CURVE ( ( 1.000000000000000000, 0.9981116584018945304, 0.9981116584018945304, 1.000000000000000000 ) ) 
 REPRESENTATION_ITEM ( '' )  );
#98299 = DIRECTION ( 'NONE',  ( -0.7071067811865486830, -0.7071067811865464625, 0.000000000000000000 ) ) ;
#98300 = DIRECTION ( 'NONE',  ( -0.7071067811865486830, 0.7071067811865464625, 0.000000000000000000 ) ) ;
#98301 = EDGE_CURVE ( 'NONE', #88210, #129741, #100656, .T. ) ;
#98302 = CARTESIAN_POINT ( 'NONE',  ( -75.48921356237309510, -27.52281430457107803, 5.000000000000000000 ) ) ;
#98304 = ORIENTED_EDGE ( 'NONE', *, *, #101514, .T. ) ;
#98303 = CARTESIAN_POINT ( 'NONE',  ( 28.82816939922332722, -8.240707523384196875, 4.000000000000000000 ) ) ;
#98305 = ADVANCED_FACE ( 'NONE', ( #12898 ), #102800, .F. ) ;
#98306 = CARTESIAN_POINT ( 'NONE',  ( 131.5423521607622774, -49.05583548141699168, -39.86617647058817226 ) ) ;
#98307 = DIRECTION ( 'NONE',  ( 0.7071067811865487940, 0.7071067811865463515, 0.000000000000000000 ) ) ;
#98308 = FACE_OUTER_BOUND ( 'NONE', #119269, .T. ) ;
#98309 = FACE_OUTER_BOUND ( 'NONE', #21867, .T. ) ;
#98311 = ADVANCED_FACE ( 'NONE', ( #70893 ), #126655, .F. ) ;
#98310 = VECTOR ( 'NONE', #139955, 1000.000000000000000 ) ;
#98312 = ORIENTED_EDGE ( 'NONE', *, *, #24189, .T. ) ;
#98313 = VERTEX_POINT ( 'NONE', #81781 ) ;
#98314 = CARTESIAN_POINT ( 'NONE',  ( 69.12543019189809002, 5.291415217122919401, 3.055000000000002824 ) ) ;
#98315 = CIRCLE ( 'NONE', #79825, 0.5000000000000004441 ) ;
#98316 = VECTOR ( 'NONE', #53664, 1000.000000000000000 ) ;
#98317 = EDGE_LOOP ( 'NONE', ( #24421, #29508, #109791, #131136 ) ) ;
#98319 = EDGE_CURVE ( 'NONE', #4377, #115184, #30021, .T. ) ;
#98318 = AXIS2_PLACEMENT_3D ( 'NONE', #123856, #47742, #136129 ) ;
#98320 = DIRECTION ( 'NONE',  ( -0.7071067811865486830, -0.7071067811865464625, 0.000000000000000000 ) ) ;
#98321 = CARTESIAN_POINT ( 'NONE',  ( -2.999999999999981792, 10.21212019023809070, -2.019456568337790969 ) ) ;
#98322 = DIRECTION ( 'NONE',  ( -1.000000000000000000, -0.000000000000000000, -0.000000000000000000 ) ) ;
#98323 = PRESENTATION_STYLE_ASSIGNMENT (( #131662 ) ) ;
#98324 = ORIENTED_EDGE ( 'NONE', *, *, #103968, .T. ) ;
#98325 = ORIENTED_EDGE ( 'NONE', *, *, #36614, .T. ) ;
#98326 = LINE ( 'NONE', #88888, #65435 ) ;
#98327 = LINE ( 'NONE', #87452, #125386 ) ;
#98328 = ADVANCED_FACE ( 'NONE', ( #119865 ), #4842, .F. ) ;
#98329 = AXIS2_PLACEMENT_3D ( 'NONE', #34519, #78747, #46886 ) ;
#98330 = VERTEX_POINT ( 'NONE', #125977 ) ;
#98331 = DIRECTION ( 'NONE',  ( -0.000000000000000000, 0.3543493200069153248, 0.9351131265310292928 ) ) ;
#98332 = LINE ( 'NONE', #102620, #85032 ) ;
#98333 = FACE_OUTER_BOUND ( 'NONE', #88370, .T. ) ;
#98334 = EDGE_CURVE ( 'NONE', #15605, #90375, #109004, .T. ) ;
#98335 = ORIENTED_EDGE ( 'NONE', *, *, #131079, .F. ) ;
#98336 = FACE_BOUND ( 'NONE', #134023, .T. ) ;
#98337 = CARTESIAN_POINT ( 'NONE',  ( -12.69999999999998153, 3.061616997868383634E-16, -2.500000000000000444 ) ) ;
#98338 = DIRECTION ( 'NONE',  ( -0.7071067811865486830, 0.7071067811865464625, 0.000000000000000000 ) ) ;
#98339 = CARTESIAN_POINT ( 'NONE',  ( 60.79166666666665719, 3.975000000000003642, -6.884901960086285300 ) ) ;
#98340 = EDGE_CURVE ( 'NONE', #82317, #73248, #113093, .T. ) ;
#98341 = CARTESIAN_POINT ( 'NONE',  ( 13.64840764549667540, -3.851859888774471706E-31, 2.500000000000001332 ) ) ;
#98342 = CARTESIAN_POINT ( 'NONE',  ( 1.031246673762481025, -0.6000000000000000888, 4.508537709115516989 ) ) ;
#98343 = SURFACE_SIDE_STYLE ('',( #11282 ) ) ;
#98344 = ORIENTED_EDGE ( 'NONE', *, *, #12104, .F. ) ;
#98345 = ORIENTED_EDGE ( 'NONE', *, *, #69492, .T. ) ;
#98346 = CARTESIAN_POINT ( 'NONE',  ( 108.9954301918981088, 5.291415217122916737, 3.055000000000001936 ) ) ;
#98347 = VERTEX_POINT ( 'NONE', #86579 ) ;
#98348 = ORIENTED_EDGE ( 'NONE', *, *, #46889, .F. ) ;
#98349 = EDGE_CURVE ( 'NONE', #26004, #34476, #92599, .T. ) ;
#98350 = CARTESIAN_POINT ( 'NONE',  ( 184.1499999999998352, -47.62213595499959951, 36.92500000000000426 ) ) ;
#98351 = CIRCLE ( 'NONE', #63604, 2.500000000000000888 ) ;
#98352 = CARTESIAN_POINT ( 'NONE',  ( 19.04500000000000881, 3.130000000000007887, -22.35000000000000142 ) ) ;
#98353 = EDGE_CURVE ( 'NONE', #133319, #34241, #107589, .T. ) ;
#98354 = ADVANCED_FACE ( 'NONE', ( #85838 ), #85126, .F. ) ;
#98355 = DIRECTION ( 'NONE',  ( -0.000000000000000000, 0.000000000000000000, 1.000000000000000000 ) ) ;
#98356 = ORIENTED_EDGE ( 'NONE', *, *, #83244, .T. ) ;
#98357 = DIRECTION ( 'NONE',  ( -1.000000000000000000, -0.000000000000000000, -0.000000000000000000 ) ) ;
#98358 = DIRECTION ( 'NONE',  ( 0.5735764363510448272, -0.8191520442889927978, 1.003171929053526103E-16 ) ) ;
#98360 = DIRECTION ( 'NONE',  ( 0.7071067811865487940, 0.7071067811865463515, -0.000000000000000000 ) ) ;
#98359 = PLANE ( 'NONE',  #71234 ) ;
#98361 = DIRECTION ( 'NONE',  ( -0.7071067811865487940, 0.7071067811865463515, -0.000000000000000000 ) ) ;
#98362 = CARTESIAN_POINT ( 'NONE',  ( 1.055009550493547277, 0.8130331625670963458, 3.860388942535410539 ) ) ;
#98363 = ORIENTED_EDGE ( 'NONE', *, *, #9348, .F. ) ;
#98364 = ADVANCED_FACE ( 'NONE', ( #37544 ), #8247, .F. ) ;
#98365 = DIRECTION ( 'NONE',  ( -0.6830127018922181881, 0.6830127018922202975, -0.2588190451025214056 ) ) ;
#98366 = CARTESIAN_POINT ( 'NONE',  ( -18.49816348513945385, -17.24070752338411339, 8.407044977365265126 ) ) ;
#98367 = ORIENTED_EDGE ( 'NONE', *, *, #102207, .T. ) ;
#98368 = ORIENTED_EDGE ( 'NONE', *, *, #134931, .T. ) ;
#98369 = EDGE_CURVE ( 'NONE', #103418, #12595, #49142, .T. ) ;
#98370 = ORIENTED_EDGE ( 'NONE', *, *, #136468, .T. ) ;
#98371 = CARTESIAN_POINT ( 'NONE',  ( 68.39626352523143282, 4.472830434245840259, -4.472830434245838482 ) ) ;
#98372 = VERTEX_POINT ( 'NONE', #93332 ) ;
#98373 = DIRECTION ( 'NONE',  ( -1.000000000000000000, 0.000000000000000000, 0.000000000000000000 ) ) ;
#98374 = VECTOR ( 'NONE', #113610, 999.9999999999998863 ) ;
#98375 = DIRECTION ( 'NONE',  ( 0.7071067811865487940, -0.7071067811865463515, 0.000000000000000000 ) ) ;
#98376 = CARTESIAN_POINT ( 'NONE',  ( 100.0420968585647756, 5.291415217122923842, -3.054999999999996163 ) ) ;
#98377 = DIRECTION ( 'NONE',  ( -0.000000000000000000, -0.3543493200069152693, 0.9351131265310292928 ) ) ;
#98378 = EDGE_CURVE ( 'NONE', #133903, #98841, #96681, .T. ) ;
#98379 = AXIS2_PLACEMENT_3D ( 'NONE', #38225, #104894, #48374 ) ;
#98380 = LINE ( 'NONE', #109239, #53525 ) ;
#98381 = EDGE_LOOP ( 'NONE', ( #95838, #105850, #16330, #48378 ) ) ;
#98382 = DIRECTION ( 'NONE',  ( 1.734723475976806848E-16, -1.000000000000000000, 0.000000000000000000 ) ) ;
#98383 = EDGE_CURVE ( 'NONE', #111457, #132148, #106752, .T. ) ;
#98384 = DIRECTION ( 'NONE',  ( 0.7071067811865487940, 0.7071067811865463515, 0.000000000000000000 ) ) ;
#98385 = CARTESIAN_POINT ( 'NONE',  ( -19.49999999999985789, -14.94781430457067906, 5.000000000000000000 ) ) ;
#98386 = DIRECTION ( 'NONE',  ( 0.7071067811865487940, 0.7071067811865463515, -0.000000000000000000 ) ) ;
#98387 = ORIENTED_EDGE ( 'NONE', *, *, #52942, .T. ) ;
#98388 = DIRECTION ( 'NONE',  ( -0.7071067811865487940, 0.7071067811865463515, -0.000000000000000000 ) ) ;
#98389 = MECHANICAL_DESIGN_GEOMETRIC_PRESENTATION_REPRESENTATION (  '', ( #5732 ), #45132 ) ;
#98390 = ORIENTED_EDGE ( 'NONE', *, *, #142541, .F. ) ;
#98391 = EDGE_LOOP ( 'NONE', ( #108138, #128372, #102822, #84687 ) ) ;
#98392 = ORIENTED_EDGE ( 'NONE', *, *, #28608, .T. ) ;
#98393 = CARTESIAN_POINT ( 'NONE',  ( 121.8287635252314516, 0.000000000000000000, -6.109999999999998543 ) ) ;
#98394 = EDGE_LOOP ( 'NONE', ( #31689, #73127, #100386, #89025 ) ) ;
#98395 = DIRECTION ( 'NONE',  ( -1.000000000000000000, -1.224606353822377258E-16, -0.000000000000000000 ) ) ;
#98396 = FACE_OUTER_BOUND ( 'NONE', #11797, .T. ) ;
#98397 = VERTEX_POINT ( 'NONE', #95994 ) ;
#98398 = CARTESIAN_POINT ( 'NONE',  ( 2.999999999999981792, -0.03360074219773551141, 5.000000000000000000 ) ) ;
#98399 = ORIENTED_EDGE ( 'NONE', *, *, #25368, .T. ) ;
#98400 = VECTOR ( 'NONE', #38035, 1000.000000000000000 ) ;
#98401 = ADVANCED_FACE ( 'NONE', ( #7549 ), #40923, .F. ) ;
#98402 = AXIS2_PLACEMENT_3D ( 'NONE', #116384, #117077, #126531 ) ;
#98403 = CARTESIAN_POINT ( 'NONE',  ( 13.54123647476855474, 0.000000000000000000, 7.934999999999990727 ) ) ;
#98404 = DIRECTION ( 'NONE',  ( 0.7071067811865487940, -0.7071067811865463515, 0.000000000000000000 ) ) ;
#98405 = COLOUR_RGB ( '', 0.09019608, 0.27058824, 0.51372549) ;
#98406 = DIRECTION ( 'NONE',  ( 0.7071067811865487940, 0.7071067811865463515, 0.000000000000000000 ) ) ;
#98407 = AXIS2_PLACEMENT_3D ( 'NONE', #109552, #10230, #134175 ) ;
#98408 = CARTESIAN_POINT ( 'NONE',  ( 10.32500000000000107, -8.432637487761466488, -4.375000000000001776 ) ) ;
#98409 = ORIENTED_EDGE ( 'NONE', *, *, #2026, .F. ) ;
#98410 = ORIENTED_EDGE ( 'NONE', *, *, #134186, .T. ) ;
#98411 = EDGE_LOOP ( 'NONE', ( #11361, #33234, #61030, #36679 ) ) ;
#98412 = DIRECTION ( 'NONE',  ( -0.6830127018922181881, 0.6830127018922202975, -0.2588190451025214056 ) ) ;
#98413 = CARTESIAN_POINT ( 'NONE',  ( -28.49999999999980460, -7.420205493532925800, -2.617629953481318772 ) ) ;
#98414 = CARTESIAN_POINT ( 'NONE',  ( -63.18398860626900415, 28.73617430169831621, 5.000000000000000000 ) ) ;
#98415 = FACE_OUTER_BOUND ( 'NONE', #14826, .T. ) ;
#98416 = CARTESIAN_POINT ( 'NONE',  ( 29.02126352523143282, -4.472830434245839371, -4.472830434245840259 ) ) ;
#98417 = CARTESIAN_POINT ( 'NONE',  ( -30.18398860626900060, 28.73617430169808173, 5.000000000000000000 ) ) ;
#98418 = LINE ( 'NONE', #143339, #2567 ) ;
#98419 = ORIENTED_EDGE ( 'NONE', *, *, #55785, .F. ) ;
#98420 = FACE_OUTER_BOUND ( 'NONE', #1215, .T. ) ;
#98421 = ORIENTED_EDGE ( 'NONE', *, *, #124552, .T. ) ;
#98422 = DIRECTION ( 'NONE',  ( -0.000000000000000000, 0.3543493200069153248, 0.9351131265310292928 ) ) ;
#98423 = VERTEX_POINT ( 'NONE', #63421 ) ;
#98425 = VERTEX_POINT ( 'NONE', #140926 ) ;
#98424 = CARTESIAN_POINT ( 'NONE',  ( -7.828169399223474656, -5.240707523384230626, 4.000000000000000000 ) ) ;
#98426 = DIRECTION ( 'NONE',  ( 0.6830127018922180770, -0.6830127018922204085, -0.2588190451025213501 ) ) ;
#98427 = ORIENTED_EDGE ( 'NONE', *, *, #4928, .F. ) ;
#98428 = CARTESIAN_POINT ( 'NONE',  ( -9.792893218813384593, 18.75929247661552779, 5.000000000000000000 ) ) ;
#98429 = ORIENTED_EDGE ( 'NONE', *, *, #102250, .T. ) ;
#98430 = DIRECTION ( 'NONE',  ( -1.000000000000000000, -0.000000000000000000, -0.000000000000000000 ) ) ;
#98431 = UNCERTAINTY_MEASURE_WITH_UNIT (LENGTH_MEASURE( 1.000000000000000082E-05 ), #119110, 'distance_accuracy_value', 'NONE');
#98432 = ORIENTED_EDGE ( 'NONE', *, *, #76437, .T. ) ;
#98433 = CARTESIAN_POINT ( 'NONE',  ( 34.92499999999998295, -18.18334561358936341, 4.500000000000000888 ) ) ;
#98434 = CARTESIAN_POINT ( 'NONE',  ( 113.3916937171295700, 2.130196079827421762, 7.950000000000001066 ) ) ;
#98435 = FACE_OUTER_BOUND ( 'NONE', #107566, .T. ) ;
#98436 = FILL_AREA_STYLE_COLOUR ( '', #13824 ) ;
#98437 = CYLINDRICAL_SURFACE ( 'NONE', #46938, 28.00000000000003197 ) ;
#98438 = CARTESIAN_POINT ( 'NONE',  ( -32.99999999999977263, 7.588810512006185505, -3.013526669885150611 ) ) ;
#98439 = DIRECTION ( 'NONE',  ( 0.7071067811865486830, -0.7071067811865464625, -0.000000000000000000 ) ) ;
#98440 = CARTESIAN_POINT ( 'NONE',  ( 6.708333333333333925, 3.047499999999997655, 5.278424836066143655 ) ) ;
#98441 = CARTESIAN_POINT ( 'NONE',  ( 13.39540314143521904, 2.126176841940962348, 7.934999999999988951 ) ) ;
#98442 = PRESENTATION_STYLE_ASSIGNMENT (( #9998 ) ) ;
#98443 = DIRECTION ( 'NONE',  ( -0.7071067811865486830, -0.7071067811865464625, 0.000000000000000000 ) ) ;
#98444 = ORIENTED_EDGE ( 'NONE', *, *, #104833, .F. ) ;
#98445 = ORIENTED_EDGE ( 'NONE', *, *, #3106, .F. ) ;
#98446 = DIRECTION ( 'NONE',  ( -0.3543493200069162685, -0.000000000000000000, -0.9351131265310288487 ) ) ;
#98447 = ORIENTED_EDGE ( 'NONE', *, *, #58949, .F. ) ;
#98448 = CARTESIAN_POINT ( 'NONE',  ( 23.99999999999984013, -0.4125381241607464222, 4.000000000000000000 ) ) ;
#98449 = CARTESIAN_POINT ( 'NONE',  ( 128.4365526510861173, -51.77943056867387384, -39.18578444878555445 ) ) ;
#98450 = EDGE_LOOP ( 'NONE', ( #82172, #126849, #50345, #107741 ) ) ;
#98451 = DIRECTION ( 'NONE',  ( -0.7071067811865487940, 0.7071067811865463515, -0.000000000000000000 ) ) ;
#98452 = CARTESIAN_POINT ( 'NONE',  ( -23.16347128873436745, 15.75929247661555976, 9.299976744542865603 ) ) ;
#98453 = EDGE_CURVE ( 'NONE', #133772, #3598, #130076, .T. ) ;
#98454 = CARTESIAN_POINT ( 'NONE',  ( 3.872664058232597739, 2.500000000000001776, 3.061616997868385113E-16 ) ) ;
#98455 = ADVANCED_FACE ( 'NONE', ( #53204 ), #31475, .F. ) ;
#98456 = EDGE_CURVE ( 'NONE', #50067, #142844, #11100, .T. ) ;
#98457 = FACE_OUTER_BOUND ( 'NONE', #66569, .T. ) ;
#98459 = ORIENTED_EDGE ( 'NONE', *, *, #81574, .F. ) ;
#98458 = FACE_OUTER_BOUND ( 'NONE', #28625, .T. ) ;
#98460 = CARTESIAN_POINT ( 'NONE',  ( 0.000000000000000000, 0.000000000000000000, 5.000000000000000000 ) ) ;
#98461 = SURFACE_SIDE_STYLE ('',( #107877 ) ) ;
#98462 = DIRECTION ( 'NONE',  ( -0.000000000000000000, 0.3543493200069153248, 0.9351131265310292928 ) ) ;
#98463 = DIRECTION ( 'NONE',  ( -0.7071067811865486830, 0.7071067811865464625, 0.000000000000000000 ) ) ;
#98464 = PLANE ( 'NONE',  #51536 ) ;
#98465 = EDGE_CURVE ( 'NONE', #118892, #13978, #129131, .T. ) ;
#98467 = EDGE_CURVE ( 'NONE', #86945, #115943, #142387, .T. ) ;
#98466 = ORIENTED_EDGE ( 'NONE', *, *, #5241, .F. ) ;
#98468 = AXIS2_PLACEMENT_3D ( 'NONE', #11245, #86720, #120746 ) ;
#98469 = ORIENTED_EDGE ( 'NONE', *, *, #72183, .T. ) ;
#98470 = ORIENTED_EDGE ( 'NONE', *, *, #80634, .T. ) ;
#98471 = CARTESIAN_POINT ( 'NONE',  ( 93.04209685856476142, 5.291415217122923842, -3.054999999999996163 ) ) ;
#98472 = VERTEX_POINT ( 'NONE', #23434 ) ;
#98473 = VECTOR ( 'NONE', #127926, 999.9999999999998863 ) ;
#98474 = EDGE_CURVE ( 'NONE', #101323, #46695, #43774, .T. ) ;
#98475 = CARTESIAN_POINT ( 'NONE',  ( 126.7224180521722730, -45.84254607569121731, 35.55177538329068909 ) ) ;
#98476 = FACE_OUTER_BOUND ( 'NONE', #61943, .T. ) ;
#98477 = VERTEX_POINT ( 'NONE', #53963 ) ;
#98478 = LINE ( 'NONE', #120190, #60697 ) ;
#98479 = DIRECTION ( 'NONE',  ( -0.5735764363510503783, -0.8191520442889886899, 0.000000000000000000 ) ) ;
#98480 = ADVANCED_FACE ( 'NONE', ( #224 ), #56836, .F. ) ;
#98481 = CARTESIAN_POINT ( 'NONE',  ( 89.74543019189812298, -5.291415217122918513, -3.055000000000000160 ) ) ;
#98482 = VECTOR ( 'NONE', #120310, 1000.000000000000227 ) ;
#98483 = ORIENTED_EDGE ( 'NONE', *, *, #116830, .T. ) ;
#98484 = CARTESIAN_POINT ( 'NONE',  ( -7.828169399223476432, 15.75929247661555976, 4.000000000000000000 ) ) ;
#98485 = CARTESIAN_POINT ( 'NONE',  ( 36.29974487139159578, -27.71228299555231445, 4.000000000000000000 ) ) ;
#98486 = ORIENTED_EDGE ( 'NONE', *, *, #68771, .T. ) ;
#98487 = VERTEX_POINT ( 'NONE', #66252 ) ;
#98488 = VERTEX_POINT ( 'NONE', #132956 ) ;
#98489 = CARTESIAN_POINT ( 'NONE',  ( -17.99999999999987210, -21.41253812416053748, 4.000000000000000000 ) ) ;
#98490 = CARTESIAN_POINT ( 'NONE',  ( -5.510786437626906675, -27.52281430457051314, 5.000000000000000000 ) ) ;
#98491 = DIRECTION ( 'NONE',  ( -0.7071067811865487940, 0.7071067811865463515, -0.000000000000000000 ) ) ;
#98492 = ADVANCED_FACE ( 'NONE', ( #87281 ), #123508, .F. ) ;
#98493 = CARTESIAN_POINT ( 'NONE',  ( 42.18398860626899705, 28.73617430169816700, 5.000000000000000000 ) ) ;
#98494 = AXIS2_PLACEMENT_3D ( 'NONE', #41954, #130395, #73861 ) ;
#98495 = CARTESIAN_POINT ( 'NONE',  ( -12.29974487139158512, -27.71228299555214747, 4.000000000000000000 ) ) ;
#98496 =( NAMED_UNIT ( * ) SI_UNIT ( $, .STERADIAN. ) SOLID_ANGLE_UNIT ( ) );
#98497 = VECTOR ( 'NONE', #36942, 1000.000000000000000 ) ;
#98498 = VERTEX_POINT ( 'NONE', #55376 ) ;
#98500 = ORIENTED_EDGE ( 'NONE', *, *, #47505, .F. ) ;
#98499 = VECTOR ( 'NONE', #139565, 1000.000000000000000 ) ;
#98501 = CARTESIAN_POINT ( 'NONE',  ( -34.92499999999997584, -6.270000000000012896, -36.39086428169088094 ) ) ;
#98502 = ORIENTED_EDGE ( 'NONE', *, *, #103550, .T. ) ;
#98503 = ORIENTED_EDGE ( 'NONE', *, *, #20749, .F. ) ;
#98504 = EDGE_CURVE ( 'NONE', #41140, #15309, #32930, .T. ) ;
#98505 = AXIS2_PLACEMENT_3D ( 'NONE', #41733, #7653, #121420 ) ;
#98506 = ADVANCED_FACE ( 'NONE', ( #33636 ), #32183, .F. ) ;
#98507 = CARTESIAN_POINT ( 'NONE',  ( -1.500000000000001332, 22.08746187583903975, 4.000000000000000000 ) ) ;
#98508 = ORIENTED_EDGE ( 'NONE', *, *, #114734, .F. ) ;
#98509 = LINE ( 'NONE', #119513, #57628 ) ;
#98510 = CARTESIAN_POINT ( 'NONE',  ( -30.48921356237309510, -27.52281430457076894, 5.000000000000000000 ) ) ;
#98511 = EDGE_CURVE ( 'NONE', #106471, #126064, #111137, .T. ) ;
#98512 = DIRECTION ( 'NONE',  ( 0.7071067811865487940, 0.7071067811865463515, 0.000000000000000000 ) ) ;
#98513 = DIRECTION ( 'NONE',  ( -0.7071067811865486830, -0.7071067811865464625, -0.000000000000000000 ) ) ;
#98514 =( NAMED_UNIT ( * ) SI_UNIT ( $, .STERADIAN. ) SOLID_ANGLE_UNIT ( ) );
#98515 = ORIENTED_EDGE ( 'NONE', *, *, #29587, .T. ) ;
#98516 = EDGE_CURVE ( 'NONE', #93730, #5674, #76418, .T. ) ;
#98517 = DIRECTION ( 'NONE',  ( -0.3543493200069163240, 0.000000000000000000, -0.9351131265310288487 ) ) ;
#98518 = ORIENTED_EDGE ( 'NONE', *, *, #53407, .F. ) ;
#98519 = LINE ( 'NONE', #8602, #136051 ) ;
#98520 = ORIENTED_EDGE ( 'NONE', *, *, #138106, .F. ) ;
#98521 = DIRECTION ( 'NONE',  ( 0.6830127018922180770, -0.6830127018922204085, -0.2588190451025213501 ) ) ;
#98522 = ORIENTED_EDGE ( 'NONE', *, *, #123365, .F. ) ;
#98523 = DIRECTION ( 'NONE',  ( 0.7071067811865486830, 0.7071067811865463515, 0.000000000000000000 ) ) ;
#98524 = ORIENTED_EDGE ( 'NONE', *, *, #119693, .T. ) ;
#98525 = VERTEX_POINT ( 'NONE', #133645 ) ;
#98526 = ORIENTED_EDGE ( 'NONE', *, *, #34673, .F. ) ;
#98527 = FACE_OUTER_BOUND ( 'NONE', #30903, .T. ) ;
#98528 = DIRECTION ( 'NONE',  ( 0.6830127018922181881, 0.6830127018922202975, -0.2588190451025214056 ) ) ;
#98529 = DIRECTION ( 'NONE',  ( 0.000000000000000000, 0.000000000000000000, -1.000000000000000000 ) ) ;
#98530 = DIRECTION ( 'NONE',  ( 0.6830127018922181881, 0.6830127018922202975, -0.2588190451025214056 ) ) ;
#98531 = CARTESIAN_POINT ( 'NONE',  ( 123.9587635252314470, 0.000000000000000000, -6.110000000000001208 ) ) ;
#98532 = CARTESIAN_POINT ( 'NONE',  ( -42.48921356237308800, -27.52281430457085065, 5.000000000000000000 ) ) ;
#98533 = EDGE_CURVE ( 'NONE', #6240, #6993, #120586, .T. ) ;
#98534 = LINE ( 'NONE', #76821, #31993 ) ;
#98535 = DIRECTION ( 'NONE',  ( 0.7071067811865487940, -0.7071067811865463515, 0.000000000000000000 ) ) ;
#98536 = CARTESIAN_POINT ( 'NONE',  ( 39.47336096364190183, -5.240707523384228850, 16.25846745537504745 ) ) ;
#98537 = FACE_OUTER_BOUND ( 'NONE', #64750, .T. ) ;
#98539 = EDGE_CURVE ( 'NONE', #65842, #141841, #122020, .T. ) ;
#98538 = DIRECTION ( 'NONE',  ( 0.7071067811865487940, 0.7071067811865463515, 0.000000000000000000 ) ) ;
#98540 = CARTESIAN_POINT ( 'NONE',  ( -5.483345613589513334, 22.22500000000000142, 4.500000000000000888 ) ) ;
#98541 = ORIENTED_EDGE ( 'NONE', *, *, #57503, .F. ) ;
#98542 = ORIENTED_EDGE ( 'NONE', *, *, #129713, .T. ) ;
#98543 = VERTEX_POINT ( 'NONE', #67707 ) ;
#98544 = CARTESIAN_POINT ( 'NONE',  ( -14.29289321881335617, -6.740707523384207533, 5.000000000000000000 ) ) ;
#98545 = ORIENTED_EDGE ( 'NONE', *, *, #71108, .F. ) ;
#98546 = VERTEX_POINT ( 'NONE', #34322 ) ;
#98547 = DIRECTION ( 'NONE',  ( -0.6830127018922180770, -0.6830127018922204085, -0.2588190451025213501 ) ) ;
#98548 = DIRECTION ( 'NONE',  ( 0.7071067811865487940, 0.7071067811865463515, 0.000000000000000000 ) ) ;
#98549 = EDGE_CURVE ( 'NONE', #42067, #106511, #121320, .T. ) ;
#98550 = CARTESIAN_POINT ( 'NONE',  ( 54.29974487139159578, -27.71228299555243879, 4.000000000000000000 ) ) ;
#98551 = ORIENTED_EDGE ( 'NONE', *, *, #124615, .T. ) ;
#98552 = CARTESIAN_POINT ( 'NONE',  ( 16.61159235450331906, 2.500000000000001332, 0.000000000000000000 ) ) ;
#98553 = ORIENTED_EDGE ( 'NONE', *, *, #52142, .F. ) ;
#98554 = CARTESIAN_POINT ( 'NONE',  ( -19.49999999999986500, 10.94296225409025247, -9.576120664313302555 ) ) ;
#98555 = VECTOR ( 'NONE', #96305, 1000.000000000000000 ) ;
#98556 = EDGE_CURVE ( 'NONE', #74147, #97217, #30553, .T. ) ;
#98557 = FACE_OUTER_BOUND ( 'NONE', #79907, .T. ) ;
#98558 = CARTESIAN_POINT ( 'NONE',  ( 15.37956980810188767, 3.967499999999998916, 6.871911579029510442 ) ) ;
#98559 = ORIENTED_EDGE ( 'NONE', *, *, #21067, .F. ) ;
#98560 = CARTESIAN_POINT ( 'NONE',  ( 92.22459685856479439, -1.637169565754161171, 6.109999999999998543 ) ) ;
#98561 = DIRECTION ( 'NONE',  ( -0.6830127018922180770, -0.6830127018922204085, -0.2588190451025213501 ) ) ;
#98562 = STYLED_ITEM ( 'NONE', ( #139536 ), #91052 ) ;
#98563 = CARTESIAN_POINT ( 'NONE',  ( 13.49999999999991118, -14.94781430457067906, 5.000000000000000000 ) ) ;
#98564 = CARTESIAN_POINT ( 'NONE',  ( -5.999999999999956479, -10.44781430457071991, 5.000000000000000000 ) ) ;
#98565 = VERTEX_POINT ( 'NONE', #78550 ) ;
#98566 = VERTEX_POINT ( 'NONE', #143081 ) ;
#98567 = ORIENTED_EDGE ( 'NONE', *, *, #60483, .T. ) ;
#98568 = DIRECTION ( 'NONE',  ( 0.000000000000000000, -1.000000000000000000, 0.000000000000000000 ) ) ;
#98569 = CARTESIAN_POINT ( 'NONE',  ( 34.49999999999975842, -1.535744391599495273, 4.994342998332161443 ) ) ;
#98570 = CARTESIAN_POINT ( 'NONE',  ( 6.005480084712508493, 28.92564299267933947, 4.000000000000000000 ) ) ;
#98571 = DIRECTION ( 'NONE',  ( 1.000000000000000000, 0.000000000000000000, 0.000000000000000000 ) ) ;
#98573 = EDGE_CURVE ( 'NONE', #130643, #15318, #87988, .T. ) ;
#98572 = ORIENTED_EDGE ( 'NONE', *, *, #125645, .F. ) ;
#98574 = CARTESIAN_POINT ( 'NONE',  ( -12.70679250724066733, 20.25929247661551358, 20.83292124670817813 ) ) ;
#98575 = EDGE_CURVE ( 'NONE', #115620, #112794, #127020, .T. ) ;
#98576 =( LENGTH_UNIT ( ) NAMED_UNIT ( * ) SI_UNIT ( .MILLI., .METRE. ) );
#98577 = CARTESIAN_POINT ( 'NONE',  ( -18.48921356237309510, -27.52281430457068367, 5.000000000000000000 ) ) ;
#98578 = ORIENTED_EDGE ( 'NONE', *, *, #50710, .T. ) ;
#98579 = LINE ( 'NONE', #12282, #5039 ) ;
#98580 = CARTESIAN_POINT ( 'NONE',  ( 153.4000000000000057, -16.48000000000005016, 34.92499999999998295 ) ) ;
#98581 = ORIENTED_EDGE ( 'NONE', *, *, #32440, .T. ) ;
#98583 = EDGE_LOOP ( 'NONE', ( #116211, #12517, #77716, #115780, #112969 ) ) ;
#98582 = DIRECTION ( 'NONE',  ( -0.7071067811865487940, 0.7071067811865463515, -0.000000000000000000 ) ) ;
#98584 = ORIENTED_EDGE ( 'NONE', *, *, #123443, .T. ) ;
#98585 = EDGE_CURVE ( 'NONE', #109345, #119897, #46602, .T. ) ;
#98586 = CARTESIAN_POINT ( 'NONE',  ( 27.18398860626900060, 28.73617430169806042, 5.000000000000000000 ) ) ;
#98587 = CARTESIAN_POINT ( 'NONE',  ( -59.99451991528749772, 28.92564299267980132, 4.000000000000000000 ) ) ;
#98588 = VERTEX_POINT ( 'NONE', #114710 ) ;
#98589 = LINE ( 'NONE', #96419, #136850 ) ;
#98590 = VECTOR ( 'NONE', #68548, 1000.000000000000000 ) ;
#98591 = LINE ( 'NONE', #75434, #93823 ) ;
#98592 = MECHANICAL_DESIGN_GEOMETRIC_PRESENTATION_REPRESENTATION (  '', ( #84740 ), #119374 ) ;
#98593 = SURFACE_SIDE_STYLE ('',( #99287 ) ) ;
#98594 = AXIS2_PLACEMENT_3D ( 'NONE', #37798, #93590, #18118 ) ;
#98595 = FACE_OUTER_BOUND ( 'NONE', #15583, .T. ) ;
#98597 = VECTOR ( 'NONE', #76185, 1000.000000000000000 ) ;
#98596 = CARTESIAN_POINT ( 'NONE',  ( 34.75611968250419181, 16.70565069852387552, 4.955485411084881164 ) ) ;
#98598 = CARTESIAN_POINT ( 'NONE',  ( 27.48921356237309155, -27.52281430457074762, 5.000000000000000000 ) ) ;
#98599 = DIRECTION ( 'NONE',  ( 0.6830127018922181881, 0.6830127018922202975, -0.2588190451025214056 ) ) ;
#98600 = FACE_OUTER_BOUND ( 'NONE', #123999, .T. ) ;
#98601 = PLANE ( 'NONE',  #131408 ) ;
#98602 = LINE ( 'NONE', #87737, #51471 ) ;
#98603 = LINE ( 'NONE', #21033, #71511 ) ;
#98604 = CONICAL_SURFACE ( 'NONE', #63956, 2.500000000000000888, 0.9599310885968822538 ) ;
#98605 = CARTESIAN_POINT ( 'NONE',  ( 110.9583333333333286, 3.974999999999997424, 6.884901960086288852 ) ) ;
#98606 = DIRECTION ( 'NONE',  ( 0.6830127018922180770, -0.6830127018922204085, -0.2588190451025213501 ) ) ;
#98607 = ORIENTED_EDGE ( 'NONE', *, *, #122526, .F. ) ;
#98608 = VERTEX_POINT ( 'NONE', #137928 ) ;
#98609 = CARTESIAN_POINT ( 'NONE',  ( 97.25000000000000000, -9.735942053221458872E-16, 7.950000000000000178 ) ) ;
#98610 = VERTEX_POINT ( 'NONE', #46686 ) ;
#98611 = ORIENTED_EDGE ( 'NONE', *, *, #118760, .T. ) ;
#98612 = ORIENTED_EDGE ( 'NONE', *, *, #137943, .F. ) ;
#98613 = LINE ( 'NONE', #142846, #80464 ) ;
#98614 = PLANE ( 'NONE',  #9130 ) ;
#98615 = VERTEX_POINT ( 'NONE', #27717 ) ;
#98616 = DIRECTION ( 'NONE',  ( 0.5735764363510451602, 0.8191520442889924647, 0.000000000000000000 ) ) ;
#98617 = CARTESIAN_POINT ( 'NONE',  ( 19.93618820137057668, -3.269999999999996021, -37.00000000000000000 ) ) ;
#98618 = CARTESIAN_POINT ( 'NONE',  ( 24.18398860626899705, 28.73617430169804265, 5.000000000000000000 ) ) ;
#98619 = LINE ( 'NONE', #142852, #97492 ) ;
#98620 = ORIENTED_EDGE ( 'NONE', *, *, #553, .F. ) ;
#98621 = EDGE_CURVE ( 'NONE', #60255, #3936, #136477, .T. ) ;
#98622 = CARTESIAN_POINT ( 'NONE',  ( 25.02392480454907187, -6.350000000000004974, -3.888253587292851012E-16 ) ) ;
#98623 = DIRECTION ( 'NONE',  ( 1.000000000000000000, 0.000000000000000000, 0.000000000000000000 ) ) ;
#98624 = CARTESIAN_POINT ( 'NONE',  ( -60.48921356237309510, -27.52281430457097500, 5.000000000000000000 ) ) ;
#98625 = DIRECTION ( 'NONE',  ( -0.7071067811865487940, 0.7071067811865463515, 0.000000000000000000 ) ) ;
#98626 = CARTESIAN_POINT ( 'NONE',  ( 23.04166666666666785, 3.047499999999993214, -5.278424836066146320 ) ) ;
#98627 = PLANE ( 'NONE',  #131112 ) ;
#98628 = CARTESIAN_POINT ( 'NONE',  ( 27.05836038379621655, -7.949999999999997513, -2.130196079827425759 ) ) ;
#98629 = ADVANCED_FACE ( 'NONE', ( #114020 ), #80008, .T. ) ;
#98630 = PLANE ( 'NONE',  #16742 ) ;
#98631 = EDGE_CURVE ( 'NONE', #137395, #65995, #60385, .T. ) ;
#98632 = EDGE_CURVE ( 'NONE', #119795, #35122, #13255, .T. ) ;
#98633 = EDGE_LOOP ( 'NONE', ( #73722, #33515, #96859, #108217 ) ) ;
#98634 = ORIENTED_EDGE ( 'NONE', *, *, #62571, .T. ) ;
#98635 = CARTESIAN_POINT ( 'NONE',  ( 116.5212635252314328, -4.472830434245839371, -4.472830434245840259 ) ) ;
#98636 = EDGE_CURVE ( 'NONE', #75086, #133116, #71251, .T. ) ;
#98637 = VERTEX_POINT ( 'NONE', #92247 ) ;
#98638 = CARTESIAN_POINT ( 'NONE',  ( 30.29974487139158867, -27.71228299555227537, 4.000000000000000000 ) ) ;
#98639 = EDGE_CURVE ( 'NONE', #4786, #97989, #74404, .T. ) ;
#98640 = CARTESIAN_POINT ( 'NONE',  ( 0.000000000000000000, 21.72500000000000142, 4.500000000000000888 ) ) ;
#98641 = MECHANICAL_DESIGN_GEOMETRIC_PRESENTATION_REPRESENTATION (  '', ( #96323 ), #24649 ) ;
#98642 = EDGE_CURVE ( 'NONE', #125846, #92174, #5233, .T. ) ;
#98643 = LINE ( 'NONE', #45035, #24816 ) ;
#98644 = DIRECTION ( 'NONE',  ( 0.3543493200069162685, -0.000000000000000000, -0.9351131265310288487 ) ) ;
#98645 = CARTESIAN_POINT ( 'NONE',  ( 2.994519915287485734, 28.92564299267940342, 4.000000000000000000 ) ) ;
#98646 = DIRECTION ( 'NONE',  ( -0.7071067811865486830, -0.7071067811865464625, 0.000000000000000000 ) ) ;
#98647 = ADVANCED_FACE ( 'NONE', ( #24866 ), #69108, .F. ) ;
#98648 = CARTESIAN_POINT ( 'NONE',  ( 114.5370968585647802, -3.054999999999998828, -5.291415217122919401 ) ) ;
#98649 = ORIENTED_EDGE ( 'NONE', *, *, #111280, .F. ) ;
#98650 = ORIENTED_EDGE ( 'NONE', *, *, #82332, .T. ) ;
#98651 = CARTESIAN_POINT ( 'NONE',  ( 71.39169371712955581, 2.130196079827421762, 7.950000000000000178 ) ) ;
#98652 = CARTESIAN_POINT ( 'NONE',  ( -33.32816939922329880, -18.74070752338409207, 4.000000000000000000 ) ) ;
#98653 = EDGE_CURVE ( 'NONE', #133448, #15838, #48322, .T. ) ;
#98654 = ORIENTED_EDGE ( 'NONE', *, *, #116627, .F. ) ;
#98655 = CARTESIAN_POINT ( 'NONE',  ( 34.85459685856477563, -1.637169565754161615, 6.110000000000000320 ) ) ;
#98656 = VERTEX_POINT ( 'NONE', #26308 ) ;
#98657 = CYLINDRICAL_SURFACE ( 'NONE', #86471, 3.378199999999994319 ) ;
#98658 = DIRECTION ( 'NONE',  ( 0.7071067811865486830, -0.7071067811865464625, -0.000000000000000000 ) ) ;
#98659 = FILL_AREA_STYLE ('',( #97965 ) ) ;
#98660 = EDGE_CURVE ( 'NONE', #109630, #89139, #29150, .T. ) ;
#98661 = CIRCLE ( 'NONE', #6105, 4.749999999999997335 ) ;
#98662 = CARTESIAN_POINT ( 'NONE',  ( 40.01626352523144448, -4.472830434245839371, 4.472830434245839371 ) ) ;
#98663 = ORIENTED_EDGE ( 'NONE', *, *, #137186, .T. ) ;
#98664 = AXIS2_PLACEMENT_3D ( 'NONE', #86201, #109367, #32534 ) ;
#98665 = DIRECTION ( 'NONE',  ( -0.000000000000000000, -0.3543493200069152693, 0.9351131265310292928 ) ) ;
#98666 = VERTEX_POINT ( 'NONE', #8766 ) ;
#98667 = EDGE_LOOP ( 'NONE', ( #1105, #72531, #135709, #84077 ) ) ;
#98668 = EDGE_LOOP ( 'NONE', ( #66214, #83052, #86341, #123086 ) ) ;
#98669 = LINE ( 'NONE', #110242, #111644 ) ;
#98670 = EDGE_LOOP ( 'NONE', ( #132646, #92546, #21607 ) ) ;
#98671 = DIRECTION ( 'NONE',  ( 0.000000000000000000, -1.000000000000000000, 0.000000000000000000 ) ) ;
#98672 = VECTOR ( 'NONE', #50019, 1000.000000000000000 ) ;
#98673 = EDGE_CURVE ( 'NONE', #100764, #50175, #60450, .T. ) ;
#98674 = DIRECTION ( 'NONE',  ( -0.7071067811865486830, 0.7071067811865464625, 0.000000000000000000 ) ) ;
#98675 = EDGE_CURVE ( 'NONE', #4732, #17436, #6631, .T. ) ;
#98676 = DIRECTION ( 'NONE',  ( -0.5735764363510503783, -0.8191520442889886899, 0.000000000000000000 ) ) ;
#98678 = FACE_BOUND ( 'NONE', #917, .T. ) ;
#98677 = VECTOR ( 'NONE', #115026, 999.9999999999998863 ) ;
#98679 = VERTEX_POINT ( 'NONE', #5931 ) ;
#98680 = DIRECTION ( 'NONE',  ( 0.000000000000000000, 0.000000000000000000, 1.000000000000000000 ) ) ;
#98681 = FACE_OUTER_BOUND ( 'NONE', #64715, .T. ) ;
#98682 = EDGE_LOOP ( 'NONE', ( #41675, #13941, #103685, #93323 ) ) ;
#98683 = FACE_OUTER_BOUND ( 'NONE', #35136, .T. ) ;
#98684 = ORIENTED_EDGE ( 'NONE', *, *, #59300, .F. ) ;
#98685 = VERTEX_POINT ( 'NONE', #116871 ) ;
#98686 = CARTESIAN_POINT ( 'NONE',  ( 31.21321903303340406, 12.75929247661558996, 10.29404684609042420 ) ) ;
#98687 = ADVANCED_FACE ( 'NONE', ( #52323 ), #95108, .F. ) ;
#98688 = VECTOR ( 'NONE', #78523, 1000.000000000000000 ) ;
#98689 = VERTEX_POINT ( 'NONE', #63253 ) ;
#98690 = AXIS2_PLACEMENT_3D ( 'NONE', #91552, #136461, #93691 ) ;
#98691 = AXIS2_PLACEMENT_3D ( 'NONE', #56639, #67495, #111686 ) ;
#98692 = CARTESIAN_POINT ( 'NONE',  ( 44.09959685856477307, -6.109999999999997655, -1.637169565754160283 ) ) ;
#98693 = ORIENTED_EDGE ( 'NONE', *, *, #128465, .F. ) ;
#98694 = DIRECTION ( 'NONE',  ( -0.7071067811865486830, -0.7071067811865464625, 0.000000000000000000 ) ) ;
#98695 = ADVANCED_FACE ( 'NONE', ( #17544 ), #61806, .F. ) ;
#98696 = CARTESIAN_POINT ( 'NONE',  ( -34.92500000000001137, 21.72500000000000142, 5.000000000000000000 ) ) ;
#98697 = VERTEX_POINT ( 'NONE', #40065 ) ;
#98698 = CARTESIAN_POINT ( 'NONE',  ( 14.99451991528749595, 28.92564299267948513, 4.000000000000000000 ) ) ;
#98699 = LINE ( 'NONE', #119716, #75964 ) ;
#98700 = CIRCLE ( 'NONE', #40876, 2.500000000000000444 ) ;
#98701 = LINE ( 'NONE', #29173, #52505 ) ;
#98702 = CARTESIAN_POINT ( 'NONE',  ( 8.816011393731004731, 28.73617430169781173, 5.000000000000000000 ) ) ;
#98703 = CARTESIAN_POINT ( 'NONE',  ( 7.139999999999985469, -39.92999999999999972, -39.50000000000000000 ) ) ;
#98704 = LINE ( 'NONE', #108846, #44793 ) ;
#98705 = DIRECTION ( 'NONE',  ( -0.000000000000000000, -0.3543493200069152693, 0.9351131265310292928 ) ) ;
#98706 = ORIENTED_EDGE ( 'NONE', *, *, #133372, .T. ) ;
#98707 = ORIENTED_EDGE ( 'NONE', *, *, #82275, .T. ) ;
#98708 = ORIENTED_EDGE ( 'NONE', *, *, #94489, .T. ) ;
#98709 = CARTESIAN_POINT ( 'NONE',  ( 22.49999999999984723, -5.568876922607755908, 4.000000000000000000 ) ) ;
#98710 = LINE ( 'NONE', #32041, #74572 ) ;
#98711 = ORIENTED_EDGE ( 'NONE', *, *, #129904, .F. ) ;
#98712 = EDGE_LOOP ( 'NONE', ( #34430, #127814, #68407, #9784 ) ) ;
#98713 = PLANE ( 'NONE',  #103470 ) ;
#98714 = ADVANCED_FACE ( 'NONE', ( #105966 ), #88257, .F. ) ;
#98715 = CARTESIAN_POINT ( 'NONE',  ( -24.70710678118637560, -12.74070752338414536, 5.000000000000000000 ) ) ;
#98716 = EDGE_LOOP ( 'NONE', ( #122971, #138086, #128630, #62465, #124681 ) ) ;
#98717 = DIRECTION ( 'NONE',  ( -0.7071067811865486830, 0.7071067811865464625, 0.000000000000000000 ) ) ;
#98718 = LINE ( 'NONE', #87148, #109208 ) ;
#98719 = EDGE_CURVE ( 'NONE', #99826, #54868, #29670, .T. ) ;
#98720 = CARTESIAN_POINT ( 'NONE',  ( 15.96290314143521805, -3.967499999999994476, 6.871911579029513106 ) ) ;
#98721 = VECTOR ( 'NONE', #137624, 1000.000000000000000 ) ;
#98722 = CARTESIAN_POINT ( 'NONE',  ( 34.42499999999998295, -12.02281430457047939, 5.000000000000000000 ) ) ;
#98723 = ORIENTED_EDGE ( 'NONE', *, *, #82785, .T. ) ;
#98724 = CARTESIAN_POINT ( 'NONE',  ( 117.0162635252314374, -4.472830434245839371, 4.472830434245839371 ) ) ;
#98725 = CARTESIAN_POINT ( 'NONE',  ( -33.79289321881321939, -2.240707523384264377, 5.000000000000000000 ) ) ;
#98726 = CARTESIAN_POINT ( 'NONE',  ( -7.140000000000001457, -39.92999999999999261, -40.00000000000000000 ) ) ;
#98728 = EDGE_LOOP ( 'NONE', ( #36168, #5910, #51644, #62739 ) ) ;
#98727 = DIRECTION ( 'NONE',  ( 1.000000000000000000, 0.000000000000000000, 0.000000000000000000 ) ) ;
#98729 = VECTOR ( 'NONE', #140037, 1000.000000000000000 ) ;
#98730 = DIRECTION ( 'NONE',  ( 1.000000000000000000, 0.000000000000000000, 0.000000000000000000 ) ) ;
#98731 = VERTEX_POINT ( 'NONE', #16857 ) ;
#98732 =( NAMED_UNIT ( * ) PLANE_ANGLE_UNIT ( ) SI_UNIT ( $, .RADIAN. ) );
#98733 = PLANE ( 'NONE',  #28517 ) ;
#98734 = LINE ( 'NONE', #32808, #58811 ) ;
#98736 = ADVANCED_FACE ( 'NONE', ( #97222 ), #51636, .T. ) ;
#98735 = ORIENTED_EDGE ( 'NONE', *, *, #135841, .T. ) ;
#98737 = EDGE_CURVE ( 'NONE', #74867, #121255, #18989, .T. ) ;
#98738 = DIRECTION ( 'NONE',  ( 0.7071067811865487940, 0.7071067811865463515, 0.000000000000000000 ) ) ;
#98739 = CARTESIAN_POINT ( 'NONE',  ( -19.72734424435373768, -1.609519425888390476, -32.19467225173904268 ) ) ;
#98740 = CONICAL_SURFACE ( 'NONE', #43208, 2.500000000000000444, 0.9599310885968830309 ) ;
#98741 = ORIENTED_EDGE ( 'NONE', *, *, #76454, .F. ) ;
#98742 = LINE ( 'NONE', #132847, #104039 ) ;
#98743 = LINE ( 'NONE', #108888, #81722 ) ;
#98744 = VERTEX_POINT ( 'NONE', #140749 ) ;
#98746 = ORIENTED_EDGE ( 'NONE', *, *, #42775, .F. ) ;
#98745 = CARTESIAN_POINT ( 'NONE',  ( -7.499999999999951150, 10.08746187583914633, 4.000000000000000000 ) ) ;
#98747 = ADVANCED_FACE ( 'NONE', ( #50207 ), #108103, .F. ) ;
#98748 = ORIENTED_EDGE ( 'NONE', *, *, #112981, .F. ) ;
#98749 = PLANE ( 'NONE',  #128309 ) ;
#98750 = DIRECTION ( 'NONE',  ( 0.000000000000000000, 0.000000000000000000, 1.000000000000000000 ) ) ;
#98751 = ORIENTED_EDGE ( 'NONE', *, *, #98539, .T. ) ;
#98752 = AXIS2_PLACEMENT_3D ( 'NONE', #87837, #73410, #8790 ) ;
#98753 = PRESENTATION_STYLE_ASSIGNMENT (( #42985 ) ) ;
#98754 = LINE ( 'NONE', #19775, #60007 ) ;
#98755 = CARTESIAN_POINT ( 'NONE',  ( -7.019877749285432955, -17.24070752338410273, 20.23474786156467786 ) ) ;
#98756 = COLOUR_RGB ( '', 0.31764706, 0.68627451, 0.89019608) ;
#98757 = ORIENTED_EDGE ( 'NONE', *, *, #91218, .T. ) ;
#98758 = DIRECTION ( 'NONE',  ( 0.7071067811865487940, -0.7071067811865463515, 0.000000000000000000 ) ) ;
#98759 = FACE_OUTER_BOUND ( 'NONE', #26191, .T. ) ;
#98760 = CARTESIAN_POINT ( 'NONE',  ( -29.99999999999978328, -15.41253812416060143, 4.000000000000000000 ) ) ;
#98761 = CYLINDRICAL_SURFACE ( 'NONE', #94582, 2.247899999999996901 ) ;
#98762 = CARTESIAN_POINT ( 'NONE',  ( 36.51626352523145158, -4.472830434245839371, 4.472830434245839371 ) ) ;
#98763 = DIRECTION ( 'NONE',  ( 0.000000000000000000, -1.000000000000000000, 0.000000000000000000 ) ) ;
#98764 = EDGE_LOOP ( 'NONE', ( #19019, #11157, #61348, #110834 ) ) ;
#98765 = VERTEX_POINT ( 'NONE', #84959 ) ;
#98766 = CARTESIAN_POINT ( 'NONE',  ( 126.8541666666666572, -2.130196079827425315, -7.950000000000001066 ) ) ;
#98767 = ORIENTED_EDGE ( 'NONE', *, *, #131975, .T. ) ;
#98768 = VECTOR ( 'NONE', #91061, 1000.000000000000000 ) ;
#98769 = VERTEX_POINT ( 'NONE', #94395 ) ;
#98770 = FACE_OUTER_BOUND ( 'NONE', #5589, .T. ) ;
#98771 = CARTESIAN_POINT ( 'NONE',  ( -56.99451991528749062, 28.92564299267978001, 4.000000000000000000 ) ) ;
#98772 = VERTEX_POINT ( 'NONE', #116161 ) ;
#98773 = CARTESIAN_POINT ( 'NONE',  ( 0.1161069444170876042, 0.3999999999999995781, 2.220360628129161906 ) ) ;
#98774 = PLANE ( 'NONE',  #60636 ) ;
#98775 = DIRECTION ( 'NONE',  ( 0.7071067811865487940, -0.7071067811865463515, 0.000000000000000000 ) ) ;
#98776 = MECHANICAL_DESIGN_GEOMETRIC_PRESENTATION_REPRESENTATION (  '', ( #112663 ), #121951 ) ;
#98777 = CARTESIAN_POINT ( 'NONE',  ( -3.183988606268992161, 28.73617430169789699, 5.000000000000000000 ) ) ;
#98778 = CARTESIAN_POINT ( 'NONE',  ( 120.3129301918980758, -1.637169565754159617, -6.110000000000001208 ) ) ;
#98779 = EDGE_LOOP ( 'NONE', ( #131223, #96373, #8070, #24945 ) ) ;
#98780 = CARTESIAN_POINT ( 'NONE',  ( -15.29974487139158867, -27.71228299555216879, 4.000000000000000000 ) ) ;
#98781 = FILL_AREA_STYLE ('',( #120513 ) ) ;
#98782 = CARTESIAN_POINT ( 'NONE',  ( 78.14583333333332860, 2.130196079827431976, -7.949999999999998401 ) ) ;
#98783 = DIRECTION ( 'NONE',  ( 0.7071067811865487940, 0.7071067811865463515, 0.000000000000000000 ) ) ;
#98784 = FACE_OUTER_BOUND ( 'NONE', #32161, .T. ) ;
#98785 = VECTOR ( 'NONE', #117539, 1000.000000000000000 ) ;
#98786 = CARTESIAN_POINT ( 'NONE',  ( 34.92499999999998295, 22.22500000000000142, 4.000000000000000000 ) ) ;
#98787 = CARTESIAN_POINT ( 'NONE',  ( -21.18398860626899349, 28.73617430169802134, 5.000000000000000000 ) ) ;
#98788 = AXIS2_PLACEMENT_3D ( 'NONE', #45061, #131308, #31989 ) ;
#98789 = CARTESIAN_POINT ( 'NONE',  ( 60.01669371712956291, 7.950000000000001066, -2.130196079827421318 ) ) ;
#98790 = LINE ( 'NONE', #99494, #123148 ) ;
#98791 = EDGE_CURVE ( 'NONE', #33564, #110484, #129165, .T. ) ;
#98792 = CARTESIAN_POINT ( 'NONE',  ( 0.000000000000000000, 0.000000000000000000, 5.000000000000000000 ) ) ;
#98793 = VERTEX_POINT ( 'NONE', #61130 ) ;
#98794 = EDGE_LOOP ( 'NONE', ( #143350, #3979, #363, #25850 ) ) ;
#98795 = CARTESIAN_POINT ( 'NONE',  ( 41.54166666666665719, -3.975000000000002753, 6.884901960086286188 ) ) ;
#98796 = EDGE_CURVE ( 'NONE', #126386, #10226, #138643, .T. ) ;
#98797 = EDGE_CURVE ( 'NONE', #114851, #32784, #30601, .T. ) ;
#98798 = DIRECTION ( 'NONE',  ( -0.7071067811865486830, 0.7071067811865464625, 0.000000000000000000 ) ) ;
#98799 = ADVANCED_FACE ( 'NONE', ( #74831 ), #119009, .T. ) ;
#98800 = PLANE ( 'NONE',  #76257 ) ;
#98801 = EDGE_LOOP ( 'NONE', ( #91817, #126252, #12184, #131050 ) ) ;
#98802 = EDGE_CURVE ( 'NONE', #91029, #64292, #32740, .T. ) ;
#98803 = FACE_OUTER_BOUND ( 'NONE', #41437, .T. ) ;
#98804 = DIRECTION ( 'NONE',  ( 1.000000000000000000, 0.000000000000000000, 0.000000000000000000 ) ) ;
#98805 = CARTESIAN_POINT ( 'NONE',  ( 46.52126352523142572, -4.472830434245839371, -4.472830434245840259 ) ) ;
#98807 = ADVANCED_FACE ( 'NONE', ( #42907 ), #142906, .F. ) ;
#98806 = VERTEX_POINT ( 'NONE', #45769 ) ;
#98808 = CYLINDRICAL_SURFACE ( 'NONE', #13211, 0.5000000000000004441 ) ;
#98809 = ORIENTED_EDGE ( 'NONE', *, *, #1682, .T. ) ;
#98810 = EDGE_LOOP ( 'NONE', ( #28103, #16769, #20129, #31320 ) ) ;
#98811 = DIRECTION ( 'NONE',  ( -0.7071067811865486830, 0.7071067811865464625, 0.000000000000000000 ) ) ;
#98812 = CARTESIAN_POINT ( 'NONE',  ( 1.199999999999999956, 5.612226965700972570E-16, -4.582731094065999322 ) ) ;
#98813 = DIRECTION ( 'NONE',  ( -0.000000000000000000, -0.000000000000000000, 1.000000000000000000 ) ) ;
#98814 = EDGE_CURVE ( 'NONE', #16402, #126916, #121839, .T. ) ;
#98815 = DIRECTION ( 'NONE',  ( -0.7071067811865487940, 0.7071067811865463515, -0.000000000000000000 ) ) ;
#98816 = VERTEX_POINT ( 'NONE', #77669 ) ;
#98817 = EDGE_CURVE ( 'NONE', #18045, #93380, #53784, .T. ) ;
#98818 = DIRECTION ( 'NONE',  ( -1.000000000000000000, -1.224606353822377258E-16, -0.000000000000000000 ) ) ;
#98820 = VERTEX_POINT ( 'NONE', #67520 ) ;
#98819 = CARTESIAN_POINT ( 'NONE',  ( 8.795806282870438864, -5.278424836066144543, 3.047499999999995879 ) ) ;
#98821 = CARTESIAN_POINT ( 'NONE',  ( 78.45876352523144703, 0.000000000000000000, -6.110000000000001208 ) ) ;
#98822 = CARTESIAN_POINT ( 'NONE',  ( 14.29166666666666785, -3.047499999999994547, 5.278424836066145431 ) ) ;
#98823 = DIRECTION ( 'NONE',  ( -0.000000000000000000, -0.000000000000000000, -1.000000000000000000 ) ) ;
#98824 = CARTESIAN_POINT ( 'NONE',  ( 2.999999999999999112, -7.600000000000061817, 28.92499999999998650 ) ) ;
#98825 = VECTOR ( 'NONE', #55068, 1000.000000000000000 ) ;
#98826 = DIRECTION ( 'NONE',  ( -0.000000000000000000, -0.3543493200069152693, 0.9351131265310292928 ) ) ;
#98827 = SURFACE_STYLE_FILL_AREA ( #121300 ) ;
#98828 = EDGE_CURVE ( 'NONE', #34776, #91297, #23242, .T. ) ;
#98829 = ORIENTED_EDGE ( 'NONE', *, *, #17686, .T. ) ;
#98830 = AXIS2_PLACEMENT_3D ( 'NONE', #139779, #130322, #97666 ) ;
#98831 =( BOUNDED_CURVE ( )  B_SPLINE_CURVE ( 2, ( #137204, #47382, #16075, #60371, #91551, #125616, #104551, #16839, #14696, #26294, #103130, #70552, #127753 ),
 .UNSPECIFIED., .F., .T. ) 
 B_SPLINE_CURVE_WITH_KNOTS ( ( 3, 2, 2, 2, 2, 2, 3 ),
 ( 0.01666666666666668031, 0.01944444444444446210, 0.02222222222222224042, 0.02500000000000002220, 0.02777777777777779705, 0.03055555555555557884, 0.03333333333333336063 ),
 .UNSPECIFIED. ) 
 CURVE ( )  GEOMETRIC_REPRESENTATION_ITEM ( )  RATIONAL_B_SPLINE_CURVE ( ( 0.9999999999999997780, 0.9659258262890685343, 1.000000000000000000, 0.9659258262890683122, 1.000000000000000000, 0.9659258262890683122, 1.000000000000000000, 0.9659258262890683122, 1.000000000000000000, 0.9659258262890683122, 1.000000000000000000, 0.9659258262890679791, 1.000000000000000444 ) ) 
 REPRESENTATION_ITEM ( '' )  );
#98832 = DIRECTION ( 'NONE',  ( 0.3543493200069162685, -0.000000000000000000, -0.9351131265310288487 ) ) ;
#98833 = CARTESIAN_POINT ( 'NONE',  ( 65.82876352523145158, 0.000000000000000000, -6.109999999999998543 ) ) ;
#98834 = CARTESIAN_POINT ( 'NONE',  ( 156.1500000000000057, -49.14999999999999147, 49.92499999999997584 ) ) ;
#98835 = DIRECTION ( 'NONE',  ( -0.5735764363510499342, -0.8191520442889891340, 0.000000000000000000 ) ) ;
#98836 = CARTESIAN_POINT ( 'NONE',  ( 9.812461875839407099, -22.22500000000000142, 4.000000000000000000 ) ) ;
#98837 = ORIENTED_EDGE ( 'NONE', *, *, #38789, .T. ) ;
#98838 = VERTEX_POINT ( 'NONE', #776 ) ;
#98839 = VECTOR ( 'NONE', #122344, 1000.000000000000000 ) ;
#98840 = DIRECTION ( 'NONE',  ( 0.7071067811865487940, 0.7071067811865463515, -0.000000000000000000 ) ) ;
#98841 = VERTEX_POINT ( 'NONE', #12380 ) ;
#98842 = VERTEX_POINT ( 'NONE', #89936 ) ;
#98843 = LINE ( 'NONE', #41617, #11967 ) ;
#98844 = EDGE_LOOP ( 'NONE', ( #131687, #6664, #38036 ) ) ;
#98845 = CARTESIAN_POINT ( 'NONE',  ( 1.042387978378689573, -0.3999999999999998002, -2.015694669338588429 ) ) ;
#98846 = CARTESIAN_POINT ( 'NONE',  ( -68.99451991528748351, 28.92564299267986172, 4.000000000000000000 ) ) ;
#98847 = EDGE_CURVE ( 'NONE', #142366, #50434, #100828, .T. ) ;
#98848 = DIRECTION ( 'NONE',  ( 0.3543493200069162685, -0.000000000000000000, -0.9351131265310288487 ) ) ;
#98849 = VECTOR ( 'NONE', #99365, 1000.000000000000000 ) ;
#98850 = FACE_BOUND ( 'NONE', #18209, .T. ) ;
#98851 = LINE ( 'NONE', #96685, #116035 ) ;
#98852 = CARTESIAN_POINT ( 'NONE',  ( 51.48921356237309510, -27.52281430457091460, 5.000000000000000000 ) ) ;
#98854 = ORIENTED_EDGE ( 'NONE', *, *, #85371, .F. ) ;
#98853 = CARTESIAN_POINT ( 'NONE',  ( 0.000000000000000000, 0.000000000000000000, 0.000000000000000000 ) ) ;
#98855 = DIRECTION ( 'NONE',  ( -0.7071067811865486830, -0.7071067811865464625, -0.000000000000000000 ) ) ;
#98856 = VERTEX_POINT ( 'NONE', #97981 ) ;
#98857 = ORIENTED_EDGE ( 'NONE', *, *, #58100, .T. ) ;
#98858 = CARTESIAN_POINT ( 'NONE',  ( 75.89126352523143737, -4.472830434245838482, -4.472830434245838482 ) ) ;
#98859 = ORIENTED_EDGE ( 'NONE', *, *, #63964, .F. ) ;
#98860 = CARTESIAN_POINT ( 'NONE',  ( 21.18398860626899349, 28.73617430169802134, 5.000000000000000000 ) ) ;
#98861 = VECTOR ( 'NONE', #82145, 1000.000000000000227 ) ;
#98862 = CARTESIAN_POINT ( 'NONE',  ( 12.19999999999999574, -22.33999999999998565, -0.5000000000000004441 ) ) ;
#98863 = ADVANCED_FACE ( 'NONE', ( #66083 ), #120397, .F. ) ;
#98864 = ORIENTED_EDGE ( 'NONE', *, *, #24396, .T. ) ;
#98865 = CARTESIAN_POINT ( 'NONE',  ( 27.18398860626900060, 28.73617430169806042, 5.000000000000000000 ) ) ;
#98866 = CARTESIAN_POINT ( 'NONE',  ( -34.92500000000001137, -2.781974347153374882, -4.476077389926508943 ) ) ;
#98867 = DIRECTION ( 'NONE',  ( -0.000000000000000000, 0.000000000000000000, 1.000000000000000000 ) ) ;
#98868 = LINE ( 'NONE', #51832, #138100 ) ;
#98869 = EDGE_CURVE ( 'NONE', #114476, #8801, #66783, .T. ) ;
#98870 = DIRECTION ( 'NONE',  ( 0.3543493200069162685, -0.000000000000000000, -0.9351131265310288487 ) ) ;
#98871 = CARTESIAN_POINT ( 'NONE',  ( -1.499999999999984013, 19.46639925780206326, 5.000000000000000000 ) ) ;
#98872 = PLANE ( 'NONE',  #4545 ) ;
#98873 = EDGE_LOOP ( 'NONE', ( #8698, #2770, #27945, #20168, #14678 ) ) ;
#98874 = CARTESIAN_POINT ( 'NONE',  ( 4.288407645496676857, -2.499999999999999556, 0.000000000000000000 ) ) ;
#98875 = ORIENTED_EDGE ( 'NONE', *, *, #60175, .T. ) ;
#98876 = DIRECTION ( 'NONE',  ( 1.000000000000000000, 0.000000000000000000, 0.000000000000000000 ) ) ;
#98877 = PLANE ( 'NONE',  #18866 ) ;
#98878 = VERTEX_POINT ( 'NONE', #45071 ) ;
#98880 = VERTEX_POINT ( 'NONE', #119688 ) ;
#98879 = PRESENTATION_LAYER_ASSIGNMENT (  '', '', ( #31740 ) ) ;
#98881 = EDGE_CURVE ( 'NONE', #114745, #62013, #11643, .T. ) ;
#98882 = CARTESIAN_POINT ( 'NONE',  ( 36.45876352523143282, 0.000000000000000000, -6.110000000000001208 ) ) ;
#98883 = VERTEX_POINT ( 'NONE', #134184 ) ;
#98884 = DIRECTION ( 'NONE',  ( 0.000000000000000000, -1.000000000000000000, 0.000000000000000000 ) ) ;
#98885 = VECTOR ( 'NONE', #8006, 1000.000000000000227 ) ;
#98886 = VECTOR ( 'NONE', #95292, 1000.000000000000000 ) ;
#98887 = DIRECTION ( 'NONE',  ( -0.7071067811865487940, 0.7071067811865463515, -0.000000000000000000 ) ) ;
#98888 = CIRCLE ( 'NONE', #117399, 28.00000000000001776 ) ;
#98889 = CARTESIAN_POINT ( 'NONE',  ( 20.75413961620377279, 3.047499999999993214, -5.278424836066146320 ) ) ;
#98890 = CARTESIAN_POINT ( 'NONE',  ( -2.007830101563949921, 12.50197052871801340, -25.33253914797327866 ) ) ;
#98891 = ORIENTED_EDGE ( 'NONE', *, *, #96163, .F. ) ;
#98892 = DIRECTION ( 'NONE',  ( -0.6830127018922181881, 0.6830127018922202975, -0.2588190451025214056 ) ) ;
#98893 = ORIENTED_EDGE ( 'NONE', *, *, #105617, .F. ) ;
#98894 = FACE_OUTER_BOUND ( 'NONE', #116525, .T. ) ;
#98895 = VECTOR ( 'NONE', #120018, 999.9999999999998863 ) ;
#98896 = CARTESIAN_POINT ( 'NONE',  ( 10.17183060077639745, 18.75929247661552779, 4.000000000000000000 ) ) ;
#98898 = VERTEX_POINT ( 'NONE', #78374 ) ;
#98897 = CARTESIAN_POINT ( 'NONE',  ( 60.48921356237309510, -27.52281430457097500, 5.000000000000000000 ) ) ;
#98899 = ORIENTED_EDGE ( 'NONE', *, *, #70383, .T. ) ;
#98900 = LINE ( 'NONE', #7040, #79726 ) ;
#98901 = PLANE ( 'NONE',  #5187 ) ;
#98902 = LINE ( 'NONE', #132300, #97978 ) ;
#98903 = VERTEX_POINT ( 'NONE', #32001 ) ;
#98904 = DIRECTION ( 'NONE',  ( 0.7071067811865487940, 0.7071067811865463515, 0.000000000000000000 ) ) ;
#98906 = ORIENTED_EDGE ( 'NONE', *, *, #102805, .T. ) ;
#98905 = ADVANCED_FACE ( 'NONE', ( #55922 ), #54496, .F. ) ;
#98907 = EDGE_LOOP ( 'NONE', ( #65936, #77186, #137745, #100260 ) ) ;
#98908 = DIRECTION ( 'NONE',  ( 0.000000000000000000, 0.000000000000000000, 1.000000000000000000 ) ) ;
#98909 = DIRECTION ( 'NONE',  ( -0.7071067811865486830, -0.7071067811865464625, -0.000000000000000000 ) ) ;
#98910 = DIRECTION ( 'NONE',  ( -0.000000000000000000, 1.000000000000000000, -0.000000000000000000 ) ) ;
#98911 = CARTESIAN_POINT ( 'NONE',  ( 4.499999999999968914, -6.839392718269127869, -8.480912228396096708 ) ) ;
#98912 = FACE_OUTER_BOUND ( 'NONE', #39929, .T. ) ;
#98914 = ADVANCED_FACE ( 'NONE', ( #44338 ), #87103, .F. ) ;
#98913 = CARTESIAN_POINT ( 'NONE',  ( 60.18398860626900415, 28.73617430169829490, 5.000000000000000000 ) ) ;
#98915 = PLANE ( 'NONE',  #59955 ) ;
#98916 = EDGE_LOOP ( 'NONE', ( #90995, #114645, #17749, #124379 ) ) ;
#98917 = EDGE_CURVE ( 'NONE', #129819, #9868, #133469, .T. ) ;
#98918 = CARTESIAN_POINT ( 'NONE',  ( 11.29289321881337393, 8.259292476615636147, 5.000000000000000000 ) ) ;
#98919 = VERTEX_POINT ( 'NONE', #65384 ) ;
#98920 = VECTOR ( 'NONE', #75888, 1000.000000000000000 ) ;
#98921 = DIRECTION ( 'NONE',  ( 0.7071067811865486830, -0.7071067811865464625, -0.000000000000000000 ) ) ;
#98922 = DIRECTION ( 'NONE',  ( 0.7071067811865487940, 0.7071067811865463515, -0.000000000000000000 ) ) ;
#98923 = CARTESIAN_POINT ( 'NONE',  ( 25.39999999999999858, -16.48000000000005016, -33.92499999999998295 ) ) ;
#98924 = VERTEX_POINT ( 'NONE', #109560 ) ;
#98925 = CARTESIAN_POINT ( 'NONE',  ( 10.00193056682090642, -22.22500000000000142, 4.500000000000000888 ) ) ;
#98926 = CARTESIAN_POINT ( 'NONE',  ( -60.18398860626900415, 28.73617430169829490, 5.000000000000000000 ) ) ;
#98927 = CARTESIAN_POINT ( 'NONE',  ( 21.59770000000000323, 3.130000000000007887, 0.000000000000000000 ) ) ;
#98928 = VERTEX_POINT ( 'NONE', #33469 ) ;
#98929 = ORIENTED_EDGE ( 'NONE', *, *, #26029, .F. ) ;
#98930 = CARTESIAN_POINT ( 'NONE',  ( 4.499999999999979572, 7.087461875839172087, 4.000000000000000000 ) ) ;
#98931 = CARTESIAN_POINT ( 'NONE',  ( 1.353980332882009030, 2.500000000000000888, 0.000000000000000000 ) ) ;
#98932 = DIRECTION ( 'NONE',  ( -0.7071067811865487940, 0.7071067811865463515, 0.000000000000000000 ) ) ;
#98933 = VECTOR ( 'NONE', #13407, 1000.000000000000000 ) ;
#98934 = CARTESIAN_POINT ( 'NONE',  ( -26.70025512860841488, -27.71228299555187391, 4.000000000000000000 ) ) ;
#98935 = CARTESIAN_POINT ( 'NONE',  ( -25.39999999999996305, 3.061616997868383141E-16, -2.500000000000000000 ) ) ;
#98936 = CARTESIAN_POINT ( 'NONE',  ( 68.74543019189812298, -5.291415217122919401, -3.055000000000000604 ) ) ;
#98937 = ADVANCED_FACE ( 'NONE', ( #10237 ), #37, .F. ) ;
#98938 = DIRECTION ( 'NONE',  ( 0.7071067811865487940, 0.7071067811865463515, 0.000000000000000000 ) ) ;
#98939 = CARTESIAN_POINT ( 'NONE',  ( -54.29974487139159578, -27.71228299555243879, 4.000000000000000000 ) ) ;
#98940 =( LENGTH_UNIT ( ) NAMED_UNIT ( * ) SI_UNIT ( .MILLI., .METRE. ) );
#98941 = LINE ( 'NONE', #116064, #95020 ) ;
#98942 = ORIENTED_EDGE ( 'NONE', *, *, #118218, .T. ) ;
#98943 = CARTESIAN_POINT ( 'NONE',  ( 11.99999999999992184, -6.412538124160689357, 4.000000000000000000 ) ) ;
#98944 = AXIS2_PLACEMENT_3D ( 'NONE', #3558, #102917, #92020 ) ;
#98945 = VERTEX_POINT ( 'NONE', #136304 ) ;
#98946 = DIRECTION ( 'NONE',  ( -0.7071067811865486830, -0.7071067811865464625, 0.000000000000000000 ) ) ;
#98947 = CARTESIAN_POINT ( 'NONE',  ( -27.18398860626900060, 28.73617430169806042, 5.000000000000000000 ) ) ;
#98948 = DIRECTION ( 'NONE',  ( -0.000000000000000000, 0.3543493200069153248, 0.9351131265310292928 ) ) ;
#98949 = CARTESIAN_POINT ( 'NONE',  ( -13.49999999999990052, 0.4311230773921797543, 4.000000000000000000 ) ) ;
#98950 = PRESENTATION_STYLE_ASSIGNMENT (( #65681 ) ) ;
#98951 = CARTESIAN_POINT ( 'NONE',  ( -20.18753812416038329, -22.22500000000000142, 4.000000000000000000 ) ) ;
#98952 = CARTESIAN_POINT ( 'NONE',  ( -23.93988928955965889, -9.740707523384180888, 10.89222023123386585 ) ) ;
#98953 = ORIENTED_EDGE ( 'NONE', *, *, #54102, .F. ) ;
#98954 = VERTEX_POINT ( 'NONE', #134925 ) ;
#98955 = CARTESIAN_POINT ( 'NONE',  ( 90.78752705046288440, 0.000000000000000000, -7.949999999999998401 ) ) ;
#98956 = DIRECTION ( 'NONE',  ( 0.7071067811865487940, 0.7071067811865463515, 0.000000000000000000 ) ) ;
#98957 = CARTESIAN_POINT ( 'NONE',  ( -0.2997448713915885632, -27.71228299555206220, 4.000000000000000000 ) ) ;
#98958 = CARTESIAN_POINT ( 'NONE',  ( 88.45419371712957002, 6.884901960086283523, 3.975000000000002753 ) ) ;
#98959 = LINE ( 'NONE', #133758, #27799 ) ;
#98960 = ADVANCED_FACE ( 'NONE', ( #2934 ), #37736, .F. ) ;
#98961 = CARTESIAN_POINT ( 'NONE',  ( -6.183988606268994381, 28.73617430169791476, 5.000000000000000000 ) ) ;
#98962 = ORIENTED_EDGE ( 'NONE', *, *, #43420, .T. ) ;
#98963 = AXIS2_PLACEMENT_3D ( 'NONE', #24692, #110255, #13084 ) ;
#98964 = CARTESIAN_POINT ( 'NONE',  ( 81.35416666666667140, -2.130196079827425315, -7.950000000000001066 ) ) ;
#98965 = DIRECTION ( 'NONE',  ( -0.7071067811865486830, -0.7071067811865464625, -0.000000000000000000 ) ) ;
#98966 = ADVANCED_FACE ( 'NONE', ( #93524, #24687 ), #102978, .F. ) ;
#98967 = CARTESIAN_POINT ( 'NONE',  ( -24.32816939922335919, -0.7407075233842701500, 4.000000000000000000 ) ) ;
#98968 = FACE_OUTER_BOUND ( 'NONE', #27676, .T. ) ;
#98969 = EDGE_LOOP ( 'NONE', ( #70035, #47715, #142539, #131110 ) ) ;
#98970 = ADVANCED_FACE ( 'NONE', ( #79842 ), #13786, .F. ) ;
#98971 = ADVANCED_FACE ( 'NONE', ( #3615 ), #124019, .F. ) ;
#98972 = DIRECTION ( 'NONE',  ( 0.7071067811865486830, -0.7071067811865464625, -0.000000000000000000 ) ) ;
#98973 = ORIENTED_EDGE ( 'NONE', *, *, #113138, .F. ) ;
#98974 = CIRCLE ( 'NONE', #140681, 2.055000000000000604 ) ;
#98975 = DIRECTION ( 'NONE',  ( 0.7071067811865486830, -0.7071067811865464625, -0.000000000000000000 ) ) ;
#98976 = CARTESIAN_POINT ( 'NONE',  ( 73.20876352523143282, -7.482591942790329030E-16, 6.110000000000001208 ) ) ;
#98977 = LINE ( 'NONE', #103107, #47771 ) ;
#98978 = ORIENTED_EDGE ( 'NONE', *, *, #76222, .T. ) ;
#98979 = DIRECTION ( 'NONE',  ( -0.000000000000000000, 0.000000000000000000, 1.000000000000000000 ) ) ;
#98980 = VECTOR ( 'NONE', #81098, 1000.000000000000000 ) ;
#98981 = DIRECTION ( 'NONE',  ( 1.000000000000000000, 0.000000000000000000, 0.000000000000000000 ) ) ;
#98982 = CARTESIAN_POINT ( 'NONE',  ( -84.29974487139159578, -27.71228299555264840, 4.000000000000000000 ) ) ;
#98983 = PRESENTATION_LAYER_ASSIGNMENT (  '', '', ( #52724 ) ) ;
#98984 = EDGE_CURVE ( 'NONE', #112859, #81705, #115225, .T. ) ;
#98985 = CARTESIAN_POINT ( 'NONE',  ( 4.495848767239241539, 0.000000000000000000, 2.500000000000000444 ) ) ;
#98986 = ADVANCED_FACE ( 'NONE', ( #15214 ), #102282, .F. ) ;
#98987 = FACE_OUTER_BOUND ( 'NONE', #128800, .T. ) ;
#98989 = VERTEX_POINT ( 'NONE', #123326 ) ;
#98988 = LINE ( 'NONE', #119310, #35983 ) ;
#98990 = FILL_AREA_STYLE_COLOUR ( '', #101602 ) ;
#98991 = PLANE ( 'NONE',  #38385 ) ;
#98992 = CARTESIAN_POINT ( 'NONE',  ( 16.49999999999988987, -13.53360074219760278, 5.000000000000000000 ) ) ;
#98993 = VECTOR ( 'NONE', #60956, 1000.000000000000000 ) ;
#98994 = VECTOR ( 'NONE', #55204, 1000.000000000000000 ) ;
#98995 = ORIENTED_EDGE ( 'NONE', *, *, #78535, .F. ) ;
#98996 = ADVANCED_FACE ( 'NONE', ( #49342 ), #47909, .F. ) ;
#98997 = EDGE_LOOP ( 'NONE', ( #32418, #90412, #57910, #91063 ) ) ;
#98998 = CARTESIAN_POINT ( 'NONE',  ( 60.37543019189810423, -5.291415217122920289, -3.055000000000001492 ) ) ;
#98999 = ORIENTED_EDGE ( 'NONE', *, *, #79423, .T. ) ;
#99000 = CARTESIAN_POINT ( 'NONE',  ( 5.510786437626906675, -27.52281430457051314, 5.000000000000000000 ) ) ;
#99001 = DIRECTION ( 'NONE',  ( -1.000000000000000000, -1.224606353822377258E-16, -0.000000000000000000 ) ) ;
#99003 = CIRCLE ( 'NONE', #52652, 2.500000000000000888 ) ;
#99002 = CARTESIAN_POINT ( 'NONE',  ( 125.2041937171295700, -6.884901960086285300, -3.975000000000000089 ) ) ;
#99004 = ORIENTED_EDGE ( 'NONE', *, *, #84884, .F. ) ;
#99006 = EDGE_CURVE ( 'NONE', #9403, #139296, #26132, .T. ) ;
#99005 = VERTEX_POINT ( 'NONE', #48593 ) ;
#99007 = CARTESIAN_POINT ( 'NONE',  ( 16.49999999999988276, -5.568876922607752356, 4.000000000000000000 ) ) ;
#99008 = SURFACE_STYLE_USAGE ( .BOTH. , #41075 ) ;
#99009 = ORIENTED_EDGE ( 'NONE', *, *, #29855, .T. ) ;
#99010 = DIRECTION ( 'NONE',  ( 0.7071067811865487940, -0.7071067811865463515, 0.000000000000000000 ) ) ;
#99011 = CARTESIAN_POINT ( 'NONE',  ( -4.499999999999966249, 9.431123077392085108, 4.000000000000000000 ) ) ;
#99012 = EDGE_CURVE ( 'NONE', #85868, #78770, #70396, .T. ) ;
#99013 = CARTESIAN_POINT ( 'NONE',  ( -33.70701326429281153, -21.74070752338405299, 4.999753212805220670 ) ) ;
#99014 = ORIENTED_EDGE ( 'NONE', *, *, #79482, .T. ) ;
#99015 = CARTESIAN_POINT ( 'NONE',  ( 10.82816939922345689, 0.7592924766157113092, 4.000000000000000000 ) ) ;
#99016 = PLANE ( 'NONE',  #61856 ) ;
#99017 = ADVANCED_FACE ( 'NONE', ( #30411 ), #139907, .F. ) ;
#99018 = CARTESIAN_POINT ( 'NONE',  ( -8.994519915287490619, 28.92564299267944250, 4.000000000000000000 ) ) ;
#99019 = CARTESIAN_POINT ( 'NONE',  ( 0.000000000000000000, 0.000000000000000000, 5.000000000000000000 ) ) ;
#99021 = EDGE_CURVE ( 'NONE', #88761, #58598, #23456, .T. ) ;
#99020 = VECTOR ( 'NONE', #112449, 1000.000000000000000 ) ;
#99022 = DIRECTION ( 'NONE',  ( -0.000000000000000000, 0.000000000000000000, 1.000000000000000000 ) ) ;
#99023 = DIRECTION ( 'NONE',  ( 0.7071067811865487940, 0.7071067811865463515, 0.000000000000000000 ) ) ;
#99024 = EDGE_CURVE ( 'NONE', #141704, #4133, #139196, .T. ) ;
#99025 = VERTEX_POINT ( 'NONE', #50032 ) ;
#99026 = EDGE_LOOP ( 'NONE', ( #65629, #25683, #18140, #122995 ) ) ;
#99027 = CARTESIAN_POINT ( 'NONE',  ( 117.1620968585647802, -5.291415217122919401, 3.054999999999997939 ) ) ;
#99028 = ORIENTED_EDGE ( 'NONE', *, *, #2727, .F. ) ;
#99029 = ORIENTED_EDGE ( 'NONE', *, *, #89128, .T. ) ;
#99030 = LINE ( 'NONE', #25042, #95611 ) ;
#99031 = CARTESIAN_POINT ( 'NONE',  ( -31.49999999999979039, -1.592773361805400301, -6.492772025301160710 ) ) ;
#99032 = CARTESIAN_POINT ( 'NONE',  ( 6.489213562373093325, -27.52281430457059841, 5.000000000000000000 ) ) ;
#99033 = ORIENTED_EDGE ( 'NONE', *, *, #13389, .T. ) ;
#99034 = CARTESIAN_POINT ( 'NONE',  ( 68.03752705046289861, -9.735942053221456900E-16, 7.949999999999998401 ) ) ;
#99035 = PLANE ( 'NONE',  #70359 ) ;
#99036 = FACE_BOUND ( 'NONE', #57084, .T. ) ;
#99037 = CARTESIAN_POINT ( 'NONE',  ( 0.000000000000000000, 0.000000000000000000, 5.000000000000000000 ) ) ;
#99038 = LINE ( 'NONE', #1149, #64637 ) ;
#99039 = CARTESIAN_POINT ( 'NONE',  ( 181.1499999999998067, -49.85820393249933602, -34.92499999999995453 ) ) ;
#99040 = VERTEX_POINT ( 'NONE', #116698 ) ;
#99041 = DIRECTION ( 'NONE',  ( -0.000000000000000000, 0.000000000000000000, 1.000000000000000000 ) ) ;
#99042 = FACE_OUTER_BOUND ( 'NONE', #129258, .T. ) ;
#99043 = ORIENTED_EDGE ( 'NONE', *, *, #141979, .T. ) ;
#99044 = ORIENTED_EDGE ( 'NONE', *, *, #127401, .F. ) ;
#99045 = ORIENTED_EDGE ( 'NONE', *, *, #15934, .T. ) ;
#99046 = CARTESIAN_POINT ( 'NONE',  ( 63.58376352523143993, -6.110000000000001208, -3.741295971395164515E-16 ) ) ;
#99047 = EDGE_LOOP ( 'NONE', ( #115384, #55902, #63045, #132625 ) ) ;
#99048 = FACE_OUTER_BOUND ( 'NONE', #86006, .T. ) ;
#99049 =( NAMED_UNIT ( * ) PLANE_ANGLE_UNIT ( ) SI_UNIT ( $, .RADIAN. ) );
#99050 = VECTOR ( 'NONE', #78043, 1000.000000000000227 ) ;
#99051 = CARTESIAN_POINT ( 'NONE',  ( 101.9379301918980900, -6.110000000000001208, 1.637169565754158951 ) ) ;
#99052 = DIRECTION ( 'NONE',  ( 0.7071067811865487940, 0.7071067811865463515, 0.000000000000000000 ) ) ;
#99053 = CARTESIAN_POINT ( 'NONE',  ( 4.966599676569746435, 6.759292476615653023, 12.28218704918523230 ) ) ;
#99054 = ORIENTED_EDGE ( 'NONE', *, *, #89600, .T. ) ;
#99055 = FACE_OUTER_BOUND ( 'NONE', #94152, .T. ) ;
#99056 = PLANE ( 'NONE',  #102641 ) ;
#99057 = DIRECTION ( 'NONE',  ( 1.000000000000000000, 0.000000000000000000, 0.000000000000000000 ) ) ;
#99058 = DIRECTION ( 'NONE',  ( 1.000000000000000000, 0.000000000000000000, 0.000000000000000000 ) ) ;
#99059 = EDGE_LOOP ( 'NONE', ( #107186, #16719, #45947, #106281 ) ) ;
#99060 = CIRCLE ( 'NONE', #136128, 2.500000000000000444 ) ;
#99061 = ORIENTED_EDGE ( 'NONE', *, *, #6508, .F. ) ;
#99062 = ORIENTED_EDGE ( 'NONE', *, *, #101746, .T. ) ;
#99063 = VERTEX_POINT ( 'NONE', #29671 ) ;
#99064 = CARTESIAN_POINT ( 'NONE',  ( 125.7662635252314658, 4.472830434245838482, -4.472830434245837594 ) ) ;
#99065 = ORIENTED_EDGE ( 'NONE', *, *, #67109, .T. ) ;
#99066 = VECTOR ( 'NONE', #112127, 1000.000000000000227 ) ;
#99067 = CARTESIAN_POINT ( 'NONE',  ( 45.29974487139158867, -27.71228299555237840, 4.000000000000000000 ) ) ;
#99068 = AXIS2_PLACEMENT_3D ( 'NONE', #58278, #24169, #57533 ) ;
#99069 = EDGE_CURVE ( 'NONE', #25861, #6819, #82656, .T. ) ;
#99070 = LINE ( 'NONE', #108507, #76439 ) ;
#99071 = EDGE_LOOP ( 'NONE', ( #62437, #48606, #123705, #79204 ) ) ;
#99072 = EDGE_CURVE ( 'NONE', #100985, #474, #18054, .T. ) ;
#99073 = CARTESIAN_POINT ( 'NONE',  ( 20.47599861414536448, 22.03583458319438648, 4.979811245910087614 ) ) ;
#99074 = VERTEX_POINT ( 'NONE', #63768 ) ;
#99075 = VECTOR ( 'NONE', #131347, 999.9999999999998863 ) ;
#99076 = VECTOR ( 'NONE', #137768, 1000.000000000000000 ) ;
#99077 = CARTESIAN_POINT ( 'NONE',  ( 8.874569808101886892, 6.871911579029510442, -3.967499999999998916 ) ) ;
#99078 = DIRECTION ( 'NONE',  ( -0.000000000000000000, 0.3543493200069153248, 0.9351131265310292928 ) ) ;
#99079 = CARTESIAN_POINT ( 'NONE',  ( 54.18398860626899705, 28.73617430169825226, 5.000000000000000000 ) ) ;
#99080 = EDGE_CURVE ( 'NONE', #49447, #141655, #39149, .T. ) ;
#99081 = CARTESIAN_POINT ( 'NONE',  ( -20.20710678118639692, -5.240707523384227073, 5.000000000000000000 ) ) ;
#99082 = ORIENTED_EDGE ( 'NONE', *, *, #30022, .T. ) ;
#99083 = ORIENTED_EDGE ( 'NONE', *, *, #102124, .F. ) ;
#99084 = EDGE_LOOP ( 'NONE', ( #137838, #38559, #100493, #66085 ) ) ;
#99085 = CARTESIAN_POINT ( 'NONE',  ( 19.68750000000000000, 4.461849672132297329, -4.461849672132302658 ) ) ;
#99086 = LINE ( 'NONE', #494, #118208 ) ;
#99087 = CARTESIAN_POINT ( 'NONE',  ( -30.18398860626900060, 28.73617430169808173, 5.000000000000000000 ) ) ;
#99088 = DIRECTION ( 'NONE',  ( -0.6830127018922180770, -0.6830127018922204085, -0.2588190451025213501 ) ) ;
#99089 = EDGE_CURVE ( 'NONE', #142779, #124724, #67487, .T. ) ;
#99090 = CARTESIAN_POINT ( 'NONE',  ( 19.49999999999985434, -17.94781430457064531, 5.000000000000000000 ) ) ;
#99091 = CARTESIAN_POINT ( 'NONE',  ( -11.99999999999991651, 4.931123077392129517, 4.000000000000000000 ) ) ;
#99092 = DIRECTION ( 'NONE',  ( 0.7071067811865487940, 0.7071067811865463515, 0.000000000000000000 ) ) ;
#99093 = CARTESIAN_POINT ( 'NONE',  ( -23.14994871458961967, -8.240707523384193323, 17.25253755692233781 ) ) ;
#99094 = ORIENTED_EDGE ( 'NONE', *, *, #3701, .T. ) ;
#99095 = DIRECTION ( 'NONE',  ( -0.7071067811865486830, -0.7071067811865464625, -0.000000000000000000 ) ) ;
#99096 = ORIENTED_EDGE ( 'NONE', *, *, #37001, .F. ) ;
#99097 = EDGE_CURVE ( 'NONE', #80191, #124824, #118835, .T. ) ;
#99098 = FACE_OUTER_BOUND ( 'NONE', #4086, .T. ) ;
#99099 = EDGE_LOOP ( 'NONE', ( #9151, #110677, #31805, #108803 ) ) ;
#99100 =( BOUNDED_CURVE ( )  B_SPLINE_CURVE ( 2, ( #130363, #18699, #42653, #62978, #120141, #107153, #140495, #84701, #43346, #86134, #40502, #96955, #119438 ),
 .UNSPECIFIED., .F., .T. ) 
 B_SPLINE_CURVE_WITH_KNOTS ( ( 3, 2, 2, 2, 2, 2, 3 ),
 ( 0.3333333333333333148, 0.3361111111111111382, 0.3388888888888889062, 0.3416666666666666741, 0.3444444444444444420, 0.3472222222222222099, 0.3499999999999999778 ),
 .UNSPECIFIED. ) 
 CURVE ( )  GEOMETRIC_REPRESENTATION_ITEM ( )  RATIONAL_B_SPLINE_CURVE ( ( 1.000000000000000000, 0.9659258262890683122, 1.000000000000000000, 0.9659258262890683122, 1.000000000000000000, 0.9659258262890683122, 1.000000000000000000, 0.9659258262890683122, 1.000000000000000000, 0.9659258262890683122, 1.000000000000000000, 0.9659258262890683122, 1.000000000000000000 ) ) 
 REPRESENTATION_ITEM ( '' )  );
#99101 = VECTOR ( 'NONE', #4555, 1000.000000000000227 ) ;
#99102 = CARTESIAN_POINT ( 'NONE',  ( 36.18398860626899705, 28.73617430169812437, 5.000000000000000000 ) ) ;
#99104 = VERTEX_POINT ( 'NONE', #117381 ) ;
#99103 = CARTESIAN_POINT ( 'NONE',  ( 42.85416666666666430, -2.130196079827425759, -7.950000000000000178 ) ) ;
#99105 = DIRECTION ( 'NONE',  ( -0.7071067811865487940, 0.7071067811865463515, -0.000000000000000000 ) ) ;
#99106 = ORIENTED_EDGE ( 'NONE', *, *, #135630, .F. ) ;
#99108 = VECTOR ( 'NONE', #11490, 1000.000000000000000 ) ;
#99107 = DIRECTION ( 'NONE',  ( -0.7071067811865486830, -0.7071067811865463515, 0.000000000000000000 ) ) ;
#99109 = ORIENTED_EDGE ( 'NONE', *, *, #91764, .T. ) ;
#99110 = CARTESIAN_POINT ( 'NONE',  ( -2.999999999999975131, 17.96639925780208102, 5.000000000000000000 ) ) ;
#99111 = VERTEX_POINT ( 'NONE', #83370 ) ;
#99112 = CARTESIAN_POINT ( 'NONE',  ( -31.49999999999977973, 4.466399257802215139, 5.000000000000000000 ) ) ;
#99113 = CARTESIAN_POINT ( 'NONE',  ( 109.6000270504628844, 5.819803920172570422, 5.819803920172574863 ) ) ;
#99114 = CARTESIAN_POINT ( 'NONE',  ( 153.6500000000000057, 0.000000000000000000, 0.000000000000000000 ) ) ;
#99115 = LINE ( 'NONE', #108551, #94556 ) ;
#99117 = EDGE_CURVE ( 'NONE', #97669, #68590, #105790, .T. ) ;
#99116 = CARTESIAN_POINT ( 'NONE',  ( -34.92500000000001137, 22.22500000000000142, 4.000000000000000000 ) ) ;
#99118 = DIRECTION ( 'NONE',  ( -0.000000000000000000, 0.3543493200069153248, 0.9351131265310292928 ) ) ;
#99119 = CARTESIAN_POINT ( 'NONE',  ( 17.79166666666666785, -3.047499999999994547, 5.278424836066145431 ) ) ;
#99120 = CARTESIAN_POINT ( 'NONE',  ( 17.62456980810188867, -6.871911579029512218, 3.967499999999996252 ) ) ;
#99121 = VECTOR ( 'NONE', #104214, 1000.000000000000000 ) ;
#99122 = LINE ( 'NONE', #1242, #4898 ) ;
#99123 = PLANE ( 'NONE',  #96402 ) ;
#99124 = ORIENTED_EDGE ( 'NONE', *, *, #104730, .T. ) ;
#99127 = VERTEX_POINT ( 'NONE', #16664 ) ;
#99126 = EDGE_CURVE ( 'NONE', #17542, #22488, #42002, .T. ) ;
#99125 = VECTOR ( 'NONE', #102702, 1000.000000000000227 ) ;
#99128 = ADVANCED_FACE ( 'NONE', ( #40585 ), #107928, .F. ) ;
#99129 = DIRECTION ( 'NONE',  ( 0.7071067811865486830, -0.7071067811865464625, -0.000000000000000000 ) ) ;
#99130 = VERTEX_POINT ( 'NONE', #137759 ) ;
#99131 = CARTESIAN_POINT ( 'NONE',  ( -0.9891197134605101970, -22.02621442084248216, 4.990779571109223767 ) ) ;
#99132 = DIRECTION ( 'NONE',  ( -0.7071067811865487940, 0.7071067811865463515, 0.000000000000000000 ) ) ;
#99133 = CARTESIAN_POINT ( 'NONE',  ( -9.489213562373095101, -27.52281430457062328, 5.000000000000000000 ) ) ;
#99134 = PRESENTATION_STYLE_ASSIGNMENT (( #99881 ) ) ;
#99135 = ORIENTED_EDGE ( 'NONE', *, *, #140665, .T. ) ;
#99136 = EDGE_CURVE ( 'NONE', #6439, #111777, #85477, .T. ) ;
#99137 = FACE_OUTER_BOUND ( 'NONE', #68022, .T. ) ;
#99138 = CARTESIAN_POINT ( 'NONE',  ( -29.99999999999977973, -13.44781430457069149, 5.000000000000000000 ) ) ;
#99139 = CARTESIAN_POINT ( 'NONE',  ( 3.792893218813434775, -2.240707523384260824, 5.000000000000000000 ) ) ;
#99140 = ADVANCED_FACE ( 'NONE', ( #38435 ), #140578, .F. ) ;
#99141 = CARTESIAN_POINT ( 'NONE',  ( 34.92499999999998295, 10.51246187583937441, 4.000000000000000000 ) ) ;
#99142 = EDGE_CURVE ( 'NONE', #80484, #71410, #77511, .T. ) ;
#99143 = CARTESIAN_POINT ( 'NONE',  ( 5.816011393731002066, 28.73617430169783304, 5.000000000000000000 ) ) ;
#99145 = ORIENTED_EDGE ( 'NONE', *, *, #94515, .F. ) ;
#99144 = LINE ( 'NONE', #122328, #91442 ) ;
#99146 = CARTESIAN_POINT ( 'NONE',  ( -2.700255128608413990, -27.71228299555204089, 4.000000000000000000 ) ) ;
#99147 = PRESENTATION_STYLE_ASSIGNMENT (( #32508 ) ) ;
#99148 = DIRECTION ( 'NONE',  ( 0.7071067811865487940, 0.7071067811865463515, -0.000000000000000000 ) ) ;
#99149 = CARTESIAN_POINT ( 'NONE',  ( 32.99999999999976552, -3.033600742197707145, 5.000000000000000000 ) ) ;
#99150 = EDGE_LOOP ( 'NONE', ( #110074, #63816, #19789, #54617, #57477 ) ) ;
#99151 = ORIENTED_EDGE ( 'NONE', *, *, #141852, .F. ) ;
#99152 = VERTEX_POINT ( 'NONE', #21676 ) ;
#99153 = CARTESIAN_POINT ( 'NONE',  ( 96.10459685856477563, 1.637169565754164946, -6.109999999999999432 ) ) ;
#99154 = AXIS2_PLACEMENT_3D ( 'NONE', #109761, #54688, #85147 ) ;
#99155 = ORIENTED_EDGE ( 'NONE', *, *, #60664, .F. ) ;
#99156 = ADVANCED_FACE ( 'NONE', ( #142050 ), #67340, .T. ) ;
#99157 = LINE ( 'NONE', #56456, #50328 ) ;
#99158 = DIRECTION ( 'NONE',  ( 0.7071067811865487940, -0.7071067811865463515, 0.000000000000000000 ) ) ;
#99159 = ORIENTED_EDGE ( 'NONE', *, *, #49080, .F. ) ;
#99160 = EDGE_CURVE ( 'NONE', #141003, #7076, #86229, .T. ) ;
#99161 = CARTESIAN_POINT ( 'NONE',  ( -31.49999999999977973, 15.43112307739202471, 4.000000000000000000 ) ) ;
#99162 = CARTESIAN_POINT ( 'NONE',  ( 49.41666666666666430, -6.884901960086287076, -3.975000000000000977 ) ) ;
#99163 = CARTESIAN_POINT ( 'NONE',  ( 87.41209685856478018, 5.291415217122921177, -3.054999999999994831 ) ) ;
#99164 = VERTEX_POINT ( 'NONE', #89090 ) ;
#99165 = CARTESIAN_POINT ( 'NONE',  ( 42.48921356237308800, -27.52281430457085065, 5.000000000000000000 ) ) ;
#99166 = CARTESIAN_POINT ( 'NONE',  ( 115.6250000000000000, -7.950000000000000178, -4.867971026610729436E-16 ) ) ;
#99167 = VECTOR ( 'NONE', #117261, 1000.000000000000000 ) ;
#99168 = VERTEX_POINT ( 'NONE', #12208 ) ;
#99169 = ORIENTED_EDGE ( 'NONE', *, *, #34243, .F. ) ;
#99170 = VECTOR ( 'NONE', #134181, 1000.000000000000227 ) ;
#99171 = ORIENTED_EDGE ( 'NONE', *, *, #28880, .F. ) ;
#99172 = DIRECTION ( 'NONE',  ( 0.000000000000000000, -1.000000000000000000, 0.000000000000000000 ) ) ;
#99173 = AXIS2_PLACEMENT_3D ( 'NONE', #72420, #62953, #96231 ) ;
#99174 = CARTESIAN_POINT ( 'NONE',  ( 14.99999999999990230, 14.58746187583908416, 4.000000000000000000 ) ) ;
#99175 = CARTESIAN_POINT ( 'NONE',  ( 19.31706980810189123, -2.126176841940956130, 7.934999999999990727 ) ) ;
#99176 = CARTESIAN_POINT ( 'NONE',  ( -24.48921356237309510, -27.52281430457072631, 5.000000000000000000 ) ) ;
#99177 = VECTOR ( 'NONE', #10099, 1000.000000000000227 ) ;
#99178 = VECTOR ( 'NONE', #40431, 1000.000000000000000 ) ;
#99179 = CARTESIAN_POINT ( 'NONE',  ( 3.302882771356463465, -48.98543874033774159, -39.51758185027075143 ) ) ;
#99180 = CARTESIAN_POINT ( 'NONE',  ( 3.328169399223498637, 11.25929247661560417, 4.000000000000000000 ) ) ;
#99181 = EDGE_CURVE ( 'NONE', #34556, #20392, #65925, .T. ) ;
#99183 = EDGE_CURVE ( 'NONE', #28440, #60272, #141301, .T. ) ;
#99182 =( NAMED_UNIT ( * ) SI_UNIT ( $, .STERADIAN. ) SOLID_ANGLE_UNIT ( ) );
#99184 = EDGE_LOOP ( 'NONE', ( #35292, #24856, #12460, #132717 ) ) ;
#99185 = EDGE_LOOP ( 'NONE', ( #64859, #61820, #134890, #43119 ) ) ;
#99186 = CARTESIAN_POINT ( 'NONE',  ( 25.49999999999982592, 14.14708470758593251, -0.5283514160167148699 ) ) ;
#99187 = VERTEX_POINT ( 'NONE', #33309 ) ;
#99188 = ORIENTED_EDGE ( 'NONE', *, *, #135517, .T. ) ;
#99189 = VECTOR ( 'NONE', #40146, 1000.000000000000000 ) ;
#99190 = EDGE_CURVE ( 'NONE', #56507, #1974, #119518, .T. ) ;
#99191 = COLOUR_RGB ( '', 0.31764706, 0.68627451, 0.89019608) ;
#99192 = CARTESIAN_POINT ( 'NONE',  ( 14.99999999999989519, 7.559798855135672291, 4.979909187984731922 ) ) ;
#99193 = EDGE_LOOP ( 'NONE', ( #134584, #103945, #61049, #39767 ) ) ;
#99194 = LINE ( 'NONE', #53596, #138642 ) ;
#99195 = CARTESIAN_POINT ( 'NONE',  ( -34.42499999999997584, -21.76999999999999247, -0.5000000000000000000 ) ) ;
#99196 = FACE_OUTER_BOUND ( 'NONE', #16887, .T. ) ;
#99197 = DIRECTION ( 'NONE',  ( 0.000000000000000000, 0.000000000000000000, 1.000000000000000000 ) ) ;
#99198 = CARTESIAN_POINT ( 'NONE',  ( 119.4166666666666714, -6.884901960086287076, -3.975000000000000977 ) ) ;
#99199 = VERTEX_POINT ( 'NONE', #22349 ) ;
#99200 = VECTOR ( 'NONE', #109998, 1000.000000000000000 ) ;
#99201 = DIRECTION ( 'NONE',  ( 0.000000000000000000, -1.000000000000000000, 0.000000000000000000 ) ) ;
#99202 = VECTOR ( 'NONE', #115247, 1000.000000000000000 ) ;
#99203 = EDGE_LOOP ( 'NONE', ( #92039, #71238, #60081, #107647, #27980, #25795 ) ) ;
#99204 = CARTESIAN_POINT ( 'NONE',  ( -7.499999999999940492, -2.947814304570798960, 5.000000000000000000 ) ) ;
#99205 = ORIENTED_EDGE ( 'NONE', *, *, #10608, .T. ) ;
#99206 = CARTESIAN_POINT ( 'NONE',  ( 115.4333603837962130, 2.130196079827431532, -7.949999999999996625 ) ) ;
#99207 = ORIENTED_EDGE ( 'NONE', *, *, #59788, .F. ) ;
#99208 = LINE ( 'NONE', #142059, #48204 ) ;
#99209 = VERTEX_POINT ( 'NONE', #75354 ) ;
#99210 = ORIENTED_EDGE ( 'NONE', *, *, #117429, .T. ) ;
#99211 = CIRCLE ( 'NONE', #36734, 2.500000000000000888 ) ;
#99212 = ORIENTED_EDGE ( 'NONE', *, *, #129977, .T. ) ;
#99213 = VECTOR ( 'NONE', #45617, 1000.000000000000227 ) ;
#99214 = LINE ( 'NONE', #110103, #102136 ) ;
#99215 = DIRECTION ( 'NONE',  ( 0.6830127018922180770, -0.6830127018922204085, -0.2588190451025213501 ) ) ;
#99216 = DIRECTION ( 'NONE',  ( -0.7071067811865486830, 0.7071067811865464625, 0.000000000000000000 ) ) ;
#99217 = CARTESIAN_POINT ( 'NONE',  ( 123.3754301918981184, -5.291415217122920289, -3.055000000000001492 ) ) ;
#99218 = DIRECTION ( 'NONE',  ( 0.6830127018922180770, -0.6830127018922204085, -0.2588190451025213501 ) ) ;
#99219 = ADVANCED_FACE ( 'NONE', ( #20215 ), #110788, .T. ) ;
#99220 = FACE_OUTER_BOUND ( 'NONE', #30572, .T. ) ;
#99222 = DIRECTION ( 'NONE',  ( -0.000000000000000000, 1.000000000000000000, -0.000000000000000000 ) ) ;
#99221 = LINE ( 'NONE', #132637, #6264 ) ;
#99223 = AXIS2_PLACEMENT_3D ( 'NONE', #19233, #77216, #63489 ) ;
#99224 = LINE ( 'NONE', #45623, #104901 ) ;
#99225 = CARTESIAN_POINT ( 'NONE',  ( 54.48921356237310221, -27.52281430457093236, 5.000000000000000000 ) ) ;
#99226 = CARTESIAN_POINT ( 'NONE',  ( 32.99999999999977973, 11.96639925780213787, 5.000000000000000000 ) ) ;
#99227 = DIRECTION ( 'NONE',  ( 0.7071067811865487940, 0.7071067811865463515, 0.000000000000000000 ) ) ;
#99228 = EDGE_LOOP ( 'NONE', ( #109917, #39842, #64983, #113605 ) ) ;
#99229 = ORIENTED_EDGE ( 'NONE', *, *, #11265, .F. ) ;
#99230 = ORIENTED_EDGE ( 'NONE', *, *, #116855, .F. ) ;
#99231 = CARTESIAN_POINT ( 'NONE',  ( -36.48921356237310221, -27.52281430457080802, 5.000000000000000000 ) ) ;
#99232 = VERTEX_POINT ( 'NONE', #120972 ) ;
#99234 = VERTEX_POINT ( 'NONE', #31834 ) ;
#99233 = EDGE_CURVE ( 'NONE', #3063, #121049, #10068, .T. ) ;
#99235 = CYLINDRICAL_SURFACE ( 'NONE', #56107, 2.500000000000000444 ) ;
#99236 = CARTESIAN_POINT ( 'NONE',  ( 107.1208603837962272, -6.884901960086286188, 3.974999999999997424 ) ) ;
#99237 = ADVANCED_FACE ( 'NONE', ( #121674 ), #44409, .T. ) ;
#99238 = DIRECTION ( 'NONE',  ( 0.7071067811865486830, -0.7071067811865464625, -0.000000000000000000 ) ) ;
#99239 = LINE ( 'NONE', #20984, #99580 ) ;
#99240 = ORIENTED_EDGE ( 'NONE', *, *, #99636, .F. ) ;
#99241 = CARTESIAN_POINT ( 'NONE',  ( 36.18398860626899705, 28.73617430169812437, 5.000000000000000000 ) ) ;
#99242 = ORIENTED_EDGE ( 'NONE', *, *, #137486, .T. ) ;
#99244 = EDGE_CURVE ( 'NONE', #46491, #94937, #141920, .T. ) ;
#99243 = DIRECTION ( 'NONE',  ( -0.7071067811865486830, 0.7071067811865464625, 0.000000000000000000 ) ) ;
#99245 = EDGE_CURVE ( 'NONE', #141085, #58174, #613, .T. ) ;
#99246 = CARTESIAN_POINT ( 'NONE',  ( 15.23373647476855375, 5.808823158059036373, 5.808823158059032821 ) ) ;
#99247 = EDGE_LOOP ( 'NONE', ( #79839, #104298, #97251, #74927 ) ) ;
#99248 = CARTESIAN_POINT ( 'NONE',  ( 81.57876352523143737, -7.482591942790327058E-16, 6.109999999999999432 ) ) ;
#99249 = CARTESIAN_POINT ( 'NONE',  ( -14.70025512860841133, -27.71228299555195917, 4.000000000000000000 ) ) ;
#99250 = ADVANCED_FACE ( 'NONE', ( #68083 ), #135452, .F. ) ;
#99251 = DIRECTION ( 'NONE',  ( -0.7071067811865487940, 0.7071067811865463515, 0.000000000000000000 ) ) ;
#99252 = ORIENTED_EDGE ( 'NONE', *, *, #34013, .T. ) ;
#99253 = EDGE_LOOP ( 'NONE', ( #57223, #48747, #137642, #52314, #119945, #126096, #54507, #79211 ) ) ;
#99254 = ORIENTED_EDGE ( 'NONE', *, *, #129635, .F. ) ;
#99255 = CARTESIAN_POINT ( 'NONE',  ( -28.82816939922332722, 6.759292476615653023, 4.000000000000000000 ) ) ;
#99256 = LINE ( 'NONE', #111592, #127338 ) ;
#99257 = CARTESIAN_POINT ( 'NONE',  ( -5.994519915287488843, 28.92564299267942118, 4.000000000000000000 ) ) ;
#99258 = CARTESIAN_POINT ( 'NONE',  ( -15.77004279457781877, 21.73644205237996729, 5.000000000000000888 ) ) ;
#99259 = DIRECTION ( 'NONE',  ( -0.7071067811865486830, -0.7071067811865464625, 0.000000000000000000 ) ) ;
#99260 = ORIENTED_EDGE ( 'NONE', *, *, #114098, .F. ) ;
#99261 = LINE ( 'NONE', #40648, #18328 ) ;
#99262 = EDGE_CURVE ( 'NONE', #467, #54775, #136852, .T. ) ;
#99263 = VECTOR ( 'NONE', #8665, 1000.000000000000000 ) ;
#99264 = FILL_AREA_STYLE_COLOUR ( '', #85943 ) ;
#99265 = DIRECTION ( 'NONE',  ( 0.7071067811865487940, -0.7071067811865463515, 0.000000000000000000 ) ) ;
#99266 = EDGE_LOOP ( 'NONE', ( #76178, #21496, #49881, #34807 ) ) ;
#99267 = EDGE_CURVE ( 'NONE', #12409, #50067, #114385, .T. ) ;
#99268 = CARTESIAN_POINT ( 'NONE',  ( -34.60428828362105236, 22.19175015946030882, 4.000000000000000000 ) ) ;
#99270 = ADVANCED_FACE ( 'NONE', ( #103487 ), #2764, .T. ) ;
#99269 = AXIS2_PLACEMENT_3D ( 'NONE', #132978, #132263, #114563 ) ;
#99271 = VECTOR ( 'NONE', #70102, 999.9999999999998863 ) ;
#99272 = AXIS2_PLACEMENT_3D ( 'NONE', #113836, #14533, #58812 ) ;
#99273 = CARTESIAN_POINT ( 'NONE',  ( 6.489213562373093325, -27.52281430457059841, 5.000000000000000000 ) ) ;
#99274 = ORIENTED_EDGE ( 'NONE', *, *, #38769, .T. ) ;
#99275 = VECTOR ( 'NONE', #6453, 1000.000000000000000 ) ;
#99277 = ORIENTED_EDGE ( 'NONE', *, *, #24860, .T. ) ;
#99276 = DIRECTION ( 'NONE',  ( 0.3543493200069162685, -0.000000000000000000, -0.9351131265310288487 ) ) ;
#99278 = ORIENTED_EDGE ( 'NONE', *, *, #110454, .F. ) ;
#99279 = CARTESIAN_POINT ( 'NONE',  ( 8.673617379884035472E-15, 2.587461875839212944, 4.000000000000000000 ) ) ;
#99280 = CARTESIAN_POINT ( 'NONE',  ( 69.18398860626899705, 28.73617430169835529, 5.000000000000000000 ) ) ;
#99281 = ADVANCED_FACE ( 'NONE', ( #125271 ), #59334, .F. ) ;
#99282 = ORIENTED_EDGE ( 'NONE', *, *, #59991, .F. ) ;
#99283 = LINE ( 'NONE', #85564, #62791 ) ;
#99284 = STYLED_ITEM ( 'NONE', ( #16005 ), #139143 ) ;
#99285 =( BOUNDED_CURVE ( )  B_SPLINE_CURVE ( 3, ( #27692, #103803, #4449, #48756 ),
 .UNSPECIFIED., .F., .T. ) 
 B_SPLINE_CURVE_WITH_KNOTS ( ( 4, 4 ),
 ( 3.858351980207623821, 3.926990816987242727 ),
 .UNSPECIFIED. ) 
 CURVE ( )  GEOMETRIC_REPRESENTATION_ITEM ( )  RATIONAL_B_SPLINE_CURVE ( ( 1.000000000000000000, 0.9996074310407763175, 0.9996074310407763175, 1.000000000000000000 ) ) 
 REPRESENTATION_ITEM ( '' )  );
#99286 = FACE_OUTER_BOUND ( 'NONE', #47289, .T. ) ;
#99287 = SURFACE_STYLE_FILL_AREA ( #110171 ) ;
#99288 = LINE ( 'NONE', #143534, #23038 ) ;
#99289 = DIRECTION ( 'NONE',  ( -0.3543493200069162685, -0.000000000000000000, -0.9351131265310288487 ) ) ;
#99290 = LINE ( 'NONE', #47149, #67725 ) ;
#99292 = ADVANCED_FACE ( 'NONE', ( #91916 ), #57906, .F. ) ;
#99291 = DIRECTION ( 'NONE',  ( -0.3543493200069162685, -0.000000000000000000, -0.9351131265310288487 ) ) ;
#99293 =( LENGTH_UNIT ( ) NAMED_UNIT ( * ) SI_UNIT ( .MILLI., .METRE. ) );
#99294 = PLANE ( 'NONE',  #50284 ) ;
#99296 = AXIS2_PLACEMENT_3D ( 'NONE', #101442, #123230, #34073 ) ;
#99295 = LINE ( 'NONE', #63862, #32969 ) ;
#99297 = DIRECTION ( 'NONE',  ( -1.000000000000000000, -1.224606353822377258E-16, -0.000000000000000000 ) ) ;
#99298 = CARTESIAN_POINT ( 'NONE',  ( 13.49999999999991118, 10.08746187583914278, 4.000000000000000000 ) ) ;
#99299 = CARTESIAN_POINT ( 'NONE',  ( -23.57322811595262735, -0.7198850472490149199, 4.205258209906618028 ) ) ;
#99300 = ORIENTED_EDGE ( 'NONE', *, *, #82795, .T. ) ;
#99301 = ORIENTED_EDGE ( 'NONE', *, *, #136683, .T. ) ;
#99302 = ADVANCED_FACE ( 'NONE', ( #48416 ), #136136, .F. ) ;
#99303 = CARTESIAN_POINT ( 'NONE',  ( 103.0833333333333286, 6.884901960086290629, -3.974999999999994316 ) ) ;
#99304 = VERTEX_POINT ( 'NONE', #35446 ) ;
#99305 = EDGE_LOOP ( 'NONE', ( #69986, #132127, #55755, #75841 ) ) ;
#99306 = EDGE_CURVE ( 'NONE', #55371, #39920, #102816, .T. ) ;
#99307 = VERTEX_POINT ( 'NONE', #45601 ) ;
#99308 = CARTESIAN_POINT ( 'NONE',  ( 9.208651418775088970, 4.584330080086930965E-16, 0.000000000000000000 ) ) ;
#99309 = LINE ( 'NONE', #10865, #48734 ) ;
#99310 = ORIENTED_EDGE ( 'NONE', *, *, #101057, .T. ) ;
#99311 = VECTOR ( 'NONE', #58414, 999.9999999999998863 ) ;
#99312 = CARTESIAN_POINT ( 'NONE',  ( 3.872664058232598183, 3.821174125832445049E-16, 0.000000000000000000 ) ) ;
#99314 = EDGE_CURVE ( 'NONE', #123801, #2587, #102100, .T. ) ;
#99313 = VECTOR ( 'NONE', #92346, 999.9999999999998863 ) ;
#99315 = CARTESIAN_POINT ( 'NONE',  ( -28.17183060077627133, 0.7592924766157034266, 4.000000000000000000 ) ) ;
#99316 = VECTOR ( 'NONE', #117975, 1000.000000000000000 ) ;
#99317 = FACE_OUTER_BOUND ( 'NONE', #8777, .T. ) ;
#99318 = LINE ( 'NONE', #120337, #60499 ) ;
#99319 = VERTEX_POINT ( 'NONE', #36821 ) ;
#99320 = DIRECTION ( 'NONE',  ( -0.6830127018922180770, -0.6830127018922204085, -0.2588190451025213501 ) ) ;
#99321 = CARTESIAN_POINT ( 'NONE',  ( -34.92500000000001137, 22.22500000000000142, 4.500000000000000888 ) ) ;
#99322 = DIRECTION ( 'NONE',  ( 0.7071067811865486830, -0.7071067811865464625, -0.000000000000000000 ) ) ;
#99323 = VECTOR ( 'NONE', #23733, 1000.000000000000000 ) ;
#99324 = DIRECTION ( 'NONE',  ( 0.000000000000000000, 1.000000000000000000, 0.000000000000000000 ) ) ;
#99325 = DIRECTION ( 'NONE',  ( -0.7071067811865486830, -0.7071067811865464625, 0.000000000000000000 ) ) ;
#99326 = CARTESIAN_POINT ( 'NONE',  ( 14.99999999999989697, -12.41253812416062985, 4.000000000000000000 ) ) ;
#99327 = CIRCLE ( 'NONE', #36835, 9.119999999999999218 ) ;
#99328 = LINE ( 'NONE', #22475, #24400 ) ;
#99329 = FACE_OUTER_BOUND ( 'NONE', #110306, .T. ) ;
#99330 = ORIENTED_EDGE ( 'NONE', *, *, #24406, .T. ) ;
#99331 = VERTEX_POINT ( 'NONE', #70228 ) ;
#99332 = CARTESIAN_POINT ( 'NONE',  ( 123.8129301918981184, -1.637169565754159617, -6.110000000000001208 ) ) ;
#99333 = ORIENTED_EDGE ( 'NONE', *, *, #113497, .F. ) ;
#99334 = EDGE_CURVE ( 'NONE', #130484, #112167, #120825, .T. ) ;
#99335 = DIRECTION ( 'NONE',  ( -0.7071067811865486830, -0.7071067811865464625, 0.000000000000000000 ) ) ;
#99336 = CARTESIAN_POINT ( 'NONE',  ( 7.499999999999951150, -5.568876922607754132, 4.000000000000000000 ) ) ;
#99337 = AXIS2_PLACEMENT_3D ( 'NONE', #19767, #64004, #119770 ) ;
#99338 = CARTESIAN_POINT ( 'NONE',  ( -22.49999999999984723, 14.14708470758589165, -0.5283514160166046247 ) ) ;
#99339 = EDGE_CURVE ( 'NONE', #128576, #102869, #81797, .T. ) ;
#99340 = DIRECTION ( 'NONE',  ( 0.7071067811865487940, 0.7071067811865463515, -0.000000000000000000 ) ) ;
#99341 = DIRECTION ( 'NONE',  ( 0.000000000000000000, -1.000000000000000000, 0.000000000000000000 ) ) ;
#99342 = CARTESIAN_POINT ( 'NONE',  ( 111.0370968585647944, -3.054999999999998828, -5.291415217122919401 ) ) ;
#99343 = EDGE_LOOP ( 'NONE', ( #17338, #601, #130770, #63823 ) ) ;
#99344 = ORIENTED_EDGE ( 'NONE', *, *, #109856, .F. ) ;
#99345 = DIRECTION ( 'NONE',  ( -0.6830127018922181881, 0.6830127018922202975, -0.2588190451025214056 ) ) ;
#99346 = VERTEX_POINT ( 'NONE', #13624 ) ;
#99347 = ORIENTED_EDGE ( 'NONE', *, *, #114521, .T. ) ;
#99348 = CARTESIAN_POINT ( 'NONE',  ( 38.20876352523143282, -7.482591942790329030E-16, 6.110000000000001208 ) ) ;
#99349 = ORIENTED_EDGE ( 'NONE', *, *, #120829, .T. ) ;
#99350 = CARTESIAN_POINT ( 'NONE',  ( -12.69999999999998153, 3.061616997868383634E-16, -2.500000000000000444 ) ) ;
#99351 = EDGE_CURVE ( 'NONE', #29293, #126178, #25228, .T. ) ;
#99352 = LINE ( 'NONE', #121823, #57144 ) ;
#99353 = CARTESIAN_POINT ( 'NONE',  ( -1.499999999999990896, 3.653845994658386331, -4.504631822206368597 ) ) ;
#99354 = ADVANCED_FACE ( 'NONE', ( #69485 ), #26666, .F. ) ;
#99355 = CARTESIAN_POINT ( 'NONE',  ( 32.43293019189810877, 1.637169565754156508, 6.110000000000000320 ) ) ;
#99356 = ORIENTED_EDGE ( 'NONE', *, *, #101420, .T. ) ;
#99357 = DIRECTION ( 'NONE',  ( 0.3543493200069162685, -0.000000000000000000, -0.9351131265310288487 ) ) ;
#99358 = ORIENTED_EDGE ( 'NONE', *, *, #126387, .T. ) ;
#99359 = EDGE_LOOP ( 'NONE', ( #100927, #53433, #53096, #22555 ) ) ;
#99360 = ORIENTED_EDGE ( 'NONE', *, *, #139986, .T. ) ;
#99361 = EDGE_CURVE ( 'NONE', #5013, #10004, #70911, .T. ) ;
#99362 = DIRECTION ( 'NONE',  ( -0.000000000000000000, -0.3543493200069152693, 0.9351131265310292928 ) ) ;
#99363 = ORIENTED_EDGE ( 'NONE', *, *, #52631, .T. ) ;
#99364 = DIRECTION ( 'NONE',  ( -0.3543493200069162685, -0.000000000000000000, -0.9351131265310288487 ) ) ;
#99365 = DIRECTION ( 'NONE',  ( 0.7071067811865486830, -0.7071067811865464625, -0.000000000000000000 ) ) ;
#99366 = PRESENTATION_STYLE_ASSIGNMENT (( #44336 ) ) ;
#99367 = VECTOR ( 'NONE', #58314, 1000.000000000000000 ) ;
#99368 = AXIS2_PLACEMENT_3D ( 'NONE', #12636, #68493, #110505 ) ;
#99369 = AXIS2_PLACEMENT_3D ( 'NONE', #58418, #26452, #15526 ) ;
#99370 = DIRECTION ( 'NONE',  ( -0.7071067811865486830, -0.7071067811865464625, 0.000000000000000000 ) ) ;
#99371 = AXIS2_PLACEMENT_3D ( 'NONE', #56325, #64297, #54865 ) ;
#99372 = FACE_BOUND ( 'NONE', #93050, .T. ) ;
#99373 = EDGE_LOOP ( 'NONE', ( #138801, #24348, #123354, #73818 ) ) ;
#99374 = DIRECTION ( 'NONE',  ( 0.6830127018922181881, 0.6830127018922202975, -0.2588190451025214056 ) ) ;
#99375 = LINE ( 'NONE', #89940, #39819 ) ;
#99376 = FACE_OUTER_BOUND ( 'NONE', #35745, .T. ) ;
#99377 = ORIENTED_EDGE ( 'NONE', *, *, #15984, .T. ) ;
#99378 = DIRECTION ( 'NONE',  ( 0.7071067811865487940, 0.7071067811865463515, 0.000000000000000000 ) ) ;
#99379 = ORIENTED_EDGE ( 'NONE', *, *, #34720, .T. ) ;
#99380 = ORIENTED_EDGE ( 'NONE', *, *, #2570, .T. ) ;
#99381 = VECTOR ( 'NONE', #86857, 1000.000000000000000 ) ;
#99382 = SURFACE_STYLE_USAGE ( .BOTH. , #88563 ) ;
#99383 = ORIENTED_EDGE ( 'NONE', *, *, #38108, .T. ) ;
#99384 = CARTESIAN_POINT ( 'NONE',  ( 44.68293019189811588, -1.637169565754158951, -6.109999999999998543 ) ) ;
#99385 = ORIENTED_EDGE ( 'NONE', *, *, #44063, .T. ) ;
#99386 = DIRECTION ( 'NONE',  ( -0.7071067811865486830, 0.7071067811865464625, 0.000000000000000000 ) ) ;
#99387 = CARTESIAN_POINT ( 'NONE',  ( -34.92500000000001137, 22.22500000000000142, 4.000000000000000000 ) ) ;
#99388 = DIRECTION ( 'NONE',  ( -0.6830127018922180770, -0.6830127018922204085, -0.2588190451025213501 ) ) ;
#99389 = ORIENTED_EDGE ( 'NONE', *, *, #119947, .T. ) ;
#99390 = DIRECTION ( 'NONE',  ( -0.7071067811865487940, 0.7071067811865463515, 0.000000000000000000 ) ) ;
#99391 = DIRECTION ( 'NONE',  ( -0.7071067811865487940, 0.7071067811865463515, -0.000000000000000000 ) ) ;
#99392 = AXIS2_PLACEMENT_3D ( 'NONE', #90402, #46221, #79588 ) ;
#99393 = VECTOR ( 'NONE', #1710, 1000.000000000000000 ) ;
#99394 = AXIS2_PLACEMENT_3D ( 'NONE', #109687, #10355, #63369 ) ;
#99395 = DIRECTION ( 'NONE',  ( 0.000000000000000000, -1.000000000000000000, 0.000000000000000000 ) ) ;
#99396 = LINE ( 'NONE', #113137, #39341 ) ;
#99397 = CARTESIAN_POINT ( 'NONE',  ( 20.97999999999999687, 2.055000000000001492, 2.516649172247811554E-16 ) ) ;
#99398 = CARTESIAN_POINT ( 'NONE',  ( -27.32816939922333432, 5.259292476615663681, 4.000000000000000000 ) ) ;
#99399 = DIRECTION ( 'NONE',  ( -0.000000000000000000, 0.000000000000000000, 1.000000000000000000 ) ) ;
#99400 = EDGE_LOOP ( 'NONE', ( #65623, #30581, #13830, #119453 ) ) ;
#99401 = EDGE_CURVE ( 'NONE', #6180, #61952, #134011, .T. ) ;
#99402 = ORIENTED_EDGE ( 'NONE', *, *, #93774, .T. ) ;
#99403 = ORIENTED_EDGE ( 'NONE', *, *, #115652, .T. ) ;
#99404 = AXIS2_PLACEMENT_3D ( 'NONE', #77811, #22663, #66933 ) ;
#99405 = CARTESIAN_POINT ( 'NONE',  ( 30.29974487139158867, -27.71228299555227537, 4.000000000000000000 ) ) ;
#99406 = DIRECTION ( 'NONE',  ( -0.000000000000000000, 0.3543493200069153248, 0.9351131265310292928 ) ) ;
#99407 = ORIENTED_EDGE ( 'NONE', *, *, #42565, .F. ) ;
#99408 = VECTOR ( 'NONE', #7482, 999.9999999999998863 ) ;
#99409 = VECTOR ( 'NONE', #133393, 1000.000000000000000 ) ;
#99410 = VERTEX_POINT ( 'NONE', #2009 ) ;
#99411 =( NAMED_UNIT ( * ) PLANE_ANGLE_UNIT ( ) SI_UNIT ( $, .RADIAN. ) );
#99412 = CARTESIAN_POINT ( 'NONE',  ( -24.48921356237309510, -27.52281430457072631, 5.000000000000000000 ) ) ;
#99413 = EDGE_CURVE ( 'NONE', #66330, #23113, #90508, .T. ) ;
#99414 = ADVANCED_FACE ( 'NONE', ( #39712 ), #83194, .T. ) ;
#99415 = DIRECTION ( 'NONE',  ( -0.7071067811865486830, -0.7071067811865464625, -0.000000000000000000 ) ) ;
#99416 = VERTEX_POINT ( 'NONE', #84625 ) ;
#99417 = AXIS2_PLACEMENT_3D ( 'NONE', #134315, #87937, #32875 ) ;
#99418 = CARTESIAN_POINT ( 'NONE',  ( -8.331532588401378447, -18.74070752338409207, 20.73178291233839232 ) ) ;
#99420 = EDGE_CURVE ( 'NONE', #103007, #22844, #127396, .T. ) ;
#99419 = CARTESIAN_POINT ( 'NONE',  ( 5.994519915287488843, 28.92564299267942118, 4.000000000000000000 ) ) ;
#99421 = EDGE_CURVE ( 'NONE', #126872, #62368, #71610, .T. ) ;
#99422 = CARTESIAN_POINT ( 'NONE',  ( 30.83790314143522338, -6.871911579029513106, -3.967499999999993587 ) ) ;
#99423 = DIRECTION ( 'NONE',  ( 0.7071067811865487940, 0.7071067811865463515, 0.000000000000000000 ) ) ;
#99424 = EDGE_CURVE ( 'NONE', #9261, #67480, #96178, .T. ) ;
#99425 = VERTEX_POINT ( 'NONE', #72363 ) ;
#99426 = CARTESIAN_POINT ( 'NONE',  ( 112.6412635252314658, 4.472830434245837594, 4.472830434245841147 ) ) ;
#99427 = EDGE_CURVE ( 'NONE', #139966, #31468, #62167, .T. ) ;
#99428 = LINE ( 'NONE', #85706, #32679 ) ;
#99429 = CARTESIAN_POINT ( 'NONE',  ( 31.82816939922331656, -20.24070752338406720, 4.000000000000000000 ) ) ;
#99430 = VECTOR ( 'NONE', #114805, 1000.000000000000000 ) ;
#99432 = EDGE_LOOP ( 'NONE', ( #96136, #18481 ) ) ;
#99431 = CARTESIAN_POINT ( 'NONE',  ( 7.499999999999951150, 3.073033219394630144, -6.593910359670951848 ) ) ;
#99433 = CARTESIAN_POINT ( 'NONE',  ( 0.000000000000000000, 60.00000000000000000, -4.000000000000000000 ) ) ;
#99434 = ORIENTED_EDGE ( 'NONE', *, *, #88489, .T. ) ;
#99435 = EDGE_CURVE ( 'NONE', #123251, #127158, #139744, .T. ) ;
#99436 = CARTESIAN_POINT ( 'NONE',  ( -34.92500000000001137, -20.33753812416080820, 4.000000000000000000 ) ) ;
#99437 = LINE ( 'NONE', #43654, #30794 ) ;
#99438 = CARTESIAN_POINT ( 'NONE',  ( 120.5833333333333286, 6.884901960086290629, -3.974999999999994316 ) ) ;
#99439 = ORIENTED_EDGE ( 'NONE', *, *, #58131, .T. ) ;
#99440 = EDGE_CURVE ( 'NONE', #32541, #105769, #137579, .T. ) ;
#99441 = CARTESIAN_POINT ( 'NONE',  ( -44.99451991528749772, 28.92564299267969474, 4.000000000000000000 ) ) ;
#99442 = CARTESIAN_POINT ( 'NONE',  ( 16.44013779566152778, 3.821174125832445049E-16, 0.000000000000000000 ) ) ;
#99443 = VERTEX_POINT ( 'NONE', #107075 ) ;
#99444 = CARTESIAN_POINT ( 'NONE',  ( 15.18398860626900237, 28.73617430169797871, 5.000000000000000000 ) ) ;
#99445 = CARTESIAN_POINT ( 'NONE',  ( 36.48921356237310221, -27.52281430457080802, 5.000000000000000000 ) ) ;
#99446 = ORIENTED_EDGE ( 'NONE', *, *, #142523, .F. ) ;
#99447 = ADVANCED_FACE ( 'NONE', ( #7005 ), #4861, .F. ) ;
#99448 = DIRECTION ( 'NONE',  ( -0.7071067811865486830, -0.7071067811865464625, 0.000000000000000000 ) ) ;
#99450 = ORIENTED_EDGE ( 'NONE', *, *, #8329, .F. ) ;
#99449 = CARTESIAN_POINT ( 'NONE',  ( -9.005480084712511157, 28.92564299267931816, 4.000000000000000000 ) ) ;
#99451 = ORIENTED_EDGE ( 'NONE', *, *, #3784, .T. ) ;
#99452 = CARTESIAN_POINT ( 'NONE',  ( 8.603643696575190347, 12.00528567777757694, -25.64165571474893568 ) ) ;
#99453 = CARTESIAN_POINT ( 'NONE',  ( 32.99999999999977263, -2.904428200921273184, -6.989807076075017278 ) ) ;
#99454 = EDGE_CURVE ( 'NONE', #75066, #139700, #97791, .T. ) ;
#99455 = ORIENTED_EDGE ( 'NONE', *, *, #59423, .F. ) ;
#99456 = DIRECTION ( 'NONE',  ( 0.7071067811865487940, 0.7071067811865463515, -0.000000000000000000 ) ) ;
#99457 = CARTESIAN_POINT ( 'NONE',  ( 30.18398860626900060, 28.73617430169808173, 5.000000000000000000 ) ) ;
#99458 = CARTESIAN_POINT ( 'NONE',  ( 27.61838490601979146, -2.240707523384260824, 13.37739548510232979 ) ) ;
#99459 = ORIENTED_EDGE ( 'NONE', *, *, #46468, .F. ) ;
#99460 = FACE_OUTER_BOUND ( 'NONE', #8186, .T. ) ;
#99461 = DIRECTION ( 'NONE',  ( 0.7071067811865487940, 0.7071067811865463515, -0.000000000000000000 ) ) ;
#99462 = DIRECTION ( 'NONE',  ( -0.7071067811865486830, -0.7071067811865464625, 0.000000000000000000 ) ) ;
#99463 = SURFACE_STYLE_USAGE ( .BOTH. , #54581 ) ;
#99464 = CARTESIAN_POINT ( 'NONE',  ( 27.03709685856478373, -3.054999999999999272, -5.291415217122919401 ) ) ;
#99465 = CARTESIAN_POINT ( 'NONE',  ( -60.29974487139158867, -27.71228299555248142, 4.000000000000000000 ) ) ;
#99466 = VERTEX_POINT ( 'NONE', #6284 ) ;
#99467 = ORIENTED_EDGE ( 'NONE', *, *, #108237, .F. ) ;
#99468 = EDGE_CURVE ( 'NONE', #109300, #134825, #117917, .T. ) ;
#99469 = CARTESIAN_POINT ( 'NONE',  ( 9.183988606268997046, 28.73617430169793607, 5.000000000000000000 ) ) ;
#99470 = ORIENTED_EDGE ( 'NONE', *, *, #5232, .T. ) ;
#99471 = EDGE_CURVE ( 'NONE', #20421, #871, #60774, .T. ) ;
#99472 = EDGE_LOOP ( 'NONE', ( #130728, #121751, #81526, #26176 ) ) ;
#99473 = DIRECTION ( 'NONE',  ( -0.000000000000000000, -0.000000000000000000, 1.000000000000000000 ) ) ;
#99474 = DIRECTION ( 'NONE',  ( 1.000000000000000000, 0.000000000000000000, 0.000000000000000000 ) ) ;
#99475 = AXIS2_PLACEMENT_3D ( 'NONE', #56368, #89654, #133883 ) ;
#99476 = VECTOR ( 'NONE', #128277, 1000.000000000000000 ) ;
#99477 = ORIENTED_EDGE ( 'NONE', *, *, #17637, .T. ) ;
#99478 = EDGE_CURVE ( 'NONE', #98566, #105535, #16476, .T. ) ;
#99479 = FACE_OUTER_BOUND ( 'NONE', #137062, .T. ) ;
#99480 = CARTESIAN_POINT ( 'NONE',  ( -14.99999999999988809, 17.96639925780207747, 5.000000000000000000 ) ) ;
#99481 = VECTOR ( 'NONE', #117578, 1000.000000000000000 ) ;
#99482 = DIRECTION ( 'NONE',  ( 0.7071067811865487940, 0.7071067811865463515, 0.000000000000000000 ) ) ;
#99483 = DIRECTION ( 'NONE',  ( -0.7071067811865486830, -0.7071067811865464625, -0.000000000000000000 ) ) ;
#99484 = CARTESIAN_POINT ( 'NONE',  ( 118.1254301918981184, 5.291415217122919401, 3.055000000000002824 ) ) ;
#99485 = VERTEX_POINT ( 'NONE', #49869 ) ;
#99486 = CARTESIAN_POINT ( 'NONE',  ( -30.48921356237309510, -27.52281430457076894, 5.000000000000000000 ) ) ;
#99487 = CARTESIAN_POINT ( 'NONE',  ( 10.49999999999993250, 1.030536316426522436, -5.498701923753822385 ) ) ;
#99488 = VECTOR ( 'NONE', #32312, 1000.000000000000000 ) ;
#99489 =( LENGTH_UNIT ( ) NAMED_UNIT ( * ) SI_UNIT ( .MILLI., .METRE. ) );
#99490 = CARTESIAN_POINT ( 'NONE',  ( -25.39999999999996305, 0.000000000000000000, 0.000000000000000000 ) ) ;
#99491 = CARTESIAN_POINT ( 'NONE',  ( 0.4644480930543400943, -0.3999999999999997446, -2.317232462839659224 ) ) ;
#99492 = DIRECTION ( 'NONE',  ( -0.000000000000000000, 0.000000000000000000, 1.000000000000000000 ) ) ;
#99493 = CARTESIAN_POINT ( 'NONE',  ( 56.80836038379622721, 7.949999999999997513, 2.130196079827431088 ) ) ;
#99494 = CARTESIAN_POINT ( 'NONE',  ( -33.29974487139158867, -27.71228299555229313, 4.000000000000000000 ) ) ;
#99495 = CARTESIAN_POINT ( 'NONE',  ( 9.299744871391588674, -27.71228299555212971, 4.000000000000000000 ) ) ;
#99496 = AXIS2_PLACEMENT_3D ( 'NONE', #98054, #76307, #42974 ) ;
#99497 = ORIENTED_EDGE ( 'NONE', *, *, #59788, .T. ) ;
#99498 = VERTEX_POINT ( 'NONE', #73061 ) ;
#99499 = CARTESIAN_POINT ( 'NONE',  ( 45.33333333333332149, -6.884901960086287964, 3.974999999999998312 ) ) ;
#99500 = ADVANCED_FACE ( 'NONE', ( #83941 ), #128141, .F. ) ;
#99501 = CARTESIAN_POINT ( 'NONE',  ( -16.49999999999988276, 13.08746187583911436, 4.000000000000000000 ) ) ;
#99502 = VECTOR ( 'NONE', #49450, 1000.000000000000000 ) ;
#99503 = AXIS2_PLACEMENT_3D ( 'NONE', #89941, #33475, #77675 ) ;
#99504 = CARTESIAN_POINT ( 'NONE',  ( 7.014532492589830248, 2.500000000000000444, 3.061616997868383634E-16 ) ) ;
#99505 = VERTEX_POINT ( 'NONE', #131700 ) ;
#99506 = CARTESIAN_POINT ( 'NONE',  ( 41.99451991528749062, 28.92564299267967343, 4.000000000000000000 ) ) ;
#99507 = VECTOR ( 'NONE', #88141, 999.9999999999998863 ) ;
#99508 = CARTESIAN_POINT ( 'NONE',  ( 35.72959685856475431, -6.110000000000000320, -1.637169565754161393 ) ) ;
#99509 = EDGE_CURVE ( 'NONE', #138069, #19604, #23667, .T. ) ;
#99510 = EDGE_LOOP ( 'NONE', ( #76062, #126488, #50456, #143430 ) ) ;
#99511 = CARTESIAN_POINT ( 'NONE',  ( -27.18398860626900060, 28.73617430169806042, 5.000000000000000000 ) ) ;
#99512 = ORIENTED_EDGE ( 'NONE', *, *, #49810, .T. ) ;
#99513 = VERTEX_POINT ( 'NONE', #41829 ) ;
#99514 = PLANE ( 'NONE',  #132878 ) ;
#99515 = AXIS2_PLACEMENT_3D ( 'NONE', #114156, #101855, #69992 ) ;
#99516 = AXIS2_PLACEMENT_3D ( 'NONE', #1423, #134127, #36241 ) ;
#99517 = DIRECTION ( 'NONE',  ( -0.7071067811865486830, -0.7071067811865464625, 0.000000000000000000 ) ) ;
#99518 = LINE ( 'NONE', #10373, #32789 ) ;
#99519 = CARTESIAN_POINT ( 'NONE',  ( -15.18398860626900237, 28.73617430169797871, 5.000000000000000000 ) ) ;
#99520 = VERTEX_POINT ( 'NONE', #88932 ) ;
#99521 = ADVANCED_FACE ( 'NONE', ( #86052 ), #99770, .F. ) ;
#99522 = CARTESIAN_POINT ( 'NONE',  ( 9.489213562373095101, -27.52281430457062328, 5.000000000000000000 ) ) ;
#99523 = VERTEX_POINT ( 'NONE', #120058 ) ;
#99524 = AXIS2_PLACEMENT_3D ( 'NONE', #112918, #23019, #569 ) ;
#99525 = CARTESIAN_POINT ( 'NONE',  ( 83.85459685856476142, -1.637169565754161615, 6.110000000000000320 ) ) ;
#99526 = DIRECTION ( 'NONE',  ( -0.000000000000000000, -0.000000000000000000, -1.000000000000000000 ) ) ;
#99527 = LINE ( 'NONE', #122728, #96384 ) ;
#99528 = FACE_OUTER_BOUND ( 'NONE', #114993, .T. ) ;
#99529 = VECTOR ( 'NONE', #134690, 999.9999999999998863 ) ;
#99530 = FACE_OUTER_BOUND ( 'NONE', #21096, .T. ) ;
#99531 = DIRECTION ( 'NONE',  ( 1.000000000000000000, 0.000000000000000000, 0.000000000000000000 ) ) ;
#99532 = ORIENTED_EDGE ( 'NONE', *, *, #62378, .T. ) ;
#99533 = VECTOR ( 'NONE', #101727, 999.9999999999998863 ) ;
#99534 = DIRECTION ( 'NONE',  ( 0.7071067811865487940, 0.7071067811865463515, 0.000000000000000000 ) ) ;
#99535 = CARTESIAN_POINT ( 'NONE',  ( 64.80793019189812298, -6.109999999999998543, 1.637169565754158063 ) ) ;
#99536 = CARTESIAN_POINT ( 'NONE',  ( -24.98480450340313652, 2.536990198832462351, 5.000000000000000000 ) ) ;
#99537 = LINE ( 'NONE', #56821, #107972 ) ;
#99538 = CARTESIAN_POINT ( 'NONE',  ( 34.42499999999998295, 7.541399257801974620, 5.000000000000000000 ) ) ;
#99539 = ORIENTED_EDGE ( 'NONE', *, *, #18605, .T. ) ;
#99540 = ORIENTED_EDGE ( 'NONE', *, *, #80488, .F. ) ;
#99541 = AXIS2_PLACEMENT_3D ( 'NONE', #21233, #111069, #89347 ) ;
#99542 = CARTESIAN_POINT ( 'NONE',  ( 11.99999999999991296, 1.931123077392161935, 4.000000000000000000 ) ) ;
#99543 = ORIENTED_EDGE ( 'NONE', *, *, #94309, .F. ) ;
#99544 = ADVANCED_FACE ( 'NONE', ( #121514 ), #65771, .T. ) ;
#99545 = ADVANCED_FACE ( 'NONE', ( #32391 ), #12064, .F. ) ;
#99546 = FACE_OUTER_BOUND ( 'NONE', #100313, .T. ) ;
#99547 = VERTEX_POINT ( 'NONE', #31673 ) ;
#99548 = DIRECTION ( 'NONE',  ( 0.7071067811865487940, -0.7071067811865463515, 0.000000000000000000 ) ) ;
#99549 = DIRECTION ( 'NONE',  ( 0.6830127018922180770, -0.6830127018922204085, -0.2588190451025213501 ) ) ;
#99550 = DIRECTION ( 'NONE',  ( 0.7071067811865487940, 0.7071067811865463515, 0.000000000000000000 ) ) ;
#99551 = AXIS2_PLACEMENT_3D ( 'NONE', #31346, #20436, #42948 ) ;
#99552 = DIRECTION ( 'NONE',  ( 0.6830127018922181881, 0.6830127018922202975, -0.2588190451025214056 ) ) ;
#99553 = FACE_BOUND ( 'NONE', #85953, .T. ) ;
#99554 = EDGE_CURVE ( 'NONE', #131602, #65100, #97622, .T. ) ;
#99555 = PLANE ( 'NONE',  #64117 ) ;
#99556 = CARTESIAN_POINT ( 'NONE',  ( 17.29289321881333663, 14.25929247661557397, 5.000000000000000000 ) ) ;
#99557 = LINE ( 'NONE', #100999, #10914 ) ;
#99559 = ORIENTED_EDGE ( 'NONE', *, *, #364, .F. ) ;
#99558 = CARTESIAN_POINT ( 'NONE',  ( 50.97502705046288440, -5.819803920172573086, 5.819803920172573086 ) ) ;
#99560 = VECTOR ( 'NONE', #88102, 1000.000000000000000 ) ;
#99561 = PLANE ( 'NONE',  #39457 ) ;
#99562 = ORIENTED_EDGE ( 'NONE', *, *, #52204, .F. ) ;
#99563 = ORIENTED_EDGE ( 'NONE', *, *, #135634, .T. ) ;
#99564 = CARTESIAN_POINT ( 'NONE',  ( 72.24543019189810877, -5.291415217122918513, -3.055000000000000160 ) ) ;
#99565 = VERTEX_POINT ( 'NONE', #118670 ) ;
#99566 = LINE ( 'NONE', #240, #126337 ) ;
#99567 = DIRECTION ( 'NONE',  ( -0.7071067811865486830, -0.7071067811865464625, 0.000000000000000000 ) ) ;
#99568 = ORIENTED_EDGE ( 'NONE', *, *, #37252, .T. ) ;
#99569 = CARTESIAN_POINT ( 'NONE',  ( -34.92500000000002558, 18.75929247661552424, 4.255531930566273324 ) ) ;
#99570 = CARTESIAN_POINT ( 'NONE',  ( -10.49999999999993250, -1.592773361805382981, -6.492772025301205119 ) ) ;
#99571 = CARTESIAN_POINT ( 'NONE',  ( 0.000000000000000000, 0.000000000000000000, 7.950000000000000178 ) ) ;
#99572 = CIRCLE ( 'NONE', #55631, 2.500000000000000888 ) ;
#99573 = CARTESIAN_POINT ( 'NONE',  ( -18.48921356237309510, -27.52281430457068367, 5.000000000000000000 ) ) ;
#99574 = FILL_AREA_STYLE ('',( #90894 ) ) ;
#99575 = CARTESIAN_POINT ( 'NONE',  ( -26.67183060077628554, 17.25929247661554200, 4.000000000000000000 ) ) ;
#99576 = DIRECTION ( 'NONE',  ( -1.000000000000000000, -1.224606353822377258E-16, -0.000000000000000000 ) ) ;
#99577 = EDGE_CURVE ( 'NONE', #119311, #111908, #109244, .T. ) ;
#99579 = EDGE_LOOP ( 'NONE', ( #75057, #63601, #100298, #132662 ) ) ;
#99578 = VECTOR ( 'NONE', #26289, 1000.000000000000000 ) ;
#99580 = VECTOR ( 'NONE', #68127, 1000.000000000000000 ) ;
#99581 = VECTOR ( 'NONE', #92148, 1000.000000000000000 ) ;
#99582 = VECTOR ( 'NONE', #31896, 999.9999999999998863 ) ;
#99583 = VERTEX_POINT ( 'NONE', #133149 ) ;
#99584 = CARTESIAN_POINT ( 'NONE',  ( 31.17183060077625711, -14.24070752338414003, 4.000000000000000000 ) ) ;
#99585 = DIRECTION ( 'NONE',  ( -0.7071067811865487940, 0.7071067811865463515, -0.000000000000000000 ) ) ;
#99586 = VECTOR ( 'NONE', #19380, 1000.000000000000000 ) ;
#99587 = ORIENTED_EDGE ( 'NONE', *, *, #127956, .T. ) ;
#99588 = ORIENTED_EDGE ( 'NONE', *, *, #57629, .T. ) ;
#99589 = EDGE_CURVE ( 'NONE', #110816, #75950, #19361, .T. ) ;
#99590 = CARTESIAN_POINT ( 'NONE',  ( 27.56293019189810778, 1.637169565754157174, 6.110000000000002984 ) ) ;
#99591 = ORIENTED_EDGE ( 'NONE', *, *, #52529, .T. ) ;
#99592 = VECTOR ( 'NONE', #102222, 1000.000000000000227 ) ;
#99593 = CARTESIAN_POINT ( 'NONE',  ( -22.49999999999984013, -5.568876922607759461, 4.000000000000000000 ) ) ;
#99594 = CARTESIAN_POINT ( 'NONE',  ( 89.18336038379622721, -2.130196079827426203, 7.949999999999996625 ) ) ;
#99595 = EDGE_CURVE ( 'NONE', #98842, #82613, #20777, .T. ) ;
#99596 = CARTESIAN_POINT ( 'NONE',  ( 27.60830628287043709, 1.633150327867687324, -6.094999999999991758 ) ) ;
#99597 = DIRECTION ( 'NONE',  ( -1.000000000000000000, -1.224606353822377258E-16, -0.000000000000000000 ) ) ;
#99598 = EDGE_CURVE ( 'NONE', #31655, #72010, #139433, .T. ) ;
#99599 = EDGE_LOOP ( 'NONE', ( #6873, #21462, #34837, #5817 ) ) ;
#99600 = DIRECTION ( 'NONE',  ( -0.6830127018922180770, -0.6830127018922204085, -0.2588190451025213501 ) ) ;
#99602 = ORIENTED_EDGE ( 'NONE', *, *, #139695, .F. ) ;
#99601 = EDGE_CURVE ( 'NONE', #86268, #6488, #75200, .T. ) ;
#99603 = DIRECTION ( 'NONE',  ( -1.000000000000000000, -1.224606353822377258E-16, -0.000000000000000000 ) ) ;
#99604 = COLOUR_RGB ( '', 0.09019608, 0.27058824, 0.51372549) ;
#99605 = DIRECTION ( 'NONE',  ( -0.6830127018922181881, 0.6830127018922202975, -0.2588190451025214056 ) ) ;
#99607 = VERTEX_POINT ( 'NONE', #43274 ) ;
#99606 = DIRECTION ( 'NONE',  ( -0.7071067811865487940, 0.7071067811865463515, 0.000000000000000000 ) ) ;
#99608 = ORIENTED_EDGE ( 'NONE', *, *, #81530, .T. ) ;
#99609 = EDGE_CURVE ( 'NONE', #31236, #4046, #96876, .T. ) ;
#99610 = DIRECTION ( 'NONE',  ( 0.7071067811865487940, 0.7071067811865463515, -0.000000000000000000 ) ) ;
#99611 = LINE ( 'NONE', #109793, #127871 ) ;
#99612 = DIRECTION ( 'NONE',  ( -0.7071067811865487940, 0.7071067811865463515, -0.000000000000000000 ) ) ;
#99613 = ORIENTED_EDGE ( 'NONE', *, *, #66263, .T. ) ;
#99614 = AXIS2_PLACEMENT_3D ( 'NONE', #80671, #89384, #67675 ) ;
#99615 = DIRECTION ( 'NONE',  ( -0.000000000000000000, 0.000000000000000000, 1.000000000000000000 ) ) ;
#99616 = VECTOR ( 'NONE', #66797, 1000.000000000000000 ) ;
#99617 = VERTEX_POINT ( 'NONE', #141122 ) ;
#99618 = EDGE_CURVE ( 'NONE', #16747, #42386, #109934, .T. ) ;
#99620 = DIRECTION ( 'NONE',  ( 0.7071067811865487940, 0.7071067811865463515, 0.000000000000000000 ) ) ;
#99619 = AXIS2_PLACEMENT_3D ( 'NONE', #133062, #77948, #11948 ) ;
#99621 = CARTESIAN_POINT ( 'NONE',  ( 28.99999999999999645, 0.000000000000000000, -7.950000000000000178 ) ) ;
#99622 = CARTESIAN_POINT ( 'NONE',  ( 69.18398860626899705, 28.73617430169835529, 5.000000000000000000 ) ) ;
#99623 = CARTESIAN_POINT ( 'NONE',  ( -63.48921356237309510, -27.52281430457099631, 5.000000000000000000 ) ) ;
#99624 = VECTOR ( 'NONE', #43166, 999.9999999999998863 ) ;
#99625 = SURFACE_STYLE_USAGE ( .BOTH. , #64894 ) ;
#99626 = DIRECTION ( 'NONE',  ( -0.7071067811865486830, -0.7071067811865464625, 0.000000000000000000 ) ) ;
#99627 = ADVANCED_FACE ( 'NONE', ( #108464 ), #143277, .F. ) ;
#99628 = DIRECTION ( 'NONE',  ( 0.7071067811865487940, 0.7071067811865463515, 0.000000000000000000 ) ) ;
#99629 = CARTESIAN_POINT ( 'NONE',  ( 0.000000000000000000, 0.000000000000000000, 10.00000000000000000 ) ) ;
#99630 = EDGE_CURVE ( 'NONE', #76459, #37329, #47585, .T. ) ;
#99631 = EDGE_LOOP ( 'NONE', ( #127297, #42404, #13503, #26890 ) ) ;
#99632 = VECTOR ( 'NONE', #48302, 1000.000000000000114 ) ;
#99633 = DIRECTION ( 'NONE',  ( 0.7071067811865486830, -0.7071067811865464625, -0.000000000000000000 ) ) ;
#99634 = ORIENTED_EDGE ( 'NONE', *, *, #116768, .T. ) ;
#99635 = LINE ( 'NONE', #22074, #23911 ) ;
#99636 = EDGE_CURVE ( 'NONE', #68994, #8228, #90320, .T. ) ;
#99637 = FILL_AREA_STYLE ('',( #56901 ) ) ;
#99638 = CARTESIAN_POINT ( 'NONE',  ( -15.32816939922342314, 14.25929247661557042, 4.000000000000000000 ) ) ;
#99639 = VERTEX_POINT ( 'NONE', #114216 ) ;
#99640 = VECTOR ( 'NONE', #108917, 1000.000000000000000 ) ;
#99641 = CARTESIAN_POINT ( 'NONE',  ( 22.49999999999984723, -7.533600742197665845, 5.000000000000000000 ) ) ;
#99642 = LINE ( 'NONE', #44615, #4755 ) ;
#99643 = CARTESIAN_POINT ( 'NONE',  ( 20.99451991528748707, 28.92564299267952777, 4.000000000000000000 ) ) ;
#99644 = VERTEX_POINT ( 'NONE', #80894 ) ;
#99645 = CARTESIAN_POINT ( 'NONE',  ( -34.49999999999975842, -10.04351517176480613, -1.623559851933904508 ) ) ;
#99646 = CARTESIAN_POINT ( 'NONE',  ( 19.82816939922339827, 18.75929247661552424, 4.000000000000000000 ) ) ;
#99647 = VECTOR ( 'NONE', #14477, 1000.000000000000114 ) ;
#99648 = DIRECTION ( 'NONE',  ( -0.000000000000000000, -0.3543493200069152693, 0.9351131265310292928 ) ) ;
#99649 = CARTESIAN_POINT ( 'NONE',  ( 52.47916666666665009, -7.950000000000000178, 2.130196079827424427 ) ) ;
#99650 = CARTESIAN_POINT ( 'NONE',  ( 23.03315071937583980, 7.620612595215163765, 4.000000000000000000 ) ) ;
#99651 = CARTESIAN_POINT ( 'NONE',  ( 59.99543019189810877, 5.291415217122917625, 3.055000000000002380 ) ) ;
#99652 = CARTESIAN_POINT ( 'NONE',  ( -54.48921356237310221, -27.52281430457093236, 5.000000000000000000 ) ) ;
#99653 = CARTESIAN_POINT ( 'NONE',  ( 0.000000000000000000, 0.000000000000000000, 0.000000000000000000 ) ) ;
#99654 = CARTESIAN_POINT ( 'NONE',  ( -23.29289321881329755, -18.74070752338409207, 5.000000000000000000 ) ) ;
#99655 = CARTESIAN_POINT ( 'NONE',  ( 32.60002705046288440, 5.819803920172570422, 5.819803920172575751 ) ) ;
#99656 = LINE ( 'NONE', #77937, #9417 ) ;
#99657 = ORIENTED_EDGE ( 'NONE', *, *, #50507, .T. ) ;
#99658 = SURFACE_STYLE_FILL_AREA ( #133051 ) ;
#99659 = EDGE_CURVE ( 'NONE', #121565, #38043, #104591, .T. ) ;
#99660 = ORIENTED_EDGE ( 'NONE', *, *, #56265, .T. ) ;
#99661 = CIRCLE ( 'NONE', #53413, 2.500000000000000888 ) ;
#99662 = LINE ( 'NONE', #120696, #45498 ) ;
#99663 = CARTESIAN_POINT ( 'NONE',  ( 6.707013264292989163, -21.74070752338407075, 4.999753212805213565 ) ) ;
#99664 = LINE ( 'NONE', #43176, #129443 ) ;
#99665 = DIRECTION ( 'NONE',  ( -0.7071067811865486830, -0.7071067811865464625, 0.000000000000000000 ) ) ;
#99666 = CARTESIAN_POINT ( 'NONE',  ( 25.39999999999999858, -18.48000000000005372, 34.92499999999998295 ) ) ;
#99667 = CARTESIAN_POINT ( 'NONE',  ( -34.42500000000001137, -22.22500000000000142, 5.000000000000000000 ) ) ;
#99668 = FACE_OUTER_BOUND ( 'NONE', #91122, .T. ) ;
#99669 = ORIENTED_EDGE ( 'NONE', *, *, #143334, .F. ) ;
#99670 = VERTEX_POINT ( 'NONE', #24355 ) ;
#99671 = CARTESIAN_POINT ( 'NONE',  ( 18.48921356237309510, -27.52281430457068367, 5.000000000000000000 ) ) ;
#99672 = DIRECTION ( 'NONE',  ( -0.6830127018922180770, -0.6830127018922204085, -0.2588190451025213501 ) ) ;
#99673 = UNCERTAINTY_MEASURE_WITH_UNIT (LENGTH_MEASURE( 1.000000000000000082E-05 ), #104116, 'distance_accuracy_value', 'NONE');
#99674 = AXIS2_PLACEMENT_3D ( 'NONE', #126215, #92134, #136364 ) ;
#99675 = CARTESIAN_POINT ( 'NONE',  ( -32.99999999999976552, -1.068876922607802538, 4.000000000000000000 ) ) ;
#99676 = EDGE_CURVE ( 'NONE', #89784, #50446, #123701, .T. ) ;
#99677 = CARTESIAN_POINT ( 'NONE',  ( -18.48921356237309510, -27.52281430457068367, 5.000000000000000000 ) ) ;
#99678 = CARTESIAN_POINT ( 'NONE',  ( 87.43336038379624142, 2.130196079827431532, -7.949999999999997513 ) ) ;
#99679 = PLANE ( 'NONE',  #25512 ) ;
#99680 = DIRECTION ( 'NONE',  ( -0.6830127018922181881, 0.6830127018922202975, -0.2588190451025214056 ) ) ;
#99681 = ORIENTED_EDGE ( 'NONE', *, *, #4165, .F. ) ;
#99682 =( BOUNDED_CURVE ( )  B_SPLINE_CURVE ( 3, ( #5278, #137977, #93749, #104616 ),
 .UNSPECIFIED., .F., .T. ) 
 B_SPLINE_CURVE_WITH_KNOTS ( ( 4, 4 ),
 ( 2.001653308786158547, 3.503810798801450854 ),
 .UNSPECIFIED. ) 
 CURVE ( )  GEOMETRIC_REPRESENTATION_ITEM ( )  RATIONAL_B_SPLINE_CURVE ( ( 1.000000000000000000, 0.8206354192515217250, 0.8206354192515217250, 1.000000000000000000 ) ) 
 REPRESENTATION_ITEM ( '' )  );
#99683 = CARTESIAN_POINT ( 'NONE',  ( 69.39583333333331439, -2.130196079827427091, 7.949999999999999289 ) ) ;
#99684 = PLANE ( 'NONE',  #30763 ) ;
#99685 = EDGE_CURVE ( 'NONE', #57414, #93303, #116183, .T. ) ;
#99686 = LINE ( 'NONE', #12675, #127271 ) ;
#99687 = LINE ( 'NONE', #34446, #105319 ) ;
#99688 = ORIENTED_EDGE ( 'NONE', *, *, #112592, .T. ) ;
#99689 = CONICAL_SURFACE ( 'NONE', #90494, 2.500000000000000888, 0.9599310885968822538 ) ;
#99690 = CARTESIAN_POINT ( 'NONE',  ( 0.000000000000000000, 0.000000000000000000, 5.000000000000000000 ) ) ;
#99691 = VECTOR ( 'NONE', #61638, 1000.000000000000000 ) ;
#99692 = ORIENTED_EDGE ( 'NONE', *, *, #97854, .F. ) ;
#99693 = VECTOR ( 'NONE', #75680, 1000.000000000000227 ) ;
#99694 = EDGE_CURVE ( 'NONE', #18830, #102325, #101196, .T. ) ;
#99695 = CARTESIAN_POINT ( 'NONE',  ( 50.99451991528749062, 28.92564299267973738, 4.000000000000000000 ) ) ;
#99696 = CARTESIAN_POINT ( 'NONE',  ( 62.56293019189811133, 1.637169565754157174, 6.110000000000002984 ) ) ;
#99697 = DIRECTION ( 'NONE',  ( 0.7071067811865487940, 0.7071067811865463515, -0.000000000000000000 ) ) ;
#99698 = VERTEX_POINT ( 'NONE', #68601 ) ;
#99699 = CIRCLE ( 'NONE', #129822, 2.500000000000000444 ) ;
#99700 = VECTOR ( 'NONE', #117288, 1000.000000000000000 ) ;
#99701 = VECTOR ( 'NONE', #14946, 1000.000000000000000 ) ;
#99702 = AXIS2_PLACEMENT_3D ( 'NONE', #65655, #54053, #43154 ) ;
#99703 = FACE_OUTER_BOUND ( 'NONE', #22259, .T. ) ;
#99704 = LINE ( 'NONE', #106446, #54543 ) ;
#99705 = CARTESIAN_POINT ( 'NONE',  ( -29.00492477221176557, -5.240707523384228850, 12.38332538355502699 ) ) ;
#99706 = DIRECTION ( 'NONE',  ( 0.6830127018922181881, 0.6830127018922202975, -0.2588190451025214056 ) ) ;
#99707 = EDGE_CURVE ( 'NONE', #21499, #119750, #112787, .T. ) ;
#99708 = DIRECTION ( 'NONE',  ( -0.000000000000000000, -0.9976538855070752332, -0.06845965770171358322 ) ) ;
#99710 = ORIENTED_EDGE ( 'NONE', *, *, #135299, .F. ) ;
#99709 = CARTESIAN_POINT ( 'NONE',  ( 13.49999999999990052, -12.66682484999665093, -0.6294897503863620125 ) ) ;
#99711 =( NAMED_UNIT ( * ) PLANE_ANGLE_UNIT ( ) SI_UNIT ( $, .RADIAN. ) );
#99712 = CARTESIAN_POINT ( 'NONE',  ( 14.27159235450332098, -2.500000000000000000, 3.061616997868384127E-16 ) ) ;
#99713 = CARTESIAN_POINT ( 'NONE',  ( 35.99451991528749772, 28.92564299267963079, 4.000000000000000000 ) ) ;
#99714 = AXIS2_PLACEMENT_3D ( 'NONE', #67271, #57132, #46996 ) ;
#99715 = CARTESIAN_POINT ( 'NONE',  ( 60.48921356237309510, -27.52281430457097500, 5.000000000000000000 ) ) ;
#99716 = VERTEX_POINT ( 'NONE', #22893 ) ;
#99717 = EDGE_LOOP ( 'NONE', ( #105125, #58524, #32274, #86899 ) ) ;
#99718 = CARTESIAN_POINT ( 'NONE',  ( 67.81293019189807580, -1.637169565754159617, -6.110000000000001208 ) ) ;
#99719 = ORIENTED_EDGE ( 'NONE', *, *, #125526, .T. ) ;
#99720 = AXIS2_PLACEMENT_3D ( 'NONE', #87098, #65376, #132043 ) ;
#99721 = FACE_OUTER_BOUND ( 'NONE', #34192, .T. ) ;
#99722 = LINE ( 'NONE', #123657, #135992 ) ;
#99723 = AXIS2_PLACEMENT_3D ( 'NONE', #27996, #136739, #115670 ) ;
#99724 = CARTESIAN_POINT ( 'NONE',  ( 15.79333936457837062, 21.75929247661549937, 4.998822639870715179 ) ) ;
#99725 = LINE ( 'NONE', #43232, #142775 ) ;
#99726 = VERTEX_POINT ( 'NONE', #13450 ) ;
#99727 = VERTEX_POINT ( 'NONE', #69307 ) ;
#99728 = DIRECTION ( 'NONE',  ( 1.000000000000000000, 0.000000000000000000, 0.000000000000000000 ) ) ;
#99729 =( NAMED_UNIT ( * ) SI_UNIT ( $, .STERADIAN. ) SOLID_ANGLE_UNIT ( ) );
#99730 = ADVANCED_FACE ( 'NONE', ( #58478 ), #3970, .F. ) ;
#99731 = VECTOR ( 'NONE', #133988, 1000.000000000000000 ) ;
#99732 = ORIENTED_EDGE ( 'NONE', *, *, #136880, .F. ) ;
#99733 = VECTOR ( 'NONE', #95966, 1000.000000000000227 ) ;
#99734 = EDGE_CURVE ( 'NONE', #55981, #136091, #90757, .T. ) ;
#99735 = PLANE ( 'NONE',  #25950 ) ;
#99736 = VECTOR ( 'NONE', #66893, 1000.000000000000114 ) ;
#99737 = LINE ( 'NONE', #33797, #115104 ) ;
#99738 = FACE_OUTER_BOUND ( 'NONE', #133410, .T. ) ;
#99739 = CONICAL_SURFACE ( 'NONE', #136790, 2.500000000000000444, 0.9599310885968830309 ) ;
#99740 = ORIENTED_EDGE ( 'NONE', *, *, #31562, .T. ) ;
#99741 = FACE_BOUND ( 'NONE', #14400, .T. ) ;
#99742 = VECTOR ( 'NONE', #94480, 1000.000000000000000 ) ;
#99743 = ADVANCED_FACE ( 'NONE', ( #12042 ), #101918, .T. ) ;
#99744 = CARTESIAN_POINT ( 'NONE',  ( -14.20710678118644488, -20.24070752338407431, 5.000000000000000000 ) ) ;
#99745 = CARTESIAN_POINT ( 'NONE',  ( 0.000000000000000000, -4.600000000000061817, 28.92500000000000426 ) ) ;
#99746 = DIRECTION ( 'NONE',  ( 0.3543493200069162685, -0.000000000000000000, -0.9351131265310288487 ) ) ;
#99747 = LINE ( 'NONE', #141100, #122158 ) ;
#99748 = SURFACE_STYLE_USAGE ( .BOTH. , #55555 ) ;
#99749 = ORIENTED_EDGE ( 'NONE', *, *, #108340, .F. ) ;
#99750 = VECTOR ( 'NONE', #58369, 999.9999999999998863 ) ;
#99751 = EDGE_LOOP ( 'NONE', ( #21752, #19149, #141305, #86933 ) ) ;
#99752 = CARTESIAN_POINT ( 'NONE',  ( 106.0787635252314516, -7.482591942790325086E-16, 6.109999999999998543 ) ) ;
#99753 = VERTEX_POINT ( 'NONE', #112101 ) ;
#99754 = DIRECTION ( 'NONE',  ( 1.000000000000000000, 0.000000000000000000, 0.000000000000000000 ) ) ;
#99755 = ORIENTED_EDGE ( 'NONE', *, *, #16485, .T. ) ;
#99756 = COLOUR_RGB ( '', 0.08235294, 0.09019608, 0.10196078) ;
#99757 = PLANE ( 'NONE',  #42353 ) ;
#99758 = VECTOR ( 'NONE', #92684, 1000.000000000000000 ) ;
#99759 = EDGE_CURVE ( 'NONE', #78430, #90132, #1834, .T. ) ;
#99760 = CARTESIAN_POINT ( 'NONE',  ( 14.81601139373099585, 28.73617430169776910, 5.000000000000000000 ) ) ;
#99761 = LINE ( 'NONE', #432, #111977 ) ;
#99762 = VERTEX_POINT ( 'NONE', #36650 ) ;
#99763 = CARTESIAN_POINT ( 'NONE',  ( 57.18398860626899705, 28.73617430169827358, 5.000000000000000000 ) ) ;
#99764 = CARTESIAN_POINT ( 'NONE',  ( -38.20003122016812824, 8.259292476615641476, 16.85664084051850509 ) ) ;
#99765 = DIRECTION ( 'NONE',  ( 0.000000000000000000, 0.000000000000000000, -1.000000000000000000 ) ) ;
#99767 = DIRECTION ( 'NONE',  ( -0.7071067811865486830, -0.7071067811865464625, 0.000000000000000000 ) ) ;
#99766 = LINE ( 'NONE', #46135, #31877 ) ;
#99768 = DIRECTION ( 'NONE',  ( -0.7071067811865486830, -0.7071067811865464625, 0.000000000000000000 ) ) ;
#99769 = AXIS2_PLACEMENT_3D ( 'NONE', #22930, #45470, #21547 ) ;
#99770 = PLANE ( 'NONE',  #25949 ) ;
#99771 = VERTEX_POINT ( 'NONE', #103320 ) ;
#99772 = FACE_OUTER_BOUND ( 'NONE', #86240, .T. ) ;
#99773 = FACE_OUTER_BOUND ( 'NONE', #93261, .T. ) ;
#99774 = ORIENTED_EDGE ( 'NONE', *, *, #35243, .F. ) ;
#99775 = VERTEX_POINT ( 'NONE', #135972 ) ;
#99776 = ORIENTED_EDGE ( 'NONE', *, *, #17042, .T. ) ;
#99777 = CARTESIAN_POINT ( 'NONE',  ( 55.41709685856477563, 3.054999999999998828, 5.291415217122922066 ) ) ;
#99778 = VECTOR ( 'NONE', #128416, 1000.000000000000000 ) ;
#99779 = ORIENTED_EDGE ( 'NONE', *, *, #69462, .F. ) ;
#99780 = FACE_OUTER_BOUND ( 'NONE', #4169, .T. ) ;
#99781 = EDGE_CURVE ( 'NONE', #132715, #8240, #46892, .T. ) ;
#99782 = CARTESIAN_POINT ( 'NONE',  ( 1.358306282870439308, -1.633150327867689988, 6.094999999999989981 ) ) ;
#99783 = CARTESIAN_POINT ( 'NONE',  ( 88.66709685856477563, -3.055000000000000160, -5.291415217122921177 ) ) ;
#99784 = DIRECTION ( 'NONE',  ( 1.000000000000000000, 0.000000000000000000, 0.000000000000000000 ) ) ;
#99785 = EDGE_CURVE ( 'NONE', #20021, #41454, #89608, .T. ) ;
#99786 = VERTEX_POINT ( 'NONE', #134573 ) ;
#99787 = CARTESIAN_POINT ( 'NONE',  ( 34.92499999999998295, -21.72500000000000142, 5.000000000000000000 ) ) ;
#99788 = VECTOR ( 'NONE', #103703, 1000.000000000000000 ) ;
#99789 = DIRECTION ( 'NONE',  ( -0.3543493200069162685, -0.000000000000000000, -0.9351131265310288487 ) ) ;
#99790 = EDGE_CURVE ( 'NONE', #42222, #82630, #91070, .T. ) ;
#99791 = EDGE_CURVE ( 'NONE', #48215, #142779, #57022, .T. ) ;
#99792 = DIRECTION ( 'NONE',  ( 0.7071067811865487940, -0.7071067811865463515, 0.000000000000000000 ) ) ;
#99794 = LINE ( 'NONE', #28505, #89210 ) ;
#99793 = AXIS2_PLACEMENT_3D ( 'NONE', #82329, #70752, #126511 ) ;
#99796 = VERTEX_POINT ( 'NONE', #14897 ) ;
#99795 = VECTOR ( 'NONE', #123127, 1000.000000000000000 ) ;
#99797 = CARTESIAN_POINT ( 'NONE',  ( 0.000000000000000000, 0.000000000000000000, 5.000000000000000000 ) ) ;
#99798 = DIRECTION ( 'NONE',  ( 0.6830127018922181881, 0.6830127018922202975, -0.2588190451025214056 ) ) ;
#99799 = ORIENTED_EDGE ( 'NONE', *, *, #21897, .T. ) ;
#99800 = B_SPLINE_CURVE_WITH_KNOTS ( 'NONE', 3,
 ( #18061, #15220, #6462, #48600 ),
 .UNSPECIFIED., .F., .F.,
 ( 4, 4 ),
 ( 0.008853860144884201713, 0.009403245473020212589 ),
 .UNSPECIFIED. ) ;
#99801 = VERTEX_POINT ( 'NONE', #59854 ) ;
#99802 = EDGE_LOOP ( 'NONE', ( #43570, #112435, #80156, #17434 ) ) ;
#99803 = CARTESIAN_POINT ( 'NONE',  ( 122.5579301918981088, 6.110000000000000320, -1.637169565754156064 ) ) ;
#99804 = VECTOR ( 'NONE', #126732, 1000.000000000000000 ) ;
#99805 = VECTOR ( 'NONE', #93797, 1000.000000000000000 ) ;
#99806 = VECTOR ( 'NONE', #6184, 1000.000000000000000 ) ;
#99807 = AXIS2_PLACEMENT_3D ( 'NONE', #114512, #57323, #36957 ) ;
#99808 = AXIS2_PLACEMENT_3D ( 'NONE', #111947, #80752, #123557 ) ;
#99809 = FACE_OUTER_BOUND ( 'NONE', #94297, .T. ) ;
#99810 = EDGE_CURVE ( 'NONE', #13309, #101471, #26503, .T. ) ;
#99811 = DIRECTION ( 'NONE',  ( 0.7071067811865487940, 0.7071067811865463515, 0.000000000000000000 ) ) ;
#99812 = EDGE_CURVE ( 'NONE', #13717, #5851, #83030, .T. ) ;
#99813 = ORIENTED_EDGE ( 'NONE', *, *, #115798, .T. ) ;
#99814 = DIRECTION ( 'NONE',  ( 0.000000000000000000, -1.000000000000000000, 0.000000000000000000 ) ) ;
#99815 = DIRECTION ( 'NONE',  ( -0.7071067811865486830, -0.7071067811865464625, 0.000000000000000000 ) ) ;
#99817 = ORIENTED_EDGE ( 'NONE', *, *, #75077, .T. ) ;
#99816 = VECTOR ( 'NONE', #131810, 1000.000000000000000 ) ;
#99818 = ADVANCED_FACE ( 'NONE', ( #70749 ), #51837, .F. ) ;
#99819 = CARTESIAN_POINT ( 'NONE',  ( 16.60373647476855297, 5.808823158059036373, 5.808823158059032821 ) ) ;
#99820 = LINE ( 'NONE', #10643, #92548 ) ;
#99821 = LINE ( 'NONE', #99079, #115399 ) ;
#99822 = AXIS2_PLACEMENT_3D ( 'NONE', #83016, #28648, #104755 ) ;
#99823 = CARTESIAN_POINT ( 'NONE',  ( -32.09920400167933252, 22.26999999999998536, -14.71147562388301289 ) ) ;
#99824 = VERTEX_POINT ( 'NONE', #62719 ) ;
#99825 = VERTEX_POINT ( 'NONE', #27199 ) ;
#99826 = VERTEX_POINT ( 'NONE', #106901 ) ;
#99827 = FACE_OUTER_BOUND ( 'NONE', #28311, .T. ) ;
#99828 = CARTESIAN_POINT ( 'NONE',  ( -42.18398860626899705, 28.73617430169816700, 5.000000000000000000 ) ) ;
#99829 = EDGE_CURVE ( 'NONE', #75799, #106339, #49197, .T. ) ;
#99830 = CARTESIAN_POINT ( 'NONE',  ( -8.534745106696862769E-17, 0.000000000000000000, 0.000000000000000000 ) ) ;
#99831 = CARTESIAN_POINT ( 'NONE',  ( 7.939999999999994174, -35.76999999999998892, -10.00000000000000178 ) ) ;
#99832 = VECTOR ( 'NONE', #115045, 1000.000000000000000 ) ;
#99833 = AXIS2_PLACEMENT_3D ( 'NONE', #120195, #109360, #11440 ) ;
#99834 = CARTESIAN_POINT ( 'NONE',  ( -14.54487008052910824, -0.7407075233842735917, 4.335043535661659675 ) ) ;
#99835 = CARTESIAN_POINT ( 'NONE',  ( 21.79289321881330821, -2.240707523384255939, 5.000000000000000000 ) ) ;
#99836 = CARTESIAN_POINT ( 'NONE',  ( 19.41932091537965732, -22.22500000000000142, -15.59309469223181210 ) ) ;
#99837 = CARTESIAN_POINT ( 'NONE',  ( -27.32816939922334853, 11.25929247661560062, 4.000000000000000000 ) ) ;
#99838 = VECTOR ( 'NONE', #84638, 1000.000000000000000 ) ;
#99839 = ORIENTED_EDGE ( 'NONE', *, *, #14346, .F. ) ;
#99840 = DIRECTION ( 'NONE',  ( -1.000000000000000000, 0.000000000000000000, 0.000000000000000000 ) ) ;
#99841 = EDGE_CURVE ( 'NONE', #88480, #78244, #116367, .T. ) ;
#99842 = ORIENTED_EDGE ( 'NONE', *, *, #21282, .T. ) ;
#99844 = VECTOR ( 'NONE', #110708, 1000.000000000000000 ) ;
#99843 = CARTESIAN_POINT ( 'NONE',  ( -20.99999999999985079, -21.03360074219752462, 5.000000000000000000 ) ) ;
#99845 = ORIENTED_EDGE ( 'NONE', *, *, #110640, .T. ) ;
#99846 = FACE_OUTER_BOUND ( 'NONE', #10734, .T. ) ;
#99848 = ORIENTED_EDGE ( 'NONE', *, *, #97654, .T. ) ;
#99847 = FACE_OUTER_BOUND ( 'NONE', #55346, .T. ) ;
#99849 = AXIS2_PLACEMENT_3D ( 'NONE', #54421, #121061, #21764 ) ;
#99850 = DIRECTION ( 'NONE',  ( -1.000000000000000000, -0.000000000000000000, -0.000000000000000000 ) ) ;
#99851 = DIRECTION ( 'NONE',  ( -0.000000000000000000, 0.3543493200069153248, 0.9351131265310292928 ) ) ;
#99852 = ORIENTED_EDGE ( 'NONE', *, *, #74200, .T. ) ;
#99853 = DIRECTION ( 'NONE',  ( -0.7071067811865487940, 0.7071067811865463515, -0.000000000000000000 ) ) ;
#99854 = ORIENTED_EDGE ( 'NONE', *, *, #91236, .T. ) ;
#99855 = DIRECTION ( 'NONE',  ( 0.7071067811865486830, -0.7071067811865464625, -0.000000000000000000 ) ) ;
#99856 = ORIENTED_EDGE ( 'NONE', *, *, #138484, .T. ) ;
#99857 = DIRECTION ( 'NONE',  ( 1.000000000000000000, 0.000000000000000000, 0.000000000000000000 ) ) ;
#99858 = EDGE_CURVE ( 'NONE', #63474, #3210, #5431, .T. ) ;
#99859 = CARTESIAN_POINT ( 'NONE',  ( 112.2250270504628986, 5.819803920172573086, -5.819803920172572198 ) ) ;
#99860 = CARTESIAN_POINT ( 'NONE',  ( 92.00000000000000000, 0.000000000000000000, -7.950000000000000178 ) ) ;
#99861 = PRESENTATION_STYLE_ASSIGNMENT (( #76716 ) ) ;
#99862 = DIRECTION ( 'NONE',  ( 0.6830127018922180770, -0.6830127018922204085, -0.2588190451025213501 ) ) ;
#99863 = DIRECTION ( 'NONE',  ( -1.000000000000000000, -1.224606353822377258E-16, -0.000000000000000000 ) ) ;
#99864 = CARTESIAN_POINT ( 'NONE',  ( -16.49999999999987921, -7.912538124160673370, 4.000000000000000000 ) ) ;
#99866 = AXIS2_PLACEMENT_3D ( 'NONE', #40717, #5896, #105932 ) ;
#99865 = CARTESIAN_POINT ( 'NONE',  ( 14.00000000000000178, 0.000000000000000000, 6.094999999999989981 ) ) ;
#99867 = CARTESIAN_POINT ( 'NONE',  ( 25.30244920428738453, -6.182694495602187423, -5.161259005940558531 ) ) ;
#99869 = VECTOR ( 'NONE', #106780, 1000.000000000000227 ) ;
#99868 = LINE ( 'NONE', #43358, #67494 ) ;
#99870 = DIRECTION ( 'NONE',  ( -0.6830127018922180770, -0.6830127018922204085, -0.2588190451025213501 ) ) ;
#99871 = VERTEX_POINT ( 'NONE', #114895 ) ;
#99872 = VERTEX_POINT ( 'NONE', #6839 ) ;
#99873 = CARTESIAN_POINT ( 'NONE',  ( 18.32266436734346726, 2.055000000000001048, 0.000000000000000000 ) ) ;
#99874 = VERTEX_POINT ( 'NONE', #51122 ) ;
#99875 = EDGE_CURVE ( 'NONE', #108597, #4396, #95317, .T. ) ;
#99876 = CARTESIAN_POINT ( 'NONE',  ( 105.0004301918981184, -3.055000000000002380, 5.291415217122920289 ) ) ;
#99877 = DIRECTION ( 'NONE',  ( -0.6830127018922181881, 0.6830127018922202975, -0.2588190451025214056 ) ) ;
#99878 = LINE ( 'NONE', #89712, #141217 ) ;
#99880 = VECTOR ( 'NONE', #99633, 1000.000000000000000 ) ;
#99879 = CARTESIAN_POINT ( 'NONE',  ( -63.29974487139158867, -27.71228299555250274, 4.000000000000000000 ) ) ;
#99881 = SURFACE_STYLE_USAGE ( .BOTH. , #54967 ) ;
#99882 = VERTEX_POINT ( 'NONE', #15573 ) ;
#99883 = DIRECTION ( 'NONE',  ( -1.084202172485504681E-16, 1.000000000000000000, 0.000000000000000000 ) ) ;
#99884 = CARTESIAN_POINT ( 'NONE',  ( 13.60986171580761805, -2.055000000000000160, 0.000000000000000000 ) ) ;
#99885 = PLANE ( 'NONE',  #104355 ) ;
#99886 = EDGE_CURVE ( 'NONE', #33831, #33645, #61324, .T. ) ;
#99887 = DIRECTION ( 'NONE',  ( 0.7071067811865487940, 0.7071067811865463515, 0.000000000000000000 ) ) ;
#99889 = ORIENTED_EDGE ( 'NONE', *, *, #65939, .F. ) ;
#99888 = CARTESIAN_POINT ( 'NONE',  ( 30.29974487139158867, -27.71228299555227537, 4.000000000000000000 ) ) ;
#99890 = FACE_OUTER_BOUND ( 'NONE', #87159, .T. ) ;
#99891 = DIRECTION ( 'NONE',  ( -0.7071067811865487940, 0.7071067811865463515, 0.000000000000000000 ) ) ;
#99892 = VECTOR ( 'NONE', #91682, 1000.000000000000000 ) ;
#99893 = DIRECTION ( 'NONE',  ( 0.5735764363510451602, 0.8191520442889924647, 0.000000000000000000 ) ) ;
#99894 = DIRECTION ( 'NONE',  ( -0.6830127018922181881, 0.6830127018922202975, -0.2588190451025214056 ) ) ;
#99895 = CARTESIAN_POINT ( 'NONE',  ( 0.000000000000000000, 0.000000000000000000, 5.000000000000000000 ) ) ;
#99896 = EDGE_LOOP ( 'NONE', ( #108451, #133012, #59440, #97172 ) ) ;
#99897 = ORIENTED_EDGE ( 'NONE', *, *, #96635, .T. ) ;
#99898 = EDGE_LOOP ( 'NONE', ( #87238, #97027, #11701, #140940 ) ) ;
#99899 = CARTESIAN_POINT ( 'NONE',  ( 89.83376352523143282, 6.110000000000001208, 1.122388791418549305E-15 ) ) ;
#99900 = VERTEX_POINT ( 'NONE', #4683 ) ;
#99901 = CARTESIAN_POINT ( 'NONE',  ( -1.499999999999980460, -17.94781430457065241, 5.000000000000000000 ) ) ;
#99902 = CYLINDRICAL_SURFACE ( 'NONE', #68868, 2.500000000000000444 ) ;
#99903 = CARTESIAN_POINT ( 'NONE',  ( -25.17183060077628909, -11.24070752338416845, 4.000000000000000000 ) ) ;
#99904 = CARTESIAN_POINT ( 'NONE',  ( 84.37086038379624142, 6.884901960086289741, -3.974999999999993427 ) ) ;
#99905 = VERTEX_POINT ( 'NONE', #48983 ) ;
#99906 = AXIS2_PLACEMENT_3D ( 'NONE', #132498, #66500, #110664 ) ;
#99907 = CARTESIAN_POINT ( 'NONE',  ( 184.1374510928294512, -50.57777258831012546, 35.91905586107260717 ) ) ;
#99908 = DIRECTION ( 'NONE',  ( -0.7071067811865486830, -0.7071067811865464625, 0.000000000000000000 ) ) ;
#99909 = AXIS2_PLACEMENT_3D ( 'NONE', #74865, #95145, #140109 ) ;
#99910 = VECTOR ( 'NONE', #75871, 1000.000000000000000 ) ;
#99911 = CARTESIAN_POINT ( 'NONE',  ( 87.26626352523145158, 4.472830434245839371, -4.472830434245838482 ) ) ;
#99912 = ORIENTED_EDGE ( 'NONE', *, *, #1454, .F. ) ;
#99913 = EDGE_CURVE ( 'NONE', #61971, #48649, #93184, .T. ) ;
#99914 = PLANE ( 'NONE',  #85977 ) ;
#99915 = VECTOR ( 'NONE', #38173, 1000.000000000000000 ) ;
#99916 = VECTOR ( 'NONE', #20869, 1000.000000000000000 ) ;
#99917 = DIRECTION ( 'NONE',  ( 1.000000000000000000, 0.000000000000000000, 0.000000000000000000 ) ) ;
#99918 = CIRCLE ( 'NONE', #28096, 5.968999999999998529 ) ;
#99919 =( GEOMETRIC_REPRESENTATION_CONTEXT ( 3 ) GLOBAL_UNCERTAINTY_ASSIGNED_CONTEXT ( ( #67965 ) ) GLOBAL_UNIT_ASSIGNED_CONTEXT ( ( #30207, #85287, #28804 ) ) REPRESENTATION_CONTEXT ( 'NONE', 'WORKASPACE' ) );
#99920 = ORIENTED_EDGE ( 'NONE', *, *, #7766, .F. ) ;
#99921 = ORIENTED_EDGE ( 'NONE', *, *, #118964, .F. ) ;
#99922 = EDGE_CURVE ( 'NONE', #74191, #107568, #27926, .T. ) ;
#99923 = ORIENTED_EDGE ( 'NONE', *, *, #107056, .F. ) ;
#99924 = DIRECTION ( 'NONE',  ( -0.7071067811865486830, 0.7071067811865464625, 0.000000000000000000 ) ) ;
#99925 = EDGE_CURVE ( 'NONE', #80487, #131140, #73581, .T. ) ;
#99926 = DIRECTION ( 'NONE',  ( 0.6830127018922181881, 0.6830127018922202975, -0.2588190451025214056 ) ) ;
#99927 = CARTESIAN_POINT ( 'NONE',  ( 17.71290314143521982, 3.967499999999992699, -6.871911579029513994 ) ) ;
#99928 = CARTESIAN_POINT ( 'NONE',  ( 36.48921356237310221, -27.52281430457080802, 5.000000000000000000 ) ) ;
#99929 = VECTOR ( 'NONE', #23578, 1000.000000000000000 ) ;
#99930 = CARTESIAN_POINT ( 'NONE',  ( 165.4899822245387782, 26.96999999999994202, 33.83144603466802636 ) ) ;
#99931 = PLANE ( 'NONE',  #44183 ) ;
#99932 = LINE ( 'NONE', #124540, #84457 ) ;
#99933 = EDGE_CURVE ( 'NONE', #51489, #134381, #94593, .T. ) ;
#99934 = ORIENTED_EDGE ( 'NONE', *, *, #32853, .F. ) ;
#99936 = EDGE_LOOP ( 'NONE', ( #64051, #74628, #108804, #101872 ) ) ;
#99935 = EDGE_CURVE ( 'NONE', #45624, #16581, #126508, .T. ) ;
#99937 = DIRECTION ( 'NONE',  ( -0.3543493200069162685, -0.000000000000000000, -0.9351131265310288487 ) ) ;
#99938 = ORIENTED_EDGE ( 'NONE', *, *, #16984, .T. ) ;
#99939 = ORIENTED_EDGE ( 'NONE', *, *, #130876, .T. ) ;
#99940 = EDGE_CURVE ( 'NONE', #24642, #60272, #106165, .T. ) ;
#99941 = AXIS2_PLACEMENT_3D ( 'NONE', #122566, #20390, #99370 ) ;
#99942 = AXIS2_PLACEMENT_3D ( 'NONE', #79476, #135257, #37351 ) ;
#99943 = LINE ( 'NONE', #107921, #49802 ) ;
#99944 = EDGE_LOOP ( 'NONE', ( #30604, #80721, #43691, #66249, #113160, #132400 ) ) ;
#99945 = CARTESIAN_POINT ( 'NONE',  ( 55.78752705046288440, 0.000000000000000000, -7.949999999999998401 ) ) ;
#99946 = LINE ( 'NONE', #69481, #63414 ) ;
#99947 = VECTOR ( 'NONE', #139417, 999.9999999999998863 ) ;
#99948 = PLANE ( 'NONE',  #114964 ) ;
#99949 = CARTESIAN_POINT ( 'NONE',  ( 51.48921356237309510, -27.52281430457091460, 5.000000000000000000 ) ) ;
#99950 = VECTOR ( 'NONE', #37863, 1000.000000000000000 ) ;
#99951 = CARTESIAN_POINT ( 'NONE',  ( 118.6874999999999716, -5.819803920172573974, 5.819803920172573086 ) ) ;
#99952 = ORIENTED_EDGE ( 'NONE', *, *, #39080, .F. ) ;
#99953 = CARTESIAN_POINT ( 'NONE',  ( 11.99999999999992006, -6.033600742197674727, 5.000000000000000000 ) ) ;
#99954 = ORIENTED_EDGE ( 'NONE', *, *, #32331, .F. ) ;
#99955 = CARTESIAN_POINT ( 'NONE',  ( -27.48921356237309155, -27.52281430457074762, 5.000000000000000000 ) ) ;
#99956 = ORIENTED_EDGE ( 'NONE', *, *, #10481, .T. ) ;
#99957 = DIRECTION ( 'NONE',  ( 0.000000000000000000, -1.000000000000000000, 0.000000000000000000 ) ) ;
#99958 = VERTEX_POINT ( 'NONE', #104771 ) ;
#99959 = CARTESIAN_POINT ( 'NONE',  ( 19.82816939922340538, 21.75929247661549937, 4.000000000000000000 ) ) ;
#99960 = EDGE_LOOP ( 'NONE', ( #141048, #122285, #107988, #13251 ) ) ;
#99961 = ORIENTED_EDGE ( 'NONE', *, *, #119403, .T. ) ;
#99962 = VECTOR ( 'NONE', #128657, 1000.000000000000000 ) ;
#99963 = EDGE_LOOP ( 'NONE', ( #76026, #72925, #10058, #24202, #3002 ) ) ;
#99964 = DIRECTION ( 'NONE',  ( 0.7071067811865487940, 0.7071067811865463515, 0.000000000000000000 ) ) ;
#99965 = EDGE_CURVE ( 'NONE', #10004, #85083, #65404, .T. ) ;
#99966 =( NAMED_UNIT ( * ) PLANE_ANGLE_UNIT ( ) SI_UNIT ( $, .RADIAN. ) );
#99967 = DIRECTION ( 'NONE',  ( 0.7071067811865487940, -0.7071067811865463515, 0.000000000000000000 ) ) ;
#99968 = SURFACE_STYLE_FILL_AREA ( #97820 ) ;
#99969 = CARTESIAN_POINT ( 'NONE',  ( -36.48921356237310221, -27.52281430457080802, 5.000000000000000000 ) ) ;
#99970 = ADVANCED_FACE ( 'NONE', ( #39540 ), #72912, .F. ) ;
#99971 = DIRECTION ( 'NONE',  ( -0.6830127018922180770, -0.6830127018922204085, -0.2588190451025213501 ) ) ;
#99973 = CARTESIAN_POINT ( 'NONE',  ( 0.000000000000000000, 0.000000000000000000, 5.000000000000000000 ) ) ;
#99972 = AXIS2_PLACEMENT_3D ( 'NONE', #108599, #9279, #120936 ) ;
#99974 = VECTOR ( 'NONE', #127684, 1000.000000000000000 ) ;
#99975 = FACE_OUTER_BOUND ( 'NONE', #51768, .T. ) ;
#99976 = EDGE_CURVE ( 'NONE', #142084, #28403, #9725, .T. ) ;
#99977 = ADVANCED_FACE ( 'NONE', ( #42403 ), #130839, .F. ) ;
#99978 =( NAMED_UNIT ( * ) PLANE_ANGLE_UNIT ( ) SI_UNIT ( $, .RADIAN. ) );
#99979 = ORIENTED_EDGE ( 'NONE', *, *, #54793, .F. ) ;
#99980 = DIRECTION ( 'NONE',  ( -0.6830127018922181881, 0.6830127018922202975, -0.2588190451025214056 ) ) ;
#99981 = CARTESIAN_POINT ( 'NONE',  ( 152.4000000000000057, -16.48000000000005016, -33.92499999999998295 ) ) ;
#99982 = VERTEX_POINT ( 'NONE', #141700 ) ;
#99983 = ORIENTED_EDGE ( 'NONE', *, *, #112457, .F. ) ;
#99984 = ORIENTED_EDGE ( 'NONE', *, *, #72580, .T. ) ;
#99985 = AXIS2_PLACEMENT_3D ( 'NONE', #138713, #83632, #27068 ) ;
#99986 = DIRECTION ( 'NONE',  ( 0.7071067811865487940, 0.7071067811865463515, 0.000000000000000000 ) ) ;
#99987 = ORIENTED_EDGE ( 'NONE', *, *, #84884, .T. ) ;
#99988 =( BOUNDED_CURVE ( )  B_SPLINE_CURVE ( 3, ( #139828, #41183, #19439, #28898 ),
 .UNSPECIFIED., .F., .T. ) 
 B_SPLINE_CURVE_WITH_KNOTS ( ( 4, 4 ),
 ( 4.712388980384689674, 6.283185307179586232 ),
 .UNSPECIFIED. ) 
 CURVE ( )  GEOMETRIC_REPRESENTATION_ITEM ( )  RATIONAL_B_SPLINE_CURVE ( ( 1.000000000000000000, 0.8047378541243649375, 0.8047378541243649375, 1.000000000000000000 ) ) 
 REPRESENTATION_ITEM ( '' )  );
#99989 = EDGE_LOOP ( 'NONE', ( #64506, #50536, #14567, #47655, #86803 ) ) ;
#99990 = DIRECTION ( 'NONE',  ( -0.000000000000000000, 0.3543493200069153248, 0.9351131265310292928 ) ) ;
#99991 = DIRECTION ( 'NONE',  ( -0.7071067811865487940, 0.7071067811865463515, -0.000000000000000000 ) ) ;
#99992 = DIRECTION ( 'NONE',  ( 0.6830127018922180770, -0.6830127018922204085, -0.2588190451025213501 ) ) ;
#99993 = EDGE_CURVE ( 'NONE', #71933, #30765, #119896, .T. ) ;
#99994 = FACE_OUTER_BOUND ( 'NONE', #29344, .T. ) ;
#99995 = EDGE_CURVE ( 'NONE', #91707, #78330, #77179, .T. ) ;
#99996 = PLANE ( 'NONE',  #39508 ) ;
#99997 = VERTEX_POINT ( 'NONE', #110455 ) ;
#99998 = LINE ( 'NONE', #42778, #39472 ) ;
#99999 = VECTOR ( 'NONE', #123245, 1000.000000000000000 ) ;
#100000 = ORIENTED_EDGE ( 'NONE', *, *, #115359, .T. ) ;
#100001 =( NAMED_UNIT ( * ) PLANE_ANGLE_UNIT ( ) SI_UNIT ( $, .RADIAN. ) );
#100002 = CARTESIAN_POINT ( 'NONE',  ( 19.90040314143521982, -7.934999999999989839, 2.126176841940957907 ) ) ;
#100003 = ORIENTED_EDGE ( 'NONE', *, *, #18077, .T. ) ;
#100004 = CARTESIAN_POINT ( 'NONE',  ( 84.34959685856478018, 6.109999999999997655, 1.637169565754163836 ) ) ;
#100005 = EDGE_CURVE ( 'NONE', #106633, #58061, #23786, .T. ) ;
#100006 = FACE_OUTER_BOUND ( 'NONE', #19764, .T. ) ;
#100007 = LINE ( 'NONE', #44961, #51176 ) ;
#100008 = ORIENTED_EDGE ( 'NONE', *, *, #132939, .F. ) ;
#100009 = VERTEX_POINT ( 'NONE', #31502 ) ;
#100010 = VERTEX_POINT ( 'NONE', #142418 ) ;
#100011 = CARTESIAN_POINT ( 'NONE',  ( 39.48921356237310221, -27.52281430457082934, 5.000000000000000000 ) ) ;
#100012 = PLANE ( 'NONE',  #74161 ) ;
#100013 = DIRECTION ( 'NONE',  ( -0.6830127018922181881, 0.6830127018922202975, -0.2588190451025214056 ) ) ;
#100016 = ADVANCED_FACE ( 'NONE', ( #109767 ), #75724, .F. ) ;
#100015 = CARTESIAN_POINT ( 'NONE',  ( 17.00344868374274299, -0.9023935745793740804, -35.76208109637431676 ) ) ;
#100014 = VECTOR ( 'NONE', #41521, 999.9999999999998863 ) ;
#100018 = DIRECTION ( 'NONE',  ( 0.7071067811865487940, 0.7071067811865463515, 0.000000000000000000 ) ) ;
#100017 = VECTOR ( 'NONE', #111010, 1000.000000000000000 ) ;
#100019 = CARTESIAN_POINT ( 'NONE',  ( 54.29974487139159578, -27.71228299555243879, 4.000000000000000000 ) ) ;
#100020 = VERTEX_POINT ( 'NONE', #98874 ) ;
#100021 = VECTOR ( 'NONE', #115800, 999.9999999999998863 ) ;
#100022 = CYLINDRICAL_SURFACE ( 'NONE', #10944, 1.000000000000000888 ) ;
#100023 = VECTOR ( 'NONE', #32008, 1000.000000000000000 ) ;
#100024 = CARTESIAN_POINT ( 'NONE',  ( -20.29289321881331531, -12.74070752338415602, 5.000000000000000000 ) ) ;
#100025 = CARTESIAN_POINT ( 'NONE',  ( 8.111591955682463606, 4.202752102959690472E-16, 0.000000000000000000 ) ) ;
#100026 = ORIENTED_EDGE ( 'NONE', *, *, #85392, .T. ) ;
#100027 = FACE_OUTER_BOUND ( 'NONE', #79156, .T. ) ;
#100028 = VECTOR ( 'NONE', #366, 999.9999999999998863 ) ;
#100029 = EDGE_CURVE ( 'NONE', #33166, #119697, #109036, .T. ) ;
#100030 = AXIS2_PLACEMENT_3D ( 'NONE', #46050, #67821, #100417 ) ;
#100031 =( GEOMETRIC_REPRESENTATION_CONTEXT ( 3 ) GLOBAL_UNCERTAINTY_ASSIGNED_CONTEXT ( ( #66506 ) ) GLOBAL_UNIT_ASSIGNED_CONTEXT ( ( #60554, #27880, #51080 ) ) REPRESENTATION_CONTEXT ( 'NONE', 'WORKASPACE' ) );
#100032 = AXIS2_PLACEMENT_3D ( 'NONE', #35567, #13736, #79070 ) ;
#100033 = DIRECTION ( 'NONE',  ( 0.6830127018922180770, -0.6830127018922204085, -0.2588190451025213501 ) ) ;
#100034 = ORIENTED_EDGE ( 'NONE', *, *, #66495, .F. ) ;
#100036 = ORIENTED_EDGE ( 'NONE', *, *, #78179, .F. ) ;
#100035 = CARTESIAN_POINT ( 'NONE',  ( 7.499999999999951150, -20.56887692260760048, 4.000000000000000000 ) ) ;
#100037 = ORIENTED_EDGE ( 'NONE', *, *, #53671, .T. ) ;
#100038 = PLANE ( 'NONE',  #102570 ) ;
#100039 = DIRECTION ( 'NONE',  ( 0.7071067811865487940, 0.7071067811865463515, -0.000000000000000000 ) ) ;
#100040 = VERTEX_POINT ( 'NONE', #132272 ) ;
#100041 = FACE_OUTER_BOUND ( 'NONE', #94663, .T. ) ;
#100042 = CARTESIAN_POINT ( 'NONE',  ( 15.48921356237309510, -27.52281430457066236, 5.000000000000000000 ) ) ;
#100043 = ADVANCED_FACE ( 'NONE', ( #32961 ), #140263, .T. ) ;
#100044 = CARTESIAN_POINT ( 'NONE',  ( 27.18398860626900060, 28.73617430169806042, 5.000000000000000000 ) ) ;
#100045 = DIRECTION ( 'NONE',  ( -0.000000000000000000, 0.000000000000000000, 1.000000000000000000 ) ) ;
#100046 = DIRECTION ( 'NONE',  ( 0.7071067811865487940, -0.7071067811865463515, 0.000000000000000000 ) ) ;
#100047 = DIRECTION ( 'NONE',  ( 0.7071067811865487940, -0.7071067811865463515, 0.000000000000000000 ) ) ;
#100048 = CARTESIAN_POINT ( 'NONE',  ( 7.748455871324196664, -11.24070752338417201, 10.39518518046007145 ) ) ;
#100049 = DIRECTION ( 'NONE',  ( -0.7071067811865487940, 0.7071067811865463515, 0.000000000000000000 ) ) ;
#100050 = CARTESIAN_POINT ( 'NONE',  ( 21.70790314143522082, -6.871911579029513106, -3.967499999999993587 ) ) ;
#100051 = CARTESIAN_POINT ( 'NONE',  ( 39.48921356237310221, -27.52281430457082934, 5.000000000000000000 ) ) ;
#100052 = CARTESIAN_POINT ( 'NONE',  ( -13.49999999999991473, 1.030536316426498233, -5.498701923753769094 ) ) ;
#100053 = EDGE_CURVE ( 'NONE', #102312, #536, #74302, .T. ) ;
#100054 = PLANE ( 'NONE',  #67376 ) ;
#100055 = DIRECTION ( 'NONE',  ( -0.000000000000000000, -0.3543493200069152693, 0.9351131265310292928 ) ) ;
#100056 = VERTEX_POINT ( 'NONE', #30807 ) ;
#100057 = VECTOR ( 'NONE', #14365, 1000.000000000000000 ) ;
#100058 = ORIENTED_EDGE ( 'NONE', *, *, #61229, .T. ) ;
#100059 = CARTESIAN_POINT ( 'NONE',  ( 101.6250000000000000, -7.950000000000000178, -4.867971026610729436E-16 ) ) ;
#100060 = AXIS2_PLACEMENT_3D ( 'NONE', #24681, #80520, #58077 ) ;
#100061 = ORIENTED_EDGE ( 'NONE', *, *, #57061, .F. ) ;
#100062 = ORIENTED_EDGE ( 'NONE', *, *, #5836, .F. ) ;
#100063 = ORIENTED_EDGE ( 'NONE', *, *, #95639, .F. ) ;
#100064 = CARTESIAN_POINT ( 'NONE',  ( 26.75159235450331963, -3.851859888774471706E-31, 2.500000000000001332 ) ) ;
#100065 = CARTESIAN_POINT ( 'NONE',  ( 23.99999999999983302, 10.55218569542905982, 5.000000000000000000 ) ) ;
#100066 = VECTOR ( 'NONE', #93478, 1000.000000000000000 ) ;
#100067 = VERTEX_POINT ( 'NONE', #52524 ) ;
#100068 = DIRECTION ( 'NONE',  ( 0.3543493200069162685, -0.000000000000000000, -0.9351131265310288487 ) ) ;
#100069 = LINE ( 'NONE', #55136, #90462 ) ;
#100070 = LINE ( 'NONE', #41385, #132133 ) ;
#100071 = DIRECTION ( 'NONE',  ( -0.6830127018922181881, 0.6830127018922202975, -0.2588190451025214056 ) ) ;
#100072 = EDGE_LOOP ( 'NONE', ( #81377, #89764, #120379, #133548 ) ) ;
#100073 = DIRECTION ( 'NONE',  ( 0.7071067811865487940, 0.7071067811865463515, 0.000000000000000000 ) ) ;
#100074 = CARTESIAN_POINT ( 'NONE',  ( 0.000000000000000000, 0.000000000000000000, 5.000000000000000000 ) ) ;
#100076 = VECTOR ( 'NONE', #111736, 1000.000000000000000 ) ;
#100075 = CARTESIAN_POINT ( 'NONE',  ( 16.17183060077635659, -17.24070752338410628, 4.000000000000000000 ) ) ;
#100077 = PLANE ( 'NONE',  #90907 ) ;
#100078 = CARTESIAN_POINT ( 'NONE',  ( -45.48921356237309510, -27.52281430457087197, 5.000000000000000000 ) ) ;
#100079 = CARTESIAN_POINT ( 'NONE',  ( 85.82919371712955581, -3.975000000000001865, 6.884901960086284411 ) ) ;
#100080 = DIRECTION ( 'NONE',  ( 0.7071067811865487940, 0.7071067811865463515, 0.000000000000000000 ) ) ;
#100081 = ORIENTED_EDGE ( 'NONE', *, *, #32387, .F. ) ;
#100082 = ORIENTED_EDGE ( 'NONE', *, *, #102902, .T. ) ;
#100083 = CARTESIAN_POINT ( 'NONE',  ( 116.9587635252314470, 0.000000000000000000, -6.110000000000001208 ) ) ;
#100084 = ORIENTED_EDGE ( 'NONE', *, *, #24904, .T. ) ;
#100085 = ADVANCED_FACE ( 'NONE', ( #41652 ), #102452, .T. ) ;
#100086 = VECTOR ( 'NONE', #43939, 999.9999999999998863 ) ;
#100087 = CARTESIAN_POINT ( 'NONE',  ( -34.49999999999976552, 1.030536316426473809, -5.498701923753725573 ) ) ;
#100088 = AXIS2_PLACEMENT_3D ( 'NONE', #135537, #60121, #127494 ) ;
#100089 = CARTESIAN_POINT ( 'NONE',  ( 26.30673006690384952, -3.740707523384244837, 12.88036043432861533 ) ) ;
#100090 = LINE ( 'NONE', #121807, #134665 ) ;
#100091 = CARTESIAN_POINT ( 'NONE',  ( 109.7245968585647660, -1.637169565754160949, 6.109999999999997655 ) ) ;
#100092 = VERTEX_POINT ( 'NONE', #135633 ) ;
#100093 = ORIENTED_EDGE ( 'NONE', *, *, #128438, .T. ) ;
#100094 = AXIS2_PLACEMENT_3D ( 'NONE', #76870, #23126, #66684 ) ;
#100095 = CARTESIAN_POINT ( 'NONE',  ( 24.79289321881328689, 15.75929247661555976, 5.000000000000000000 ) ) ;
#100096 = CARTESIAN_POINT ( 'NONE',  ( -3.005480084712505828, 28.92564299267936079, 4.000000000000000000 ) ) ;
#100097 = EDGE_LOOP ( 'NONE', ( #100582, #136336, #92369, #32022 ) ) ;
#100098 = VERTEX_POINT ( 'NONE', #88756 ) ;
#100099 = CARTESIAN_POINT ( 'NONE',  ( 40.25043019189809712, 3.055000000000002824, -5.291415217122919401 ) ) ;
#100100 = EDGE_CURVE ( 'NONE', #97786, #78830, #68967, .T. ) ;
#100101 = ORIENTED_EDGE ( 'NONE', *, *, #135362, .T. ) ;
#100102 = FACE_OUTER_BOUND ( 'NONE', #66300, .T. ) ;
#100103 = CARTESIAN_POINT ( 'NONE',  ( -19.49999999999986500, 13.56627193232213102, -10.57019076586072970 ) ) ;
#100104 = ADVANCED_FACE ( 'NONE', ( #136327 ), #137054, .T. ) ;
#100105 = CARTESIAN_POINT ( 'NONE',  ( -6.299744871391586898, -27.71228299555210484, 4.000000000000000000 ) ) ;
#100106 = VECTOR ( 'NONE', #47345, 999.9999999999998863 ) ;
#100107 = EDGE_CURVE ( 'NONE', #41056, #73002, #58109, .T. ) ;
#100108 = CARTESIAN_POINT ( 'NONE',  ( 31.26626352523144092, 4.472830434245839371, -4.472830434245838482 ) ) ;
#100109 = ORIENTED_EDGE ( 'NONE', *, *, #50804, .F. ) ;
#100110 = ADVANCED_FACE ( 'NONE', ( #37019 ), #92099, .T. ) ;
#100111 = LINE ( 'NONE', #87093, #105704 ) ;
#100112 = ORIENTED_EDGE ( 'NONE', *, *, #34819, .T. ) ;
#100113 = ORIENTED_EDGE ( 'NONE', *, *, #65967, .T. ) ;
#100114 = VECTOR ( 'NONE', #73819, 1000.000000000000000 ) ;
#100115 = CIRCLE ( 'NONE', #141721, 2.055000000000000604 ) ;
#100116 = ORIENTED_EDGE ( 'NONE', *, *, #127291, .F. ) ;
#100117 = VECTOR ( 'NONE', #140559, 1000.000000000000227 ) ;
#100118 = VECTOR ( 'NONE', #111953, 999.9999999999998863 ) ;
#100119 = ADVANCED_FACE ( 'NONE', ( #115985 ), #93552, .F. ) ;
#100120 = DIRECTION ( 'NONE',  ( -0.7071067811865487940, 0.7071067811865463515, -0.000000000000000000 ) ) ;
#100121 = VERTEX_POINT ( 'NONE', #126181 ) ;
#100122 = CARTESIAN_POINT ( 'NONE',  ( 51.18398860626899705, 28.73617430169823095, 5.000000000000000000 ) ) ;
#100124 = DIRECTION ( 'NONE',  ( -0.000000000000000000, 0.000000000000000000, 1.000000000000000000 ) ) ;
#100123 = AXIS2_PLACEMENT_3D ( 'NONE', #47362, #121979, #69807 ) ;
#100125 = CIRCLE ( 'NONE', #86265, 2.500000000000000444 ) ;
#100126 = SURFACE_STYLE_USAGE ( .BOTH. , #112423 ) ;
#100127 = EDGE_CURVE ( 'NONE', #61837, #89365, #132985, .T. ) ;
#100128 = DIRECTION ( 'NONE',  ( -0.3543493200069162685, -0.000000000000000000, -0.9351131265310288487 ) ) ;
#100129 = FACE_BOUND ( 'NONE', #59665, .T. ) ;
#100130 = ORIENTED_EDGE ( 'NONE', *, *, #59651, .F. ) ;
#100131 = CARTESIAN_POINT ( 'NONE',  ( -25.39999999999996305, 0.000000000000000000, 0.000000000000000000 ) ) ;
#100132 = DIRECTION ( 'NONE',  ( 1.000000000000000000, 0.000000000000000000, 0.000000000000000000 ) ) ;
#100133 = DIRECTION ( 'NONE',  ( 0.7071067811865487940, 0.7071067811865463515, 0.000000000000000000 ) ) ;
#100134 = DIRECTION ( 'NONE',  ( -0.7071067811865486830, -0.7071067811865464625, -0.000000000000000000 ) ) ;
#100135 = ORIENTED_EDGE ( 'NONE', *, *, #111734, .T. ) ;
#100136 = DIRECTION ( 'NONE',  ( -0.7071067811865486830, -0.7071067811865464625, 0.000000000000000000 ) ) ;
#100137 = ORIENTED_EDGE ( 'NONE', *, *, #20728, .F. ) ;
#100139 = ORIENTED_EDGE ( 'NONE', *, *, #21378, .T. ) ;
#100138 = ADVANCED_FACE ( 'NONE', ( #33664 ), #80552, .F. ) ;
#100140 = EDGE_CURVE ( 'NONE', #58586, #58453, #71819, .T. ) ;
#100141 = ORIENTED_EDGE ( 'NONE', *, *, #102990, .T. ) ;
#100142 = CARTESIAN_POINT ( 'NONE',  ( 49.64126352523144448, 4.472830434245835818, 4.472830434245840259 ) ) ;
#100143 = VERTEX_POINT ( 'NONE', #114568 ) ;
#100144 = VECTOR ( 'NONE', #95163, 1000.000000000000000 ) ;
#100145 = PLANE ( 'NONE',  #62604 ) ;
#100146 = DIRECTION ( 'NONE',  ( 0.6830127018922181881, 0.6830127018922202975, -0.2588190451025214056 ) ) ;
#100147 = EDGE_CURVE ( 'NONE', #58174, #81446, #26854, .T. ) ;
#100148 = ORIENTED_EDGE ( 'NONE', *, *, #3995, .F. ) ;
#100149 = DIRECTION ( 'NONE',  ( 0.7071067811865487940, 0.7071067811865463515, 0.000000000000000000 ) ) ;
#100150 = FACE_OUTER_BOUND ( 'NONE', #49549, .T. ) ;
#100151 = VECTOR ( 'NONE', #41293, 1000.000000000000000 ) ;
#100152 = EDGE_CURVE ( 'NONE', #55245, #79341, #16691, .T. ) ;
#100153 = EDGE_CURVE ( 'NONE', #119622, #38956, #115245, .T. ) ;
#100154 = DIRECTION ( 'NONE',  ( 0.7071067811865486830, -0.7071067811865464625, -0.000000000000000000 ) ) ;
#100155 = PLANE ( 'NONE',  #115647 ) ;
#100156 = FACE_OUTER_BOUND ( 'NONE', #67452, .T. ) ;
#100157 = VECTOR ( 'NONE', #10635, 1000.000000000000000 ) ;
#100158 = PLANE ( 'NONE',  #63311 ) ;
#100159 = SURFACE_STYLE_USAGE ( .BOTH. , #71636 ) ;
#100160 = VERTEX_POINT ( 'NONE', #137783 ) ;
#100161 = ORIENTED_EDGE ( 'NONE', *, *, #110082, .F. ) ;
#100162 = ORIENTED_EDGE ( 'NONE', *, *, #143524, .T. ) ;
#100163 = EDGE_LOOP ( 'NONE', ( #72644, #25334, #79076, #66990 ) ) ;
#100164 = VECTOR ( 'NONE', #76923, 1000.000000000000000 ) ;
#100165 = FACE_OUTER_BOUND ( 'NONE', #31035, .T. ) ;
#100166 = CARTESIAN_POINT ( 'NONE',  ( 36.39169371712955581, 2.130196079827421762, 7.950000000000000178 ) ) ;
#100167 = ORIENTED_EDGE ( 'NONE', *, *, #128286, .T. ) ;
#100168 = EDGE_CURVE ( 'NONE', #59322, #100356, #83394, .T. ) ;
#100169 = VERTEX_POINT ( 'NONE', #95677 ) ;
#100170 = FACE_OUTER_BOUND ( 'NONE', #55720, .T. ) ;
#100171 = PLANE ( 'NONE',  #101205 ) ;
#100172 = ADVANCED_FACE ( 'NONE', ( #97061 ), #73937, .F. ) ;
#100173 = CARTESIAN_POINT ( 'NONE',  ( -17.99999999999986144, 20.58746187583903620, 4.000000000000000000 ) ) ;
#100174 = ORIENTED_EDGE ( 'NONE', *, *, #28660, .T. ) ;
#100175 = FACE_OUTER_BOUND ( 'NONE', #14414, .T. ) ;
#100176 = DIRECTION ( 'NONE',  ( -0.7071067811865486830, -0.7071067811865464625, 0.000000000000000000 ) ) ;
#100177 = CARTESIAN_POINT ( 'NONE',  ( 27.33790314143521982, -6.871911579029513106, -3.967499999999993587 ) ) ;
#100178 = DIRECTION ( 'NONE',  ( -0.000000000000000000, -0.3543493200069152693, 0.9351131265310292928 ) ) ;
#100179 = VERTEX_POINT ( 'NONE', #130478 ) ;
#100180 = CARTESIAN_POINT ( 'NONE',  ( 109.7245968585647660, -1.637169565754161171, 6.109999999999998543 ) ) ;
#100181 = EDGE_CURVE ( 'NONE', #74923, #36339, #31164, .T. ) ;
#100182 = LINE ( 'NONE', #63980, #104457 ) ;
#100183 = AXIS2_PLACEMENT_3D ( 'NONE', #100495, #3288, #59160 ) ;
#100184 = LINE ( 'NONE', #34934, #51946 ) ;
#100186 = ORIENTED_EDGE ( 'NONE', *, *, #31862, .T. ) ;
#100185 = DIRECTION ( 'NONE',  ( 0.7071067811865487940, -0.7071067811865463515, 0.000000000000000000 ) ) ;
#100188 = VECTOR ( 'NONE', #3379, 1000.000000000000000 ) ;
#100187 = CARTESIAN_POINT ( 'NONE',  ( 39.48921356237310221, -27.52281430457082934, 5.000000000000000000 ) ) ;
#100189 = EDGE_LOOP ( 'NONE', ( #125410, #74629, #119173, #44777 ) ) ;
#100190 = CARTESIAN_POINT ( 'NONE',  ( -24.48921356237309510, -27.52281430457072631, 5.000000000000000000 ) ) ;
#100191 = EDGE_CURVE ( 'NONE', #40356, #123762, #107264, .T. ) ;
#100192 = CARTESIAN_POINT ( 'NONE',  ( 2.207106781186533251, 18.75929247661552424, 5.000000000000000000 ) ) ;
#100193 = DIRECTION ( 'NONE',  ( -0.000000000000000000, 0.3543493200069153248, 0.9351131265310292928 ) ) ;
#100194 = ORIENTED_EDGE ( 'NONE', *, *, #62605, .T. ) ;
#100195 = CARTESIAN_POINT ( 'NONE',  ( 26.68342038867194432, -6.740707523384216415, 11.88629033278118108 ) ) ;
#100196 = DIRECTION ( 'NONE',  ( -0.000000000000000000, -0.3543493200069152693, 0.9351131265310292928 ) ) ;
#100197 = DIRECTION ( 'NONE',  ( -0.000000000000000000, -0.000000000000000000, 1.000000000000000000 ) ) ;
#100198 = ORIENTED_EDGE ( 'NONE', *, *, #40086, .T. ) ;
#100199 = VECTOR ( 'NONE', #54304, 1000.000000000000227 ) ;
#100200 = LINE ( 'NONE', #847, #77058 ) ;
#100201 = ORIENTED_EDGE ( 'NONE', *, *, #77580, .F. ) ;
#100202 = CARTESIAN_POINT ( 'NONE',  ( 7.251592354503322291, -5.777789833161707559E-31, 2.500000000000001332 ) ) ;
#100204 = ORIENTED_EDGE ( 'NONE', *, *, #124972, .F. ) ;
#100203 = CYLINDRICAL_SURFACE ( 'NONE', #143473, 0.5000000000000004441 ) ;
#100205 = ORIENTED_EDGE ( 'NONE', *, *, #107001, .F. ) ;
#100206 = STYLED_ITEM ( 'NONE', ( #54286 ), #78835 ) ;
#100207 = DIRECTION ( 'NONE',  ( -0.000000000000000000, 0.000000000000000000, 1.000000000000000000 ) ) ;
#100208 = DIRECTION ( 'NONE',  ( -4.681814790819591790E-17, -0.3543493200069152693, 0.9351131265310292928 ) ) ;
#100209 = ORIENTED_EDGE ( 'NONE', *, *, #124152, .F. ) ;
#100210 = DIRECTION ( 'NONE',  ( 0.3543493200069162685, -0.000000000000000000, -0.9351131265310288487 ) ) ;
#100211 = CARTESIAN_POINT ( 'NONE',  ( -17.33153258840132338, -18.74070752338409207, 20.73178291233837101 ) ) ;
#100212 = CARTESIAN_POINT ( 'NONE',  ( -29.99999999999978684, 4.931123077392138399, 4.000000000000000000 ) ) ;
#100213 = ORIENTED_EDGE ( 'NONE', *, *, #2569, .F. ) ;
#100214 = CARTESIAN_POINT ( 'NONE',  ( 14.99999999999989519, -13.39766691384881803, -10.96608748226469210 ) ) ;
#100215 = DIRECTION ( 'NONE',  ( 1.248002500702738701E-15, 1.000000000000000000, -0.000000000000000000 ) ) ;
#100216 = DIRECTION ( 'NONE',  ( -0.7071067811865487940, 0.7071067811865463515, 0.000000000000000000 ) ) ;
#100217 = VECTOR ( 'NONE', #26906, 1000.000000000000000 ) ;
#100218 = CARTESIAN_POINT ( 'NONE',  ( 28.64126352523144092, 4.472830434245837594, 4.472830434245841147 ) ) ;
#100219 = CARTESIAN_POINT ( 'NONE',  ( 12.51280225271498736, 3.821174125832445049E-16, 0.000000000000000000 ) ) ;
#100220 = AXIS2_PLACEMENT_3D ( 'NONE', #137821, #70459, #15270 ) ;
#100221 = CIRCLE ( 'NONE', #40032, 2.500000000000000888 ) ;
#100222 = VERTEX_POINT ( 'NONE', #8624 ) ;
#100223 = ORIENTED_EDGE ( 'NONE', *, *, #2686, .T. ) ;
#100224 = VERTEX_POINT ( 'NONE', #7939 ) ;
#100225 = VERTEX_POINT ( 'NONE', #85498 ) ;
#100226 = VECTOR ( 'NONE', #56162, 1000.000000000000227 ) ;
#100227 = VECTOR ( 'NONE', #17159, 1000.000000000000000 ) ;
#100228 = CARTESIAN_POINT ( 'NONE',  ( -39.18398860626899705, 28.73617430169814568, 5.000000000000000000 ) ) ;
#100229 = LINE ( 'NONE', #102389, #108696 ) ;
#100230 = ORIENTED_EDGE ( 'NONE', *, *, #83308, .F. ) ;
#100231 = CARTESIAN_POINT ( 'NONE',  ( 26.99451991528749417, 28.92564299267956685, 4.000000000000000000 ) ) ;
#100232 = LINE ( 'NONE', #23361, #92982 ) ;
#100233 = DIRECTION ( 'NONE',  ( 0.7071067811865487940, -0.7071067811865463515, 0.000000000000000000 ) ) ;
#100234 = FACE_OUTER_BOUND ( 'NONE', #70603, .T. ) ;
#100235 = CARTESIAN_POINT ( 'NONE',  ( 125.8545968585647756, -1.637169565754161615, 6.110000000000000320 ) ) ;
#100236 = ORIENTED_EDGE ( 'NONE', *, *, #129485, .F. ) ;
#100237 = DIRECTION ( 'NONE',  ( 0.000000000000000000, 0.000000000000000000, 1.000000000000000000 ) ) ;
#100238 = CARTESIAN_POINT ( 'NONE',  ( 13.99806943317892127, -22.22500000000000142, 4.500000000000000888 ) ) ;
#100239 = DIRECTION ( 'NONE',  ( 0.7071067811865486830, -0.7071067811865464625, -0.000000000000000000 ) ) ;
#100240 = CARTESIAN_POINT ( 'NONE',  ( 0.4678577423086575093, 6.868554027058086042, -3.322579193147489285 ) ) ;
#100241 = CARTESIAN_POINT ( 'NONE',  ( 24.48921356237309510, -27.52281430457072631, 5.000000000000000000 ) ) ;
#100242 = DIRECTION ( 'NONE',  ( -0.7071067811865487940, 0.7071067811865463515, 0.000000000000000000 ) ) ;
#100243 = LINE ( 'NONE', #97345, #45828 ) ;
#100244 = CARTESIAN_POINT ( 'NONE',  ( 49.80836038379622721, 7.949999999999997513, 2.130196079827431088 ) ) ;
#100245 = PLANE ( 'NONE',  #69988 ) ;
#100247 = PLANE ( 'NONE',  #50803 ) ;
#100246 = VECTOR ( 'NONE', #44620, 1000.000000000000000 ) ;
#100248 = ORIENTED_EDGE ( 'NONE', *, *, #142835, .F. ) ;
#100249 = ORIENTED_EDGE ( 'NONE', *, *, #5155, .T. ) ;
#100250 = CARTESIAN_POINT ( 'NONE',  ( 49.41666666666666430, -6.884901960086287076, -3.975000000000000977 ) ) ;
#100251 = CARTESIAN_POINT ( 'NONE',  ( -45.48921356237309510, -27.52281430457087197, 5.000000000000000000 ) ) ;
#100252 = ADVANCED_FACE ( 'NONE', ( #75374 ), #63793, .F. ) ;
#100253 = LINE ( 'NONE', #133605, #108595 ) ;
#100254 = ORIENTED_EDGE ( 'NONE', *, *, #126878, .T. ) ;
#100255 = LINE ( 'NONE', #132183, #52539 ) ;
#100256 = AXIS2_PLACEMENT_3D ( 'NONE', #29525, #30253, #96900 ) ;
#100257 = DIRECTION ( 'NONE',  ( -0.7071067811865486830, -0.7071067811865464625, 0.000000000000000000 ) ) ;
#100258 = CARTESIAN_POINT ( 'NONE',  ( 38.35459685856476852, -1.637169565754161615, 6.110000000000000320 ) ) ;
#100259 = VECTOR ( 'NONE', #59051, 1000.000000000000227 ) ;
#100260 = ORIENTED_EDGE ( 'NONE', *, *, #112708, .T. ) ;
#100261 = SURFACE_STYLE_USAGE ( .BOTH. , #110389 ) ;
#100262 = ORIENTED_EDGE ( 'NONE', *, *, #97993, .T. ) ;
#100263 = EDGE_LOOP ( 'NONE', ( #107970, #33967, #111180, #105870 ) ) ;
#100264 = DIRECTION ( 'NONE',  ( -1.000000000000000000, -1.224606353822377258E-16, -0.000000000000000000 ) ) ;
#100265 = DIRECTION ( 'NONE',  ( 0.7071067811865487940, 0.7071067811865463515, -0.000000000000000000 ) ) ;
#100266 = DIRECTION ( 'NONE',  ( -0.000000000000000000, 0.3543493200069152138, -0.9351131265310292928 ) ) ;
#100267 = EDGE_CURVE ( 'NONE', #3922, #76836, #30437, .T. ) ;
#100268 = CARTESIAN_POINT ( 'NONE',  ( -34.92500000000001137, -22.22500000000000142, 0.4999999999999995559 ) ) ;
#100269 = ORIENTED_EDGE ( 'NONE', *, *, #86501, .F. ) ;
#100270 = DIRECTION ( 'NONE',  ( 0.000000000000000000, -1.000000000000000000, 0.000000000000000000 ) ) ;
#100271 = EDGE_CURVE ( 'NONE', #31963, #94490, #7211, .T. ) ;
#100272 = EDGE_CURVE ( 'NONE', #80339, #5588, #105819, .T. ) ;
#100273 = ORIENTED_EDGE ( 'NONE', *, *, #76639, .F. ) ;
#100274 = LINE ( 'NONE', #46657, #30906 ) ;
#100275 = CYLINDRICAL_SURFACE ( 'NONE', #9142, 6.499999999999999112 ) ;
#100276 = PLANE ( 'NONE',  #22295 ) ;
#100277 = SURFACE_STYLE_FILL_AREA ( #5009 ) ;
#100278 = CARTESIAN_POINT ( 'NONE',  ( -4.828169399223498637, 6.759292476615651246, 4.000000000000000000 ) ) ;
#100279 = SURFACE_SIDE_STYLE ('',( #98827 ) ) ;
#100281 = EDGE_CURVE ( 'NONE', #16142, #15535, #51484, .T. ) ;
#100280 = AXIS2_PLACEMENT_3D ( 'NONE', #102889, #26040, #137667 ) ;
#100282 = EDGE_CURVE ( 'NONE', #42749, #22851, #117408, .T. ) ;
#100283 = VERTEX_POINT ( 'NONE', #60972 ) ;
#100284 = VECTOR ( 'NONE', #77913, 1000.000000000000000 ) ;
#100285 = DIRECTION ( 'NONE',  ( -1.000000000000000000, 0.000000000000000000, 0.000000000000000000 ) ) ;
#100286 = CARTESIAN_POINT ( 'NONE',  ( 54.59959685856476597, -6.109999999999997655, -1.637169565754160283 ) ) ;
#100287 = CARTESIAN_POINT ( 'NONE',  ( 48.78752705046289151, 0.000000000000000000, -7.949999999999998401 ) ) ;
#100288 = ADVANCED_FACE ( 'NONE', ( #139932 ), #40609, .F. ) ;
#100289 = VECTOR ( 'NONE', #17722, 1000.000000000000000 ) ;
#100290 = CARTESIAN_POINT ( 'NONE',  ( 15.18079593298623564, -2.055000000000000160, 0.000000000000000000 ) ) ;
#100291 = CARTESIAN_POINT ( 'NONE',  ( 0.000000000000000000, 0.000000000000000000, 5.000000000000000000 ) ) ;
#100292 = ORIENTED_EDGE ( 'NONE', *, *, #53462, .F. ) ;
#100293 = CIRCLE ( 'NONE', #58640, 2.500000000000000888 ) ;
#100294 = LINE ( 'NONE', #78539, #37696 ) ;
#100295 = ORIENTED_EDGE ( 'NONE', *, *, #110295, .T. ) ;
#100296 = EDGE_CURVE ( 'NONE', #101043, #111265, #28300, .T. ) ;
#100297 = CARTESIAN_POINT ( 'NONE',  ( 20.99999999999986855, 17.58746187583907172, 4.000000000000000000 ) ) ;
#100298 = ORIENTED_EDGE ( 'NONE', *, *, #106570, .T. ) ;
#100299 = DIRECTION ( 'NONE',  ( 0.7071067811865487940, 0.7071067811865463515, 0.000000000000000000 ) ) ;
#100300 = PLANE ( 'NONE',  #31749 ) ;
#100301 = LINE ( 'NONE', #123506, #2179 ) ;
#100302 = VECTOR ( 'NONE', #25482, 1000.000000000000000 ) ;
#100303 = CARTESIAN_POINT ( 'NONE',  ( -7.140000000000001457, -35.69931938766895740, -8.025146269613532723 ) ) ;
#100304 = FACE_BOUND ( 'NONE', #74689, .T. ) ;
#100305 = DIRECTION ( 'NONE',  ( 0.3543493200069162685, -0.000000000000000000, -0.9351131265310288487 ) ) ;
#100306 = DIRECTION ( 'NONE',  ( 0.7071067811865487940, -0.7071067811865463515, 0.000000000000000000 ) ) ;
#100307 = VECTOR ( 'NONE', #61272, 1000.000000000000000 ) ;
#100308 = DIRECTION ( 'NONE',  ( 0.6830127018922180770, -0.6830127018922204085, -0.2588190451025213501 ) ) ;
#100310 = ORIENTED_EDGE ( 'NONE', *, *, #84447, .F. ) ;
#100309 = DIRECTION ( 'NONE',  ( -0.000000000000000000, -0.3543493200069152693, 0.9351131265310292928 ) ) ;
#100311 = EDGE_CURVE ( 'NONE', #43879, #22057, #129732, .T. ) ;
#100312 = CARTESIAN_POINT ( 'NONE',  ( -25.39999999999996305, 3.061616997868383141E-16, -2.500000000000000000 ) ) ;
#100313 = EDGE_LOOP ( 'NONE', ( #2205, #27237, #14532, #15640 ) ) ;
#100314 = ORIENTED_EDGE ( 'NONE', *, *, #82799, .T. ) ;
#100315 = CARTESIAN_POINT ( 'NONE',  ( 74.43293019189810877, 1.637169565754156508, 6.110000000000000320 ) ) ;
#100316 = ORIENTED_EDGE ( 'NONE', *, *, #5223, .T. ) ;
#100317 = CARTESIAN_POINT ( 'NONE',  ( 47.99451991528749062, 28.92564299267971251, 4.000000000000000000 ) ) ;
#100318 = EDGE_CURVE ( 'NONE', #46180, #4087, #127612, .T. ) ;
#100319 = EDGE_LOOP ( 'NONE', ( #97499, #93307, #57086, #17318 ) ) ;
#100320 = DIRECTION ( 'NONE',  ( -0.6830127018922180770, -0.6830127018922204085, -0.2588190451025213501 ) ) ;
#100321 = AXIS2_PLACEMENT_3D ( 'NONE', #15117, #123224, #23893 ) ;
#100322 = AXIS2_PLACEMENT_3D ( 'NONE', #89961, #134214, #57380 ) ;
#100323 = DIRECTION ( 'NONE',  ( -0.7071067811865486830, 0.7071067811865464625, 0.000000000000000000 ) ) ;
#100324 = ADVANCED_FACE ( 'NONE', ( #5788 ), #19547, .F. ) ;
#100325 = CARTESIAN_POINT ( 'NONE',  ( 54.29974487139159578, -27.71228299555243879, 4.000000000000000000 ) ) ;
#100326 = FACE_OUTER_BOUND ( 'NONE', #50216, .T. ) ;
#100327 = DIRECTION ( 'NONE',  ( -0.7071067811865486830, -0.7071067811865464625, 0.000000000000000000 ) ) ;
#100328 = EDGE_CURVE ( 'NONE', #24144, #94048, #116724, .T. ) ;
#100329 = CARTESIAN_POINT ( 'NONE',  ( 9.682526172861077640, 4.202752102959690472E-16, 0.000000000000000000 ) ) ;
#100330 = DIRECTION ( 'NONE',  ( -0.5735764363510507113, 0.8191520442889885789, 1.003171929053520926E-16 ) ) ;
#100331 = ORIENTED_EDGE ( 'NONE', *, *, #129468, .F. ) ;
#100332 = AXIS2_PLACEMENT_3D ( 'NONE', #118256, #53002, #66067 ) ;
#100333 = VERTEX_POINT ( 'NONE', #6480 ) ;
#100334 = FACE_OUTER_BOUND ( 'NONE', #45652, .T. ) ;
#100335 = DIRECTION ( 'NONE',  ( 0.7071067811865487940, 0.7071067811865463515, -0.000000000000000000 ) ) ;
#100336 = VERTEX_POINT ( 'NONE', #139219 ) ;
#100337 = ADVANCED_FACE ( 'NONE', ( #99975 ), #67362, .T. ) ;
#100338 = ORIENTED_EDGE ( 'NONE', *, *, #85433, .T. ) ;
#100339 = ORIENTED_EDGE ( 'NONE', *, *, #5206, .F. ) ;
#100340 = CARTESIAN_POINT ( 'NONE',  ( 25.95876352523143638, 0.000000000000000000, -6.110000000000001208 ) ) ;
#100341 = ORIENTED_EDGE ( 'NONE', *, *, #21727, .F. ) ;
#100342 = CARTESIAN_POINT ( 'NONE',  ( 30.48921356237309510, -27.52281430457076894, 5.000000000000000000 ) ) ;
#100344 = EDGE_CURVE ( 'NONE', #57042, #84048, #89112, .T. ) ;
#100343 = VECTOR ( 'NONE', #7386, 1000.000000000000000 ) ;
#100345 = DIRECTION ( 'NONE',  ( 0.7071067811865486830, -0.7071067811865464625, -0.000000000000000000 ) ) ;
#100346 = VECTOR ( 'NONE', #16763, 1000.000000000000000 ) ;
#100347 = CARTESIAN_POINT ( 'NONE',  ( 31.10830628287042998, 1.633150327867687324, -6.094999999999991758 ) ) ;
#100348 = CARTESIAN_POINT ( 'NONE',  ( 18.92835661504068412, 2.123974822113010585, -30.34497721346233590 ) ) ;
#100349 = ORIENTED_EDGE ( 'NONE', *, *, #1110, .F. ) ;
#100350 = EDGE_CURVE ( 'NONE', #47692, #74087, #89797, .T. ) ;
#100351 = FACE_OUTER_BOUND ( 'NONE', #97451, .T. ) ;
#100352 = DIRECTION ( 'NONE',  ( -0.6830127018922181881, 0.6830127018922202975, -0.2588190451025214056 ) ) ;
#100353 = CARTESIAN_POINT ( 'NONE',  ( -30.32816939922332011, -18.74070752338409562, 4.000000000000000000 ) ) ;
#100355 = EDGE_LOOP ( 'NONE', ( #133381, #47262, #29451, #59398 ) ) ;
#100354 = FACE_OUTER_BOUND ( 'NONE', #101589, .T. ) ;
#100356 = VERTEX_POINT ( 'NONE', #56520 ) ;
#100357 = PLANE ( 'NONE',  #3282 ) ;
#100358 = CARTESIAN_POINT ( 'NONE',  ( -7.140000000000001457, -35.76999999999998892, -7.899272885403731514 ) ) ;
#100359 = VECTOR ( 'NONE', #40286, 1000.000000000000000 ) ;
#100360 = DIRECTION ( 'NONE',  ( -1.000000000000000000, 0.000000000000000000, 0.000000000000000000 ) ) ;
#100361 = ORIENTED_EDGE ( 'NONE', *, *, #129635, .T. ) ;
#100362 = LINE ( 'NONE', #133013, #29641 ) ;
#100363 = CARTESIAN_POINT ( 'NONE',  ( 33.18398860626899705, 28.73617430169810305, 5.000000000000000000 ) ) ;
#100364 = VERTEX_POINT ( 'NONE', #120996 ) ;
#100365 = ADVANCED_FACE ( 'NONE', ( #134039 ), #87667, .F. ) ;
#100366 = VECTOR ( 'NONE', #87341, 1000.000000000000000 ) ;
#100367 = DIRECTION ( 'NONE',  ( 0.7071067811865487940, 0.7071067811865463515, 0.000000000000000000 ) ) ;
#100368 = CARTESIAN_POINT ( 'NONE',  ( 28.56249999999998934, -5.819803920172573086, -5.819803920172573974 ) ) ;
#100369 = CARTESIAN_POINT ( 'NONE',  ( 11.67183060077639567, 5.259292476615665457, 4.000000000000000000 ) ) ;
#100370 = FACE_OUTER_BOUND ( 'NONE', #134737, .T. ) ;
#100371 = CARTESIAN_POINT ( 'NONE',  ( 6.005480084712508493, 28.92564299267933947, 4.000000000000000000 ) ) ;
#100373 = VECTOR ( 'NONE', #20641, 1000.000000000000000 ) ;
#100372 = DIRECTION ( 'NONE',  ( 0.000000000000000000, -1.000000000000000000, 0.000000000000000000 ) ) ;
#100374 = LINE ( 'NONE', #25647, #40171 ) ;
#100375 = EDGE_CURVE ( 'NONE', #37842, #126541, #43452, .T. ) ;
#100376 = CARTESIAN_POINT ( 'NONE',  ( 6.183988606268994381, 28.73617430169791476, 5.000000000000000000 ) ) ;
#100377 = ORIENTED_EDGE ( 'NONE', *, *, #72378, .F. ) ;
#100378 = ORIENTED_EDGE ( 'NONE', *, *, #16557, .F. ) ;
#100379 = CARTESIAN_POINT ( 'NONE',  ( 25.16975813788240046, -6.350000000000002309, -1.701477371937631267 ) ) ;
#100380 = DIRECTION ( 'NONE',  ( -0.7071067811865487940, 0.7071067811865463515, -0.000000000000000000 ) ) ;
#100381 = VECTOR ( 'NONE', #127212, 1000.000000000000000 ) ;
#100382 = FILL_AREA_STYLE ('',( #22075 ) ) ;
#100383 = FACE_OUTER_BOUND ( 'NONE', #38726, .T. ) ;
#100384 = EDGE_CURVE ( 'NONE', #143396, #34958, #44931, .T. ) ;
#100386 = ORIENTED_EDGE ( 'NONE', *, *, #78306, .T. ) ;
#100385 = VECTOR ( 'NONE', #119244, 1000.000000000000000 ) ;
#100387 = PLANE ( 'NONE',  #15947 ) ;
#100388 = PLANE ( 'NONE',  #51093 ) ;
#100389 = CARTESIAN_POINT ( 'NONE',  ( 13.10966639810773948, 3.759292476615678336, 4.164048746910661514 ) ) ;
#100390 = ORIENTED_EDGE ( 'NONE', *, *, #26776, .F. ) ;
#100391 = CARTESIAN_POINT ( 'NONE',  ( 12.70710678118646086, -0.7407075233842770334, 5.000000000000000000 ) ) ;
#100392 = LINE ( 'NONE', #109826, #9434 ) ;
#100393 = FACE_OUTER_BOUND ( 'NONE', #140372, .T. ) ;
#100394 = AXIS2_PLACEMENT_3D ( 'NONE', #22751, #35128, #47457 ) ;
#100395 = DIRECTION ( 'NONE',  ( -0.6830127018922180770, -0.6830127018922204085, -0.2588190451025213501 ) ) ;
#100396 = CARTESIAN_POINT ( 'NONE',  ( 58.39126352523145158, -4.472830434245839371, -4.472830434245839371 ) ) ;
#100398 = EDGE_CURVE ( 'NONE', #38295, #133583, #34018, .T. ) ;
#100397 =( BOUNDED_CURVE ( )  B_SPLINE_CURVE ( 3, ( #133191, #136014, #45476, #59215 ),
 .UNSPECIFIED., .F., .F. ) 
 B_SPLINE_CURVE_WITH_KNOTS ( ( 4, 4 ),
 ( 5.043186909253414285, 5.074607125596365620 ),
 .UNSPECIFIED. ) 
 CURVE ( )  GEOMETRIC_REPRESENTATION_ITEM ( )  RATIONAL_B_SPLINE_CURVE ( ( 1.000000000000000000, 0.9999177325257868620, 0.9999177325257868620, 1.000000000000000000 ) ) 
 REPRESENTATION_ITEM ( '' )  );
#100399 = DIRECTION ( 'NONE',  ( 0.6830127018922181881, 0.6830127018922202975, -0.2588190451025214056 ) ) ;
#100400 = CARTESIAN_POINT ( 'NONE',  ( -31.49999999999977263, 0.05218569542916537407, 5.000000000000000000 ) ) ;
#100401 = EDGE_CURVE ( 'NONE', #86941, #21557, #132615, .T. ) ;
#100402 = DIRECTION ( 'NONE',  ( 0.7071067811865486830, -0.7071067811865464625, -0.000000000000000000 ) ) ;
#100403 = VERTEX_POINT ( 'NONE', #120247 ) ;
#100404 = ORIENTED_EDGE ( 'NONE', *, *, #132894, .T. ) ;
#100405 = AXIS2_PLACEMENT_3D ( 'NONE', #9001, #54032, #32248 ) ;
#100406 = CARTESIAN_POINT ( 'NONE',  ( 11.67183060077638856, -12.74070752338415247, 4.000000000000000000 ) ) ;
#100407 = LINE ( 'NONE', #1050, #41477 ) ;
#100408 = LINE ( 'NONE', #79412, #122998 ) ;
#100409 = CARTESIAN_POINT ( 'NONE',  ( -17.99999999999987210, -6.033600742197671174, 5.000000000000000000 ) ) ;
#100410 = EDGE_CURVE ( 'NONE', #7925, #92630, #93316, .T. ) ;
#100411 = CARTESIAN_POINT ( 'NONE',  ( 106.5375270504628844, -9.735942053221456900E-16, 7.949999999999998401 ) ) ;
#100412 = LINE ( 'NONE', #122132, #89377 ) ;
#100413 = ORIENTED_EDGE ( 'NONE', *, *, #14516, .T. ) ;
#100415 = ORIENTED_EDGE ( 'NONE', *, *, #22440, .T. ) ;
#100414 = STYLED_ITEM ( 'NONE', ( #100974 ), #79637 ) ;
#100416 = CARTESIAN_POINT ( 'NONE',  ( 14.70692117890024697, 4.584330080086930965E-16, 0.000000000000000000 ) ) ;
#100417 = DIRECTION ( 'NONE',  ( 0.000000000000000000, -1.000000000000000000, 0.000000000000000000 ) ) ;
#100418 = DIRECTION ( 'NONE',  ( -1.000000000000000000, -0.000000000000000000, -0.000000000000000000 ) ) ;
#100419 = LINE ( 'NONE', #43899, #108397 ) ;
#100420 = CARTESIAN_POINT ( 'NONE',  ( 71.97502705046289861, -5.819803920172572198, 5.819803920172572198 ) ) ;
#100421 = CARTESIAN_POINT ( 'NONE',  ( 3.250000000000000000, 0.000000000000000000, 0.000000000000000000 ) ) ;
#100422 = VECTOR ( 'NONE', #17235, 1000.000000000000000 ) ;
#100423 = FACE_OUTER_BOUND ( 'NONE', #110415, .T. ) ;
#100424 = ORIENTED_EDGE ( 'NONE', *, *, #132591, .T. ) ;
#100425 = CARTESIAN_POINT ( 'NONE',  ( 75.52083333333332860, 7.949999999999999289, 2.130196079827431532 ) ) ;
#100426 = DIRECTION ( 'NONE',  ( -0.000000000000000000, -0.3543493200069152693, 0.9351131265310292928 ) ) ;
#100427 = DIRECTION ( 'NONE',  ( -0.6830127018922181881, 0.6830127018922202975, -0.2588190451025214056 ) ) ;
#100428 = DIRECTION ( 'NONE',  ( 0.6830127018922180770, -0.6830127018922204085, -0.2588190451025213501 ) ) ;
#100429 = VERTEX_POINT ( 'NONE', #21697 ) ;
#100430 = VECTOR ( 'NONE', #67369, 1000.000000000000000 ) ;
#100431 = CARTESIAN_POINT ( 'NONE',  ( 10.63753812416090483, 22.22500000000000142, 4.000000000000000000 ) ) ;
#100432 = CARTESIAN_POINT ( 'NONE',  ( 68.97959685856477563, 6.109999999999999432, 1.637169565754164280 ) ) ;
#100433 = ORIENTED_EDGE ( 'NONE', *, *, #93674, .T. ) ;
#100434 = EDGE_CURVE ( 'NONE', #35824, #46067, #20965, .T. ) ;
#100435 = ORIENTED_EDGE ( 'NONE', *, *, #84945, .F. ) ;
#100436 = LINE ( 'NONE', #4430, #111448 ) ;
#100437 = CARTESIAN_POINT ( 'NONE',  ( -32.99999999999977263, -0.8619312979532278707, -5.102805207349900840 ) ) ;
#100438 = CARTESIAN_POINT ( 'NONE',  ( 43.43749999999999289, 5.819803920172574863, -5.819803920172573086 ) ) ;
#100439 = DIRECTION ( 'NONE',  ( -0.3543493200069162685, -0.000000000000000000, -0.9351131265310288487 ) ) ;
#100440 = ADVANCED_FACE ( 'NONE', ( #22375 ), #30833, .T. ) ;
#100442 = ORIENTED_EDGE ( 'NONE', *, *, #133595, .T. ) ;
#100441 = DIRECTION ( 'NONE',  ( -0.7071067811865486830, -0.7071067811865464625, 0.000000000000000000 ) ) ;
#100443 = CARTESIAN_POINT ( 'NONE',  ( -0.7071067811865381358, -6.740707523384216415, 5.000000000000000000 ) ) ;
#100444 = PLANE ( 'NONE',  #131006 ) ;
#100445 = CARTESIAN_POINT ( 'NONE',  ( 0.000000000000000000, 21.72500000000000142, 4.500000000000000888 ) ) ;
#100446 = CARTESIAN_POINT ( 'NONE',  ( -34.42500000000001137, 21.72500000000000142, 0.4999999999999995559 ) ) ;
#100447 = ORIENTED_EDGE ( 'NONE', *, *, #60923, .F. ) ;
#100448 = EDGE_CURVE ( 'NONE', #48047, #125864, #34725, .T. ) ;
#100450 = ORIENTED_EDGE ( 'NONE', *, *, #57006, .F. ) ;
#100449 = EDGE_CURVE ( 'NONE', #58745, #64560, #99224, .T. ) ;
#100451 = EDGE_CURVE ( 'NONE', #40957, #96751, #68671, .T. ) ;
#100452 = CARTESIAN_POINT ( 'NONE',  ( 67.66709685856477563, -3.055000000000000160, -5.291415217122921177 ) ) ;
#100453 = COLOUR_RGB ( '', 0.09019608, 0.27058824, 0.51372549) ;
#100454 = ORIENTED_EDGE ( 'NONE', *, *, #124363, .T. ) ;
#100455 = EDGE_CURVE ( 'NONE', #64729, #5522, #64486, .T. ) ;
#100456 = FACE_OUTER_BOUND ( 'NONE', #22491, .T. ) ;
#100457 = LINE ( 'NONE', #78699, #54992 ) ;
#100458 = EDGE_CURVE ( 'NONE', #21974, #94538, #33333, .T. ) ;
#100459 = DIRECTION ( 'NONE',  ( 0.6830127018922181881, 0.6830127018922202975, -0.2588190451025214056 ) ) ;
#100460 = LINE ( 'NONE', #11994, #57133 ) ;
#100461 = VERTEX_POINT ( 'NONE', #10096 ) ;
#100462 = ORIENTED_EDGE ( 'NONE', *, *, #52827, .F. ) ;
#100463 = ADVANCED_FACE ( 'NONE', ( #55773 ), #637, .F. ) ;
#100464 = FACE_OUTER_BOUND ( 'NONE', #114344, .T. ) ;
#100465 = CARTESIAN_POINT ( 'NONE',  ( -17.47596317121671206, -2.821126053013751633, -34.02141742961515547 ) ) ;
#100466 = CIRCLE ( 'NONE', #114313, 2.999999999999999112 ) ;
#100467 = ADVANCED_FACE ( 'NONE', ( #126020 ), #91266, .F. ) ;
#100468 = ORIENTED_EDGE ( 'NONE', *, *, #134840, .T. ) ;
#100469 = AXIS2_PLACEMENT_3D ( 'NONE', #120288, #19585, #41327 ) ;
#100471 = AXIS2_PLACEMENT_3D ( 'NONE', #108963, #9658, #53930 ) ;
#100470 = CARTESIAN_POINT ( 'NONE',  ( 10.32500000000000107, -9.500000000000001776, 4.375000000000001776 ) ) ;
#100472 = DIRECTION ( 'NONE',  ( 0.6830127018922180770, -0.6830127018922204085, -0.2588190451025213501 ) ) ;
#100473 = FACE_OUTER_BOUND ( 'NONE', #139882, .T. ) ;
#100474 = VERTEX_POINT ( 'NONE', #48444 ) ;
#100475 = VECTOR ( 'NONE', #51715, 999.9999999999998863 ) ;
#100476 = EDGE_CURVE ( 'NONE', #69514, #5966, #2788, .T. ) ;
#100477 = VECTOR ( 'NONE', #97272, 1000.000000000000000 ) ;
#100478 = FACE_BOUND ( 'NONE', #71852, .T. ) ;
#100479 = CARTESIAN_POINT ( 'NONE',  ( -10.82816939922345334, 3.759292476615676559, 4.000000000000000000 ) ) ;
#100480 = CARTESIAN_POINT ( 'NONE',  ( 34.92499999999998295, 21.72500000000000142, 4.165035510187005130 ) ) ;
#100481 = CARTESIAN_POINT ( 'NONE',  ( 0.000000000000000000, 0.000000000000000000, 0.000000000000000000 ) ) ;
#100482 = FACE_OUTER_BOUND ( 'NONE', #99898, .T. ) ;
#100483 = ADVANCED_FACE ( 'NONE', ( #36158 ), #104218, .F. ) ;
#100484 = AXIS2_PLACEMENT_3D ( 'NONE', #66634, #76074, #22368 ) ;
#100485 = DIRECTION ( 'NONE',  ( -0.7071067811865487940, 0.7071067811865463515, -0.000000000000000000 ) ) ;
#100486 = DIRECTION ( 'NONE',  ( 1.000000000000000000, 0.000000000000000000, 0.000000000000000000 ) ) ;
#100487 = EDGE_LOOP ( 'NONE', ( #86593, #50574, #28798, #68313 ) ) ;
#100488 = VECTOR ( 'NONE', #4160, 1000.000000000000000 ) ;
#100489 = ORIENTED_EDGE ( 'NONE', *, *, #13089, .T. ) ;
#100490 = CARTESIAN_POINT ( 'NONE',  ( 103.0162635252314374, -4.472830434245838482, 4.472830434245838482 ) ) ;
#100491 = ORIENTED_EDGE ( 'NONE', *, *, #76799, .T. ) ;
#100492 = PLANE ( 'NONE',  #16499 ) ;
#100493 = ORIENTED_EDGE ( 'NONE', *, *, #9965, .T. ) ;
#100494 = VECTOR ( 'NONE', #139659, 1000.000000000000000 ) ;
#100495 = CARTESIAN_POINT ( 'NONE',  ( -14.81601139373099585, 28.73617430169776910, 5.000000000000000000 ) ) ;
#100496 = CARTESIAN_POINT ( 'NONE',  ( 4.274972949537105826, 4.461849672132300881, 4.461849672132299105 ) ) ;
#100497 = DIRECTION ( 'NONE',  ( 0.6830127018922181881, 0.6830127018922202975, -0.2588190451025214056 ) ) ;
#100498 = ORIENTED_EDGE ( 'NONE', *, *, #83296, .T. ) ;
#100499 = CARTESIAN_POINT ( 'NONE',  ( 29.67183060077626067, -9.740707523384182664, 4.000000000000000000 ) ) ;
#100500 = LINE ( 'NONE', #78042, #1465 ) ;
#100501 = LINE ( 'NONE', #135969, #73539 ) ;
#100502 = DIRECTION ( 'NONE',  ( -0.7071067811865487940, 0.7071067811865463515, 0.000000000000000000 ) ) ;
#100503 = EDGE_CURVE ( 'NONE', #14737, #137211, #80388, .T. ) ;
#100504 = LINE ( 'NONE', #130995, #46256 ) ;
#100505 = CONICAL_SURFACE ( 'NONE', #125965, 2.500000000000000888, 0.9599310885968822538 ) ;
#100506 = CARTESIAN_POINT ( 'NONE',  ( -7.499999999999951150, 11.52377502935401843, -1.522421517564068294 ) ) ;
#100507 = ORIENTED_EDGE ( 'NONE', *, *, #94727, .T. ) ;
#100508 = DIRECTION ( 'NONE',  ( 1.000000000000000000, 1.224606353822377258E-16, 0.000000000000000000 ) ) ;
#100509 = EDGE_CURVE ( 'NONE', #76331, #99958, #124579, .T. ) ;
#100510 = DIRECTION ( 'NONE',  ( 0.6830127018922180770, -0.6830127018922204085, -0.2588190451025214056 ) ) ;
#100511 = ORIENTED_EDGE ( 'NONE', *, *, #97822, .T. ) ;
#100512 = ORIENTED_EDGE ( 'NONE', *, *, #39360, .F. ) ;
#100513 = ORIENTED_EDGE ( 'NONE', *, *, #109373, .T. ) ;
#100514 = CARTESIAN_POINT ( 'NONE',  ( 52.79209685856476852, -5.291415217122921177, 3.054999999999999272 ) ) ;
#100515 = ORIENTED_EDGE ( 'NONE', *, *, #120721, .T. ) ;
#100516 = ADVANCED_FACE ( 'NONE', ( #91939 ), #26694, .T. ) ;
#100517 = CYLINDRICAL_SURFACE ( 'NONE', #48951, 0.5000000000000004441 ) ;
#100518 = AXIS2_PLACEMENT_3D ( 'NONE', #1691, #44573, #22043 ) ;
#100519 = CARTESIAN_POINT ( 'NONE',  ( 5.879139616203772789, -5.278424836066145431, -3.047499999999993658 ) ) ;
#100520 = CARTESIAN_POINT ( 'NONE',  ( 92.45876352523144703, 0.000000000000000000, -6.110000000000001208 ) ) ;
#100521 = DIRECTION ( 'NONE',  ( -0.3543493200069162685, -0.000000000000000000, -0.9351131265310288487 ) ) ;
#100522 = EDGE_LOOP ( 'NONE', ( #112186, #93712, #100058, #43892 ) ) ;
#100523 = EDGE_CURVE ( 'NONE', #104775, #70234, #103512, .T. ) ;
#100524 = VERTEX_POINT ( 'NONE', #70250 ) ;
#100525 = CARTESIAN_POINT ( 'NONE',  ( -4.499999999999974243, 6.431123077392122411, 4.000000000000000000 ) ) ;
#100526 = CARTESIAN_POINT ( 'NONE',  ( 24.98480450340313652, 2.536990198832462351, 5.000000000000000000 ) ) ;
#100527 = ORIENTED_EDGE ( 'NONE', *, *, #26036, .T. ) ;
#100528 = AXIS2_PLACEMENT_3D ( 'NONE', #121506, #101190, #137230 ) ;
#100529 = CARTESIAN_POINT ( 'NONE',  ( -22.49999999999984013, -16.53360074219757081, 5.000000000000000000 ) ) ;
#100530 = CARTESIAN_POINT ( 'NONE',  ( 75.29974487139158157, -27.71228299555258445, 4.000000000000000000 ) ) ;
#100531 = ORIENTED_EDGE ( 'NONE', *, *, #81776, .T. ) ;
#100532 = LINE ( 'NONE', #91098, #133775 ) ;
#100533 = EDGE_CURVE ( 'NONE', #11291, #118868, #114410, .T. ) ;
#100534 = ORIENTED_EDGE ( 'NONE', *, *, #67389, .F. ) ;
#100535 = ORIENTED_EDGE ( 'NONE', *, *, #24735, .F. ) ;
#100536 = VERTEX_POINT ( 'NONE', #70936 ) ;
#100537 = PLANE ( 'NONE',  #44770 ) ;
#100538 = PLANE ( 'NONE',  #109359 ) ;
#100539 = ADVANCED_FACE ( 'NONE', ( #13648 ), #81827, .T. ) ;
#100540 = LINE ( 'NONE', #36687, #2285 ) ;
#100541 = CARTESIAN_POINT ( 'NONE',  ( 52.60764783923757193, -49.05583548141699879, 39.86617647058822200 ) ) ;
#100542 = ORIENTED_EDGE ( 'NONE', *, *, #51948, .F. ) ;
#100543 = AXIS2_PLACEMENT_3D ( 'NONE', #112789, #33828, #91072 ) ;
#100544 = CARTESIAN_POINT ( 'NONE',  ( 42.29974487139158157, -27.71228299555235708, 4.000000000000000000 ) ) ;
#100545 = VECTOR ( 'NONE', #65499, 1000.000000000000000 ) ;
#100546 = CARTESIAN_POINT ( 'NONE',  ( 14.41623647476855297, -7.934999999999990727, 4.858786175617117713E-16 ) ) ;
#100547 = ADVANCED_FACE ( 'NONE', ( #123172 ), #38291, .F. ) ;
#100548 = CARTESIAN_POINT ( 'NONE',  ( 10.49999999999993605, -14.94781430457067195, 5.000000000000000000 ) ) ;
#100549 = CARTESIAN_POINT ( 'NONE',  ( 8.700255128608413102, -27.71228299555199825, 4.000000000000000000 ) ) ;
#100550 = ADVANCED_FACE ( 'NONE', ( #93376 ), #36845, .F. ) ;
#100551 =( BOUNDED_CURVE ( )  B_SPLINE_CURVE ( 3, ( #120795, #119350, #108454, #120049 ),
 .UNSPECIFIED., .F., .T. ) 
 B_SPLINE_CURVE_WITH_KNOTS ( ( 4, 4 ),
 ( 3.581556339957213897, 3.677360298529522176 ),
 .UNSPECIFIED. ) 
 CURVE ( )  GEOMETRIC_REPRESENTATION_ITEM ( )  RATIONAL_B_SPLINE_CURVE ( ( 1.000000000000000000, 0.9992352797041761381, 0.9992352797041761381, 1.000000000000000000 ) ) 
 REPRESENTATION_ITEM ( '' )  );
#100552 = DIRECTION ( 'NONE',  ( 0.7071067811865487940, 0.7071067811865463515, 0.000000000000000000 ) ) ;
#100553 = EDGE_LOOP ( 'NONE', ( #94010, #33835, #136661, #44520 ) ) ;
#100554 = VECTOR ( 'NONE', #141044, 1000.000000000000227 ) ;
#100555 = ORIENTED_EDGE ( 'NONE', *, *, #3588, .F. ) ;
#100556 = ORIENTED_EDGE ( 'NONE', *, *, #115652, .F. ) ;
#100557 = CARTESIAN_POINT ( 'NONE',  ( 21.00000000000000000, 0.000000000000000000, 6.094999999999989981 ) ) ;
#100558 = CARTESIAN_POINT ( 'NONE',  ( 57.29166666666665719, 3.975000000000003642, -6.884901960086285300 ) ) ;
#100559 = DIRECTION ( 'NONE',  ( -0.7071067811865486830, -0.7071067811865464625, 0.000000000000000000 ) ) ;
#100561 = ADVANCED_FACE ( 'NONE', ( #37586 ), #115086, .T. ) ;
#100560 = DIRECTION ( 'NONE',  ( -0.6830127018922180770, -0.6830127018922204085, -0.2588190451025213501 ) ) ;
#100562 = DIRECTION ( 'NONE',  ( 0.7071067811865487940, 0.7071067811865463515, -0.000000000000000000 ) ) ;
#100563 = DIRECTION ( 'NONE',  ( -0.7071067811865487940, 0.7071067811865463515, 0.000000000000000000 ) ) ;
#100564 = EDGE_CURVE ( 'NONE', #8692, #58822, #28853, .T. ) ;
#100565 = CIRCLE ( 'NONE', #38071, 4.000000000000000000 ) ;
#100566 = CARTESIAN_POINT ( 'NONE',  ( -14.99451991528749595, 28.92564299267948513, 4.000000000000000000 ) ) ;
#100567 = DIRECTION ( 'NONE',  ( -0.7071067811865486830, -0.7071067811865464625, -0.000000000000000000 ) ) ;
#100568 = CARTESIAN_POINT ( 'NONE',  ( -30.18398860626900060, 28.73617430169808173, 5.000000000000000000 ) ) ;
#100569 = ORIENTED_EDGE ( 'NONE', *, *, #105631, .T. ) ;
#100570 = CARTESIAN_POINT ( 'NONE',  ( -12.69999999999998153, 0.000000000000000000, 0.000000000000000000 ) ) ;
#100571 = ORIENTED_EDGE ( 'NONE', *, *, #25779, .T. ) ;
#100572 = CARTESIAN_POINT ( 'NONE',  ( 17.53166427279083806, -3.156388896525972765, -35.18412642963648551 ) ) ;
#100573 = VERTEX_POINT ( 'NONE', #101392 ) ;
#100574 = CARTESIAN_POINT ( 'NONE',  ( 54.48921356237310221, -27.52281430457093236, 5.000000000000000000 ) ) ;
#100576 = ORIENTED_EDGE ( 'NONE', *, *, #112457, .T. ) ;
#100575 = CARTESIAN_POINT ( 'NONE',  ( 10.49999999999991829, -12.08601207473288675, -10.46905243149096698 ) ) ;
#100577 = AXIS2_PLACEMENT_3D ( 'NONE', #75408, #131206, #31894 ) ;
#100578 = ADVANCED_FACE ( 'NONE', ( #112978 ), #57933, .T. ) ;
#100579 = DIRECTION ( 'NONE',  ( -0.7071067811865486830, -0.7071067811865464625, -0.000000000000000000 ) ) ;
#100580 = ORIENTED_EDGE ( 'NONE', *, *, #125053, .T. ) ;
#100581 = SURFACE_STYLE_FILL_AREA ( #76706 ) ;
#100582 = ORIENTED_EDGE ( 'NONE', *, *, #44682, .T. ) ;
#100583 = DIRECTION ( 'NONE',  ( 0.6830127018922180770, -0.6830127018922204085, -0.2588190451025213501 ) ) ;
#100584 = VERTEX_POINT ( 'NONE', #106355 ) ;
#100585 =( BOUNDED_CURVE ( )  B_SPLINE_CURVE ( 3, ( #9193, #107118, #97677, #143324 ),
 .UNSPECIFIED., .F., .F. ) 
 B_SPLINE_CURVE_WITH_KNOTS ( ( 4, 4 ),
 ( 1.208578181583239486, 1.359146454359484890 ),
 .UNSPECIFIED. ) 
 CURVE ( )  GEOMETRIC_REPRESENTATION_ITEM ( )  RATIONAL_B_SPLINE_CURVE ( ( 1.000000000000000000, 0.9981116584018941973, 0.9981116584018941973, 1.000000000000000000 ) ) 
 REPRESENTATION_ITEM ( '' )  );
#100586 = CIRCLE ( 'NONE', #56646, 2.055000000000001048 ) ;
#100587 = CARTESIAN_POINT ( 'NONE',  ( 28.82816939922333432, -5.240707523384228850, 4.000000000000000000 ) ) ;
#100588 = CARTESIAN_POINT ( 'NONE',  ( 110.3291937171295700, -3.975000000000001865, 6.884901960086284411 ) ) ;
#100590 = VECTOR ( 'NONE', #46742, 1000.000000000000000 ) ;
#100589 = SURFACE_STYLE_FILL_AREA ( #112873 ) ;
#100591 = VECTOR ( 'NONE', #96229, 1000.000000000000000 ) ;
#100592 = FACE_OUTER_BOUND ( 'NONE', #125813, .T. ) ;
#100593 = ORIENTED_EDGE ( 'NONE', *, *, #3055, .F. ) ;
#100594 = CARTESIAN_POINT ( 'NONE',  ( -18.70710678118641113, 14.25929247661557397, 5.000000000000000000 ) ) ;
#100595 = DIRECTION ( 'NONE',  ( -0.000000000000000000, -0.3543493200069152693, 0.9351131265310292928 ) ) ;
#100596 = LINE ( 'NONE', #70145, #99323 ) ;
#100597 = CARTESIAN_POINT ( 'NONE',  ( 14.14583333333333570, -1.633150327867689988, 6.094999999999989981 ) ) ;
#100598 = LINE ( 'NONE', #68692, #7449 ) ;
#100599 = CARTESIAN_POINT ( 'NONE',  ( 11.24139925780195171, 21.72500000000000142, 5.000000000000000000 ) ) ;
#100600 = DIRECTION ( 'NONE',  ( 0.3543493200069163795, -9.265275131829747941E-33, -0.9351131265310288487 ) ) ;
#100601 = ORIENTED_EDGE ( 'NONE', *, *, #65646, .T. ) ;
#100602 = EDGE_LOOP ( 'NONE', ( #140163, #56196, #60951, #68556, #39563 ) ) ;
#100603 = VECTOR ( 'NONE', #37381, 1000.000000000000227 ) ;
#100604 = PLANE ( 'NONE',  #90723 ) ;
#100605 = ORIENTED_EDGE ( 'NONE', *, *, #8448, .T. ) ;
#100606 = CARTESIAN_POINT ( 'NONE',  ( 95.08376352523144703, -6.110000000000001208, -3.741295971395164515E-16 ) ) ;
#100607 = CARTESIAN_POINT ( 'NONE',  ( 24.48921356237309510, -27.52281430457072631, 5.000000000000000000 ) ) ;
#100608 = CARTESIAN_POINT ( 'NONE',  ( 32.99999999999976552, -0.03360074219773898085, 5.000000000000000000 ) ) ;
#100609 = DIRECTION ( 'NONE',  ( 1.192622389734054877E-16, -1.000000000000000000, 0.000000000000000000 ) ) ;
#100610 = LINE ( 'NONE', #34629, #142784 ) ;
#100611 = ORIENTED_EDGE ( 'NONE', *, *, #70273, .F. ) ;
#100612 = DIRECTION ( 'NONE',  ( 1.000000000000000000, 0.000000000000000000, 0.000000000000000000 ) ) ;
#100613 = CARTESIAN_POINT ( 'NONE',  ( 80.99451991528748351, 28.92564299267994699, 4.000000000000000000 ) ) ;
#100614 = CARTESIAN_POINT ( 'NONE',  ( 5.207106781186514155, 3.759292476615676559, 5.000000000000000000 ) ) ;
#100615 = DIRECTION ( 'NONE',  ( -0.7071067811865486830, -0.7071067811865464625, -0.000000000000000000 ) ) ;
#100617 = ORIENTED_EDGE ( 'NONE', *, *, #94692, .F. ) ;
#100616 = LINE ( 'NONE', #22289, #70671 ) ;
#100618 = DIRECTION ( 'NONE',  ( -1.000000000000000000, -0.000000000000000000, -0.000000000000000000 ) ) ;
#100619 = CARTESIAN_POINT ( 'NONE',  ( 0.000000000000000000, 0.000000000000000000, 5.000000000000000000 ) ) ;
#100620 = CARTESIAN_POINT ( 'NONE',  ( -6.183988606268994381, 28.73617430169791476, 5.000000000000000000 ) ) ;
#100621 = DIRECTION ( 'NONE',  ( -0.7071067811865487940, 0.7071067811865463515, -0.000000000000000000 ) ) ;
#100622 = CARTESIAN_POINT ( 'NONE',  ( 19.49999999999985789, -2.777013188829488666, 4.549262955118046570 ) ) ;
#100623 = ORIENTED_EDGE ( 'NONE', *, *, #61229, .F. ) ;
#100624 = VERTEX_POINT ( 'NONE', #52710 ) ;
#100625 = VERTEX_POINT ( 'NONE', #127422 ) ;
#100626 = ADVANCED_FACE ( 'NONE', ( #129560 ), #72389, .F. ) ;
#100627 = CARTESIAN_POINT ( 'NONE',  ( 93.62543019189811844, 5.291415217122919401, 3.055000000000002824 ) ) ;
#100628 = VERTEX_POINT ( 'NONE', #38997 ) ;
#100629 = EDGE_CURVE ( 'NONE', #71583, #122249, #8459, .T. ) ;
#100630 = DIRECTION ( 'NONE',  ( 0.7071067811865486830, -0.7071067811865464625, -0.000000000000000000 ) ) ;
#100631 = CARTESIAN_POINT ( 'NONE',  ( 14.92733143757284786, -1.141545485034857643, 4.000000000000000000 ) ) ;
#100632 = EDGE_CURVE ( 'NONE', #17012, #123516, #40449, .T. ) ;
#100633 = DIRECTION ( 'NONE',  ( -0.6830127018922181881, 0.6830127018922202975, -0.2588190451025214056 ) ) ;
#100634 = DIRECTION ( 'NONE',  ( -0.7071067811865486830, -0.7071067811865464625, 0.000000000000000000 ) ) ;
#100635 = ORIENTED_EDGE ( 'NONE', *, *, #51219, .T. ) ;
#100636 = ADVANCED_FACE ( 'NONE', ( #52020 ), #94779, .F. ) ;
#100637 = DIRECTION ( 'NONE',  ( 0.3543493200069162685, -0.000000000000000000, -0.9351131265310288487 ) ) ;
#100639 = AXIS2_PLACEMENT_3D ( 'NONE', #90706, #134943, #35631 ) ;
#100638 = DIRECTION ( 'NONE',  ( -0.7071067811865487940, 0.7071067811865463515, -0.000000000000000000 ) ) ;
#100640 = CARTESIAN_POINT ( 'NONE',  ( -30.29974487139158867, -27.71228299555227537, 4.000000000000000000 ) ) ;
#100641 = CARTESIAN_POINT ( 'NONE',  ( 85.07876352523143737, -7.482591942790325086E-16, 6.109999999999998543 ) ) ;
#100642 = ORIENTED_EDGE ( 'NONE', *, *, #27887, .T. ) ;
#100643 = CARTESIAN_POINT ( 'NONE',  ( 32.99999999999977263, 4.931123077392136622, 4.000000000000000000 ) ) ;
#100644 = DIRECTION ( 'NONE',  ( -0.6830127018922181881, 0.6830127018922202975, -0.2588190451025214056 ) ) ;
#100645 = EDGE_LOOP ( 'NONE', ( #70826, #17039, #348, #120404 ) ) ;
#100646 = ORIENTED_EDGE ( 'NONE', *, *, #122470, .T. ) ;
#100647 = ADVANCED_FACE ( 'NONE', ( #28842 ), #95503, .F. ) ;
#100648 = DIRECTION ( 'NONE',  ( -0.7071067811865487940, 0.7071067811865463515, 0.000000000000000000 ) ) ;
#100649 = ADVANCED_FACE ( 'NONE', ( #104955 ), #126696, .T. ) ;
#100650 = CARTESIAN_POINT ( 'NONE',  ( -31.49999999999976552, 19.08746187583905041, 4.000000000000000000 ) ) ;
#100651 = CARTESIAN_POINT ( 'NONE',  ( 21.79623647476855552, 7.934999999999990727, -1.457635852685135314E-15 ) ) ;
#100652 = CARTESIAN_POINT ( 'NONE',  ( -28.49999999999980460, 13.46639925780212721, 5.000000000000000000 ) ) ;
#100653 = VECTOR ( 'NONE', #17573, 1000.000000000000000 ) ;
#100654 = LINE ( 'NONE', #77491, #66521 ) ;
#100655 = EDGE_CURVE ( 'NONE', #29435, #26904, #61503, .T. ) ;
#100656 = LINE ( 'NONE', #69467, #99731 ) ;
#100657 = FACE_OUTER_BOUND ( 'NONE', #78363, .T. ) ;
#100658 = VECTOR ( 'NONE', #5713, 1000.000000000000114 ) ;
#100659 = ORIENTED_EDGE ( 'NONE', *, *, #120341, .F. ) ;
#100660 = VERTEX_POINT ( 'NONE', #94076 ) ;
#100661 = VECTOR ( 'NONE', #98956, 999.9999999999998863 ) ;
#100662 = LINE ( 'NONE', #99186, #105805 ) ;
#100663 = ORIENTED_EDGE ( 'NONE', *, *, #108275, .T. ) ;
#100664 = EDGE_LOOP ( 'NONE', ( #96944, #94405, #106562, #84602 ) ) ;
#100665 = ADVANCED_FACE ( 'NONE', ( #19381 ), #49899, .F. ) ;
#100666 = PLANE ( 'NONE',  #42759 ) ;
#100667 = ORIENTED_EDGE ( 'NONE', *, *, #12056, .F. ) ;
#100668 = CARTESIAN_POINT ( 'NONE',  ( -11.99999999999991296, -0.8619312979532105512, -5.102805207349851990 ) ) ;
#100669 = DIRECTION ( 'NONE',  ( -0.7071067811865486830, -0.7071067811865464625, -0.000000000000000000 ) ) ;
#100670 = ADVANCED_FACE ( 'NONE', ( #39736 ), #139031, .F. ) ;
#100671 = CARTESIAN_POINT ( 'NONE',  ( 2.671830600776447628, 14.25929247661557575, 4.000000000000000000 ) ) ;
#100672 = CARTESIAN_POINT ( 'NONE',  ( 0.000000000000000000, 0.000000000000000000, 5.000000000000000000 ) ) ;
#100673 = ORIENTED_EDGE ( 'NONE', *, *, #33505, .F. ) ;
#100674 =( NAMED_UNIT ( * ) SI_UNIT ( $, .STERADIAN. ) SOLID_ANGLE_UNIT ( ) );
#100675 = VERTEX_POINT ( 'NONE', #28123 ) ;
#100676 = CARTESIAN_POINT ( 'NONE',  ( -20.51078643762690490, -27.52281430457041012, 5.000000000000000000 ) ) ;
#100677 = ORIENTED_EDGE ( 'NONE', *, *, #141765, .T. ) ;
#100678 = CARTESIAN_POINT ( 'NONE',  ( 0.000000000000000000, 0.000000000000000000, 5.000000000000000000 ) ) ;
#100679 = EDGE_LOOP ( 'NONE', ( #34039, #129787, #116138, #86926 ) ) ;
#100680 = LINE ( 'NONE', #36830, #64438 ) ;
#100681 = ORIENTED_EDGE ( 'NONE', *, *, #107060, .T. ) ;
#100682 = VERTEX_POINT ( 'NONE', #83221 ) ;
#100683 = VERTEX_POINT ( 'NONE', #16504 ) ;
#100684 = ADVANCED_FACE ( 'NONE', ( #139765 ), #117236, .F. ) ;
#100685 = VECTOR ( 'NONE', #103949, 999.9999999999998863 ) ;
#100686 = CARTESIAN_POINT ( 'NONE',  ( -7.171830600776416986, 15.75929247661555976, 4.000000000000000000 ) ) ;
#100687 = AXIS2_PLACEMENT_3D ( 'NONE', #68997, #67582, #113175 ) ;
#100688 = CARTESIAN_POINT ( 'NONE',  ( 0.4892135623730947680, -27.52281430457055578, 5.000000000000000000 ) ) ;
#100689 = CARTESIAN_POINT ( 'NONE',  ( 0.000000000000000000, -7.600000000000060041, 31.92499999999998295 ) ) ;
#100690 = CARTESIAN_POINT ( 'NONE',  ( 122.7920968585647756, -5.291415217122921177, 3.054999999999999272 ) ) ;
#100691 = DIRECTION ( 'NONE',  ( 0.7071067811865487940, 0.7071067811865463515, 0.000000000000000000 ) ) ;
#100692 = CIRCLE ( 'NONE', #82193, 2.500000000000000888 ) ;
#100693 = EDGE_CURVE ( 'NONE', #58993, #124257, #51629, .T. ) ;
#100694 = DIRECTION ( 'NONE',  ( 0.3543493200069162685, -0.000000000000000000, -0.9351131265310288487 ) ) ;
#100695 = PLANE ( 'NONE',  #31071 ) ;
#100696 = DIRECTION ( 'NONE',  ( -0.000000000000000000, -0.3543493200069152693, 0.9351131265310292928 ) ) ;
#100697 = DIRECTION ( 'NONE',  ( -0.7071067811865487940, 0.7071067811865463515, -0.000000000000000000 ) ) ;
#100698 = VERTEX_POINT ( 'NONE', #107797 ) ;
#100699 = FACE_OUTER_BOUND ( 'NONE', #95275, .T. ) ;
#100700 = CARTESIAN_POINT ( 'NONE',  ( 18.18398860626898994, 28.73617430169800002, 5.000000000000000000 ) ) ;
#100701 = DIRECTION ( 'NONE',  ( -0.6830127018922180770, -0.6830127018922204085, -0.2588190451025214056 ) ) ;
#100702 = EDGE_CURVE ( 'NONE', #75355, #10476, #51312, .T. ) ;
#100703 = ORIENTED_EDGE ( 'NONE', *, *, #136575, .T. ) ;
#100704 = ORIENTED_EDGE ( 'NONE', *, *, #16984, .F. ) ;
#100705 = PLANE ( 'NONE',  #109686 ) ;
#100706 = ORIENTED_EDGE ( 'NONE', *, *, #68404, .F. ) ;
#100707 = ORIENTED_EDGE ( 'NONE', *, *, #29386, .T. ) ;
#100708 = CARTESIAN_POINT ( 'NONE',  ( 48.18398860626899705, 28.73617430169820608, 5.000000000000000000 ) ) ;
#100709 = CARTESIAN_POINT ( 'NONE',  ( -12.18398860626900060, 28.73617430169795739, 5.000000000000000000 ) ) ;
#100710 = DIRECTION ( 'NONE',  ( -0.000000000000000000, 0.3543493200069153248, 0.9351131265310292928 ) ) ;
#100711 = EDGE_CURVE ( 'NONE', #34037, #33763, #42843, .T. ) ;
#100712 = LINE ( 'NONE', #90551, #125054 ) ;
#100713 = FACE_OUTER_BOUND ( 'NONE', #38278, .T. ) ;
#100714 = ORIENTED_EDGE ( 'NONE', *, *, #113823, .F. ) ;
#100715 = FACE_OUTER_BOUND ( 'NONE', #40075, .T. ) ;
#100716 = ORIENTED_EDGE ( 'NONE', *, *, #23726, .T. ) ;
#100717 = CARTESIAN_POINT ( 'NONE',  ( 23.63159235450331863, 9.902892378096218942E-16, 0.000000000000000000 ) ) ;
#100718 = CARTESIAN_POINT ( 'NONE',  ( 21.79623647476855552, 7.934999999999990727, -1.457635852685135314E-15 ) ) ;
#100719 = VERTEX_POINT ( 'NONE', #41131 ) ;
#100720 = CARTESIAN_POINT ( 'NONE',  ( 85.95376352523145158, -6.109999999999999432, -3.741295971395163529E-16 ) ) ;
#100721 = CARTESIAN_POINT ( 'NONE',  ( 9.748460325766547641, -8.447629293701412578, 4.346447159401130023 ) ) ;
#100722 = VERTEX_POINT ( 'NONE', #64322 ) ;
#100723 = ORIENTED_EDGE ( 'NONE', *, *, #118057, .T. ) ;
#100724 = ORIENTED_EDGE ( 'NONE', *, *, #79755, .T. ) ;
#100725 = DIRECTION ( 'NONE',  ( 0.7071067811865487940, 0.7071067811865463515, 0.000000000000000000 ) ) ;
#100726 = PLANE ( 'NONE',  #129601 ) ;
#100727 = CARTESIAN_POINT ( 'NONE',  ( -3.793339364578453665, 21.75929247661549581, 4.998822639870701856 ) ) ;
#100728 = DIRECTION ( 'NONE',  ( -0.000000000000000000, 0.000000000000000000, 1.000000000000000000 ) ) ;
#100729 = EDGE_LOOP ( 'NONE', ( #110361, #96724, #16308, #70494 ) ) ;
#100730 = ADVANCED_FACE ( 'NONE', ( #131722 ), #44002, .F. ) ;
#100731 = CARTESIAN_POINT ( 'NONE',  ( -21.18398860626899349, 28.73617430169802134, 5.000000000000000000 ) ) ;
#100732 = CARTESIAN_POINT ( 'NONE',  ( 0.000000000000000000, 0.000000000000000000, 0.000000000000000000 ) ) ;
#100733 = VERTEX_POINT ( 'NONE', #111370 ) ;
#100734 = CARTESIAN_POINT ( 'NONE',  ( 8.994519915287490619, 28.92564299267944250, 4.000000000000000000 ) ) ;
#100735 = CARTESIAN_POINT ( 'NONE',  ( 8.897059064271770623, -2.055000000000000160, 2.789133085058097101E-16 ) ) ;
#100736 = ORIENTED_EDGE ( 'NONE', *, *, #60935, .T. ) ;
#100737 = ADVANCED_FACE ( 'NONE', ( #88221 ), #67180, .F. ) ;
#100739 = ORIENTED_EDGE ( 'NONE', *, *, #104858, .F. ) ;
#100738 = DIRECTION ( 'NONE',  ( -0.7071067811865486830, -0.7071067811865464625, 0.000000000000000000 ) ) ;
#100740 = ORIENTED_EDGE ( 'NONE', *, *, #51253, .T. ) ;
#100741 = EDGE_CURVE ( 'NONE', #55203, #134557, #20075, .T. ) ;
#100742 = CARTESIAN_POINT ( 'NONE',  ( 4.184256412735922304, -2.055000000000000160, 0.000000000000000000 ) ) ;
#100743 = ORIENTED_EDGE ( 'NONE', *, *, #71161, .T. ) ;
#100744 = SURFACE_STYLE_FILL_AREA ( #91320 ) ;
#100745 = DIRECTION ( 'NONE',  ( 0.7071067811865486830, -0.7071067811865464625, -0.000000000000000000 ) ) ;
#100746 = CARTESIAN_POINT ( 'NONE',  ( 8.999999999999937828, -6.108550654416951886, -3.114665004254947078 ) ) ;
#100747 = VECTOR ( 'NONE', #87586, 1000.000000000000227 ) ;
#100748 = LINE ( 'NONE', #1399, #11417 ) ;
#100749 = CARTESIAN_POINT ( 'NONE',  ( -34.92500000000001137, 22.22500000000000142, 4.000000000000000000 ) ) ;
#100751 = DIRECTION ( 'NONE',  ( 0.7071067811865487940, 0.7071067811865463515, 0.000000000000000000 ) ) ;
#100750 = VECTOR ( 'NONE', #44090, 1000.000000000000000 ) ;
#100752 = CARTESIAN_POINT ( 'NONE',  ( -34.92500000000001137, 22.22500000000000142, 4.500000000000000888 ) ) ;
#100753 = DIRECTION ( 'NONE',  ( -0.3543493200069162685, -0.000000000000000000, -0.9351131265310288487 ) ) ;
#100754 = CARTESIAN_POINT ( 'NONE',  ( -24.29974487139158867, -27.71228299555223273, 4.000000000000000000 ) ) ;
#100755 = CARTESIAN_POINT ( 'NONE',  ( 24.47873647476856007, -5.808823158059033709, 5.808823158059035485 ) ) ;
#100756 = DIRECTION ( 'NONE',  ( -1.000000000000000000, -0.000000000000000000, -0.000000000000000000 ) ) ;
#100757 = CARTESIAN_POINT ( 'NONE',  ( 12.48921356237309155, -27.52281430457064104, 5.000000000000000000 ) ) ;
#100758 = DIRECTION ( 'NONE',  ( 0.3543493200069162685, -0.000000000000000000, -0.9351131265310288487 ) ) ;
#100759 = DIRECTION ( 'NONE',  ( 1.000000000000000000, 0.000000000000000000, 0.000000000000000000 ) ) ;
#100760 = VERTEX_POINT ( 'NONE', #54196 ) ;
#100761 = ADVANCED_FACE ( 'NONE', ( #108489 ), #53436, .F. ) ;
#100762 = ORIENTED_EDGE ( 'NONE', *, *, #73087, .T. ) ;
#100763 = CARTESIAN_POINT ( 'NONE',  ( 102.0625000000000000, -5.819803920172572198, -5.819803920172573086 ) ) ;
#100764 = VERTEX_POINT ( 'NONE', #78066 ) ;
#100765 = VECTOR ( 'NONE', #117301, 999.9999999999998863 ) ;
#100766 = VERTEX_POINT ( 'NONE', #77372 ) ;
#100767 = ORIENTED_EDGE ( 'NONE', *, *, #25151, .T. ) ;
#100768 = LINE ( 'NONE', #134122, #84988 ) ;
#100769 = CARTESIAN_POINT ( 'NONE',  ( 88.50000000000000000, 0.000000000000000000, -7.950000000000000178 ) ) ;
#100770 = DIRECTION ( 'NONE',  ( -0.6830127018922180770, -0.6830127018922204085, -0.2588190451025213501 ) ) ;
#100771 = ORIENTED_EDGE ( 'NONE', *, *, #97353, .T. ) ;
#100772 = PLANE ( 'NONE',  #2335 ) ;
#100773 = CARTESIAN_POINT ( 'NONE',  ( -1.180000000000000604, 10.00000000000000178, 10.00000000000000000 ) ) ;
#100774 = CARTESIAN_POINT ( 'NONE',  ( -16.83455439249994612, 8.717631302929021331, 5.000000000000000000 ) ) ;
#100775 = DIRECTION ( 'NONE',  ( 0.000000000000000000, 0.000000000000000000, 1.000000000000000000 ) ) ;
#100776 = ORIENTED_EDGE ( 'NONE', *, *, #117625, .T. ) ;
#100777 = CARTESIAN_POINT ( 'NONE',  ( -12.69999999999998153, 3.061616997868383634E-16, -2.500000000000000444 ) ) ;
#100778 = LINE ( 'NONE', #98109, #107202 ) ;
#100779 =( NAMED_UNIT ( * ) SI_UNIT ( $, .STERADIAN. ) SOLID_ANGLE_UNIT ( ) );
#100780 = CARTESIAN_POINT ( 'NONE',  ( -18.18398860626898994, 28.73617430169800002, 5.000000000000000000 ) ) ;
#100781 = CARTESIAN_POINT ( 'NONE',  ( 34.49999999999976552, 10.08746187583914100, 4.000000000000000000 ) ) ;
#100782 = CARTESIAN_POINT ( 'NONE',  ( 24.99033360189226016, 3.759292476615681888, 4.478963035907999490 ) ) ;
#100783 = LINE ( 'NONE', #135568, #68621 ) ;
#100784 = FACE_OUTER_BOUND ( 'NONE', #56134, .T. ) ;
#100785 = DIRECTION ( 'NONE',  ( -1.000000000000000000, -1.224606353822377258E-16, -0.000000000000000000 ) ) ;
#100786 = AXIS2_PLACEMENT_3D ( 'NONE', #66305, #101763, #22048 ) ;
#100787 = VERTEX_POINT ( 'NONE', #75910 ) ;
#100788 = ORIENTED_EDGE ( 'NONE', *, *, #65154, .F. ) ;
#100790 = ADVANCED_FACE ( 'NONE', ( #122243 ), #31692, .F. ) ;
#100789 = VECTOR ( 'NONE', #111666, 1000.000000000000000 ) ;
#100791 = CARTESIAN_POINT ( 'NONE',  ( 120.1670968585647756, -3.055000000000000160, -5.291415217122921177 ) ) ;
#100792 = ORIENTED_EDGE ( 'NONE', *, *, #68754, .T. ) ;
#100793 = AXIS2_PLACEMENT_3D ( 'NONE', #20234, #64479, #87658 ) ;
#100794 = ADVANCED_FACE ( 'NONE', ( #119383 ), #12060, .T. ) ;
#100795 = CARTESIAN_POINT ( 'NONE',  ( 7.828169399223472880, 15.75929247661555976, 4.000000000000000000 ) ) ;
#100796 = DIRECTION ( 'NONE',  ( 0.000000000000000000, 0.06845965770171351383, -0.9976538855070752332 ) ) ;
#100797 = EDGE_CURVE ( 'NONE', #55578, #59038, #55600, .T. ) ;
#100798 = EDGE_CURVE ( 'NONE', #118739, #109940, #462, .T. ) ;
#100799 = CARTESIAN_POINT ( 'NONE',  ( 18.18398860626898994, 28.73617430169800002, 5.000000000000000000 ) ) ;
#100800 = DIRECTION ( 'NONE',  ( 0.7071067811865486830, -0.7071067811865464625, -0.000000000000000000 ) ) ;
#100801 = CARTESIAN_POINT ( 'NONE',  ( 113.6620968585647944, -5.291415217122919401, 3.054999999999997939 ) ) ;
#100802 = VERTEX_POINT ( 'NONE', #130311 ) ;
#100803 = ORIENTED_EDGE ( 'NONE', *, *, #13422, .F. ) ;
#100804 = DIRECTION ( 'NONE',  ( -0.7071067811865486830, -0.7071067811865464625, -0.000000000000000000 ) ) ;
#100805 = ORIENTED_EDGE ( 'NONE', *, *, #40975, .T. ) ;
#100806 = EDGE_LOOP ( 'NONE', ( #63377, #77068, #85695, #136755 ) ) ;
#100808 = ADVANCED_FACE ( 'NONE', ( #30998 ), #66478, .T. ) ;
#100807 = CARTESIAN_POINT ( 'NONE',  ( 38.35459685856476852, -1.637169565754161615, 6.110000000000000320 ) ) ;
#100809 = EDGE_LOOP ( 'NONE', ( #31657, #38175, #2113, #92610 ) ) ;
#100810 = CARTESIAN_POINT ( 'NONE',  ( -5.999999999999963585, -5.527737879153202805, -7.983877177622358268 ) ) ;
#100811 = EDGE_CURVE ( 'NONE', #129125, #134614, #22215, .T. ) ;
#100812 = DIRECTION ( 'NONE',  ( 0.000000000000000000, -0.000000000000000000, 1.000000000000000000 ) ) ;
#100813 = EDGE_CURVE ( 'NONE', #139420, #27206, #109242, .T. ) ;
#100814 = CARTESIAN_POINT ( 'NONE',  ( -34.49999999999975842, 16.46425560840032176, 4.994342998332164107 ) ) ;
#100815 = ORIENTED_EDGE ( 'NONE', *, *, #76948, .T. ) ;
#100816 = CARTESIAN_POINT ( 'NONE',  ( -42.18398860626899705, 28.73617430169816700, 5.000000000000000000 ) ) ;
#100817 = ORIENTED_EDGE ( 'NONE', *, *, #60791, .T. ) ;
#100818 = ORIENTED_EDGE ( 'NONE', *, *, #82015, .T. ) ;
#100819 = EDGE_CURVE ( 'NONE', #134245, #97576, #116497, .T. ) ;
#100820 = ORIENTED_EDGE ( 'NONE', *, *, #53964, .T. ) ;
#100821 = CARTESIAN_POINT ( 'NONE',  ( 29.99999999999978328, -16.02097659208068947, -11.96015758381215655 ) ) ;
#100822 = LINE ( 'NONE', #12374, #129848 ) ;
#100823 = ORIENTED_EDGE ( 'NONE', *, *, #33078, .T. ) ;
#100824 = PLANE ( 'NONE',  #87712 ) ;
#100825 = DIRECTION ( 'NONE',  ( 0.000000000000000000, 0.000000000000000000, 1.000000000000000000 ) ) ;
#100826 = EDGE_CURVE ( 'NONE', #40283, #116562, #21531, .T. ) ;
#100827 = FILL_AREA_STYLE ('',( #101529 ) ) ;
#100828 = LINE ( 'NONE', #43591, #95279 ) ;
#100829 = FACE_BOUND ( 'NONE', #69717, .T. ) ;
#100830 = ORIENTED_EDGE ( 'NONE', *, *, #48101, .T. ) ;
#100831 = DIRECTION ( 'NONE',  ( -0.7071067811865486830, -0.7071067811865464625, 0.000000000000000000 ) ) ;
#100832 = CARTESIAN_POINT ( 'NONE',  ( -8.816011393731004731, 28.73617430169781173, 5.000000000000000000 ) ) ;
#100833 = FACE_OUTER_BOUND ( 'NONE', #43500, .T. ) ;
#100834 = CARTESIAN_POINT ( 'NONE',  ( 17.99999999999986855, -19.06887692260762179, 4.000000000000000000 ) ) ;
#100835 = ORIENTED_EDGE ( 'NONE', *, *, #135338, .T. ) ;
#100836 = ADVANCED_FACE ( 'NONE', ( #54889 ), #99056, .T. ) ;
#100837 = CARTESIAN_POINT ( 'NONE',  ( 25.12913961620377279, 5.278424836066147208, 3.047499999999990550 ) ) ;
#100838 = ORIENTED_EDGE ( 'NONE', *, *, #110062, .F. ) ;
#100839 = ADVANCED_FACE ( 'NONE', ( #14915 ), #91091, .F. ) ;
#100840 = VERTEX_POINT ( 'NONE', #125112 ) ;
#100841 = VERTEX_POINT ( 'NONE', #48267 ) ;
#100842 = EDGE_CURVE ( 'NONE', #7890, #92905, #47604, .T. ) ;
#100843 = VECTOR ( 'NONE', #129306, 1000.000000000000227 ) ;
#100844 = CARTESIAN_POINT ( 'NONE',  ( 51.97459685856478728, 1.637169565754164280, -6.109999999999996767 ) ) ;
#100845 = ORIENTED_EDGE ( 'NONE', *, *, #47212, .T. ) ;
#100846 = CARTESIAN_POINT ( 'NONE',  ( -19.49999999999987210, 1.030536316426487797, -5.498701923753756660 ) ) ;
#100847 = DIRECTION ( 'NONE',  ( -0.7071067811865486830, -0.7071067811865464625, -0.000000000000000000 ) ) ;
#100848 = VERTEX_POINT ( 'NONE', #135993 ) ;
#100849 = CARTESIAN_POINT ( 'NONE',  ( -9.328169399223456892, -15.74070752338412049, 4.000000000000000000 ) ) ;
#100850 = DIRECTION ( 'NONE',  ( 0.7071067811865487940, 0.7071067811865463515, 0.000000000000000000 ) ) ;
#100851 = DIRECTION ( 'NONE',  ( -0.7071067811865486830, -0.7071067811865464625, 0.000000000000000000 ) ) ;
#100852 = MECHANICAL_DESIGN_GEOMETRIC_PRESENTATION_REPRESENTATION (  '', ( #107469 ), #110053 ) ;
#100853 = CARTESIAN_POINT ( 'NONE',  ( -20.99451991528748707, 28.92564299267952777, 4.000000000000000000 ) ) ;
#100854 = CARTESIAN_POINT ( 'NONE',  ( 27.41161490594811667, 22.22500000000000142, 4.777194822843816802 ) ) ;
#100855 = PLANE ( 'NONE',  #51697 ) ;
#100856 = ORIENTED_EDGE ( 'NONE', *, *, #87043, .F. ) ;
#100857 = ORIENTED_EDGE ( 'NONE', *, *, #74603, .F. ) ;
#100858 = EDGE_LOOP ( 'NONE', ( #8306, #26454, #65076, #17775 ) ) ;
#100859 = ORIENTED_EDGE ( 'NONE', *, *, #70884, .F. ) ;
#100860 = LINE ( 'NONE', #90727, #98275 ) ;
#100861 = CARTESIAN_POINT ( 'NONE',  ( 35.80836038379622721, 7.949999999999996625, 2.130196079827431088 ) ) ;
#100862 = ORIENTED_EDGE ( 'NONE', *, *, #10281, .T. ) ;
#100863 = VERTEX_POINT ( 'NONE', #102673 ) ;
#100864 = SURFACE_STYLE_USAGE ( .BOTH. , #132092 ) ;
#100865 = CARTESIAN_POINT ( 'NONE',  ( -57.29974487139158157, -27.71228299555246011, 4.000000000000000000 ) ) ;
#100866 = VERTEX_POINT ( 'NONE', #122984 ) ;
#100867 = DIRECTION ( 'NONE',  ( 0.6830127018922180770, -0.6830127018922204085, -0.2588190451025213501 ) ) ;
#100868 = VECTOR ( 'NONE', #118609, 1000.000000000000227 ) ;
#100869 = CARTESIAN_POINT ( 'NONE',  ( 14.81601139373099585, 28.73617430169776910, 5.000000000000000000 ) ) ;
#100870 = CARTESIAN_POINT ( 'NONE',  ( 25.29623647476855908, 7.934999999999990727, -1.457635852685135314E-15 ) ) ;
#100871 = AXIS2_PLACEMENT_3D ( 'NONE', #91536, #124150, #135068 ) ;
#100872 = DIRECTION ( 'NONE',  ( 0.7071067811865487940, -0.7071067811865463515, 0.000000000000000000 ) ) ;
#100873 = ORIENTED_EDGE ( 'NONE', *, *, #17194, .T. ) ;
#100875 = FACE_OUTER_BOUND ( 'NONE', #83593, .T. ) ;
#100874 = CARTESIAN_POINT ( 'NONE',  ( 108.5579301918980946, 6.110000000000001208, -1.637169565754156286 ) ) ;
#100876 = VECTOR ( 'NONE', #61686, 1000.000000000000227 ) ;
#100877 = CARTESIAN_POINT ( 'NONE',  ( 0.000000000000000000, 0.000000000000000000, 5.000000000000000000 ) ) ;
#100878 = CARTESIAN_POINT ( 'NONE',  ( -36.51168605928409505, 6.759292476615653023, 16.35960578974477997 ) ) ;
#100879 = CARTESIAN_POINT ( 'NONE',  ( -11.29289321881338104, -0.7407075233842770334, 5.000000000000000000 ) ) ;
#100881 = VERTEX_POINT ( 'NONE', #67936 ) ;
#100880 = CARTESIAN_POINT ( 'NONE',  ( 19.10813147593277250, 2.055000000000001048, 0.000000000000000000 ) ) ;
#100882 = CARTESIAN_POINT ( 'NONE',  ( -63.18398860626900415, 28.73617430169831621, 5.000000000000000000 ) ) ;
#100883 = ORIENTED_EDGE ( 'NONE', *, *, #137151, .F. ) ;
#100884 = VECTOR ( 'NONE', #118564, 1000.000000000000000 ) ;
#100885 = DIRECTION ( 'NONE',  ( -1.000000000000000000, -0.000000000000000000, -0.000000000000000000 ) ) ;
#100886 = DIRECTION ( 'NONE',  ( 0.000000000000000000, 0.000000000000000000, -1.000000000000000000 ) ) ;
#100887 = CARTESIAN_POINT ( 'NONE',  ( 120.8750000000000000, 7.950000000000000178, 1.460391307983218535E-15 ) ) ;
#100888 = ORIENTED_EDGE ( 'NONE', *, *, #89518, .T. ) ;
#100889 = CARTESIAN_POINT ( 'NONE',  ( 61.46640106136307935, -43.14999999999999147, 34.92499999999998295 ) ) ;
#100890 = DIRECTION ( 'NONE',  ( -1.000000000000000000, -0.000000000000000000, -0.000000000000000000 ) ) ;
#100891 = DIRECTION ( 'NONE',  ( 1.000000000000000000, 1.224606353822377258E-16, 0.000000000000000000 ) ) ;
#100892 = VERTEX_POINT ( 'NONE', #125853 ) ;
#100893 = LINE ( 'NONE', #132125, #53876 ) ;
#100894 = ORIENTED_EDGE ( 'NONE', *, *, #99685, .T. ) ;
#100895 = LINE ( 'NONE', #68321, #85467 ) ;
#100896 = ADVANCED_FACE ( 'NONE', ( #2604 ), #3992, .F. ) ;
#100898 = ORIENTED_EDGE ( 'NONE', *, *, #117573, .F. ) ;
#100897 = FACE_OUTER_BOUND ( 'NONE', #57953, .T. ) ;
#100900 = EDGE_LOOP ( 'NONE', ( #9479, #137863, #58059, #49812 ) ) ;
#100899 = EDGE_CURVE ( 'NONE', #52088, #131561, #36669, .T. ) ;
#100901 = CARTESIAN_POINT ( 'NONE',  ( 0.3281693992235323876, 11.25929247661561305, 4.000000000000000000 ) ) ;
#100902 = DIRECTION ( 'NONE',  ( -0.000000000000000000, 0.3543493200069153248, 0.9351131265310292928 ) ) ;
#100903 = ORIENTED_EDGE ( 'NONE', *, *, #41847, .F. ) ;
#100904 = CARTESIAN_POINT ( 'NONE',  ( 59.99451991528749772, 28.92564299267980132, 4.000000000000000000 ) ) ;
#100905 = DIRECTION ( 'NONE',  ( 0.7071067811865487940, 0.7071067811865463515, 0.000000000000000000 ) ) ;
#100906 = DIRECTION ( 'NONE',  ( -1.000000000000000000, -1.224606353822377258E-16, -0.000000000000000000 ) ) ;
#100907 = VERTEX_POINT ( 'NONE', #25071 ) ;
#100908 = EDGE_CURVE ( 'NONE', #93195, #56372, #37402, .T. ) ;
#100909 = DIRECTION ( 'NONE',  ( -0.000000000000000000, -0.3543493200069152693, 0.9351131265310292928 ) ) ;
#100910 = CARTESIAN_POINT ( 'NONE',  ( -18.18398860626898994, 28.73617430169800002, 5.000000000000000000 ) ) ;
#100911 = DIRECTION ( 'NONE',  ( -0.3543493200069162685, -0.000000000000000000, -0.9351131265310288487 ) ) ;
#100912 = CARTESIAN_POINT ( 'NONE',  ( 180.4193221990230143, -52.14999999999999147, 40.92499999999998295 ) ) ;
#100913 = CARTESIAN_POINT ( 'NONE',  ( 9.792893218813389922, 3.759292476615674783, 5.000000000000000000 ) ) ;
#100914 = CARTESIAN_POINT ( 'NONE',  ( 31.70376352523145158, 6.109999999999999432, 1.122388791418549108E-15 ) ) ;
#100915 = DIRECTION ( 'NONE',  ( -0.7071067811865486830, -0.7071067811865464625, -0.000000000000000000 ) ) ;
#100916 = ORIENTED_EDGE ( 'NONE', *, *, #21463, .F. ) ;
#100917 = EDGE_CURVE ( 'NONE', #28997, #34677, #26525, .T. ) ;
#100918 = ORIENTED_EDGE ( 'NONE', *, *, #28333, .F. ) ;
#100919 = ORIENTED_EDGE ( 'NONE', *, *, #26524, .T. ) ;
#100920 = DIRECTION ( 'NONE',  ( -0.7071067811865486830, -0.7071067811865464625, 0.000000000000000000 ) ) ;
#100921 = VERTEX_POINT ( 'NONE', #112809 ) ;
#100922 = ORIENTED_EDGE ( 'NONE', *, *, #51620, .F. ) ;
#100923 = ORIENTED_EDGE ( 'NONE', *, *, #10751, .T. ) ;
#100924 = CARTESIAN_POINT ( 'NONE',  ( 1.666965064704732269, -1.287028696899377367E-11, -6.428034935295263708 ) ) ;
#100925 = CARTESIAN_POINT ( 'NONE',  ( 176.2838169021916599, 7.919999999999943086, -18.97500000000001918 ) ) ;
#100926 = EDGE_CURVE ( 'NONE', #101563, #23274, #92466, .T. ) ;
#100927 = ORIENTED_EDGE ( 'NONE', *, *, #8104, .F. ) ;
#100928 = DIRECTION ( 'NONE',  ( 1.000000000000000000, -0.000000000000000000, 0.000000000000000000 ) ) ;
#100929 = CARTESIAN_POINT ( 'NONE',  ( 0.000000000000000000, 0.000000000000000000, 5.000000000000000000 ) ) ;
#100930 = FACE_OUTER_BOUND ( 'NONE', #3984, .T. ) ;
#100931 = DIRECTION ( 'NONE',  ( 0.6830127018922181881, 0.6830127018922202975, -0.2588190451025214056 ) ) ;
#100932 = CARTESIAN_POINT ( 'NONE',  ( 121.0420968585647756, 5.291415217122923842, -3.054999999999996163 ) ) ;
#100933 = ORIENTED_EDGE ( 'NONE', *, *, #9161, .F. ) ;
#100934 = PLANE ( 'NONE',  #71946 ) ;
#100935 = SURFACE_STYLE_USAGE ( .BOTH. , #43708 ) ;
#100936 = CARTESIAN_POINT ( 'NONE',  ( 78.72916666666665719, 7.950000000000001954, -2.130196079827421762 ) ) ;
#100937 = LINE ( 'NONE', #1594, #3954 ) ;
#100938 = CARTESIAN_POINT ( 'NONE',  ( 13.64840764549667540, 9.139736423841732040E-16, 0.000000000000000000 ) ) ;
#100939 = LINE ( 'NONE', #142332, #60814 ) ;
#100940 = FACE_OUTER_BOUND ( 'NONE', #119588, .T. ) ;
#100941 = CARTESIAN_POINT ( 'NONE',  ( 48.93336038379622721, 2.130196079827431532, -7.949999999999997513 ) ) ;
#100942 = VECTOR ( 'NONE', #75177, 1000.000000000000000 ) ;
#100943 = CARTESIAN_POINT ( 'NONE',  ( 2.999999999999978240, -21.41253812416053748, 4.000000000000000000 ) ) ;
#100944 = DIRECTION ( 'NONE',  ( 1.000000000000000000, 0.000000000000000000, 0.000000000000000000 ) ) ;
#100945 = ORIENTED_EDGE ( 'NONE', *, *, #13984, .F. ) ;
#100946 = ORIENTED_EDGE ( 'NONE', *, *, #138932, .T. ) ;
#100947 = CARTESIAN_POINT ( 'NONE',  ( 48.97916666666665009, -7.950000000000001066, 2.130196079827424427 ) ) ;
#100948 = VECTOR ( 'NONE', #97778, 1000.000000000000000 ) ;
#100949 = LINE ( 'NONE', #88676, #59930 ) ;
#100950 = EDGE_CURVE ( 'NONE', #126104, #99826, #81647, .T. ) ;
#100951 = ORIENTED_EDGE ( 'NONE', *, *, #17009, .T. ) ;
#100952 = LINE ( 'NONE', #109694, #101072 ) ;
#100954 = EDGE_CURVE ( 'NONE', #75725, #42588, #114915, .T. ) ;
#100953 = DIRECTION ( 'NONE',  ( -0.7071067811865486830, 0.7071067811865464625, 0.000000000000000000 ) ) ;
#100955 = EDGE_CURVE ( 'NONE', #3311, #70705, #57045, .T. ) ;
#100956 = CARTESIAN_POINT ( 'NONE',  ( 36.75043019189811133, 3.055000000000002824, -5.291415217122919401 ) ) ;
#100958 = ORIENTED_EDGE ( 'NONE', *, *, #23020, .F. ) ;
#100957 = VECTOR ( 'NONE', #102965, 1000.000000000000000 ) ;
#100959 = CARTESIAN_POINT ( 'NONE',  ( 14.99999999999989875, -1.209798855135680418, 4.371887122346866050 ) ) ;
#100960 = ORIENTED_EDGE ( 'NONE', *, *, #80367, .T. ) ;
#100961 = LINE ( 'NONE', #25542, #40363 ) ;
#100962 = EDGE_CURVE ( 'NONE', #71933, #99127, #70074, .T. ) ;
#100963 = CARTESIAN_POINT ( 'NONE',  ( 152.4000000000000057, 25.96999999999993847, -33.92499999999998295 ) ) ;
#100964 = LINE ( 'NONE', #11069, #113795 ) ;
#100965 = CARTESIAN_POINT ( 'NONE',  ( -7.410090645198278203, 9.759292476615614831, 11.28811694763777140 ) ) ;
#100966 = EDGE_LOOP ( 'NONE', ( #38926, #11375, #98, #10345, #130535 ) ) ;
#100967 = VECTOR ( 'NONE', #92575, 999.9999999999998863 ) ;
#100968 = ADVANCED_FACE ( 'NONE', ( #114240 ), #59873, .T. ) ;
#100969 = DIRECTION ( 'NONE',  ( -0.7071067811865486830, -0.7071067811865464625, -0.000000000000000000 ) ) ;
#100970 = ORIENTED_EDGE ( 'NONE', *, *, #111575, .F. ) ;
#100971 = CARTESIAN_POINT ( 'NONE',  ( -8.999999999999941380, -6.108550654416969650, -3.114665004254987046 ) ) ;
#100972 = EDGE_CURVE ( 'NONE', #60071, #117911, #103343, .T. ) ;
#100973 = DIRECTION ( 'NONE',  ( 0.7071067811865487940, 0.7071067811865463515, -0.000000000000000000 ) ) ;
#100974 = PRESENTATION_STYLE_ASSIGNMENT (( #88699 ) ) ;
#100975 = DIRECTION ( 'NONE',  ( -1.000000000000000000, -1.224606353822377258E-16, -0.000000000000000000 ) ) ;
#100976 = STYLED_ITEM ( 'NONE', ( #132206 ), #121822 ) ;
#100977 = VERTEX_POINT ( 'NONE', #12769 ) ;
#100978 = EDGE_CURVE ( 'NONE', #138243, #22107, #101216, .T. ) ;
#100979 = CARTESIAN_POINT ( 'NONE',  ( -12.20000000000000284, -40.42999999999999261, -40.00000000000000000 ) ) ;
#100980 = CARTESIAN_POINT ( 'NONE',  ( 60.14126352523143737, 4.472830434245836706, 4.472830434245840259 ) ) ;
#100981 = VECTOR ( 'NONE', #136255, 1000.000000000000000 ) ;
#100982 = DIRECTION ( 'NONE',  ( 1.000000000000000000, 1.369518533665900312E-16, -0.000000000000000000 ) ) ;
#100983 = PLANE ( 'NONE',  #142690 ) ;
#100984 = DIRECTION ( 'NONE',  ( -0.6830127018922180770, -0.6830127018922204085, -0.2588190451025213501 ) ) ;
#100985 = VERTEX_POINT ( 'NONE', #134594 ) ;
#100986 = VECTOR ( 'NONE', #110527, 1000.000000000000000 ) ;
#100987 = CARTESIAN_POINT ( 'NONE',  ( 1.629999999999999893, -0.3999999999999997446, -2.303088455023527104 ) ) ;
#100988 = ADVANCED_FACE ( 'NONE', ( #35291 ), #79533, .F. ) ;
#100989 = ORIENTED_EDGE ( 'NONE', *, *, #112172, .F. ) ;
#100990 = DIRECTION ( 'NONE',  ( 0.6830127018922181881, 0.6830127018922202975, -0.2588190451025214056 ) ) ;
#100991 = ORIENTED_EDGE ( 'NONE', *, *, #141914, .F. ) ;
#100992 = DIRECTION ( 'NONE',  ( 0.7071067811865487940, 0.7071067811865463515, -0.000000000000000000 ) ) ;
#100993 = CARTESIAN_POINT ( 'NONE',  ( 0.000000000000000000, 0.000000000000000000, 5.000000000000000000 ) ) ;
#100994 = CARTESIAN_POINT ( 'NONE',  ( 1.499999999999990896, -12.66682484999666336, -0.6294897503863906563 ) ) ;
#100995 = CARTESIAN_POINT ( 'NONE',  ( -23.51078643762690490, -27.52281430457038880, 5.000000000000000000 ) ) ;
#100996 = FACE_BOUND ( 'NONE', #44483, .T. ) ;
#100997 = CARTESIAN_POINT ( 'NONE',  ( -5.999999999999960032, -0.03360074219773551141, 5.000000000000000000 ) ) ;
#100998 = DIRECTION ( 'NONE',  ( -1.000000000000000000, -0.000000000000000000, -0.000000000000000000 ) ) ;
#100999 = CARTESIAN_POINT ( 'NONE',  ( 63.29974487139158867, -27.71228299555250274, 4.000000000000000000 ) ) ;
#101001 = ORIENTED_EDGE ( 'NONE', *, *, #109635, .T. ) ;
#101000 = LINE ( 'NONE', #69116, #11101 ) ;
#101002 = DIRECTION ( 'NONE',  ( -0.7071067811865486830, 0.7071067811865464625, 0.000000000000000000 ) ) ;
#101003 = VERTEX_POINT ( 'NONE', #61340 ) ;
#101004 = ADVANCED_FACE ( 'NONE', ( #84493 ), #19213, .F. ) ;
#101005 = EDGE_CURVE ( 'NONE', #76368, #13267, #93909, .T. ) ;
#101006 = VERTEX_POINT ( 'NONE', #27949 ) ;
#101007 = CARTESIAN_POINT ( 'NONE',  ( 78.66209685856479439, -5.291415217122919401, 3.054999999999997939 ) ) ;
#101008 = ORIENTED_EDGE ( 'NONE', *, *, #38013, .F. ) ;
#101009 = EDGE_CURVE ( 'NONE', #100121, #58114, #94612, .T. ) ;
#101010 = DIRECTION ( 'NONE',  ( 0.7071067811865487940, 0.7071067811865463515, -0.000000000000000000 ) ) ;
#101011 = ORIENTED_EDGE ( 'NONE', *, *, #107462, .T. ) ;
#101012 = CARTESIAN_POINT ( 'NONE',  ( -47.99451991528749062, 28.92564299267971251, 4.000000000000000000 ) ) ;
#101013 = VECTOR ( 'NONE', #135741, 999.9999999999998863 ) ;
#101014 = DIRECTION ( 'NONE',  ( -0.6830127018922180770, -0.6830127018922204085, -0.2588190451025213501 ) ) ;
#101015 = CARTESIAN_POINT ( 'NONE',  ( 3.781626882924918220, 21.74787736706806385, 4.999607392498048419 ) ) ;
#101016 = CARTESIAN_POINT ( 'NONE',  ( 1.629999999999999893, 0.3999999999999995226, 2.303088455023526215 ) ) ;
#101018 = DIRECTION ( 'NONE',  ( -0.000000000000000000, -0.000000000000000000, 1.000000000000000000 ) ) ;
#101017 = CARTESIAN_POINT ( 'NONE',  ( 27.18398860626900060, 28.73617430169806042, 5.000000000000000000 ) ) ;
#101019 = LINE ( 'NONE', #56863, #127969 ) ;
#101020 = CARTESIAN_POINT ( 'NONE',  ( -34.92500000000001137, 22.22500000000000142, 4.000000000000000000 ) ) ;
#101021 = ORIENTED_EDGE ( 'NONE', *, *, #71464, .F. ) ;
#101022 = AXIS2_PLACEMENT_3D ( 'NONE', #101094, #123608, #58375 ) ;
#101023 = ORIENTED_EDGE ( 'NONE', *, *, #96736, .T. ) ;
#101024 = DIRECTION ( 'NONE',  ( -0.7071067811865487940, 0.7071067811865463515, -0.000000000000000000 ) ) ;
#101025 = DIRECTION ( 'NONE',  ( 0.3543493200069162685, -0.000000000000000000, -0.9351131265310288487 ) ) ;
#101026 = VERTEX_POINT ( 'NONE', #4704 ) ;
#101027 = ORIENTED_EDGE ( 'NONE', *, *, #118629, .T. ) ;
#101028 = ORIENTED_EDGE ( 'NONE', *, *, #15831, .T. ) ;
#101029 = DIRECTION ( 'NONE',  ( -0.000000000000000000, 0.000000000000000000, 1.000000000000000000 ) ) ;
#101030 = VERTEX_POINT ( 'NONE', #74327 ) ;
#101031 = DIRECTION ( 'NONE',  ( 0.7071067811865487940, -0.7071067811865463515, 0.000000000000000000 ) ) ;
#101032 = VECTOR ( 'NONE', #131521, 1000.000000000000000 ) ;
#101033 = PLANE ( 'NONE',  #53994 ) ;
#101034 = CARTESIAN_POINT ( 'NONE',  ( 0.7962364747685526378, 7.934999999999990727, -1.457635852685135314E-15 ) ) ;
#101035 = PLANE ( 'NONE',  #100518 ) ;
#101036 = VERTEX_POINT ( 'NONE', #115624 ) ;
#101037 = VECTOR ( 'NONE', #139721, 1000.000000000000000 ) ;
#101038 = LINE ( 'NONE', #45984, #133721 ) ;
#101040 = EDGE_CURVE ( 'NONE', #23492, #34867, #118516, .T. ) ;
#101039 = DIRECTION ( 'NONE',  ( -1.000000000000000000, 0.000000000000000000, 0.000000000000000000 ) ) ;
#101041 = CARTESIAN_POINT ( 'NONE',  ( -25.01899999999999835, 3.174999999999998046, 5.000000000000000000 ) ) ;
#101043 = VERTEX_POINT ( 'NONE', #73603 ) ;
#101042 = CARTESIAN_POINT ( 'NONE',  ( -0.4892135623730947680, -27.52281430457055578, 5.000000000000000000 ) ) ;
#101044 = EDGE_LOOP ( 'NONE', ( #118654, #70959, #105205, #82998 ) ) ;
#101045 =( NAMED_UNIT ( * ) SI_UNIT ( $, .STERADIAN. ) SOLID_ANGLE_UNIT ( ) );
#101046 = DIRECTION ( 'NONE',  ( -0.000000000000000000, 0.3543493200069153248, 0.9351131265310292928 ) ) ;
#101047 = LINE ( 'NONE', #101771, #61092 ) ;
#101048 = ORIENTED_EDGE ( 'NONE', *, *, #35578, .T. ) ;
#101049 = CARTESIAN_POINT ( 'NONE',  ( -7.940000000000007496, -60.26999999999998892, -10.00000000000000178 ) ) ;
#101050 = VECTOR ( 'NONE', #59161, 1000.000000000000000 ) ;
#101051 = CARTESIAN_POINT ( 'NONE',  ( -18.18398860626898994, 28.73617430169800002, 5.000000000000000000 ) ) ;
#101052 = FACE_OUTER_BOUND ( 'NONE', #37278, .T. ) ;
#101053 = FACE_OUTER_BOUND ( 'NONE', #139977, .T. ) ;
#101054 = CARTESIAN_POINT ( 'NONE',  ( 15.98840764549667703, 9.139736423841732040E-16, 0.000000000000000000 ) ) ;
#101055 = CARTESIAN_POINT ( 'NONE',  ( -12.69999999999998153, 0.000000000000000000, 2.500000000000000444 ) ) ;
#101056 = CARTESIAN_POINT ( 'NONE',  ( -19.49999999999985789, -5.947814304570772315, 5.000000000000000000 ) ) ;
#101057 = EDGE_CURVE ( 'NONE', #106956, #85580, #60619, .T. ) ;
#101058 = LINE ( 'NONE', #35133, #84146 ) ;
#101059 = AXIS2_PLACEMENT_3D ( 'NONE', #22152, #20733, #64260 ) ;
#101060 = DIRECTION ( 'NONE',  ( 0.000000000000000000, -0.000000000000000000, 1.000000000000000000 ) ) ;
#101061 = EDGE_CURVE ( 'NONE', #17266, #20431, #6151, .T. ) ;
#101063 = EDGE_LOOP ( 'NONE', ( #18972, #40317, #91755, #107430 ) ) ;
#101062 = EDGE_CURVE ( 'NONE', #135705, #60317, #105487, .T. ) ;
#101064 = VERTEX_POINT ( 'NONE', #93199 ) ;
#101065 = DIRECTION ( 'NONE',  ( 0.000000000000000000, 1.000000000000000000, -0.000000000000000000 ) ) ;
#101066 = LINE ( 'NONE', #35141, #100284 ) ;
#101067 = VECTOR ( 'NONE', #43573, 1000.000000000000227 ) ;
#101069 = ADVANCED_FACE ( 'NONE', ( #50428 ), #138868, .F. ) ;
#101068 = CIRCLE ( 'NONE', #10712, 0.5000000000000004441 ) ;
#101070 = EDGE_CURVE ( 'NONE', #117324, #82150, #117078, .T. ) ;
#101071 = CARTESIAN_POINT ( 'NONE',  ( 20.99999999999984723, -19.06887692260762179, 4.000000000000000000 ) ) ;
#101072 = VECTOR ( 'NONE', #1611, 1000.000000000000000 ) ;
#101073 = ORIENTED_EDGE ( 'NONE', *, *, #39142, .F. ) ;
#101074 = DIRECTION ( 'NONE',  ( -0.6830127018922181881, 0.6830127018922202975, -0.2588190451025214056 ) ) ;
#101075 = PLANE ( 'NONE',  #20543 ) ;
#101076 = CARTESIAN_POINT ( 'NONE',  ( -15.18398860626900237, 28.73617430169797871, 5.000000000000000000 ) ) ;
#101077 = ORIENTED_EDGE ( 'NONE', *, *, #21128, .T. ) ;
#101078 = EDGE_CURVE ( 'NONE', #89322, #103729, #30075, .T. ) ;
#101079 =( NAMED_UNIT ( * ) PLANE_ANGLE_UNIT ( ) SI_UNIT ( $, .RADIAN. ) );
#101080 = CARTESIAN_POINT ( 'NONE',  ( 111.5416666666666572, -3.975000000000002753, 6.884901960086286188 ) ) ;
#101081 = UNCERTAINTY_MEASURE_WITH_UNIT (LENGTH_MEASURE( 1.000000000000000082E-05 ), #15718, 'distance_accuracy_value', 'NONE');
#101082 = DIRECTION ( 'NONE',  ( -1.000000000000000000, -1.224606353822377258E-16, -0.000000000000000000 ) ) ;
#101083 = VECTOR ( 'NONE', #46238, 1000.000000000000000 ) ;
#101084 = CARTESIAN_POINT ( 'NONE',  ( 6.471592354503322042, 9.902892378096218942E-16, 0.000000000000000000 ) ) ;
#101085 = CARTESIAN_POINT ( 'NONE',  ( 56.64126352523144448, 4.472830434245837594, 4.472830434245841147 ) ) ;
#101086 = CARTESIAN_POINT ( 'NONE',  ( 8.700255128608413102, -27.71228299555199825, 4.000000000000000000 ) ) ;
#101087 = EDGE_CURVE ( 'NONE', #95318, #121873, #82350, .T. ) ;
#101088 = PLANE ( 'NONE',  #85785 ) ;
#101089 = CARTESIAN_POINT ( 'NONE',  ( 24.64327148205084939, 5.259292476615662792, 4.831541298974423526 ) ) ;
#101090 = ORIENTED_EDGE ( 'NONE', *, *, #71416, .F. ) ;
#101091 = CARTESIAN_POINT ( 'NONE',  ( 29.99451991528749417, 28.92564299267958816, 4.000000000000000000 ) ) ;
#101092 = ADVANCED_FACE ( 'NONE', ( #95337 ), #39562, .F. ) ;
#101093 = ORIENTED_EDGE ( 'NONE', *, *, #96635, .F. ) ;
#101094 = CARTESIAN_POINT ( 'NONE',  ( 3.087196949643289834, 3.821174125832445049E-16, 0.000000000000000000 ) ) ;
#101095 = ADVANCED_FACE ( 'NONE', ( #72218 ), #40972, .F. ) ;
#101096 = DIRECTION ( 'NONE',  ( -0.7071067811865487940, 0.7071067811865463515, 0.000000000000000000 ) ) ;
#101097 = FACE_OUTER_BOUND ( 'NONE', #16353, .T. ) ;
#101098 = LINE ( 'NONE', #132351, #34694 ) ;
#101099 = CARTESIAN_POINT ( 'NONE',  ( -5.999999999999956479, -8.731860332648846423, -2.120594902707551022 ) ) ;
#101100 = CARTESIAN_POINT ( 'NONE',  ( 0.000000000000000000, 0.000000000000000000, 5.000000000000000000 ) ) ;
#101101 = ORIENTED_EDGE ( 'NONE', *, *, #93430, .T. ) ;
#101102 = ORIENTED_EDGE ( 'NONE', *, *, #67953, .T. ) ;
#101103 = LINE ( 'NONE', #70666, #9247 ) ;
#101104 = FACE_BOUND ( 'NONE', #136267, .T. ) ;
#101105 = UNCERTAINTY_MEASURE_WITH_UNIT (LENGTH_MEASURE( 1.000000000000000082E-05 ), #21990, 'distance_accuracy_value', 'NONE');
#101106 = EDGE_CURVE ( 'NONE', #96749, #64832, #42536, .T. ) ;
#101107 = DIRECTION ( 'NONE',  ( -1.000000000000000000, -1.224606353822377258E-16, -0.000000000000000000 ) ) ;
#101108 = CARTESIAN_POINT ( 'NONE',  ( 21.70612307739180125, 22.22500000000000142, 4.000000000000000000 ) ) ;
#101109 = CARTESIAN_POINT ( 'NONE',  ( 77.07919371712957002, 3.975000000000002753, -6.884901960086283523 ) ) ;
#101110 = CARTESIAN_POINT ( 'NONE',  ( 18.18398860626898994, 28.73617430169800002, 5.000000000000000000 ) ) ;
#101111 = VECTOR ( 'NONE', #104969, 1000.000000000000000 ) ;
#101112 = PLANE ( 'NONE',  #11230 ) ;
#101113 = ORIENTED_EDGE ( 'NONE', *, *, #1847, .T. ) ;
#101114 = CARTESIAN_POINT ( 'NONE',  ( 73.04166666666667140, -3.975000000000002753, 6.884901960086286188 ) ) ;
#101115 = LINE ( 'NONE', #109141, #104825 ) ;
#101116 = FACE_OUTER_BOUND ( 'NONE', #68913, .T. ) ;
#101117 = DIRECTION ( 'NONE',  ( -0.7071067811865487940, 0.7071067811865463515, 0.000000000000000000 ) ) ;
#101118 = EDGE_CURVE ( 'NONE', #56866, #102894, #17756, .T. ) ;
#101119 = VECTOR ( 'NONE', #86363, 999.9999999999998863 ) ;
#101120 = ORIENTED_EDGE ( 'NONE', *, *, #7853, .T. ) ;
#101121 = DIRECTION ( 'NONE',  ( -0.7071067811865486830, -0.7071067811865464625, 0.000000000000000000 ) ) ;
#101122 = EDGE_CURVE ( 'NONE', #94913, #120463, #140284, .T. ) ;
#101123 = DIRECTION ( 'NONE',  ( 0.5735764363510448272, -0.8191520442889927978, 1.003171929053526103E-16 ) ) ;
#101124 = CARTESIAN_POINT ( 'NONE',  ( 69.56293019189810423, 1.637169565754157174, 6.110000000000002984 ) ) ;
#101125 = ADVANCED_FACE ( 'NONE', ( #119224 ), #53252, .F. ) ;
#101126 = STYLED_ITEM ( 'NONE', ( #125561 ), #11702 ) ;
#101127 = ORIENTED_EDGE ( 'NONE', *, *, #40098, .T. ) ;
#101128 = ORIENTED_EDGE ( 'NONE', *, *, #130389, .F. ) ;
#101129 = EDGE_CURVE ( 'NONE', #68093, #119637, #57668, .T. ) ;
#101130 = DIRECTION ( 'NONE',  ( 0.3543493200069162685, -0.000000000000000000, -0.9351131265310288487 ) ) ;
#101131 = FACE_OUTER_BOUND ( 'NONE', #34534, .T. ) ;
#101132 = CIRCLE ( 'NONE', #103394, 4.000000000000000000 ) ;
#101133 = DIRECTION ( 'NONE',  ( 0.7071067811865487940, 0.7071067811865463515, -0.000000000000000000 ) ) ;
#101134 = CARTESIAN_POINT ( 'NONE',  ( 34.92499999999998295, 22.22500000000000142, 4.500000000000000888 ) ) ;
#101136 = ORIENTED_EDGE ( 'NONE', *, *, #8146, .T. ) ;
#101135 = DIRECTION ( 'NONE',  ( 0.7071067811865487940, 0.7071067811865463515, 0.000000000000000000 ) ) ;
#101137 = DIRECTION ( 'NONE',  ( -0.7071067811865486830, 0.7071067811865464625, 0.000000000000000000 ) ) ;
#101138 = FACE_OUTER_BOUND ( 'NONE', #53777, .T. ) ;
#101139 = DIRECTION ( 'NONE',  ( 0.7071067811865487940, 0.7071067811865463515, 0.000000000000000000 ) ) ;
#101140 = CARTESIAN_POINT ( 'NONE',  ( 22.22840764549667725, -2.499999999999996003, 0.000000000000000000 ) ) ;
#101141 = ORIENTED_EDGE ( 'NONE', *, *, #91430, .F. ) ;
#101142 = VECTOR ( 'NONE', #52348, 1000.000000000000000 ) ;
#101143 = ORIENTED_EDGE ( 'NONE', *, *, #19330, .T. ) ;
#101144 = CARTESIAN_POINT ( 'NONE',  ( 57.89626352523144703, 4.472830434245840259, -4.472830434245839371 ) ) ;
#101145 = ORIENTED_EDGE ( 'NONE', *, *, #6349, .F. ) ;
#101146 = VECTOR ( 'NONE', #87990, 1000.000000000000114 ) ;
#101147 = ADVANCED_FACE ( 'NONE', ( #88043 ), #76473, .T. ) ;
#101148 = DIRECTION ( 'NONE',  ( 0.000000000000000000, -1.000000000000000000, 0.000000000000000000 ) ) ;
#101149 = CARTESIAN_POINT ( 'NONE',  ( 6.183988606268994381, 28.73617430169791476, 5.000000000000000000 ) ) ;
#101150 = DIRECTION ( 'NONE',  ( -0.7071067811865486830, 0.7071067811865464625, 0.000000000000000000 ) ) ;
#101151 = CIRCLE ( 'NONE', #10785, 9.119999999999999218 ) ;
#101152 = FACE_OUTER_BOUND ( 'NONE', #139178, .T. ) ;
#101153 = CARTESIAN_POINT ( 'NONE',  ( 5.204170427930421283E-15, -12.41253812416063163, 4.000000000000000000 ) ) ;
#101154 = ORIENTED_EDGE ( 'NONE', *, *, #103224, .F. ) ;
#101155 = ORIENTED_EDGE ( 'NONE', *, *, #94664, .F. ) ;
#101156 = DIRECTION ( 'NONE',  ( -0.000000000000000000, -0.3543493200069152693, 0.9351131265310292928 ) ) ;
#101158 = ADVANCED_FACE ( 'NONE', ( #87336 ), #110478, .F. ) ;
#101157 =( NAMED_UNIT ( * ) PLANE_ANGLE_UNIT ( ) SI_UNIT ( $, .RADIAN. ) );
#101159 = ORIENTED_EDGE ( 'NONE', *, *, #30496, .F. ) ;
#101160 = PLANE ( 'NONE',  #93008 ) ;
#101161 = CARTESIAN_POINT ( 'NONE',  ( 112.5166937171295700, 7.950000000000000178, -2.130196079827421318 ) ) ;
#101162 = CARTESIAN_POINT ( 'NONE',  ( 17.51078643762690845, -27.52281430457043143, 5.000000000000000000 ) ) ;
#101163 = VERTEX_POINT ( 'NONE', #132294 ) ;
#101164 = VECTOR ( 'NONE', #124537, 1000.000000000000000 ) ;
#101165 = FACE_BOUND ( 'NONE', #1807, .T. ) ;
#101166 = DIRECTION ( 'NONE',  ( 0.3543493200069162685, -0.000000000000000000, -0.9351131265310288487 ) ) ;
#101167 = EDGE_CURVE ( 'NONE', #27559, #48586, #75056, .T. ) ;
#101168 = DIRECTION ( 'NONE',  ( 0.7071067811865486830, -0.7071067811865464625, -0.000000000000000000 ) ) ;
#101169 = CARTESIAN_POINT ( 'NONE',  ( 37.12086038379622011, -6.884901960086286188, 3.974999999999997424 ) ) ;
#101170 = LINE ( 'NONE', #124362, #101272 ) ;
#101171 = VECTOR ( 'NONE', #13253, 1000.000000000000000 ) ;
#101172 = VECTOR ( 'NONE', #8754, 999.9999999999998863 ) ;
#101173 = DIRECTION ( 'NONE',  ( 0.7071067811865487940, 0.7071067811865463515, 0.000000000000000000 ) ) ;
#101174 = DIRECTION ( 'NONE',  ( 0.9096487118207651212, -0.3366810010545840393, -0.2432799305567678316 ) ) ;
#101175 = ORIENTED_EDGE ( 'NONE', *, *, #17605, .T. ) ;
#101176 = EDGE_CURVE ( 'NONE', #20563, #133316, #86635, .T. ) ;
#101177 = EDGE_LOOP ( 'NONE', ( #89997, #25218, #97255, #40452 ) ) ;
#101178 = CARTESIAN_POINT ( 'NONE',  ( 100.3912635252314516, -4.472830434245838482, -4.472830434245838482 ) ) ;
#101179 = ORIENTED_EDGE ( 'NONE', *, *, #93264, .F. ) ;
#101180 = CARTESIAN_POINT ( 'NONE',  ( 20.81601139373100295, 28.73617430169773002, 5.000000000000000000 ) ) ;
#101181 = ORIENTED_EDGE ( 'NONE', *, *, #71622, .T. ) ;
#101182 = VECTOR ( 'NONE', #122333, 999.9999999999998863 ) ;
#101183 = MECHANICAL_DESIGN_GEOMETRIC_PRESENTATION_REPRESENTATION (  '', ( #115025 ), #94248 ) ;
#101184 = CARTESIAN_POINT ( 'NONE',  ( -6.183988606268994381, 28.73617430169791476, 5.000000000000000000 ) ) ;
#101185 = CARTESIAN_POINT ( 'NONE',  ( 34.92499999999998295, -22.22500000000000142, 4.500000000000000888 ) ) ;
#101187 = EDGE_CURVE ( 'NONE', #89674, #3009, #64159, .T. ) ;
#101186 = FACE_OUTER_BOUND ( 'NONE', #111298, .T. ) ;
#101188 = ORIENTED_EDGE ( 'NONE', *, *, #133421, .F. ) ;
#101189 = DIRECTION ( 'NONE',  ( -0.3543493200069163240, -0.000000000000000000, 0.9351131265310288487 ) ) ;
#101190 = DIRECTION ( 'NONE',  ( -0.000000000000000000, 0.000000000000000000, 1.000000000000000000 ) ) ;
#101191 = CARTESIAN_POINT ( 'NONE',  ( -6.707106781186501721, 20.25929247661552424, 5.000000000000000000 ) ) ;
#101192 = CARTESIAN_POINT ( 'NONE',  ( 25.40000000000000213, 7.943993692193106249, -0.1521560028100145123 ) ) ;
#101194 = LINE ( 'NONE', #1832, #35850 ) ;
#101193 = CARTESIAN_POINT ( 'NONE',  ( 68.95833333333332860, 3.974999999999997424, 6.884901960086288852 ) ) ;
#101195 = LINE ( 'NONE', #1833, #141094 ) ;
#101196 = LINE ( 'NONE', #35974, #46811 ) ;
#101197 = ORIENTED_EDGE ( 'NONE', *, *, #36450, .F. ) ;
#101198 = CARTESIAN_POINT ( 'NONE',  ( -59.99451991528749772, 28.92564299267980132, 4.000000000000000000 ) ) ;
#101199 = PLANE ( 'NONE',  #127540 ) ;
#101200 = ORIENTED_EDGE ( 'NONE', *, *, #32301, .T. ) ;
#101201 = ORIENTED_EDGE ( 'NONE', *, *, #22341, .T. ) ;
#101202 = EDGE_CURVE ( 'NONE', #56149, #94083, #8990, .T. ) ;
#101203 = VERTEX_POINT ( 'NONE', #11147 ) ;
#101204 = CARTESIAN_POINT ( 'NONE',  ( 53.66709685856477563, -3.055000000000000160, -5.291415217122921177 ) ) ;
#101205 = AXIS2_PLACEMENT_3D ( 'NONE', #10967, #111003, #75561 ) ;
#101206 = ORIENTED_EDGE ( 'NONE', *, *, #136392, .F. ) ;
#101207 = CARTESIAN_POINT ( 'NONE',  ( -12.20000000000000284, -34.64999999999999147, -40.00000000000000000 ) ) ;
#101208 = VECTOR ( 'NONE', #3164, 1000.000000000000000 ) ;
#101209 = CARTESIAN_POINT ( 'NONE',  ( 3.108306282870439752, 1.633150327867687324, -6.094999999999991758 ) ) ;
#101210 = CARTESIAN_POINT ( 'NONE',  ( 88.37543019189811844, -5.291415217122920289, -3.055000000000001492 ) ) ;
#101211 = LINE ( 'NONE', #69322, #140069 ) ;
#101212 = ORIENTED_EDGE ( 'NONE', *, *, #15901, .T. ) ;
#101213 = ORIENTED_EDGE ( 'NONE', *, *, #40780, .T. ) ;
#101214 = CARTESIAN_POINT ( 'NONE',  ( -34.82816939922328459, 6.759292476615660128, 4.000000000000000000 ) ) ;
#101215 = VECTOR ( 'NONE', #15018, 1000.000000000000000 ) ;
#101216 = LINE ( 'NONE', #1858, #72563 ) ;
#101217 = ORIENTED_EDGE ( 'NONE', *, *, #63195, .T. ) ;
#101218 =( BOUNDED_CURVE ( )  B_SPLINE_CURVE ( 2, ( #125784, #26459, #5387, #113446, #27875, #125047, #50359, #6084, #72146, #138075, #70710, #116318, #15533 ),
 .UNSPECIFIED., .F., .F. ) 
 B_SPLINE_CURVE_WITH_KNOTS ( ( 3, 2, 2, 2, 2, 2, 3 ),
 ( 0.1666666666666666574, 0.1694444444444444531, 0.1722222222222222210, 0.1749999999999999889, 0.1777777777777777846, 0.1805555555555555525, 0.1833333333333333204 ),
 .UNSPECIFIED. ) 
 CURVE ( )  GEOMETRIC_REPRESENTATION_ITEM ( )  RATIONAL_B_SPLINE_CURVE ( ( 1.000000000000000000, 0.9659258262890683122, 1.000000000000000000, 0.9659258262890683122, 1.000000000000000000, 0.9659258262890683122, 1.000000000000000000, 0.9659258262890683122, 1.000000000000000000, 0.9659258262890683122, 1.000000000000000000, 0.9659258262890683122, 1.000000000000000000 ) ) 
 REPRESENTATION_ITEM ( '' )  );
#101219 = CARTESIAN_POINT ( 'NONE',  ( 12.69999999999999751, -34.51840020119763608, 17.97447928118983640 ) ) ;
#101220 = DIRECTION ( 'NONE',  ( -0.000000000000000000, 0.3543493200069153248, 0.9351131265310292928 ) ) ;
#101221 = FACE_OUTER_BOUND ( 'NONE', #14418, .T. ) ;
#101222 = ORIENTED_EDGE ( 'NONE', *, *, #130086, .F. ) ;
#101223 = LINE ( 'NONE', #113520, #71283 ) ;
#101224 = VERTEX_POINT ( 'NONE', #120641 ) ;
#101225 = VERTEX_POINT ( 'NONE', #21359 ) ;
#101226 = ORIENTED_EDGE ( 'NONE', *, *, #101244, .T. ) ;
#101227 = EDGE_CURVE ( 'NONE', #41056, #139347, #44582, .T. ) ;
#101229 = AXIS2_PLACEMENT_3D ( 'NONE', #13554, #99877, #110717 ) ;
#101228 = FILL_AREA_STYLE ('',( #123731 ) ) ;
#101230 = EDGE_CURVE ( 'NONE', #11497, #141976, #41679, .T. ) ;
#101231 = FACE_OUTER_BOUND ( 'NONE', #103679, .T. ) ;
#101232 = DIRECTION ( 'NONE',  ( 0.6830127018922180770, -0.6830127018922204085, -0.2588190451025213501 ) ) ;
#101233 = CARTESIAN_POINT ( 'NONE',  ( -36.29974487139159578, -27.71228299555231445, 4.000000000000000000 ) ) ;
#101235 = EDGE_CURVE ( 'NONE', #87818, #98610, #98212, .T. ) ;
#101234 = EDGE_CURVE ( 'NONE', #36181, #74016, #54016, .T. ) ;
#101236 = ADVANCED_FACE ( 'NONE', ( #85892 ), #66307, .T. ) ;
#101237 = CARTESIAN_POINT ( 'NONE',  ( -69.18398860626899705, 28.73617430169835529, 5.000000000000000000 ) ) ;
#101238 = ORIENTED_EDGE ( 'NONE', *, *, #124096, .F. ) ;
#101239 = PLANE ( 'NONE',  #107492 ) ;
#101240 = EDGE_CURVE ( 'NONE', #90151, #118264, #19909, .T. ) ;
#101241 = EDGE_CURVE ( 'NONE', #113850, #88227, #141722, .T. ) ;
#101242 = CARTESIAN_POINT ( 'NONE',  ( 22.14540314143522082, -2.126176841940958351, -7.934999999999989839 ) ) ;
#101243 = DIRECTION ( 'NONE',  ( -0.7071067811865487940, 0.7071067811865463515, 0.000000000000000000 ) ) ;
#101244 = EDGE_CURVE ( 'NONE', #118849, #121710, #42425, .T. ) ;
#101245 = DIRECTION ( 'NONE',  ( 0.6830127018922180770, -0.6830127018922204085, -0.2588190451025213501 ) ) ;
#101246 = AXIS2_PLACEMENT_3D ( 'NONE', #32744, #44341, #43595 ) ;
#101247 = CARTESIAN_POINT ( 'NONE',  ( -31.92499999999997584, 22.26999999999998181, -14.71147562388301822 ) ) ;
#101248 = ORIENTED_EDGE ( 'NONE', *, *, #30517, .F. ) ;
#101249 = ORIENTED_EDGE ( 'NONE', *, *, #43851, .T. ) ;
#101250 = ADVANCED_FACE ( 'NONE', ( #68467 ), #12372, .T. ) ;
#101251 = ORIENTED_EDGE ( 'NONE', *, *, #85649, .T. ) ;
#101252 = CARTESIAN_POINT ( 'NONE',  ( 57.72916666666665009, 7.950000000000001954, -2.130196079827421762 ) ) ;
#101253 = UNCERTAINTY_MEASURE_WITH_UNIT (LENGTH_MEASURE( 1.000000000000000082E-05 ), #49543, 'distance_accuracy_value', 'NONE');
#101254 = EDGE_CURVE ( 'NONE', #126555, #30495, #11883, .T. ) ;
#101255 = LINE ( 'NONE', #33878, #47326 ) ;
#101256 = LINE ( 'NONE', #37448, #4189 ) ;
#101257 = CARTESIAN_POINT ( 'NONE',  ( 22.49999999999984013, -19.53360074219753884, 5.000000000000000000 ) ) ;
#101258 = EDGE_CURVE ( 'NONE', #118938, #119988, #93413, .T. ) ;
#101260 = AXIS2_PLACEMENT_3D ( 'NONE', #2485, #38025, #115517 ) ;
#101259 = CARTESIAN_POINT ( 'NONE',  ( 24.41159235450331977, 9.902892378096218942E-16, 0.000000000000000000 ) ) ;
#101261 = DIRECTION ( 'NONE',  ( 0.000000000000000000, 0.000000000000000000, 1.000000000000000000 ) ) ;
#101262 = CARTESIAN_POINT ( 'NONE',  ( -12.70000000000000284, -25.33999999999998565, 2.999999999999999112 ) ) ;
#101263 = CARTESIAN_POINT ( 'NONE',  ( 18.18398860626898994, 28.73617430169800002, 5.000000000000000000 ) ) ;
#101264 = PLANE ( 'NONE',  #102013 ) ;
#101265 = VERTEX_POINT ( 'NONE', #58326 ) ;
#101266 = ORIENTED_EDGE ( 'NONE', *, *, #77670, .T. ) ;
#101267 = AXIS2_PLACEMENT_3D ( 'NONE', #122992, #134600, #135319 ) ;
#101268 = EDGE_CURVE ( 'NONE', #122875, #81952, #102507, .T. ) ;
#101269 = DIRECTION ( 'NONE',  ( -0.000000000000000000, 0.000000000000000000, 1.000000000000000000 ) ) ;
#101271 = ORIENTED_EDGE ( 'NONE', *, *, #82055, .T. ) ;
#101270 = DIRECTION ( 'NONE',  ( -0.7071067811865486830, -0.7071067811865464625, 0.000000000000000000 ) ) ;
#101272 = VECTOR ( 'NONE', #25756, 1000.000000000000000 ) ;
#101273 = DIRECTION ( 'NONE',  ( -0.3543493200069162685, -0.000000000000000000, -0.9351131265310288487 ) ) ;
#101274 = CARTESIAN_POINT ( 'NONE',  ( 9.183988606268997046, 28.73617430169793607, 5.000000000000000000 ) ) ;
#101275 = ORIENTED_EDGE ( 'NONE', *, *, #110861, .T. ) ;
#101276 = ORIENTED_EDGE ( 'NONE', *, *, #2911, .T. ) ;
#101277 = DIRECTION ( 'NONE',  ( -0.000000000000000000, -0.3543493200069152693, 0.9351131265310292928 ) ) ;
#101278 = ORIENTED_EDGE ( 'NONE', *, *, #47938, .F. ) ;
#101279 = EDGE_CURVE ( 'NONE', #82336, #19260, #2425, .T. ) ;
#101280 = AXIS2_PLACEMENT_3D ( 'NONE', #87647, #141307, #107933 ) ;
#101281 = AXIS2_PLACEMENT_3D ( 'NONE', #85464, #41254, #138449 ) ;
#101282 = DIRECTION ( 'NONE',  ( 1.000000000000000000, 1.224606353822377258E-16, 0.000000000000000000 ) ) ;
#101284 = CARTESIAN_POINT ( 'NONE',  ( 98.80836038379622721, 7.949999999999997513, 2.130196079827431088 ) ) ;
#101283 = AXIS2_PLACEMENT_3D ( 'NONE', #113249, #49479, #4428 ) ;
#101285 = CARTESIAN_POINT ( 'NONE',  ( -5.999999999999956479, 9.631307414974321190, -9.079085613539556121 ) ) ;
#101286 = DIRECTION ( 'NONE',  ( 0.7071067811865487940, 0.7071067811865463515, 0.000000000000000000 ) ) ;
#101287 = ORIENTED_EDGE ( 'NONE', *, *, #30985, .T. ) ;
#101288 = DIRECTION ( 'NONE',  ( -0.6830127018922181881, 0.6830127018922202975, -0.2588190451025214056 ) ) ;
#101289 = DIRECTION ( 'NONE',  ( -0.3543493200069162685, -0.000000000000000000, -0.9351131265310288487 ) ) ;
#101290 = DIRECTION ( 'NONE',  ( -0.6830127018922180770, -0.6830127018922204085, -0.2588190451025213501 ) ) ;
#101291 = CARTESIAN_POINT ( 'NONE',  ( 12.39583333333333570, 1.633150327867687324, -6.094999999999991758 ) ) ;
#101292 = DIRECTION ( 'NONE',  ( 1.000000000000000000, 0.000000000000000000, 0.000000000000000000 ) ) ;
#101293 = VECTOR ( 'NONE', #74435, 1000.000000000000000 ) ;
#101294 = LINE ( 'NONE', #104117, #83845 ) ;
#101295 = CARTESIAN_POINT ( 'NONE',  ( -6.299744871391586898, -27.71228299555210484, 4.000000000000000000 ) ) ;
#101296 = ORIENTED_EDGE ( 'NONE', *, *, #137788, .T. ) ;
#101297 = CARTESIAN_POINT ( 'NONE',  ( -20.99999999999985079, -2.904428200921332248, -6.989807076074896486 ) ) ;
#101298 = ADVANCED_FACE ( 'NONE', ( #81478 ), #45989, .F. ) ;
#101299 = ORIENTED_EDGE ( 'NONE', *, *, #141152, .T. ) ;
#101300 = CARTESIAN_POINT ( 'NONE',  ( 92.31293019189811844, -1.637169565754159617, -6.110000000000001208 ) ) ;
#101302 = EDGE_CURVE ( 'NONE', #61052, #74659, #124236, .T. ) ;
#101301 = B_SPLINE_CURVE_WITH_KNOTS ( 'NONE', 3,
 ( #49656, #39478, #52462, #63392, #117692, #94531, #27146, #6069, #62651, #17677 ),
 .UNSPECIFIED., .F., .F.,
 ( 4, 2, 2, 2, 4 ),
 ( 0.000000000000000000, 0.0009391669472699282553, 0.001878333894539856511, 0.002817500841809784766, 0.003756667789079713021 ),
 .UNSPECIFIED. ) ;
#101303 = PLANE ( 'NONE',  #101229 ) ;
#101304 = FACE_OUTER_BOUND ( 'NONE', #140612, .T. ) ;
#101305 = FACE_OUTER_BOUND ( 'NONE', #17410, .T. ) ;
#101306 = CARTESIAN_POINT ( 'NONE',  ( 125.9828883629132434, -46.44928942427409169, -35.85226645762418940 ) ) ;
#101307 = ORIENTED_EDGE ( 'NONE', *, *, #130646, .F. ) ;
#101308 = CARTESIAN_POINT ( 'NONE',  ( 54.18398860626899705, 28.73617430169825226, 5.000000000000000000 ) ) ;
#101309 = LINE ( 'NONE', #81739, #113730 ) ;
#101310 = ADVANCED_FACE ( 'NONE', ( #46738 ), #25625, .F. ) ;
#101311 = CARTESIAN_POINT ( 'NONE',  ( -17.29298673570684386, -21.74070752338406720, 4.999753212805220670 ) ) ;
#101312 = EDGE_LOOP ( 'NONE', ( #105767, #68090, #48430, #74372 ) ) ;
#101313 = PLANE ( 'NONE',  #127254 ) ;
#101314 = PLANE ( 'NONE',  #109583 ) ;
#101316 = VERTEX_POINT ( 'NONE', #56171 ) ;
#101315 = DIRECTION ( 'NONE',  ( 0.7071067811865487940, 0.7071067811865463515, 0.000000000000000000 ) ) ;
#101317 = VECTOR ( 'NONE', #119220, 1000.000000000000000 ) ;
#101318 = CARTESIAN_POINT ( 'NONE',  ( 29.29289321881325137, -6.740707523384214639, 5.000000000000000000 ) ) ;
#101319 = CARTESIAN_POINT ( 'NONE',  ( -12.48921356237309155, -27.52281430457064104, 5.000000000000000000 ) ) ;
#101320 = LINE ( 'NONE', #79633, #73383 ) ;
#101321 = CARTESIAN_POINT ( 'NONE',  ( 33.48921356237309510, -27.52281430457078670, 5.000000000000000000 ) ) ;
#101322 = ORIENTED_EDGE ( 'NONE', *, *, #47590, .T. ) ;
#101323 = VERTEX_POINT ( 'NONE', #67008 ) ;
#101324 = ORIENTED_EDGE ( 'NONE', *, *, #95731, .F. ) ;
#101325 = CARTESIAN_POINT ( 'NONE',  ( 79.77126352523144703, 4.472830434245839371, 4.472830434245842035 ) ) ;
#101326 = ORIENTED_EDGE ( 'NONE', *, *, #106127, .F. ) ;
#101327 = EDGE_CURVE ( 'NONE', #108649, #99762, #69901, .T. ) ;
#101328 = LINE ( 'NONE', #79643, #37035 ) ;
#101329 = DIRECTION ( 'NONE',  ( 0.7071067811865486830, -0.7071067811865464625, -0.000000000000000000 ) ) ;
#101330 = PLANE ( 'NONE',  #68935 ) ;
#101331 = CARTESIAN_POINT ( 'NONE',  ( 31.49999999999978684, -14.94781430457067906, 5.000000000000000000 ) ) ;
#101332 = ORIENTED_EDGE ( 'NONE', *, *, #70716, .T. ) ;
#101333 = CARTESIAN_POINT ( 'NONE',  ( 17.51078643762690845, -27.52281430457043143, 5.000000000000000000 ) ) ;
#101334 = LINE ( 'NONE', #133965, #116043 ) ;
#101335 = CARTESIAN_POINT ( 'NONE',  ( -7.499999999999952927, 3.431123077392153053, 4.000000000000000000 ) ) ;
#101336 = CARTESIAN_POINT ( 'NONE',  ( 87.55793019189812298, 6.110000000000000320, -1.637169565754156064 ) ) ;
#101337 = VERTEX_POINT ( 'NONE', #57580 ) ;
#101338 = EDGE_CURVE ( 'NONE', #75799, #106925, #47447, .T. ) ;
#101339 = DIRECTION ( 'NONE',  ( -0.7071067811865486830, -0.7071067811865464625, 0.000000000000000000 ) ) ;
#101340 = DIRECTION ( 'NONE',  ( -0.000000000000000000, 0.000000000000000000, 1.000000000000000000 ) ) ;
#101341 = ORIENTED_EDGE ( 'NONE', *, *, #46718, .F. ) ;
#101342 = ORIENTED_EDGE ( 'NONE', *, *, #7475, .T. ) ;
#101343 = EDGE_CURVE ( 'NONE', #128314, #32532, #135148, .T. ) ;
#101344 = PLANE ( 'NONE',  #102509 ) ;
#101345 = DIRECTION ( 'NONE',  ( 0.000000000000000000, -1.000000000000000000, 0.000000000000000000 ) ) ;
#101346 = CARTESIAN_POINT ( 'NONE',  ( 21.06706980810188412, 2.126176841940952134, -7.934999999999992504 ) ) ;
#101347 = CARTESIAN_POINT ( 'NONE',  ( 25.40000000000000924, -6.239863630333645439, -0.7640341322893426934 ) ) ;
#101348 =( NAMED_UNIT ( * ) SI_UNIT ( $, .STERADIAN. ) SOLID_ANGLE_UNIT ( ) );
#101349 = CARTESIAN_POINT ( 'NONE',  ( -13.10332671766740020, 3.690788593506699300, 4.000000000000000000 ) ) ;
#101350 = CARTESIAN_POINT ( 'NONE',  ( 8.994519915287490619, 28.92564299267944250, 4.000000000000000000 ) ) ;
#101351 =( LENGTH_UNIT ( ) NAMED_UNIT ( * ) SI_UNIT ( .MILLI., .METRE. ) );
#101352 = ADVANCED_FACE ( 'NONE', ( #100354 ), #23489, .F. ) ;
#101353 = EDGE_LOOP ( 'NONE', ( #102235, #42973, #63783, #48006 ) ) ;
#101354 = ORIENTED_EDGE ( 'NONE', *, *, #89221, .F. ) ;
#101355 = CARTESIAN_POINT ( 'NONE',  ( -21.18398860626899349, 28.73617430169802134, 5.000000000000000000 ) ) ;
#101356 = ORIENTED_EDGE ( 'NONE', *, *, #110861, .F. ) ;
#101357 = ORIENTED_EDGE ( 'NONE', *, *, #116657, .F. ) ;
#101358 = EDGE_CURVE ( 'NONE', #7759, #68447, #1005, .T. ) ;
#101359 = AXIS2_PLACEMENT_3D ( 'NONE', #122689, #132899, #56055 ) ;
#101361 = EDGE_CURVE ( 'NONE', #61121, #39262, #35842, .T. ) ;
#101360 = CARTESIAN_POINT ( 'NONE',  ( 8.292893218813404133, 2.259292476615696099, 5.000000000000000000 ) ) ;
#101362 = ORIENTED_EDGE ( 'NONE', *, *, #99012, .T. ) ;
#101363 = CARTESIAN_POINT ( 'NONE',  ( 56.80836038379622011, 7.949999999999996625, 2.130196079827431088 ) ) ;
#101364 = FACE_OUTER_BOUND ( 'NONE', #88642, .T. ) ;
#101365 = DIRECTION ( 'NONE',  ( 0.7071067811865487940, 0.7071067811865463515, 0.000000000000000000 ) ) ;
#101366 = AXIS2_PLACEMENT_3D ( 'NONE', #29365, #76481, #108326 ) ;
#101367 = DIRECTION ( 'NONE',  ( -0.7071067811865487940, 0.7071067811865463515, 0.000000000000000000 ) ) ;
#101368 = ORIENTED_EDGE ( 'NONE', *, *, #41328, .T. ) ;
#101369 = CARTESIAN_POINT ( 'NONE',  ( -2.999999999999981792, -13.39766691384884290, -10.96608748226465124 ) ) ;
#101370 = AXIS2_PLACEMENT_3D ( 'NONE', #25577, #11836, #56119 ) ;
#101371 = ORIENTED_EDGE ( 'NONE', *, *, #112062, .T. ) ;
#101372 = CARTESIAN_POINT ( 'NONE',  ( 0.000000000000000000, 0.000000000000000000, 0.000000000000000000 ) ) ;
#101373 = ORIENTED_EDGE ( 'NONE', *, *, #60001, .F. ) ;
#101374 = LINE ( 'NONE', #46330, #9759 ) ;
#101375 = ADVANCED_FACE ( 'NONE', ( #59036 ), #67759, .F. ) ;
#101376 = ORIENTED_EDGE ( 'NONE', *, *, #105684, .T. ) ;
#101377 = PLANE ( 'NONE',  #25001 ) ;
#101378 = ORIENTED_EDGE ( 'NONE', *, *, #110774, .T. ) ;
#101379 = ORIENTED_EDGE ( 'NONE', *, *, #119556, .F. ) ;
#101380 = VECTOR ( 'NONE', #108471, 1000.000000000000227 ) ;
#101381 = ORIENTED_EDGE ( 'NONE', *, *, #110002, .T. ) ;
#101382 = VECTOR ( 'NONE', #89418, 1000.000000000000000 ) ;
#101383 = CARTESIAN_POINT ( 'NONE',  ( 94.77083333333331439, -7.949999999999998401, -2.130196079827426203 ) ) ;
#101384 = LINE ( 'NONE', #25246, #140126 ) ;
#101385 = CARTESIAN_POINT ( 'NONE',  ( 10.83999999999999986, 9.521314400968980422E-16, 0.000000000000000000 ) ) ;
#101386 = CARTESIAN_POINT ( 'NONE',  ( 11.81601139373100651, 28.73617430169779041, 5.000000000000000000 ) ) ;
#101387 = CARTESIAN_POINT ( 'NONE',  ( 117.3962635252314470, 4.472830434245840259, -4.472830434245838482 ) ) ;
#101388 = FACE_OUTER_BOUND ( 'NONE', #17732, .T. ) ;
#101389 = DIRECTION ( 'NONE',  ( 0.000000000000000000, -1.000000000000000000, 0.000000000000000000 ) ) ;
#101391 = DIRECTION ( 'NONE',  ( 0.3543493200069162685, -0.000000000000000000, -0.9351131265310288487 ) ) ;
#101390 = DIRECTION ( 'NONE',  ( -0.7071067811865486830, 0.7071067811865464625, 0.000000000000000000 ) ) ;
#101392 = CARTESIAN_POINT ( 'NONE',  ( -12.20000000000000107, -40.29840020119761590, 19.55137198191482995 ) ) ;
#101393 = LINE ( 'NONE', #99225, #71415 ) ;
#101394 = VERTEX_POINT ( 'NONE', #103188 ) ;
#101395 = CARTESIAN_POINT ( 'NONE',  ( 51.18398860626899705, 28.73617430169823095, 5.000000000000000000 ) ) ;
#101396 = PLANE ( 'NONE',  #118932 ) ;
#101397 = ORIENTED_EDGE ( 'NONE', *, *, #58516, .F. ) ;
#101398 = ORIENTED_EDGE ( 'NONE', *, *, #95325, .T. ) ;
#101399 = CARTESIAN_POINT ( 'NONE',  ( 48.29974487139158867, -27.71228299555239971, 4.000000000000000000 ) ) ;
#101400 = ORIENTED_EDGE ( 'NONE', *, *, #85839, .F. ) ;
#101401 = VECTOR ( 'NONE', #90349, 1000.000000000000227 ) ;
#101402 = FACE_OUTER_BOUND ( 'NONE', #69937, .T. ) ;
#101403 = CARTESIAN_POINT ( 'NONE',  ( 14.04580628287044064, 5.278424836066143655, -3.047499999999997655 ) ) ;
#101404 = LINE ( 'NONE', #25267, #16155 ) ;
#101405 = DIRECTION ( 'NONE',  ( 0.000000000000000000, 1.000000000000000000, 0.000000000000000000 ) ) ;
#101406 = EDGE_LOOP ( 'NONE', ( #123459, #90020, #43652, #60434 ) ) ;
#101407 = CARTESIAN_POINT ( 'NONE',  ( 25.01899999999999835, 3.174999999999997158, 4.000000000000000000 ) ) ;
#101408 = EDGE_LOOP ( 'NONE', ( #141438, #125731, #138762, #15393 ) ) ;
#101409 =( BOUNDED_CURVE ( )  B_SPLINE_CURVE ( 3, ( #125793, #92412, #56985, #70013 ),
 .UNSPECIFIED., .F., .T. ) 
 B_SPLINE_CURVE_WITH_KNOTS ( ( 4, 4 ),
 ( 5.143245962375958769, 6.645403452391243526 ),
 .UNSPECIFIED. ) 
 CURVE ( )  GEOMETRIC_REPRESENTATION_ITEM ( )  RATIONAL_B_SPLINE_CURVE ( ( 1.000000000000000000, 0.8206354192515232793, 0.8206354192515232793, 1.000000000000000000 ) ) 
 REPRESENTATION_ITEM ( '' )  );
#101410 = CARTESIAN_POINT ( 'NONE',  ( -57.48921356237308800, -27.52281430457095368, 5.000000000000000000 ) ) ;
#101411 = EDGE_CURVE ( 'NONE', #80458, #114963, #80060, .T. ) ;
#101412 = CARTESIAN_POINT ( 'NONE',  ( 21.50456980810188412, 6.871911579029510442, -3.967499999999998916 ) ) ;
#101413 = EDGE_LOOP ( 'NONE', ( #31376, #40265, #34021, #80970 ) ) ;
#101414 = CARTESIAN_POINT ( 'NONE',  ( 83.47459685856478018, 1.637169565754164280, -6.109999999999997655 ) ) ;
#101415 = ADVANCED_FACE ( 'NONE', ( #35114 ), #142180, .T. ) ;
#101416 = FACE_OUTER_BOUND ( 'NONE', #38977, .T. ) ;
#101417 = CARTESIAN_POINT ( 'NONE',  ( -34.47516574401891631, -5.971932658884116840, 4.998110765256836174 ) ) ;
#101418 = ORIENTED_EDGE ( 'NONE', *, *, #114167, .F. ) ;
#101419 = ORIENTED_EDGE ( 'NONE', *, *, #10478, .T. ) ;
#101420 = EDGE_CURVE ( 'NONE', #40729, #16613, #93753, .T. ) ;
#101421 = ORIENTED_EDGE ( 'NONE', *, *, #132071, .T. ) ;
#101422 = FACE_OUTER_BOUND ( 'NONE', #20149, .T. ) ;
#101423 = DIRECTION ( 'NONE',  ( -0.000000000000000000, 0.000000000000000000, 1.000000000000000000 ) ) ;
#101424 = LINE ( 'NONE', #10134, #46547 ) ;
#101426 = VECTOR ( 'NONE', #30065, 1000.000000000000000 ) ;
#101425 = LINE ( 'NONE', #26721, #91389 ) ;
#101427 = EDGE_CURVE ( 'NONE', #119455, #103076, #54136, .T. ) ;
#101428 = DIRECTION ( 'NONE',  ( -0.7071067811865487940, 0.7071067811865463515, 0.000000000000000000 ) ) ;
#101429 = ORIENTED_EDGE ( 'NONE', *, *, #65791, .T. ) ;
#101430 = AXIS2_PLACEMENT_3D ( 'NONE', #91802, #115664, #36707 ) ;
#101431 = ADVANCED_FACE ( 'NONE', ( #48835 ), #70617, .T. ) ;
#101432 =( NAMED_UNIT ( * ) PLANE_ANGLE_UNIT ( ) SI_UNIT ( $, .RADIAN. ) );
#101433 = DIRECTION ( 'NONE',  ( 0.000000000000000000, -1.000000000000000000, 0.000000000000000000 ) ) ;
#101434 = ORIENTED_EDGE ( 'NONE', *, *, #92127, .T. ) ;
#101435 = CARTESIAN_POINT ( 'NONE',  ( 25.49999999999983302, 19.46639925780206326, 5.000000000000000000 ) ) ;
#101436 = ORIENTED_EDGE ( 'NONE', *, *, #825, .T. ) ;
#101437 = EDGE_CURVE ( 'NONE', #38444, #80430, #123664, .T. ) ;
#101438 = VERTEX_POINT ( 'NONE', #105329 ) ;
#101439 = ORIENTED_EDGE ( 'NONE', *, *, #132076, .F. ) ;
#101440 = EDGE_CURVE ( 'NONE', #143191, #20063, #15431, .T. ) ;
#101441 = DIRECTION ( 'NONE',  ( -0.5735764363510499342, -0.8191520442889891340, 0.000000000000000000 ) ) ;
#101442 = CARTESIAN_POINT ( 'NONE',  ( -54.48921356237310221, -27.52281430457093236, 5.000000000000000000 ) ) ;
#101443 = VERTEX_POINT ( 'NONE', #83617 ) ;
#101444 = DIRECTION ( 'NONE',  ( -0.7071067811865486830, 0.7071067811865464625, 0.000000000000000000 ) ) ;
#101445 = ORIENTED_EDGE ( 'NONE', *, *, #17173, .T. ) ;
#101446 = EDGE_CURVE ( 'NONE', #86990, #111757, #104620, .T. ) ;
#101447 = CARTESIAN_POINT ( 'NONE',  ( 27.85005128541007124, -8.240707523384196875, 17.25253755692245861 ) ) ;
#101448 = DIRECTION ( 'NONE',  ( 0.000000000000000000, -1.000000000000000000, 0.000000000000000000 ) ) ;
#101449 = LINE ( 'NONE', #2097, #2195 ) ;
#101450 = AXIS2_PLACEMENT_3D ( 'NONE', #63959, #43613, #20416 ) ;
#101451 = CARTESIAN_POINT ( 'NONE',  ( 18.79289321881332597, -5.240707523384228850, 5.000000000000000000 ) ) ;
#101452 = PLANE ( 'NONE',  #92918 ) ;
#101453 = FACE_OUTER_BOUND ( 'NONE', #14002, .T. ) ;
#101454 = LINE ( 'NONE', #126086, #5414 ) ;
#101455 = CARTESIAN_POINT ( 'NONE',  ( -31.82816939922330945, 6.759292476615653023, 4.000000000000000000 ) ) ;
#101456 = CARTESIAN_POINT ( 'NONE',  ( 17.62456980810188867, -6.871911579029512218, 3.967499999999996252 ) ) ;
#101457 = CARTESIAN_POINT ( 'NONE',  ( 22.17183060077632106, -5.240707523384228850, 4.000000000000000000 ) ) ;
#101458 = LINE ( 'NONE', #135542, #1904 ) ;
#101459 = DIRECTION ( 'NONE',  ( 0.6830127018922180770, -0.6830127018922204085, -0.2588190451025213501 ) ) ;
#101460 = DIRECTION ( 'NONE',  ( 0.7071067811865487940, 0.7071067811865463515, 0.000000000000000000 ) ) ;
#101461 = EDGE_LOOP ( 'NONE', ( #74520, #52288, #3199 ) ) ;
#101462 = ORIENTED_EDGE ( 'NONE', *, *, #28259, .T. ) ;
#101463 = CARTESIAN_POINT ( 'NONE',  ( 87.77083333333331439, -7.949999999999999289, -2.130196079827426203 ) ) ;
#101464 = ORIENTED_EDGE ( 'NONE', *, *, #140070, .T. ) ;
#101465 = EDGE_LOOP ( 'NONE', ( #21622, #66216, #30449, #30458 ) ) ;
#101466 = ORIENTED_EDGE ( 'NONE', *, *, #138594, .T. ) ;
#101467 = EDGE_CURVE ( 'NONE', #73986, #540, #137265, .T. ) ;
#101468 = CARTESIAN_POINT ( 'NONE',  ( -30.65671000166194915, 3.759292476615681888, 13.27625715073258661 ) ) ;
#101469 = CARTESIAN_POINT ( 'NONE',  ( -0.2997448713915885632, -27.71228299555206220, 4.000000000000000000 ) ) ;
#101470 = DIRECTION ( 'NONE',  ( 0.7071067811865486830, -0.7071067811865464625, -0.000000000000000000 ) ) ;
#101471 = VERTEX_POINT ( 'NONE', #82891 ) ;
#101472 = AXIS2_PLACEMENT_3D ( 'NONE', #78040, #123694, #57013 ) ;
#101473 = AXIS2_PLACEMENT_3D ( 'NONE', #136187, #112315, #102866 ) ;
#101474 = LINE ( 'NONE', #56606, #41695 ) ;
#101475 = DIRECTION ( 'NONE',  ( 0.6830127018922180770, -0.6830127018922204085, -0.2588190451025213501 ) ) ;
#101476 = VECTOR ( 'NONE', #99746, 1000.000000000000227 ) ;
#101477 = CARTESIAN_POINT ( 'NONE',  ( 18.48921356237309510, -27.52281430457068367, 5.000000000000000000 ) ) ;
#101478 = CARTESIAN_POINT ( 'NONE',  ( -14.29387692260794118, 22.22500000000000142, 4.000000000000000000 ) ) ;
#101479 = CARTESIAN_POINT ( 'NONE',  ( 19.35292824042819149, -2.786763769301527027, 4.186878071398587586 ) ) ;
#101480 = PLANE ( 'NONE',  #98007 ) ;
#101481 = LINE ( 'NONE', #2134, #88450 ) ;
#101483 = DIRECTION ( 'NONE',  ( -0.7071067811865487940, 0.7071067811865463515, 0.000000000000000000 ) ) ;
#101482 = AXIS2_PLACEMENT_3D ( 'NONE', #44185, #87671, #42044 ) ;
#101484 = CARTESIAN_POINT ( 'NONE',  ( 16.49999999999987566, 1.030536316426515553, -5.498701923753840148 ) ) ;
#101485 = LINE ( 'NONE', #24640, #70899 ) ;
#101486 = VECTOR ( 'NONE', #131156, 1000.000000000000000 ) ;
#101487 = CARTESIAN_POINT ( 'NONE',  ( -21.70710678118639692, -15.74070752338412049, 5.000000000000000000 ) ) ;
#101488 = ADVANCED_FACE ( 'NONE', ( #127080 ), #59719, .F. ) ;
#101489 = LINE ( 'NONE', #21066, #107074 ) ;
#101490 = ORIENTED_EDGE ( 'NONE', *, *, #114101, .F. ) ;
#101491 = ORIENTED_EDGE ( 'NONE', *, *, #53829, .T. ) ;
#101492 = CARTESIAN_POINT ( 'NONE',  ( 122.7920968585647756, -5.291415217122921177, 3.054999999999999272 ) ) ;
#101493 = EDGE_LOOP ( 'NONE', ( #12243, #71662, #15368, #28552 ) ) ;
#101494 = EDGE_CURVE ( 'NONE', #3971, #108000, #127827, .T. ) ;
#101495 = DIRECTION ( 'NONE',  ( -0.6830127018922180770, -0.6830127018922204085, -0.2588190451025213501 ) ) ;
#101496 = LINE ( 'NONE', #113808, #1689 ) ;
#101497 = CARTESIAN_POINT ( 'NONE',  ( 84.18398860626899705, 28.73617430169846187, 5.000000000000000000 ) ) ;
#101498 = DIRECTION ( 'NONE',  ( -1.000000000000000000, -1.224606353822377258E-16, -0.000000000000000000 ) ) ;
#101499 = VECTOR ( 'NONE', #86138, 999.9999999999998863 ) ;
#101500 = CARTESIAN_POINT ( 'NONE',  ( 117.4537635252314516, -6.109999999999998543, -3.741295971395162543E-16 ) ) ;
#101501 = ORIENTED_EDGE ( 'NONE', *, *, #71896, .F. ) ;
#101502 = EDGE_CURVE ( 'NONE', #119845, #53035, #38662, .T. ) ;
#101503 = ORIENTED_EDGE ( 'NONE', *, *, #116656, .T. ) ;
#101504 = CARTESIAN_POINT ( 'NONE',  ( -45.18398860626900415, 28.73617430169818832, 5.000000000000000000 ) ) ;
#101505 = VECTOR ( 'NONE', #39065, 1000.000000000000227 ) ;
#101506 = CARTESIAN_POINT ( 'NONE',  ( 0.000000000000000000, 0.000000000000000000, 5.000000000000000000 ) ) ;
#101507 = VECTOR ( 'NONE', #85742, 1000.000000000000000 ) ;
#101508 = VECTOR ( 'NONE', #90537, 1000.000000000000000 ) ;
#101509 = VERTEX_POINT ( 'NONE', #73439 ) ;
#101510 = EDGE_LOOP ( 'NONE', ( #50497, #82043, #20783, #94091 ) ) ;
#101511 = EDGE_CURVE ( 'NONE', #24720, #19355, #6690, .T. ) ;
#101512 = ORIENTED_EDGE ( 'NONE', *, *, #11243, .F. ) ;
#101513 = CARTESIAN_POINT ( 'NONE',  ( 22.25000000000000000, 0.000000000000000000, 1.749999999999999778 ) ) ;
#101514 = EDGE_CURVE ( 'NONE', #60374, #21741, #40805, .T. ) ;
#101515 = CARTESIAN_POINT ( 'NONE',  ( 28.64126352523144092, 4.472830434245836706, 4.472830434245840259 ) ) ;
#101516 = EDGE_LOOP ( 'NONE', ( #107939, #4945, #75113, #33215 ) ) ;
#101517 = ORIENTED_EDGE ( 'NONE', *, *, #45307, .T. ) ;
#101518 = CARTESIAN_POINT ( 'NONE',  ( 1.516262732464673579, 0.4000000000000001887, -2.467792535850613866 ) ) ;
#101519 = VERTEX_POINT ( 'NONE', #71303 ) ;
#101520 = VERTEX_POINT ( 'NONE', #115458 ) ;
#101521 = ORIENTED_EDGE ( 'NONE', *, *, #117436, .F. ) ;
#101522 = VECTOR ( 'NONE', #64726, 1000.000000000000000 ) ;
#101523 = PLANE ( 'NONE',  #49485 ) ;
#101524 = CARTESIAN_POINT ( 'NONE',  ( 26.40000000000000568, -16.48000000000005016, 34.92499999999998295 ) ) ;
#101525 = LINE ( 'NONE', #124014, #111301 ) ;
#101526 = EDGE_CURVE ( 'NONE', #40992, #96671, #27772, .T. ) ;
#101527 = EDGE_LOOP ( 'NONE', ( #81741, #127802, #71722, #79815 ) ) ;
#101528 = DIRECTION ( 'NONE',  ( 1.000000000000000000, 0.000000000000000000, 0.000000000000000000 ) ) ;
#101529 = FILL_AREA_STYLE_COLOUR ( '', #4237 ) ;
#101530 = DIRECTION ( 'NONE',  ( -0.7071067811865486830, -0.7071067811865464625, 0.000000000000000000 ) ) ;
#101531 = ADVANCED_FACE ( 'NONE', ( #94449 ), #72769, .F. ) ;
#101532 = FACE_BOUND ( 'NONE', #80718, .T. ) ;
#101533 = ORIENTED_EDGE ( 'NONE', *, *, #83599, .T. ) ;
#101534 = DIRECTION ( 'NONE',  ( -0.3543493200069162685, -0.000000000000000000, -0.9351131265310288487 ) ) ;
#101535 = CARTESIAN_POINT ( 'NONE',  ( -12.70000000000000462, -22.26999999999999247, -40.00000000000000000 ) ) ;
#101536 = DIRECTION ( 'NONE',  ( -1.000000000000000000, -1.224606353822377258E-16, -0.000000000000000000 ) ) ;
#101538 = EDGE_CURVE ( 'NONE', #101635, #130156, #106019, .T. ) ;
#101537 = DIRECTION ( 'NONE',  ( 0.7071067811865487940, -0.7071067811865463515, 0.000000000000000000 ) ) ;
#101539 = ORIENTED_EDGE ( 'NONE', *, *, #102888, .F. ) ;
#101540 = CYLINDRICAL_SURFACE ( 'NONE', #57432, 0.5000000000000004441 ) ;
#101541 = ORIENTED_EDGE ( 'NONE', *, *, #93484, .F. ) ;
#101542 = VERTEX_POINT ( 'NONE', #139435 ) ;
#101543 = ORIENTED_EDGE ( 'NONE', *, *, #116370, .F. ) ;
#101544 = CARTESIAN_POINT ( 'NONE',  ( 45.84959685856478018, 6.109999999999996767, 1.637169565754163836 ) ) ;
#101545 = ORIENTED_EDGE ( 'NONE', *, *, #88197, .F. ) ;
#101546 = DIRECTION ( 'NONE',  ( 0.7071067811865487940, 0.7071067811865463515, 0.000000000000000000 ) ) ;
#101547 = DIRECTION ( 'NONE',  ( -1.000000000000000000, -1.224606353822377258E-16, -0.000000000000000000 ) ) ;
#101548 = VERTEX_POINT ( 'NONE', #84334 ) ;
#101549 = CARTESIAN_POINT ( 'NONE',  ( 25.97159235450331849, -2.500000000000000000, 3.061616997868384127E-16 ) ) ;
#101550 = CARTESIAN_POINT ( 'NONE',  ( -27.00548008471251293, 28.92564299267919381, 4.000000000000000000 ) ) ;
#101551 = EDGE_CURVE ( 'NONE', #20167, #34213, #7427, .T. ) ;
#101552 = FACE_OUTER_BOUND ( 'NONE', #69298, .T. ) ;
#101553 = DIRECTION ( 'NONE',  ( -0.000000000000000000, 0.3543493200069153248, 0.9351131265310292928 ) ) ;
#101554 = DIRECTION ( 'NONE',  ( -0.000000000000000000, 0.000000000000000000, 1.000000000000000000 ) ) ;
#101555 = FACE_OUTER_BOUND ( 'NONE', #66724, .T. ) ;
#101556 = ORIENTED_EDGE ( 'NONE', *, *, #34724, .T. ) ;
#101557 = ORIENTED_EDGE ( 'NONE', *, *, #49934, .T. ) ;
#101558 = EDGE_LOOP ( 'NONE', ( #82307, #46160, #6643, #89915 ) ) ;
#101559 = ORIENTED_EDGE ( 'NONE', *, *, #138957, .F. ) ;
#101560 = DIRECTION ( 'NONE',  ( -0.7071067811865487940, 0.7071067811865463515, -0.000000000000000000 ) ) ;
#101561 = VECTOR ( 'NONE', #125992, 1000.000000000000114 ) ;
#101562 = AXIS2_PLACEMENT_3D ( 'NONE', #8481, #110662, #52734 ) ;
#101563 = VERTEX_POINT ( 'NONE', #31358 ) ;
#101564 = VECTOR ( 'NONE', #92791, 1000.000000000000227 ) ;
#101566 = ORIENTED_EDGE ( 'NONE', *, *, #5281, .T. ) ;
#101565 = VECTOR ( 'NONE', #84786, 1000.000000000000000 ) ;
#101567 = FILL_AREA_STYLE ('',( #89974 ) ) ;
#101568 = CARTESIAN_POINT ( 'NONE',  ( 32.20710678118632586, -5.240707523384230626, 5.000000000000000000 ) ) ;
#101569 = VERTEX_POINT ( 'NONE', #75578 ) ;
#101570 = FACE_OUTER_BOUND ( 'NONE', #8303, .T. ) ;
#101571 = STYLED_ITEM ( 'NONE', ( #42603 ), #124980 ) ;
#101572 = VECTOR ( 'NONE', #2458, 1000.000000000000000 ) ;
#101573 = LINE ( 'NONE', #134232, #44472 ) ;
#101574 = CARTESIAN_POINT ( 'NONE',  ( 25.15040314143521627, 7.934999999999989839, -2.126176841940961904 ) ) ;
#101575 = EDGE_CURVE ( 'NONE', #123357, #88687, #19412, .T. ) ;
#101576 = DIRECTION ( 'NONE',  ( 0.7071067811865487940, -0.7071067811865463515, 0.000000000000000000 ) ) ;
#101577 = ORIENTED_EDGE ( 'NONE', *, *, #93811, .T. ) ;
#101579 = DIRECTION ( 'NONE',  ( -0.7071067811865486830, -0.7071067811865464625, 0.000000000000000000 ) ) ;
#101578 = CARTESIAN_POINT ( 'NONE',  ( 113.2245968585647944, -1.637169565754161171, 6.109999999999998543 ) ) ;
#101580 = EDGE_CURVE ( 'NONE', #111310, #305, #8471, .T. ) ;
#101581 = FACE_OUTER_BOUND ( 'NONE', #48975, .T. ) ;
#101582 = DIRECTION ( 'NONE',  ( -0.000000000000000000, -0.9647414015272163246, 0.2631995976047502017 ) ) ;
#101583 = ORIENTED_EDGE ( 'NONE', *, *, #43215, .F. ) ;
#101584 = LINE ( 'NONE', #2246, #31044 ) ;
#101586 = ORIENTED_EDGE ( 'NONE', *, *, #121714, .T. ) ;
#101585 = PLANE ( 'NONE',  #130590 ) ;
#101587 = AXIS2_PLACEMENT_3D ( 'NONE', #69570, #61551, #15127 ) ;
#101588 = LINE ( 'NONE', #100882, #74060 ) ;
#101589 = EDGE_LOOP ( 'NONE', ( #130985, #99451, #42835, #131845 ) ) ;
#101590 = CARTESIAN_POINT ( 'NONE',  ( -12.20000000000000284, -34.64999999999999147, -39.50000000000000000 ) ) ;
#101591 = CARTESIAN_POINT ( 'NONE',  ( 6.499999999999999112, 7.960204194457794491E-16, 10.00000000000000000 ) ) ;
#101592 = PLANE ( 'NONE',  #91034 ) ;
#101593 = ADVANCED_FACE ( 'NONE', ( #119749 ), #3160, .T. ) ;
#101594 = EDGE_CURVE ( 'NONE', #23245, #27314, #65437, .T. ) ;
#101595 = DIRECTION ( 'NONE',  ( 0.000000000000000000, -1.000000000000000000, 0.000000000000000000 ) ) ;
#101596 = ORIENTED_EDGE ( 'NONE', *, *, #15388, .T. ) ;
#101597 = CARTESIAN_POINT ( 'NONE',  ( -34.42500000000001137, -22.22500000000000142, 5.000000000000000000 ) ) ;
#101598 =( GEOMETRIC_REPRESENTATION_CONTEXT ( 3 ) GLOBAL_UNCERTAINTY_ASSIGNED_CONTEXT ( ( #79421 ) ) GLOBAL_UNIT_ASSIGNED_CONTEXT ( ( #126590, #27281, #139669 ) ) REPRESENTATION_CONTEXT ( 'NONE', 'WORKASPACE' ) );
#101599 = CARTESIAN_POINT ( 'NONE',  ( -21.48921356237309155, -27.52281430457070499, 5.000000000000000000 ) ) ;
#101600 = DIRECTION ( 'NONE',  ( -0.6830127018922180770, -0.6830127018922204085, -0.2588190451025213501 ) ) ;
#101601 = ORIENTED_EDGE ( 'NONE', *, *, #70004, .F. ) ;
#101602 = COLOUR_RGB ( '', 0.40784314, 0.44705882, 0.49803922) ;
#101604 = CIRCLE ( 'NONE', #129337, 5.968999999999998529 ) ;
#101603 = LINE ( 'NONE', #124087, #100217 ) ;
#101605 = ORIENTED_EDGE ( 'NONE', *, *, #27130, .T. ) ;
#101606 = VECTOR ( 'NONE', #57792, 1000.000000000000000 ) ;
#101607 = EDGE_CURVE ( 'NONE', #37108, #113729, #97273, .T. ) ;
#101608 = DIRECTION ( 'NONE',  ( -0.000000000000000000, -0.3543493200069152693, 0.9351131265310292928 ) ) ;
#101610 = ORIENTED_EDGE ( 'NONE', *, *, #80022, .T. ) ;
#101609 = CARTESIAN_POINT ( 'NONE',  ( -24.29974487139158867, -27.71228299555223273, 4.000000000000000000 ) ) ;
#101611 = EDGE_CURVE ( 'NONE', #54692, #44739, #142274, .T. ) ;
#101612 = ORIENTED_EDGE ( 'NONE', *, *, #131219, .F. ) ;
#101613 = CARTESIAN_POINT ( 'NONE',  ( 9.990891321718962104, 11.37382169669887055, -26.06733581495564422 ) ) ;
#101614 =( GEOMETRIC_REPRESENTATION_CONTEXT ( 3 ) GLOBAL_UNCERTAINTY_ASSIGNED_CONTEXT ( ( #44818 ) ) GLOBAL_UNIT_ASSIGNED_CONTEXT ( ( #99293, #103583, #136224 ) ) REPRESENTATION_CONTEXT ( 'NONE', 'WORKASPACE' ) );
#101615 = DIRECTION ( 'NONE',  ( 1.000000000000000000, 0.000000000000000000, 0.000000000000000000 ) ) ;
#101616 = ORIENTED_EDGE ( 'NONE', *, *, #88700, .F. ) ;
#101617 = VECTOR ( 'NONE', #9335, 1000.000000000000000 ) ;
#101618 = ADVANCED_FACE ( 'NONE', ( #53078 ), #142957, .F. ) ;
#101619 = LINE ( 'NONE', #71686, #34459 ) ;
#101620 = CARTESIAN_POINT ( 'NONE',  ( 23.78840764549667597, 9.139736423841732040E-16, 0.000000000000000000 ) ) ;
#101621 = ORIENTED_EDGE ( 'NONE', *, *, #120441, .T. ) ;
#101622 = CARTESIAN_POINT ( 'NONE',  ( 0.000000000000000000, 0.000000000000000000, 5.000000000000000000 ) ) ;
#101623 = CARTESIAN_POINT ( 'NONE',  ( 12.29974487139158512, -27.71228299555214747, 4.000000000000000000 ) ) ;
#101624 = DIRECTION ( 'NONE',  ( 1.000000000000000000, 0.000000000000000000, 0.000000000000000000 ) ) ;
#101625 = EDGE_CURVE ( 'NONE', #118545, #101563, #29903, .T. ) ;
#101626 = VECTOR ( 'NONE', #37984, 1000.000000000000000 ) ;
#101627 = LINE ( 'NONE', #13879, #81796 ) ;
#101628 = DIRECTION ( 'NONE',  ( 1.000000000000000000, 0.000000000000000000, 0.000000000000000000 ) ) ;
#101629 = DIRECTION ( 'NONE',  ( -0.3543493200069162685, -0.000000000000000000, -0.9351131265310288487 ) ) ;
#101630 = ORIENTED_EDGE ( 'NONE', *, *, #98051, .F. ) ;
#101631 = ORIENTED_EDGE ( 'NONE', *, *, #5607, .T. ) ;
#101632 = VERTEX_POINT ( 'NONE', #20447 ) ;
#101633 = CARTESIAN_POINT ( 'NONE',  ( 123.2083333333333428, -3.974999999999999201, -6.884901960086287964 ) ) ;
#101634 = ORIENTED_EDGE ( 'NONE', *, *, #126914, .F. ) ;
#101635 = VERTEX_POINT ( 'NONE', #87155 ) ;
#101636 = ORIENTED_EDGE ( 'NONE', *, *, #69297, .T. ) ;
#101637 = EDGE_CURVE ( 'NONE', #11327, #53362, #100466, .T. ) ;
#101638 = CARTESIAN_POINT ( 'NONE',  ( 1.425881352870889796, -2.124795774637151080, -6.328817049275281548 ) ) ;
#101639 = CARTESIAN_POINT ( 'NONE',  ( -34.49999999999976552, -2.173586137069173585, -4.605770156576189045 ) ) ;
#101640 = EDGE_LOOP ( 'NONE', ( #119998, #58901, #123614, #140910, #108122 ) ) ;
#101641 = DIRECTION ( 'NONE',  ( 0.7071067811865486830, -0.7071067811865464625, -0.000000000000000000 ) ) ;
#101642 = CARTESIAN_POINT ( 'NONE',  ( 127.2418942207595478, -46.18886352141520035, 34.92499999999998295 ) ) ;
#101643 = CARTESIAN_POINT ( 'NONE',  ( -17.29289321881333308, -9.740707523384182664, 5.000000000000000000 ) ) ;
#101644 = CARTESIAN_POINT ( 'NONE',  ( -81.48921356237309510, -27.52281430457112066, 5.000000000000000000 ) ) ;
#101645 = CARTESIAN_POINT ( 'NONE',  ( 118.2712635252314470, 4.472830434245839371, 4.472830434245842035 ) ) ;
#101646 = ORIENTED_EDGE ( 'NONE', *, *, #67017, .T. ) ;
#101647 = EDGE_CURVE ( 'NONE', #49817, #137771, #118338, .T. ) ;
#101648 = CARTESIAN_POINT ( 'NONE',  ( -54.48921356237310221, -27.52281430457093236, 5.000000000000000000 ) ) ;
#101649 = CARTESIAN_POINT ( 'NONE',  ( 105.9541937171295700, 6.884901960086283523, 3.975000000000002753 ) ) ;
#101650 = EDGE_CURVE ( 'NONE', #92907, #34958, #74885, .T. ) ;
#101651 = CARTESIAN_POINT ( 'NONE',  ( -16.49999999999987566, 19.46639925780206326, 5.000000000000000000 ) ) ;
#101652 = CARTESIAN_POINT ( 'NONE',  ( 0.6405549847417550957, 7.449887432306902646, -0.4886591319612960671 ) ) ;
#101653 = FACE_OUTER_BOUND ( 'NONE', #8559, .T. ) ;
#101654 = LINE ( 'NONE', #81370, #40010 ) ;
#101655 = LINE ( 'NONE', #2313, #69003 ) ;
#101656 = CARTESIAN_POINT ( 'NONE',  ( 43.82919371712955581, -3.975000000000001865, 6.884901960086284411 ) ) ;
#101657 = EDGE_CURVE ( 'NONE', #140051, #94242, #63304, .T. ) ;
#101658 = LINE ( 'NONE', #35008, #102356 ) ;
#101659 = DIRECTION ( 'NONE',  ( -1.000000000000000000, -0.000000000000000000, -0.000000000000000000 ) ) ;
#101660 = ORIENTED_EDGE ( 'NONE', *, *, #84426, .F. ) ;
#101661 = EDGE_LOOP ( 'NONE', ( #138998, #7009, #74307, #47754 ) ) ;
#101662 = CARTESIAN_POINT ( 'NONE',  ( 45.91666666666666430, -6.884901960086287076, -3.975000000000000977 ) ) ;
#101663 = ORIENTED_EDGE ( 'NONE', *, *, #82165, .T. ) ;
#101664 = CARTESIAN_POINT ( 'NONE',  ( -34.45011844616455221, -10.48371918836241257, 5.000000000000000888 ) ) ;
#101665 = EDGE_LOOP ( 'NONE', ( #134417, #136299, #100435 ) ) ;
#101666 = DIRECTION ( 'NONE',  ( 0.7071067811865487940, -0.7071067811865463515, 0.000000000000000000 ) ) ;
#101667 = PLANE ( 'NONE',  #19084 ) ;
#101668 = CARTESIAN_POINT ( 'NONE',  ( 40.54209685856477563, 5.291415217122923842, -3.054999999999996163 ) ) ;
#101669 = ORIENTED_EDGE ( 'NONE', *, *, #91935, .T. ) ;
#101670 = EDGE_CURVE ( 'NONE', #81264, #110646, #107473, .T. ) ;
#101671 = DIRECTION ( 'NONE',  ( -0.7071067811865486830, -0.7071067811865464625, -0.000000000000000000 ) ) ;
#101673 = ORIENTED_EDGE ( 'NONE', *, *, #56461, .T. ) ;
#101672 = STYLED_ITEM ( 'NONE', ( #86386 ), #939 ) ;
#101674 = LINE ( 'NONE', #111860, #61293 ) ;
#101675 = VECTOR ( 'NONE', #81616, 1000.000000000000000 ) ;
#101676 = AXIS2_PLACEMENT_3D ( 'NONE', #136310, #36995, #130328 ) ;
#101677 = VECTOR ( 'NONE', #55522, 1000.000000000000000 ) ;
#101678 = CARTESIAN_POINT ( 'NONE',  ( 153.4000000000000057, 26.96999999999993847, -34.92499999999998295 ) ) ;
#101680 =( BOUNDED_CURVE ( )  B_SPLINE_CURVE ( 3, ( #42071, #109444, #53654, #65259 ),
 .UNSPECIFIED., .F., .F. ) 
 B_SPLINE_CURVE_WITH_KNOTS ( ( 4, 4 ),
 ( 5.043186909253406291, 5.074607125596344304 ),
 .UNSPECIFIED. ) 
 CURVE ( )  GEOMETRIC_REPRESENTATION_ITEM ( )  RATIONAL_B_SPLINE_CURVE ( ( 1.000000000000000000, 0.9999177325257868620, 0.9999177325257868620, 1.000000000000000000 ) ) 
 REPRESENTATION_ITEM ( '' )  );
#101679 = CARTESIAN_POINT ( 'NONE',  ( -25.49999999999982236, 10.46639925780215563, 5.000000000000000000 ) ) ;
#101681 = AXIS2_PLACEMENT_3D ( 'NONE', #67335, #111528, #102815 ) ;
#101682 = CARTESIAN_POINT ( 'NONE',  ( -7.940000000000007496, -39.92999999999999261, -7.752100000000004876 ) ) ;
#101683 = ORIENTED_EDGE ( 'NONE', *, *, #7484, .F. ) ;
#101684 = LINE ( 'NONE', #79279, #134534 ) ;
#101685 = EDGE_CURVE ( 'NONE', #60588, #107292, #54551, .T. ) ;
#101686 = ORIENTED_EDGE ( 'NONE', *, *, #98453, .F. ) ;
#101687 = CARTESIAN_POINT ( 'NONE',  ( 0.000000000000000000, 0.000000000000000000, 5.000000000000000000 ) ) ;
#101688 = DIRECTION ( 'NONE',  ( 0.7071067811865487940, 0.7071067811865463515, 0.000000000000000000 ) ) ;
#101689 = DIRECTION ( 'NONE',  ( -0.7071067811865486830, -0.7071067811865464625, -0.000000000000000000 ) ) ;
#101690 = DIRECTION ( 'NONE',  ( -0.7071067811865486830, 0.7071067811865464625, 0.000000000000000000 ) ) ;
#101691 = DIRECTION ( 'NONE',  ( -1.000000000000000000, -1.224606353822377258E-16, -0.000000000000000000 ) ) ;
#101692 = VECTOR ( 'NONE', #113200, 1000.000000000000000 ) ;
#101693 = CARTESIAN_POINT ( 'NONE',  ( 87.72502705046289861, 5.819803920172573974, -5.819803920172573086 ) ) ;
#101694 = CARTESIAN_POINT ( 'NONE',  ( 62.03709685856478728, -3.054999999999998828, -5.291415217122919401 ) ) ;
#101695 = CARTESIAN_POINT ( 'NONE',  ( 7.251592354503322291, 9.902892378096218942E-16, 0.000000000000000000 ) ) ;
#101696 = ADVANCED_FACE ( 'NONE', ( #108154 ), #108869, .F. ) ;
#101697 = DIRECTION ( 'NONE',  ( 4.681814790819592407E-17, 0.3543493200069153248, 0.9351131265310292928 ) ) ;
#101699 = ORIENTED_EDGE ( 'NONE', *, *, #71492, .T. ) ;
#101698 = DIRECTION ( 'NONE',  ( 1.000000000000000000, 0.000000000000000000, 0.000000000000000000 ) ) ;
#101700 = ORIENTED_EDGE ( 'NONE', *, *, #93971, .F. ) ;
#101701 = VECTOR ( 'NONE', #103399, 1000.000000000000000 ) ;
#101702 = AXIS2_PLACEMENT_3D ( 'NONE', #90067, #58226, #24121 ) ;
#101703 = PLANE ( 'NONE',  #74742 ) ;
#101704 = ORIENTED_EDGE ( 'NONE', *, *, #70586, .F. ) ;
#101705 =( GEOMETRIC_REPRESENTATION_CONTEXT ( 3 ) GLOBAL_UNCERTAINTY_ASSIGNED_CONTEXT ( ( #21424 ) ) GLOBAL_UNIT_ASSIGNED_CONTEXT ( ( #3737, #92197, #81374 ) ) REPRESENTATION_CONTEXT ( 'NONE', 'WORKASPACE' ) );
#101706 = DIRECTION ( 'NONE',  ( 0.000000000000000000, 0.000000000000000000, -1.000000000000000000 ) ) ;
#101707 = EDGE_CURVE ( 'NONE', #87888, #69646, #32062, .T. ) ;
#101708 = VERTEX_POINT ( 'NONE', #120450 ) ;
#101709 = DIRECTION ( 'NONE',  ( 0.3543493200069162685, -0.000000000000000000, -0.9351131265310288487 ) ) ;
#101710 = CARTESIAN_POINT ( 'NONE',  ( 28.49999999999980815, -2.568876922607781221, 4.000000000000000000 ) ) ;
#101711 = CARTESIAN_POINT ( 'NONE',  ( 17.29298673570682254, -21.74070752338406720, 4.999753212805220670 ) ) ;
#101712 = VECTOR ( 'NONE', #117538, 999.9999999999998863 ) ;
#101713 = VECTOR ( 'NONE', #24949, 1000.000000000000000 ) ;
#101715 = VECTOR ( 'NONE', #26220, 1000.000000000000000 ) ;
#101714 = CARTESIAN_POINT ( 'NONE',  ( 1.953608656376216022E-15, -6.270000000000002238, -37.00000000000000000 ) ) ;
#101716 = EDGE_CURVE ( 'NONE', #64740, #122408, #87869, .T. ) ;
#101717 = FACE_BOUND ( 'NONE', #75760, .T. ) ;
#101718 = CARTESIAN_POINT ( 'NONE',  ( 63.18398860626900415, 28.73617430169831621, 5.000000000000000000 ) ) ;
#101719 = CARTESIAN_POINT ( 'NONE',  ( 8.585466709768445170, 3.821174125832445049E-16, 0.000000000000000000 ) ) ;
#101720 = EDGE_CURVE ( 'NONE', #103883, #24621, #77024, .T. ) ;
#101721 = LINE ( 'NONE', #98852, #115105 ) ;
#101723 = ORIENTED_EDGE ( 'NONE', *, *, #142549, .F. ) ;
#101722 = DIRECTION ( 'NONE',  ( -0.7071067811865486830, -0.7071067811865464625, -0.000000000000000000 ) ) ;
#101724 = VECTOR ( 'NONE', #125190, 1000.000000000000227 ) ;
#101725 = ORIENTED_EDGE ( 'NONE', *, *, #81653, .F. ) ;
#101726 = AXIS2_PLACEMENT_3D ( 'NONE', #17760, #53072, #115629 ) ;
#101727 = DIRECTION ( 'NONE',  ( 0.7071067811865487940, 0.7071067811865463515, 0.000000000000000000 ) ) ;
#101728 = EDGE_LOOP ( 'NONE', ( #24767, #113907, #34170, #107407 ) ) ;
#101729 = EDGE_LOOP ( 'NONE', ( #56696, #110886, #12840 ) ) ;
#101730 = CARTESIAN_POINT ( 'NONE',  ( 76.91209685856479439, 5.291415217122921177, -3.054999999999994831 ) ) ;
#101731 = ORIENTED_EDGE ( 'NONE', *, *, #117008, .T. ) ;
#101732 = EDGE_CURVE ( 'NONE', #85633, #4933, #33521, .T. ) ;
#101733 = CARTESIAN_POINT ( 'NONE',  ( -10.06996025486402502, -0.7407075233842770334, 13.87443053587613129 ) ) ;
#101734 = VERTEX_POINT ( 'NONE', #2987 ) ;
#101735 = CARTESIAN_POINT ( 'NONE',  ( 12.48921356237309155, -27.52281430457064104, 5.000000000000000000 ) ) ;
#101736 = AXIS2_PLACEMENT_3D ( 'NONE', #849, #56735, #21908 ) ;
#101737 = EDGE_CURVE ( 'NONE', #72846, #126683, #113170, .T. ) ;
#101738 = DIRECTION ( 'NONE',  ( -0.3543493200069163240, -0.000000000000000000, 0.9351131265310288487 ) ) ;
#101739 = CARTESIAN_POINT ( 'NONE',  ( 12.19999999999999574, -59.76999999999998892, -40.00000000000000000 ) ) ;
#101740 = DIRECTION ( 'NONE',  ( 0.7071067811865486830, -0.7071067811865464625, -0.000000000000000000 ) ) ;
#101742 = CARTESIAN_POINT ( 'NONE',  ( -27.18398860626900060, 28.73617430169806042, 5.000000000000000000 ) ) ;
#101741 = CYLINDRICAL_SURFACE ( 'NONE', #34331, 7.950000000000000178 ) ;
#101743 = LINE ( 'NONE', #33661, #9959 ) ;
#101744 = DIRECTION ( 'NONE',  ( 1.000000000000000000, 0.000000000000000000, 0.000000000000000000 ) ) ;
#101745 = ORIENTED_EDGE ( 'NONE', *, *, #73493, .F. ) ;
#101746 = EDGE_CURVE ( 'NONE', #87121, #27504, #137511, .T. ) ;
#101747 = ORIENTED_EDGE ( 'NONE', *, *, #104535, .T. ) ;
#101748 = CARTESIAN_POINT ( 'NONE',  ( -18.51789069628991768, -2.771357050275779610, 4.325358181756085330 ) ) ;
#101749 = PLANE ( 'NONE',  #14211 ) ;
#101750 = VERTEX_POINT ( 'NONE', #122627 ) ;
#101751 = ORIENTED_EDGE ( 'NONE', *, *, #135297, .F. ) ;
#101752 = VERTEX_POINT ( 'NONE', #100880 ) ;
#101753 = CARTESIAN_POINT ( 'NONE',  ( 30.91709685856476497, 3.054999999999998828, 5.291415217122922066 ) ) ;
#101754 = ORIENTED_EDGE ( 'NONE', *, *, #106639, .T. ) ;
#101755 = PLANE ( 'NONE',  #69484 ) ;
#101756 = DIRECTION ( 'NONE',  ( 0.7071067811865486830, -0.7071067811865464625, -0.000000000000000000 ) ) ;
#101757 = CARTESIAN_POINT ( 'NONE',  ( -1.682930191898113881, -2.126176841940956130, 7.934999999999991616 ) ) ;
#101758 = CARTESIAN_POINT ( 'NONE',  ( 16.45742106731621490, 0.9613713492673662264, -33.49048331797056477 ) ) ;
#101759 = VERTEX_POINT ( 'NONE', #1534 ) ;
#101760 = DIRECTION ( 'NONE',  ( 0.7071067811865487940, 0.7071067811865463515, -0.000000000000000000 ) ) ;
#101761 = EDGE_CURVE ( 'NONE', #13547, #87703, #133524, .T. ) ;
#101762 = CARTESIAN_POINT ( 'NONE',  ( -57.29974487139158157, -27.71228299555246011, 4.000000000000000000 ) ) ;
#101763 = DIRECTION ( 'NONE',  ( -1.000000000000000000, 0.000000000000000000, -0.000000000000000000 ) ) ;
#101765 = VERTEX_POINT ( 'NONE', #46560 ) ;
#101764 = DIRECTION ( 'NONE',  ( 0.6830127018922180770, -0.6830127018922204085, -0.2588190451025213501 ) ) ;
#101766 = ORIENTED_EDGE ( 'NONE', *, *, #94714, .T. ) ;
#101767 = LINE ( 'NONE', #47450, #42656 ) ;
#101768 = DIRECTION ( 'NONE',  ( 0.000000000000000000, -1.000000000000000000, 0.000000000000000000 ) ) ;
#101769 = ADVANCED_FACE ( 'NONE', ( #102339 ), #66838, .T. ) ;
#101770 = ADVANCED_FACE ( 'NONE', ( #24046 ), #121897, .F. ) ;
#101771 = CARTESIAN_POINT ( 'NONE',  ( -5.700255128608413102, -27.71228299555201957, 4.000000000000000000 ) ) ;
#101772 = ORIENTED_EDGE ( 'NONE', *, *, #88721, .F. ) ;
#101773 = DIRECTION ( 'NONE',  ( -0.6830127018922181881, 0.6830127018922202975, -0.2588190451025214056 ) ) ;
#101774 = SURFACE_STYLE_USAGE ( .BOTH. , #57591 ) ;
#101775 = CARTESIAN_POINT ( 'NONE',  ( 62.99451991528749772, 28.92564299267982264, 4.000000000000000000 ) ) ;
#101776 = CARTESIAN_POINT ( 'NONE',  ( -32.29289321881323360, 20.25929247661551003, 5.000000000000000000 ) ) ;
#101777 = MECHANICAL_DESIGN_GEOMETRIC_PRESENTATION_REPRESENTATION (  '', ( #39178 ), #104021 ) ;
#101778 = AXIS2_PLACEMENT_3D ( 'NONE', #54908, #75243, #97675 ) ;
#101779 = AXIS2_PLACEMENT_3D ( 'NONE', #123385, #58143, #124778 ) ;
#101780 = LINE ( 'NONE', #80074, #76031 ) ;
#101781 = EDGE_CURVE ( 'NONE', #51968, #46484, #13134, .T. ) ;
#101782 = DIRECTION ( 'NONE',  ( 0.7071067811865486830, -0.7071067811865464625, -0.000000000000000000 ) ) ;
#101783 = AXIS2_PLACEMENT_3D ( 'NONE', #128667, #49710, #107615 ) ;
#101784 = FACE_OUTER_BOUND ( 'NONE', #27821, .T. ) ;
#101785 = EDGE_CURVE ( 'NONE', #75355, #18399, #79899, .T. ) ;
#101786 = CARTESIAN_POINT ( 'NONE',  ( 23.20710678118638981, -11.24070752338417201, 5.000000000000000000 ) ) ;
#101787 = ORIENTED_EDGE ( 'NONE', *, *, #52070, .T. ) ;
#101788 = ADVANCED_FACE ( 'NONE', ( #124074 ), #101585, .F. ) ;
#101789 = ORIENTED_EDGE ( 'NONE', *, *, #20617, .T. ) ;
#101790 = COLOUR_RGB ( '', 0.09019608, 0.27058824, 0.51372549) ;
#101791 = CARTESIAN_POINT ( 'NONE',  ( 0.000000000000000000, 0.000000000000000000, 5.000000000000000000 ) ) ;
#101792 = CARTESIAN_POINT ( 'NONE',  ( 0.1245698081018861286, -6.871911579029512218, 3.967499999999996252 ) ) ;
#101793 = CARTESIAN_POINT ( 'NONE',  ( 30.48921356237309510, -27.52281430457076894, 5.000000000000000000 ) ) ;
#101794 = EDGE_CURVE ( 'NONE', #98472, #42161, #45123, .T. ) ;
#101795 = VECTOR ( 'NONE', #63318, 1000.000000000000000 ) ;
#101796 = CARTESIAN_POINT ( 'NONE',  ( 7.499999999999947597, -19.53360074219753884, 5.000000000000000000 ) ) ;
#101797 = CARTESIAN_POINT ( 'NONE',  ( 75.29974487139158157, -27.71228299555258445, 4.000000000000000000 ) ) ;
#101798 = ADVANCED_FACE ( 'NONE', ( #88605 ), #11698, .F. ) ;
#101799 = LINE ( 'NONE', #132323, #127865 ) ;
#101800 = VERTEX_POINT ( 'NONE', #89300 ) ;
#101801 = SURFACE_STYLE_FILL_AREA ( #3192 ) ;
#101802 = CARTESIAN_POINT ( 'NONE',  ( 12.18398860626900060, 28.73617430169795739, 5.000000000000000000 ) ) ;
#101803 = AXIS2_PLACEMENT_3D ( 'NONE', #111650, #132723, #113051 ) ;
#101804 = AXIS2_PLACEMENT_3D ( 'NONE', #120907, #63706, #140515 ) ;
#101805 = EDGE_CURVE ( 'NONE', #128291, #66418, #68993, .T. ) ;
#101806 = CARTESIAN_POINT ( 'NONE',  ( -7.140000000000001457, -35.14999999999999147, -39.50000000000000000 ) ) ;
#101807 = CARTESIAN_POINT ( 'NONE',  ( 59.84959685856477307, 6.109999999999997655, 1.637169565754163836 ) ) ;
#101808 = DIRECTION ( 'NONE',  ( 0.7071067811865487940, 0.7071067811865463515, -0.000000000000000000 ) ) ;
#101809 = VECTOR ( 'NONE', #109876, 1000.000000000000000 ) ;
#101810 = DIRECTION ( 'NONE',  ( 0.6830127018922180770, 0.6830127018922202975, -0.2588190451025213501 ) ) ;
#101811 = DIRECTION ( 'NONE',  ( -1.000000000000000000, -0.000000000000000000, -0.000000000000000000 ) ) ;
#101812 = VERTEX_POINT ( 'NONE', #134976 ) ;
#101813 = CARTESIAN_POINT ( 'NONE',  ( -5.241399257802002332, 21.72500000000000853, 5.000000000000000000 ) ) ;
#101814 = ORIENTED_EDGE ( 'NONE', *, *, #57461, .F. ) ;
#101815 = ADVANCED_FACE ( 'NONE', ( #35674 ), #118550, .F. ) ;
#101816 = DIRECTION ( 'NONE',  ( 0.000000000000000000, 1.000000000000000000, 0.000000000000000000 ) ) ;
#101817 = VECTOR ( 'NONE', #43216, 1000.000000000000000 ) ;
#101818 = CONICAL_SURFACE ( 'NONE', #6771, 2.055000000000000604, 0.9599310885968764806 ) ;
#101819 = VECTOR ( 'NONE', #46230, 999.9999999999998863 ) ;
#101820 = DIRECTION ( 'NONE',  ( 0.7071067811865486830, -0.7071067811865464625, -0.000000000000000000 ) ) ;
#101821 = DIRECTION ( 'NONE',  ( 1.000000000000000000, -0.000000000000000000, -0.000000000000000000 ) ) ;
#101822 = LINE ( 'NONE', #125000, #9169 ) ;
#101823 = CARTESIAN_POINT ( 'NONE',  ( 3.096670641874039287, -2.240707523384260824, 15.26439735382753149 ) ) ;
#101824 = CARTESIAN_POINT ( 'NONE',  ( 26.28769006033953914, -21.73547319004781286, 4.999917730833664642 ) ) ;
#101825 = CONICAL_SURFACE ( 'NONE', #106438, 2.500000000000000444, 0.9599310885968830309 ) ;
#101826 = VERTEX_POINT ( 'NONE', #19250 ) ;
#101827 = ORIENTED_EDGE ( 'NONE', *, *, #8861, .T. ) ;
#101828 = DIRECTION ( 'NONE',  ( 0.7071067811865487940, -0.7071067811865463515, 0.000000000000000000 ) ) ;
#101829 = CARTESIAN_POINT ( 'NONE',  ( 0.1839886062690032631, 28.73617430169787568, 5.000000000000000000 ) ) ;
#101830 = CIRCLE ( 'NONE', #111008, 2.055000000000001048 ) ;
#101831 = CARTESIAN_POINT ( 'NONE',  ( 0.000000000000000000, -7.600000000000061817, 28.92499999999998650 ) ) ;
#101832 = CARTESIAN_POINT ( 'NONE',  ( 78.18398860626899705, 28.73617430169841924, 5.000000000000000000 ) ) ;
#101833 = CARTESIAN_POINT ( 'NONE',  ( 74.30836038379624142, 7.949999999999997513, 2.130196079827431088 ) ) ;
#101835 = EDGE_CURVE ( 'NONE', #94364, #3251, #119950, .T. ) ;
#101834 = FACE_OUTER_BOUND ( 'NONE', #69698, .T. ) ;
#101836 = CARTESIAN_POINT ( 'NONE',  ( -19.49999999999986500, -12.08601207473291161, -10.46905243149090481 ) ) ;
#101837 = EDGE_LOOP ( 'NONE', ( #3226, #64304, #142507, #564 ) ) ;
#101838 = CARTESIAN_POINT ( 'NONE',  ( 77.85416666666667140, -2.130196079827425315, -7.950000000000001066 ) ) ;
#101839 = LINE ( 'NONE', #115523, #79325 ) ;
#101840 = CARTESIAN_POINT ( 'NONE',  ( 72.48921356237309510, -27.52281430457106026, 5.000000000000000000 ) ) ;
#101841 = CYLINDRICAL_SURFACE ( 'NONE', #116912, 2.500000000000000444 ) ;
#101842 = AXIS2_PLACEMENT_3D ( 'NONE', #60856, #75806, #104282 ) ;
#101843 = ORIENTED_EDGE ( 'NONE', *, *, #79343, .F. ) ;
#101844 = EDGE_CURVE ( 'NONE', #52145, #11858, #63506, .T. ) ;
#101845 = DIRECTION ( 'NONE',  ( -0.7071067811865487940, 0.7071067811865463515, 0.000000000000000000 ) ) ;
#101846 = CARTESIAN_POINT ( 'NONE',  ( 6.066782984417857350, 4.584330080086930965E-16, 0.000000000000000000 ) ) ;
#101847 = CARTESIAN_POINT ( 'NONE',  ( 68.83376352523143282, 6.110000000000001208, 1.122388791418549305E-15 ) ) ;
#101848 = DIRECTION ( 'NONE',  ( -1.000000000000000000, -0.000000000000000000, -0.000000000000000000 ) ) ;
#101849 = EDGE_LOOP ( 'NONE', ( #14549, #130314, #96920, #51322 ) ) ;
#101850 = VERTEX_POINT ( 'NONE', #75787 ) ;
#101851 = VECTOR ( 'NONE', #140788, 1000.000000000000227 ) ;
#101852 = CARTESIAN_POINT ( 'NONE',  ( -33.51665438641022376, 22.22500000000000142, 4.500000000000000888 ) ) ;
#101853 = LINE ( 'NONE', #22828, #141533 ) ;
#101854 = LINE ( 'NONE', #1778, #74184 ) ;
#101855 = DIRECTION ( 'NONE',  ( 0.6830127018922181881, 0.6830127018922202975, -0.2588190451025214056 ) ) ;
#101857 = ORIENTED_EDGE ( 'NONE', *, *, #132612, .T. ) ;
#101856 = CARTESIAN_POINT ( 'NONE',  ( 84.99999999999998579, 0.000000000000000000, -7.950000000000000178 ) ) ;
#101858 = DIRECTION ( 'NONE',  ( 0.7071067811865487940, -0.7071067811865463515, 0.000000000000000000 ) ) ;
#101859 = DIRECTION ( 'NONE',  ( 1.000000000000000000, 0.000000000000000000, 0.000000000000000000 ) ) ;
#101860 = DIRECTION ( 'NONE',  ( -0.7071067811865486830, -0.7071067811865464625, -0.000000000000000000 ) ) ;
#101861 = SURFACE_STYLE_USAGE ( .BOTH. , #91017 ) ;
#101862 = EDGE_LOOP ( 'NONE', ( #55830, #38113, #48576, #59575 ) ) ;
#101863 = ORIENTED_EDGE ( 'NONE', *, *, #94382, .F. ) ;
#101864 = CARTESIAN_POINT ( 'NONE',  ( 56.29209685856477563, -5.291415217122921177, 3.054999999999999272 ) ) ;
#101865 = EDGE_LOOP ( 'NONE', ( #131277, #124914, #17267, #21932 ) ) ;
#101866 = CARTESIAN_POINT ( 'NONE',  ( -12.69999999999998153, 3.061616997868383634E-16, -2.500000000000000444 ) ) ;
#101867 = PLANE ( 'NONE',  #66577 ) ;
#101868 = DIRECTION ( 'NONE',  ( 0.000000000000000000, 1.000000000000000000, 0.000000000000000000 ) ) ;
#101869 = CARTESIAN_POINT ( 'NONE',  ( -39.48921356237310221, -27.52281430457082934, 5.000000000000000000 ) ) ;
#101870 = CARTESIAN_POINT ( 'NONE',  ( -34.49999999999975842, 4.464255608400450548, 4.994342998332166772 ) ) ;
#101871 = ORIENTED_EDGE ( 'NONE', *, *, #127631, .F. ) ;
#101872 = ORIENTED_EDGE ( 'NONE', *, *, #82652, .T. ) ;
#101873 = DIRECTION ( 'NONE',  ( 0.000000000000000000, 0.000000000000000000, 1.000000000000000000 ) ) ;
#101874 = DIRECTION ( 'NONE',  ( 0.000000000000000000, 1.000000000000000000, 0.000000000000000000 ) ) ;
#101876 = VERTEX_POINT ( 'NONE', #19948 ) ;
#101875 = VECTOR ( 'NONE', #92659, 999.9999999999998863 ) ;
#101877 = CARTESIAN_POINT ( 'NONE',  ( 5.281315875828549444, 4.584330080086930965E-16, 0.000000000000000000 ) ) ;
#101878 = CARTESIAN_POINT ( 'NONE',  ( 113.2458603837962272, 3.974999999999996980, 6.884901960086287964 ) ) ;
#101879 = CARTESIAN_POINT ( 'NONE',  ( 14.60438740478481989, -0.8081507193758268315, 4.000000000000000000 ) ) ;
#101880 = VECTOR ( 'NONE', #68979, 1000.000000000000000 ) ;
#101881 = AXIS2_PLACEMENT_3D ( 'NONE', #104459, #70471, #25465 ) ;
#101882 = CIRCLE ( 'NONE', #39401, 2.500000000000000444 ) ;
#101883 = ORIENTED_EDGE ( 'NONE', *, *, #134458, .T. ) ;
#101885 = ADVANCED_FACE ( 'NONE', ( #76510 ), #20658, .T. ) ;
#101884 = PRESENTATION_LAYER_ASSIGNMENT (  '', '', ( #90396 ) ) ;
#101886 = EDGE_CURVE ( 'NONE', #47321, #30178, #53293, .T. ) ;
#101887 = FACE_BOUND ( 'NONE', #143317, .T. ) ;
#101888 = LINE ( 'NONE', #67132, #105777 ) ;
#101889 = DIRECTION ( 'NONE',  ( 0.7071067811865486830, -0.7071067811865464625, -0.000000000000000000 ) ) ;
#101890 = FACE_OUTER_BOUND ( 'NONE', #59579, .T. ) ;
#101891 = VECTOR ( 'NONE', #49075, 999.9999999999998863 ) ;
#101892 = DIRECTION ( 'NONE',  ( 0.000000000000000000, 0.000000000000000000, 1.000000000000000000 ) ) ;
#101893 = EDGE_CURVE ( 'NONE', #103695, #97839, #52582, .T. ) ;
#101894 = ADVANCED_FACE ( 'NONE', ( #64913 ), #85204, .F. ) ;
#101895 = CARTESIAN_POINT ( 'NONE',  ( 0.000000000000000000, 0.000000000000000000, 5.000000000000000000 ) ) ;
#101896 = DIRECTION ( 'NONE',  ( -0.6639864884492345798, 0.6060772209810636468, 0.4379410295516115159 ) ) ;
#101897 = ORIENTED_EDGE ( 'NONE', *, *, #124018, .T. ) ;
#101898 = ORIENTED_EDGE ( 'NONE', *, *, #29920, .T. ) ;
#101899 = CARTESIAN_POINT ( 'NONE',  ( 100.6829301918981088, -1.637169565754158951, -6.109999999999998543 ) ) ;
#101900 = ORIENTED_EDGE ( 'NONE', *, *, #47864, .T. ) ;
#101901 = EDGE_CURVE ( 'NONE', #38919, #85630, #132664, .T. ) ;
#101902 = CARTESIAN_POINT ( 'NONE',  ( -15.18398860626900237, 28.73617430169797871, 5.000000000000000000 ) ) ;
#101903 = VERTEX_POINT ( 'NONE', #9789 ) ;
#101904 = VECTOR ( 'NONE', #105727, 1000.000000000000000 ) ;
#101905 = FACE_OUTER_BOUND ( 'NONE', #84104, .T. ) ;
#101906 = DIRECTION ( 'NONE',  ( -0.7071067811865486830, -0.7071067811865464625, 0.000000000000000000 ) ) ;
#101907 = ADVANCED_FACE ( 'NONE', ( #109098 ), #96760, .T. ) ;
#101908 = VECTOR ( 'NONE', #42335, 1000.000000000000000 ) ;
#101909 = DIRECTION ( 'NONE',  ( 0.7071067811865487940, 0.7071067811865463515, 0.000000000000000000 ) ) ;
#101910 = EDGE_LOOP ( 'NONE', ( #55821, #120733, #24929, #120863 ) ) ;
#101911 = CARTESIAN_POINT ( 'NONE',  ( 21.79289321881330821, -14.24070752338414003, 5.000000000000000000 ) ) ;
#101912 = DIRECTION ( 'NONE',  ( 0.3543493200069162685, -0.000000000000000000, -0.9351131265310288487 ) ) ;
#101913 = LINE ( 'NONE', #2575, #140664 ) ;
#101914 = CARTESIAN_POINT ( 'NONE',  ( -26.99999999999980815, -3.412538124160723108, 4.000000000000000000 ) ) ;
#101915 = VECTOR ( 'NONE', #33747, 1000.000000000000000 ) ;
#101916 = CARTESIAN_POINT ( 'NONE',  ( 10.49999999999992362, 21.05218569542895679, 5.000000000000000000 ) ) ;
#101917 = ADVANCED_FACE ( 'NONE', ( #30113 ), #40320, .T. ) ;
#101918 = PLANE ( 'NONE',  #69979 ) ;
#101919 = EDGE_LOOP ( 'NONE', ( #103154, #90680, #87137, #41939 ) ) ;
#101920 = AXIS2_PLACEMENT_3D ( 'NONE', #72471, #60142, #104308 ) ;
#101921 = DIRECTION ( 'NONE',  ( -0.7071067811865487940, 0.7071067811865463515, -0.000000000000000000 ) ) ;
#101922 = DIRECTION ( 'NONE',  ( 0.3543493200069163240, -0.000000000000000000, 0.9351131265310288487 ) ) ;
#101923 = ORIENTED_EDGE ( 'NONE', *, *, #7999, .F. ) ;
#101924 = ORIENTED_EDGE ( 'NONE', *, *, #86387, .F. ) ;
#101925 = VECTOR ( 'NONE', #44786, 1000.000000000000000 ) ;
#101926 = ORIENTED_EDGE ( 'NONE', *, *, #118658, .F. ) ;
#101927 = CARTESIAN_POINT ( 'NONE',  ( 57.02126352523143993, -4.472830434245838482, -4.472830434245840259 ) ) ;
#101928 = EDGE_CURVE ( 'NONE', #44583, #143262, #54060, .T. ) ;
#101929 = ORIENTED_EDGE ( 'NONE', *, *, #41601, .T. ) ;
#101930 = AXIS2_PLACEMENT_3D ( 'NONE', #128648, #96690, #29320 ) ;
#101931 = CARTESIAN_POINT ( 'NONE',  ( 7.774972949537104938, 4.461849672132300881, 4.461849672132299105 ) ) ;
#101932 = CARTESIAN_POINT ( 'NONE',  ( 90.70876352523143282, -7.482591942790329030E-16, 6.110000000000001208 ) ) ;
#101933 = CARTESIAN_POINT ( 'NONE',  ( -24.48921356237309510, -27.52281430457072631, 5.000000000000000000 ) ) ;
#101934 = ORIENTED_EDGE ( 'NONE', *, *, #114068, .F. ) ;
#101935 = FACE_OUTER_BOUND ( 'NONE', #4486, .T. ) ;
#101936 = EDGE_CURVE ( 'NONE', #49860, #142463, #41718, .T. ) ;
#101937 = ORIENTED_EDGE ( 'NONE', *, *, #70482, .T. ) ;
#101938 = LINE ( 'NONE', #37399, #101991 ) ;
#101939 = AXIS2_PLACEMENT_3D ( 'NONE', #114123, #59079, #125736 ) ;
#101940 = DIRECTION ( 'NONE',  ( 1.321231229586337907E-16, -0.9647414015272156584, 0.2631995976047526442 ) ) ;
#101941 = ORIENTED_EDGE ( 'NONE', *, *, #45534, .T. ) ;
#101942 = CARTESIAN_POINT ( 'NONE',  ( 29.99451991528749417, 28.92564299267958816, 4.000000000000000000 ) ) ;
#101943 = LINE ( 'NONE', #35294, #140935 ) ;
#101944 = ADVANCED_FACE ( 'NONE', ( #130168 ), #87372, .T. ) ;
#101946 = EDGE_CURVE ( 'NONE', #110269, #27958, #141763, .T. ) ;
#101945 = CARTESIAN_POINT ( 'NONE',  ( 125.6204301918981088, 3.055000000000002380, -5.291415217122917625 ) ) ;
#101947 = ORIENTED_EDGE ( 'NONE', *, *, #124068, .F. ) ;
#101948 = CARTESIAN_POINT ( 'NONE',  ( 19.00193056682084247, -22.22500000000000142, 4.500000000000000888 ) ) ;
#101949 = ORIENTED_EDGE ( 'NONE', *, *, #40129, .T. ) ;
#101950 = ORIENTED_EDGE ( 'NONE', *, *, #57503, .T. ) ;
#101951 = ORIENTED_EDGE ( 'NONE', *, *, #61266, .F. ) ;
#101952 = LINE ( 'NONE', #3327, #37809 ) ;
#101953 = CIRCLE ( 'NONE', #41828, 2.500000000000000888 ) ;
#101954 = EDGE_CURVE ( 'NONE', #122361, #96060, #130892, .T. ) ;
#101955 = CARTESIAN_POINT ( 'NONE',  ( 13.21321903303351242, 12.75929247661559351, 10.29404684609038334 ) ) ;
#101956 = EDGE_CURVE ( 'NONE', #61607, #37747, #18500, .T. ) ;
#101957 = DIRECTION ( 'NONE',  ( 0.7071067811865487940, 0.7071067811865463515, 0.000000000000000000 ) ) ;
#101958 = DIRECTION ( 'NONE',  ( -0.3543493200069162685, -0.000000000000000000, -0.9351131265310288487 ) ) ;
#101959 = EDGE_LOOP ( 'NONE', ( #96627, #67238, #101287, #18286, #60212 ) ) ;
#101960 = VECTOR ( 'NONE', #101273, 1000.000000000000227 ) ;
#101961 = VECTOR ( 'NONE', #39209, 1000.000000000000000 ) ;
#101962 = CARTESIAN_POINT ( 'NONE',  ( 24.48921356237309510, -27.52281430457072631, 5.000000000000000000 ) ) ;
#101963 = CARTESIAN_POINT ( 'NONE',  ( 21.99956980810188867, -3.967499999999998028, -6.871911579029511330 ) ) ;
#101964 = CARTESIAN_POINT ( 'NONE',  ( 30.29177708983029405, -15.74070752338411339, 19.73771281079104156 ) ) ;
#101965 = CARTESIAN_POINT ( 'NONE',  ( -23.42830866441053317, 7.233000843196644603, 4.333645886165178318 ) ) ;
#101966 = EDGE_CURVE ( 'NONE', #133473, #83408, #96078, .T. ) ;
#101967 = LINE ( 'NONE', #2634, #21145 ) ;
#101968 = ORIENTED_EDGE ( 'NONE', *, *, #25258, .F. ) ;
#101969 = ORIENTED_EDGE ( 'NONE', *, *, #191, .T. ) ;
#101970 = EDGE_LOOP ( 'NONE', ( #24335, #131915, #119520, #12677 ) ) ;
#101971 = DIRECTION ( 'NONE',  ( -0.6830127018922180770, -0.6830127018922204085, -0.2588190451025213501 ) ) ;
#101972 = CARTESIAN_POINT ( 'NONE',  ( 13.49999999999990052, -12.08601207473287964, -10.46905243149097409 ) ) ;
#101974 = ADVANCED_FACE ( 'NONE', ( #100393 ), #14552, .T. ) ;
#101973 = VECTOR ( 'NONE', #110979, 999.9999999999998863 ) ;
#101975 = CARTESIAN_POINT ( 'NONE',  ( 27.53159235450332076, 9.902892378096218942E-16, 0.000000000000000000 ) ) ;
#101976 = CARTESIAN_POINT ( 'NONE',  ( 6.536636313907743911, 9.243372422612678108, -2.206661907051261640 ) ) ;
#101977 = AXIS2_PLACEMENT_3D ( 'NONE', #142053, #107243, #42741 ) ;
#101978 = VECTOR ( 'NONE', #119849, 1000.000000000000000 ) ;
#101979 = DIRECTION ( 'NONE',  ( 0.6830127018922180770, -0.6830127018922204085, -0.2588190451025213501 ) ) ;
#101980 = CARTESIAN_POINT ( 'NONE',  ( -19.05000000000000071, 3.174999999999997158, 4.000000000000000000 ) ) ;
#101981 = LINE ( 'NONE', #24418, #97618 ) ;
#101982 = PLANE ( 'NONE',  #88295 ) ;
#101983 = CARTESIAN_POINT ( 'NONE',  ( 17.07999999999999829, 9.521314400968980422E-16, 0.000000000000000000 ) ) ;
#101984 = ORIENTED_EDGE ( 'NONE', *, *, #22878, .F. ) ;
#101985 = AXIS2_PLACEMENT_3D ( 'NONE', #24559, #103527, #9766 ) ;
#101986 = VECTOR ( 'NONE', #1911, 1000.000000000000000 ) ;
#101987 = VECTOR ( 'NONE', #142628, 1000.000000000000000 ) ;
#101989 = CARTESIAN_POINT ( 'NONE',  ( 17.42520222878246372, -2.544454608235909188, -33.49760814689099675 ) ) ;
#101988 = CIRCLE ( 'NONE', #127776, 2.500000000000000888 ) ;
#101990 = VERTEX_POINT ( 'NONE', #43869 ) ;
#101991 = VECTOR ( 'NONE', #114238, 999.9999999999998863 ) ;
#101992 = CARTESIAN_POINT ( 'NONE',  ( 16.17183060077635659, -2.240707523384260824, 4.000000000000000000 ) ) ;
#101994 = ORIENTED_EDGE ( 'NONE', *, *, #2270, .F. ) ;
#101993 = CARTESIAN_POINT ( 'NONE',  ( -34.47516574401892342, 15.02806734111566733, 4.998110765256835286 ) ) ;
#101995 = CARTESIAN_POINT ( 'NONE',  ( 34.92499999999998295, 21.00612307739175222, 4.000000000000000000 ) ) ;
#101996 = PLANE ( 'NONE',  #54163 ) ;
#101997 = EDGE_LOOP ( 'NONE', ( #69433, #53851, #95424, #134260 ) ) ;
#101998 = CARTESIAN_POINT ( 'NONE',  ( -12.48921356237309155, -27.52281430457064104, 5.000000000000000000 ) ) ;
#101999 = ORIENTED_EDGE ( 'NONE', *, *, #88071, .T. ) ;
#102000 = CARTESIAN_POINT ( 'NONE',  ( -1.179999999999998606, -6.391994993740215847, 6.750000000000000888 ) ) ;
#102001 = AXIS2_PLACEMENT_3D ( 'NONE', #28922, #126107, #38375 ) ;
#102002 = ORIENTED_EDGE ( 'NONE', *, *, #58480, .F. ) ;
#102003 = CARTESIAN_POINT ( 'NONE',  ( 6.712309939660229041, -21.73547319004781286, 4.999917730833665530 ) ) ;
#102004 = CARTESIAN_POINT ( 'NONE',  ( 102.3083603837962130, 7.949999999999997513, 2.130196079827431088 ) ) ;
#102005 = CARTESIAN_POINT ( 'NONE',  ( 15.98840764549667703, 9.139736423841732040E-16, 0.000000000000000000 ) ) ;
#102006 = CARTESIAN_POINT ( 'NONE',  ( 19.30725242247703122, 9.139235811853160030, 4.261625515810899323 ) ) ;
#102007 = ORIENTED_EDGE ( 'NONE', *, *, #52460, .T. ) ;
#102008 = DIRECTION ( 'NONE',  ( -0.7071067811865487940, 0.7071067811865463515, -0.000000000000000000 ) ) ;
#102009 = CARTESIAN_POINT ( 'NONE',  ( 18.48921356237309510, -27.52281430457068367, 5.000000000000000000 ) ) ;
#102010 = LINE ( 'NONE', #36061, #60041 ) ;
#102011 = CARTESIAN_POINT ( 'NONE',  ( 14.29166666666666785, -3.047499999999994547, 5.278424836066145431 ) ) ;
#102013 = AXIS2_PLACEMENT_3D ( 'NONE', #46213, #90389, #134638 ) ;
#102012 = CARTESIAN_POINT ( 'NONE',  ( 22.58290314143522082, 3.967499999999992699, -6.871911579029513994 ) ) ;
#102014 = FACE_OUTER_BOUND ( 'NONE', #41996, .T. ) ;
#102015 = FACE_OUTER_BOUND ( 'NONE', #91769, .T. ) ;
#102016 = ORIENTED_EDGE ( 'NONE', *, *, #49502, .T. ) ;
#102017 = AXIS2_PLACEMENT_3D ( 'NONE', #93679, #5906, #50179 ) ;
#102018 = DIRECTION ( 'NONE',  ( 0.7071067811865487940, -0.7071067811865463515, 0.000000000000000000 ) ) ;
#102019 = ORIENTED_EDGE ( 'NONE', *, *, #96343, .T. ) ;
#102020 = CIRCLE ( 'NONE', #30192, 0.5000000000000004441 ) ;
#102021 = CARTESIAN_POINT ( 'NONE',  ( 95.52126352523141861, -4.472830434245839371, -4.472830434245840259 ) ) ;
#102022 = VECTOR ( 'NONE', #21945, 1000.000000000000000 ) ;
#102023 = LINE ( 'NONE', #65867, #131141 ) ;
#102024 = FACE_OUTER_BOUND ( 'NONE', #128878, .T. ) ;
#102025 = LINE ( 'NONE', #66548, #42401 ) ;
#102026 = DIRECTION ( 'NONE',  ( -0.6830127018922180770, -0.6830127018922204085, -0.2588190451025213501 ) ) ;
#102027 = VERTEX_POINT ( 'NONE', #67799 ) ;
#102028 = AXIS2_PLACEMENT_3D ( 'NONE', #82388, #17797, #80955 ) ;
#102029 = DIRECTION ( 'NONE',  ( 0.7071067811865487940, 0.7071067811865463515, 0.000000000000000000 ) ) ;
#102030 = FACE_OUTER_BOUND ( 'NONE', #130316, .T. ) ;
#102031 = CARTESIAN_POINT ( 'NONE',  ( 36.29974487139159578, -27.71228299555231445, 4.000000000000000000 ) ) ;
#102032 = ORIENTED_EDGE ( 'NONE', *, *, #110021, .T. ) ;
#102033 = CARTESIAN_POINT ( 'NONE',  ( 24.75149461641275295, 4.949500604449032615, 4.299609778361314305 ) ) ;
#102034 = LINE ( 'NONE', #143387, #802 ) ;
#102036 = ORIENTED_EDGE ( 'NONE', *, *, #53964, .F. ) ;
#102035 = CARTESIAN_POINT ( 'NONE',  ( 12.70710678118645909, 5.259292476615661016, 5.000000000000000000 ) ) ;
#102037 = PLANE ( 'NONE',  #43991 ) ;
#102038 = DIRECTION ( 'NONE',  ( 1.000000000000000000, 0.000000000000000000, 0.000000000000000000 ) ) ;
#102039 = CARTESIAN_POINT ( 'NONE',  ( 36.48921356237310221, -27.52281430457080802, 5.000000000000000000 ) ) ;
#102040 = CARTESIAN_POINT ( 'NONE',  ( 6.183988606268994381, 28.73617430169791476, 5.000000000000000000 ) ) ;
#102041 = SURFACE_STYLE_FILL_AREA ( #37515 ) ;
#102042 = ORIENTED_EDGE ( 'NONE', *, *, #7903, .F. ) ;
#102043 = ORIENTED_EDGE ( 'NONE', *, *, #116715, .F. ) ;
#102044 = EDGE_LOOP ( 'NONE', ( #108496, #69773, #40034, #79607 ) ) ;
#102045 = CARTESIAN_POINT ( 'NONE',  ( 87.35459685856476142, -1.637169565754161615, 6.110000000000000320 ) ) ;
#102046 = VECTOR ( 'NONE', #18327, 1000.000000000000000 ) ;
#102047 = VERTEX_POINT ( 'NONE', #10494 ) ;
#102048 = DIRECTION ( 'NONE',  ( 0.5735764363510444941, 0.8191520442889929088, 0.000000000000000000 ) ) ;
#102049 = CARTESIAN_POINT ( 'NONE',  ( -25.39999999999996305, 0.000000000000000000, 0.000000000000000000 ) ) ;
#102050 = FACE_OUTER_BOUND ( 'NONE', #63242, .T. ) ;
#102051 = DIRECTION ( 'NONE',  ( 1.321231229586337907E-16, -0.9647414015272156584, 0.2631995976047526442 ) ) ;
#102052 = ORIENTED_EDGE ( 'NONE', *, *, #70240, .F. ) ;
#102053 = DIRECTION ( 'NONE',  ( -0.7071067811865487940, 0.7071067811865463515, -0.000000000000000000 ) ) ;
#102054 = DIRECTION ( 'NONE',  ( -0.6830127018922181881, 0.6830127018922202975, -0.2588190451025214056 ) ) ;
#102055 = LINE ( 'NONE', #100640, #127438 ) ;
#102056 = CARTESIAN_POINT ( 'NONE',  ( 78.51626352523145158, -4.472830434245839371, 4.472830434245839371 ) ) ;
#102057 = VERTEX_POINT ( 'NONE', #111989 ) ;
#102058 = CARTESIAN_POINT ( 'NONE',  ( -13.17183060077637435, 21.75929247661549581, 4.000000000000000000 ) ) ;
#102059 = EDGE_CURVE ( 'NONE', #3378, #36518, #665, .T. ) ;
#102060 = LINE ( 'NONE', #1292, #26106 ) ;
#102061 = ORIENTED_EDGE ( 'NONE', *, *, #77573, .T. ) ;
#102062 = ORIENTED_EDGE ( 'NONE', *, *, #54497, .T. ) ;
#102063 = EDGE_CURVE ( 'NONE', #116772, #119169, #318, .T. ) ;
#102064 = PLANE ( 'NONE',  #132639 ) ;
#102065 = EDGE_CURVE ( 'NONE', #30212, #49717, #109827, .T. ) ;
#102066 = EDGE_CURVE ( 'NONE', #83184, #11113, #56211, .T. ) ;
#102067 = DIRECTION ( 'NONE',  ( -0.7071067811865487940, 0.7071067811865463515, -0.000000000000000000 ) ) ;
#102068 = CARTESIAN_POINT ( 'NONE',  ( 24.56706980810188767, 2.126176841940952134, -7.934999999999992504 ) ) ;
#102069 = CARTESIAN_POINT ( 'NONE',  ( -27.18398860626900060, 28.73617430169806042, 5.000000000000000000 ) ) ;
#102070 = VECTOR ( 'NONE', #23364, 999.9999999999998863 ) ;
#102071 = CONICAL_SURFACE ( 'NONE', #118178, 2.055000000000000604, 0.9599310885968764806 ) ;
#102072 = CARTESIAN_POINT ( 'NONE',  ( -13.39656807105348690, -14.24070752338412937, 19.24067776001722763 ) ) ;
#102073 = CARTESIAN_POINT ( 'NONE',  ( -39.48921356237310221, -27.52281430457082934, 5.000000000000000000 ) ) ;
#102074 = EDGE_CURVE ( 'NONE', #127030, #100787, #22087, .T. ) ;
#102075 = EDGE_CURVE ( 'NONE', #72701, #38008, #86279, .T. ) ;
#102076 = CARTESIAN_POINT ( 'NONE',  ( 22.49999999999984013, -13.53360074219759746, 5.000000000000000000 ) ) ;
#102077 = FILL_AREA_STYLE ('',( #91228 ) ) ;
#102078 = ORIENTED_EDGE ( 'NONE', *, *, #95436, .T. ) ;
#102079 = ORIENTED_EDGE ( 'NONE', *, *, #90482, .F. ) ;
#102081 = EDGE_CURVE ( 'NONE', #98477, #25649, #56910, .T. ) ;
#102080 = LINE ( 'NONE', #113653, #131302 ) ;
#102082 = EDGE_LOOP ( 'NONE', ( #21127, #54566, #42203, #121331 ) ) ;
#102083 = ORIENTED_EDGE ( 'NONE', *, *, #80202, .T. ) ;
#102084 = EDGE_CURVE ( 'NONE', #19532, #56087, #13346, .T. ) ;
#102085 = AXIS2_PLACEMENT_3D ( 'NONE', #41319, #44214, #132669 ) ;
#102086 =( BOUNDED_SURFACE ( )  B_SPLINE_SURFACE ( 3, 2, ( 
 ( #72594, #26885, #71131 ),
 ( #93580, #86980, #65980 ),
 ( #21728, #141356, #76110 ),
 ( #131202, #42070, #97095 ) ),
 .UNSPECIFIED., .F., .F., .F. ) 
 B_SPLINE_SURFACE_WITH_KNOTS ( ( 4, 4 ),
 ( 3, 3 ),
 ( -4.336808689942017736E-19, 0.001630001914283392113 ),
 ( 0.000000000000000000, 1.000000000000000000 ),
 .UNSPECIFIED. ) 
 GEOMETRIC_REPRESENTATION_ITEM ( )  RATIONAL_B_SPLINE_SURFACE ( (
 ( 1.000000000000000000, 0.7180326832784531543, 1.000000000000000000),
 ( 1.000000000000000000, 0.7157206429707758666, 1.000000000000000000),
 ( 1.000000000000000000, 0.7121002461815039153, 1.000000000000000000),
 ( 1.000000000000000000, 0.7071067811865475727, 1.000000000000000000) ) ) 
 REPRESENTATION_ITEM ( '' )  SURFACE ( )  );
#102087 = AXIS2_PLACEMENT_3D ( 'NONE', #48986, #94596, #114220 ) ;
#102088 = EDGE_CURVE ( 'NONE', #134621, #58130, #35150, .T. ) ;
#102089 = VECTOR ( 'NONE', #6263, 1000.000000000000000 ) ;
#102090 = CARTESIAN_POINT ( 'NONE',  ( 11.51078643762690490, -27.52281430457047406, 5.000000000000000000 ) ) ;
#102091 = ORIENTED_EDGE ( 'NONE', *, *, #99812, .T. ) ;
#102092 = DIRECTION ( 'NONE',  ( -0.6830127018922180770, -0.6830127018922204085, -0.2588190451025213501 ) ) ;
#102093 = CARTESIAN_POINT ( 'NONE',  ( -0.005480084712502889671, 28.92564299267938210, 4.000000000000000000 ) ) ;
#102094 = CARTESIAN_POINT ( 'NONE',  ( -34.92500000000001137, 17.71849043720405348, 4.759050581649335143 ) ) ;
#102095 = VECTOR ( 'NONE', #42257, 1000.000000000000227 ) ;
#102096 = VECTOR ( 'NONE', #75107, 1000.000000000000227 ) ;
#102097 = VECTOR ( 'NONE', #60658, 999.9999999999998863 ) ;
#102098 = VECTOR ( 'NONE', #52989, 1000.000000000000227 ) ;
#102099 =( BOUNDED_CURVE ( )  B_SPLINE_CURVE ( 3, ( #68206, #134875, #110207, #36252 ),
 .UNSPECIFIED., .F., .T. ) 
 B_SPLINE_CURVE_WITH_KNOTS ( ( 4, 4 ),
 ( 4.712388980384689674, 6.283185307179586232 ),
 .UNSPECIFIED. ) 
 CURVE ( )  GEOMETRIC_REPRESENTATION_ITEM ( )  RATIONAL_B_SPLINE_CURVE ( ( 1.000000000000000000, 0.8047378541243649375, 0.8047378541243649375, 1.000000000000000000 ) ) 
 REPRESENTATION_ITEM ( '' )  );
#102100 = LINE ( 'NONE', #80364, #53706 ) ;
#102101 = ORIENTED_EDGE ( 'NONE', *, *, #87568, .F. ) ;
#102102 = VECTOR ( 'NONE', #70766, 1000.000000000000227 ) ;
#102104 = EDGE_CURVE ( 'NONE', #16103, #113523, #139593, .T. ) ;
#102103 = DIRECTION ( 'NONE',  ( -1.000000000000000000, -1.224606353822377258E-16, -0.000000000000000000 ) ) ;
#102105 =( LENGTH_UNIT ( ) NAMED_UNIT ( * ) SI_UNIT ( .MILLI., .METRE. ) );
#102106 = ORIENTED_EDGE ( 'NONE', *, *, #13788, .T. ) ;
#102107 = CARTESIAN_POINT ( 'NONE',  ( 1.042387978378689573, 4.202752102959690472E-16, 0.000000000000000000 ) ) ;
#102108 = ORIENTED_EDGE ( 'NONE', *, *, #114682, .F. ) ;
#102109 = EDGE_LOOP ( 'NONE', ( #28227, #124859, #81710, #140555 ) ) ;
#102110 = DIRECTION ( 'NONE',  ( -0.7071067811865486830, -0.7071067811865464625, 0.000000000000000000 ) ) ;
#102111 = ORIENTED_EDGE ( 'NONE', *, *, #130697, .T. ) ;
#102112 = EDGE_LOOP ( 'NONE', ( #120566, #83852, #134920, #18779, #4560 ) ) ;
#102113 = VECTOR ( 'NONE', #63008, 1000.000000000000000 ) ;
#102114 = EDGE_CURVE ( 'NONE', #66021, #103933, #122115, .T. ) ;
#102115 = ORIENTED_EDGE ( 'NONE', *, *, #64125, .T. ) ;
#102116 = CARTESIAN_POINT ( 'NONE',  ( 95.06250000000000000, -5.819803920172573086, -5.819803920172573974 ) ) ;
#102117 = LINE ( 'NONE', #126012, #135473 ) ;
#102118 = LINE ( 'NONE', #100688, #11252 ) ;
#102119 = DIRECTION ( 'NONE',  ( 0.000000000000000000, -1.000000000000000000, 0.000000000000000000 ) ) ;
#102120 = CARTESIAN_POINT ( 'NONE',  ( 121.1879301918980900, 6.110000000000002984, -1.637169565754156730 ) ) ;
#102121 = LINE ( 'NONE', #91261, #42590 ) ;
#102122 = AXIS2_PLACEMENT_3D ( 'NONE', #25040, #114200, #3286 ) ;
#102123 = CARTESIAN_POINT ( 'NONE',  ( -33.48921356237309510, -27.52281430457078670, 5.000000000000000000 ) ) ;
#102124 = EDGE_CURVE ( 'NONE', #84513, #81345, #89500, .T. ) ;
#102125 = AXIS2_PLACEMENT_3D ( 'NONE', #15480, #18151, #140670 ) ;
#102126 = DIRECTION ( 'NONE',  ( 0.7071067811865487940, -0.7071067811865463515, 0.000000000000000000 ) ) ;
#102127 = VECTOR ( 'NONE', #131501, 1000.000000000000000 ) ;
#102129 = EDGE_CURVE ( 'NONE', #135680, #39409, #24253, .T. ) ;
#102128 = CARTESIAN_POINT ( 'NONE',  ( 15.83159235450332147, 9.902892378096218942E-16, 0.000000000000000000 ) ) ;
#102130 = ORIENTED_EDGE ( 'NONE', *, *, #31773, .F. ) ;
#102131 = VECTOR ( 'NONE', #117690, 999.9999999999998863 ) ;
#102132 = DIRECTION ( 'NONE',  ( 0.000000000000000000, -1.000000000000000000, 0.000000000000000000 ) ) ;
#102133 = LINE ( 'NONE', #78239, #114726 ) ;
#102134 = ORIENTED_EDGE ( 'NONE', *, *, #34327, .F. ) ;
#102135 = EDGE_CURVE ( 'NONE', #75508, #58706, #79386, .T. ) ;
#102136 = VECTOR ( 'NONE', #55764, 1000.000000000000000 ) ;
#102137 = EDGE_LOOP ( 'NONE', ( #62991, #33462, #43718, #109251, #96713 ) ) ;
#102138 = DIRECTION ( 'NONE',  ( 0.7071067811865487940, 0.7071067811865463515, -0.000000000000000000 ) ) ;
#102139 = VERTEX_POINT ( 'NONE', #24939 ) ;
#102140 = VECTOR ( 'NONE', #106594, 1000.000000000000000 ) ;
#102141 = ADVANCED_FACE ( 'NONE', ( #33723 ), #68499, .F. ) ;
#102142 = FACE_OUTER_BOUND ( 'NONE', #110827, .T. ) ;
#102143 = CARTESIAN_POINT ( 'NONE',  ( -54.18398860626899705, 28.73617430169825226, 5.000000000000000000 ) ) ;
#102144 = CIRCLE ( 'NONE', #139203, 2.500000000000000888 ) ;
#102145 = LINE ( 'NONE', #34742, #26423 ) ;
#102146 = CARTESIAN_POINT ( 'NONE',  ( 0.1839886062690032631, 28.73617430169787568, 5.000000000000000000 ) ) ;
#102147 = EDGE_LOOP ( 'NONE', ( #137976, #41890, #10920, #78050 ) ) ;
#102148 = LINE ( 'NONE', #2804, #53529 ) ;
#102149 = ORIENTED_EDGE ( 'NONE', *, *, #38317, .T. ) ;
#102150 = EDGE_CURVE ( 'NONE', #29906, #114615, #66346, .T. ) ;
#102151 = LINE ( 'NONE', #134061, #127866 ) ;
#102152 = VECTOR ( 'NONE', #95464, 1000.000000000000000 ) ;
#102153 = CARTESIAN_POINT ( 'NONE',  ( 29.08790314143522338, 6.871911579029515771, 3.967499999999989146 ) ) ;
#102154 = ORIENTED_EDGE ( 'NONE', *, *, #119046, .F. ) ;
#102155 = CARTESIAN_POINT ( 'NONE',  ( -13.49999999999989697, -14.94781430457067550, 5.000000000000000000 ) ) ;
#102156 = EDGE_CURVE ( 'NONE', #112560, #117136, #77237, .T. ) ;
#102157 = CARTESIAN_POINT ( 'NONE',  ( 98.37086038379622721, 6.884901960086289741, -3.974999999999993427 ) ) ;
#102158 = VERTEX_POINT ( 'NONE', #48151 ) ;
#102159 = ORIENTED_EDGE ( 'NONE', *, *, #32080, .T. ) ;
#102160 =( GEOMETRIC_REPRESENTATION_CONTEXT ( 3 ) GLOBAL_UNCERTAINTY_ASSIGNED_CONTEXT ( ( #11554 ) ) GLOBAL_UNIT_ASSIGNED_CONTEXT ( ( #123803, #70165, #5542 ) ) REPRESENTATION_CONTEXT ( 'NONE', 'WORKASPACE' ) );
#102161 = ORIENTED_EDGE ( 'NONE', *, *, #88746, .T. ) ;
#102162 = CARTESIAN_POINT ( 'NONE',  ( -12.20000000000000462, -22.33999999999998565, 3.000000000000000000 ) ) ;
#102163 = FACE_OUTER_BOUND ( 'NONE', #54545, .T. ) ;
#102164 = CARTESIAN_POINT ( 'NONE',  ( -23.70822291016937911, -15.74070752338412404, 19.73771281079092077 ) ) ;
#102165 =( GEOMETRIC_REPRESENTATION_CONTEXT ( 3 ) GLOBAL_UNCERTAINTY_ASSIGNED_CONTEXT ( ( #4207 ) ) GLOBAL_UNIT_ASSIGNED_CONTEXT ( ( #53487, #139075, #108531 ) ) REPRESENTATION_CONTEXT ( 'NONE', 'WORKASPACE' ) );
#102166 = CARTESIAN_POINT ( 'NONE',  ( -21.00548008471250938, 28.92564299267923644, 4.000000000000000000 ) ) ;
#102167 = ORIENTED_EDGE ( 'NONE', *, *, #2197, .F. ) ;
#102168 = FACE_OUTER_BOUND ( 'NONE', #57682, .T. ) ;
#102169 = LINE ( 'NONE', #79004, #15584 ) ;
#102170 = CARTESIAN_POINT ( 'NONE',  ( -8.816011393731004731, 28.73617430169781173, 5.000000000000000000 ) ) ;
#102172 = CIRCLE ( 'NONE', #39680, 2.055000000000000604 ) ;
#102171 = DIRECTION ( 'NONE',  ( -0.000000000000000000, -0.3543493200069152693, 0.9351131265310292928 ) ) ;
#102173 = ORIENTED_EDGE ( 'NONE', *, *, #95325, .F. ) ;
#102174 = AXIS2_PLACEMENT_3D ( 'NONE', #50103, #26204, #37063 ) ;
#102175 = CARTESIAN_POINT ( 'NONE',  ( 29.67183060077626067, 8.259292476615637923, 4.000000000000000000 ) ) ;
#102176 = ORIENTED_EDGE ( 'NONE', *, *, #126600, .T. ) ;
#102178 = ADVANCED_FACE ( 'NONE', ( #38697 ), #114791, .F. ) ;
#102177 = ORIENTED_EDGE ( 'NONE', *, *, #84109, .T. ) ;
#102179 = ORIENTED_EDGE ( 'NONE', *, *, #61124, .T. ) ;
#102180 = ADVANCED_FACE ( 'NONE', ( #71334 ), #82229, .F. ) ;
#102181 = CARTESIAN_POINT ( 'NONE',  ( -30.18398860626900060, 28.73617430169808173, 5.000000000000000000 ) ) ;
#102182 = LINE ( 'NONE', #68164, #39104 ) ;
#102184 = ORIENTED_EDGE ( 'NONE', *, *, #69206, .T. ) ;
#102183 = VECTOR ( 'NONE', #32682, 1000.000000000000227 ) ;
#102185 = DIRECTION ( 'NONE',  ( -0.5735764363510501562, 0.8191520442889890230, 1.003171929053521419E-16 ) ) ;
#102186 = ORIENTED_EDGE ( 'NONE', *, *, #14808, .T. ) ;
#102187 = DIRECTION ( 'NONE',  ( -0.000000000000000000, 0.3543493200069152138, -0.9351131265310292928 ) ) ;
#102188 = DIRECTION ( 'NONE',  ( 0.000000000000000000, -1.000000000000000000, 0.000000000000000000 ) ) ;
#102189 = PLANE ( 'NONE',  #124880 ) ;
#102190 = LINE ( 'NONE', #136220, #34675 ) ;
#102191 = FACE_OUTER_BOUND ( 'NONE', #14604, .T. ) ;
#102192 = CARTESIAN_POINT ( 'NONE',  ( -13.49999999999991473, -12.08601207473291161, -10.46905243149091547 ) ) ;
#102193 = CARTESIAN_POINT ( 'NONE',  ( 63.18398860626900415, 28.73617430169831621, 5.000000000000000000 ) ) ;
#102194 = DIRECTION ( 'NONE',  ( -0.7071067811865486830, -0.7071067811865464625, 0.000000000000000000 ) ) ;
#102195 = CARTESIAN_POINT ( 'NONE',  ( 17.04123647476855652, 0.000000000000000000, 7.934999999999990727 ) ) ;
#102196 = CARTESIAN_POINT ( 'NONE',  ( -14.29289321881335795, -3.740707523384239952, 5.000000000000000000 ) ) ;
#102197 = DIRECTION ( 'NONE',  ( 1.000000000000000000, 0.000000000000000000, 0.000000000000000000 ) ) ;
#102198 = CONICAL_SURFACE ( 'NONE', #132330, 2.055000000000001048, 0.9599310885968758145 ) ;
#102199 = LINE ( 'NONE', #36915, #65205 ) ;
#102200 = CARTESIAN_POINT ( 'NONE',  ( 0.000000000000000000, 0.000000000000000000, 5.000000000000000000 ) ) ;
#102201 = ORIENTED_EDGE ( 'NONE', *, *, #14061, .T. ) ;
#102202 = EDGE_CURVE ( 'NONE', #134912, #21649, #138013, .T. ) ;
#102203 = ORIENTED_EDGE ( 'NONE', *, *, #98631, .T. ) ;
#102204 = VECTOR ( 'NONE', #137246, 1000.000000000000000 ) ;
#102205 = CARTESIAN_POINT ( 'NONE',  ( 95.50000000000000000, 0.000000000000000000, -7.950000000000000178 ) ) ;
#102206 = AXIS2_PLACEMENT_3D ( 'NONE', #84450, #64827, #108271 ) ;
#102207 = EDGE_CURVE ( 'NONE', #76282, #53303, #80783, .T. ) ;
#102208 = EDGE_LOOP ( 'NONE', ( #47110, #136382, #141590, #62502 ) ) ;
#102209 = ORIENTED_EDGE ( 'NONE', *, *, #110445, .F. ) ;
#102210 = ORIENTED_EDGE ( 'NONE', *, *, #17744, .T. ) ;
#102211 = DIRECTION ( 'NONE',  ( -0.7071067811865487940, 0.7071067811865463515, 0.000000000000000000 ) ) ;
#102212 = CARTESIAN_POINT ( 'NONE',  ( 11.30840764549667554, 2.500000000000000888, 3.061616997868383141E-16 ) ) ;
#102213 = AXIS2_PLACEMENT_3D ( 'NONE', #20287, #94988, #64526 ) ;
#102214 = CIRCLE ( 'NONE', #30488, 2.500000000000000444 ) ;
#102215 = PRESENTATION_LAYER_ASSIGNMENT (  '', '', ( #69843 ) ) ;
#102216 = VECTOR ( 'NONE', #59301, 1000.000000000000227 ) ;
#102217 = CARTESIAN_POINT ( 'NONE',  ( 12.99859279590333472, 8.843460517209971172, -3.474509921214832708 ) ) ;
#102218 = VERTEX_POINT ( 'NONE', #91645 ) ;
#102219 = LINE ( 'NONE', #94861, #78753 ) ;
#102220 = VECTOR ( 'NONE', #40116, 1000.000000000000000 ) ;
#102221 = LINE ( 'NONE', #58020, #106561 ) ;
#102222 = DIRECTION ( 'NONE',  ( -0.3543493200069162685, -0.000000000000000000, -0.9351131265310288487 ) ) ;
#102223 = CARTESIAN_POINT ( 'NONE',  ( 126.2410695880550833, 6.589327892697261824, -2.966880743088488259 ) ) ;
#102224 = EDGE_CURVE ( 'NONE', #134353, #40105, #36548, .T. ) ;
#102225 = CARTESIAN_POINT ( 'NONE',  ( 127.2245968585647660, -1.637169565754160949, 6.109999999999997655 ) ) ;
#102226 = LINE ( 'NONE', #123271, #130410 ) ;
#102227 = LINE ( 'NONE', #135564, #54319 ) ;
#102228 = VECTOR ( 'NONE', #123476, 1000.000000000000000 ) ;
#102229 = LINE ( 'NONE', #2880, #95353 ) ;
#102230 = LINE ( 'NONE', #113068, #68427 ) ;
#102231 = DIRECTION ( 'NONE',  ( 0.000000000000000000, -1.000000000000000000, 0.000000000000000000 ) ) ;
#102232 = LINE ( 'NONE', #89202, #114823 ) ;
#102233 = FACE_OUTER_BOUND ( 'NONE', #101728, .T. ) ;
#102234 = PLANE ( 'NONE',  #39964 ) ;
#102235 = ORIENTED_EDGE ( 'NONE', *, *, #96319, .T. ) ;
#102236 = ORIENTED_EDGE ( 'NONE', *, *, #179, .F. ) ;
#102237 = CARTESIAN_POINT ( 'NONE',  ( 107.1879301918980900, 6.110000000000002984, -1.637169565754156730 ) ) ;
#102238 = VERTEX_POINT ( 'NONE', #82925 ) ;
#102239 = AXIS2_PLACEMENT_3D ( 'NONE', #79320, #92264, #68434 ) ;
#102240 = CARTESIAN_POINT ( 'NONE',  ( -32.20710678118632586, 12.75929247661558463, 5.000000000000000000 ) ) ;
#102241 = DIRECTION ( 'NONE',  ( 1.000000000000000000, 0.000000000000000000, 0.000000000000000000 ) ) ;
#102242 = CARTESIAN_POINT ( 'NONE',  ( -15.00548008471250228, 28.92564299267927552, 4.000000000000000000 ) ) ;
#102243 = VECTOR ( 'NONE', #92797, 999.9999999999998863 ) ;
#102244 = VECTOR ( 'NONE', #86188, 999.9999999999998863 ) ;
#102245 = CARTESIAN_POINT ( 'NONE',  ( 102.4329301918980946, 1.637169565754156508, 6.110000000000000320 ) ) ;
#102246 = ORIENTED_EDGE ( 'NONE', *, *, #136268, .F. ) ;
#102247 = VECTOR ( 'NONE', #138686, 1000.000000000000000 ) ;
#102248 = EDGE_LOOP ( 'NONE', ( #78888, #57745, #99657, #68369 ) ) ;
#102249 = CARTESIAN_POINT ( 'NONE',  ( -18.48921356237309510, -27.52281430457068367, 5.000000000000000000 ) ) ;
#102250 = EDGE_CURVE ( 'NONE', #22506, #117264, #58361, .T. ) ;
#102251 = VECTOR ( 'NONE', #83291, 1000.000000000000227 ) ;
#102252 = CARTESIAN_POINT ( 'NONE',  ( 12.18398860626900060, 28.73617430169795739, 5.000000000000000000 ) ) ;
#102253 = ORIENTED_EDGE ( 'NONE', *, *, #40625, .T. ) ;
#102254 = EDGE_LOOP ( 'NONE', ( #41685, #123398, #618, #129227, #83625 ) ) ;
#102255 = EDGE_LOOP ( 'NONE', ( #80927, #56346, #30445, #38850, #9298 ) ) ;
#102256 = VECTOR ( 'NONE', #72825, 1000.000000000000000 ) ;
#102257 = CARTESIAN_POINT ( 'NONE',  ( 63.18398860626900415, 28.73617430169831621, 5.000000000000000000 ) ) ;
#102258 = ADVANCED_FACE ( 'NONE', ( #127111 ), #27810, .F. ) ;
#102259 = EDGE_CURVE ( 'NONE', #11839, #99425, #126401, .T. ) ;
#102260 = ADVANCED_FACE ( 'NONE', ( #103914 ), #118652, .T. ) ;
#102261 = CARTESIAN_POINT ( 'NONE',  ( 33.30793019189810877, -6.109999999999998543, 1.637169565754158063 ) ) ;
#102262 = EDGE_CURVE ( 'NONE', #119015, #53073, #93786, .T. ) ;
#102263 = ORIENTED_EDGE ( 'NONE', *, *, #2270, .T. ) ;
#102264 = ORIENTED_EDGE ( 'NONE', *, *, #68622, .T. ) ;
#102266 = EDGE_CURVE ( 'NONE', #129488, #61952, #14066, .T. ) ;
#102265 = CARTESIAN_POINT ( 'NONE',  ( 15.05159235450332034, 9.902892378096218942E-16, 0.000000000000000000 ) ) ;
#102267 = ORIENTED_EDGE ( 'NONE', *, *, #6788, .F. ) ;
#102268 = VERTEX_POINT ( 'NONE', #69939 ) ;
#102269 = VECTOR ( 'NONE', #123989, 1000.000000000000000 ) ;
#102270 = VERTEX_POINT ( 'NONE', #4562 ) ;
#102271 = AXIS2_PLACEMENT_3D ( 'NONE', #87898, #66170, #110339 ) ;
#102272 = EDGE_CURVE ( 'NONE', #128989, #14082, #48869, .T. ) ;
#102273 = LINE ( 'NONE', #102972, #63344 ) ;
#102274 = EDGE_CURVE ( 'NONE', #60720, #104026, #125720, .T. ) ;
#102275 = SURFACE_STYLE_FILL_AREA ( #110947 ) ;
#102276 = CARTESIAN_POINT ( 'NONE',  ( -19.93618820137057668, -6.270000000050818478, -40.00000000000000000 ) ) ;
#102277 = EDGE_LOOP ( 'NONE', ( #43194, #102293, #109508, #44983 ) ) ;
#102278 = CARTESIAN_POINT ( 'NONE',  ( 25.82816939922335209, 15.75929247661555976, 4.000000000000000000 ) ) ;
#102279 = AXIS2_PLACEMENT_3D ( 'NONE', #117233, #62916, #140439 ) ;
#102280 = VECTOR ( 'NONE', #69915, 1000.000000000000000 ) ;
#102281 = CARTESIAN_POINT ( 'NONE',  ( 17.67183060077634593, -3.740707523384244837, 4.000000000000000000 ) ) ;
#102282 = PLANE ( 'NONE',  #37450 ) ;
#102283 = EDGE_CURVE ( 'NONE', #92108, #91730, #5324, .T. ) ;
#102284 = FACE_BOUND ( 'NONE', #140354, .T. ) ;
#102285 = ORIENTED_EDGE ( 'NONE', *, *, #80475, .T. ) ;
#102286 = ADVANCED_FACE ( 'NONE', ( #16942 ), #38001, .F. ) ;
#102287 = CARTESIAN_POINT ( 'NONE',  ( 62.78752705046289151, 0.000000000000000000, -7.949999999999998401 ) ) ;
#102288 = DIRECTION ( 'NONE',  ( 0.7071067811865487940, 0.7071067811865463515, -0.000000000000000000 ) ) ;
#102289 = CARTESIAN_POINT ( 'NONE',  ( 0.2569208697893812232, 2.055000000000001048, 0.000000000000000000 ) ) ;
#102290 = ORIENTED_EDGE ( 'NONE', *, *, #48223, .F. ) ;
#102291 = CARTESIAN_POINT ( 'NONE',  ( -34.47516574401891631, -16.50948238788421918, 4.998110765256836174 ) ) ;
#102292 = VERTEX_POINT ( 'NONE', #59066 ) ;
#102293 = ORIENTED_EDGE ( 'NONE', *, *, #93252, .T. ) ;
#102294 = AXIS2_PLACEMENT_3D ( 'NONE', #103260, #16224, #70684 ) ;
#102296 = EDGE_CURVE ( 'NONE', #2768, #55124, #49604, .T. ) ;
#102295 =( BOUNDED_CURVE ( )  B_SPLINE_CURVE ( 3, ( #126454, #105416, #49662, #72139 ),
 .UNSPECIFIED., .F., .T. ) 
 B_SPLINE_CURVE_WITH_KNOTS ( ( 4, 4 ),
 ( 5.106027341939292086, 6.645403452391244414 ),
 .UNSPECIFIED. ) 
 CURVE ( )  GEOMETRIC_REPRESENTATION_ITEM ( )  RATIONAL_B_SPLINE_CURVE ( ( 1.000000000000000000, 0.8120851936182307274, 0.8120851936182307274, 1.000000000000000000 ) ) 
 REPRESENTATION_ITEM ( '' )  );
#102297 = ORIENTED_EDGE ( 'NONE', *, *, #59876, .T. ) ;
#102298 = CARTESIAN_POINT ( 'NONE',  ( 42.20376352523144448, 6.109999999999998543, 1.122388791418548911E-15 ) ) ;
#102299 = ORIENTED_EDGE ( 'NONE', *, *, #142873, .F. ) ;
#102300 = DIRECTION ( 'NONE',  ( -0.6830127018922181881, 0.6830127018922202975, -0.2588190451025214056 ) ) ;
#102301 = CARTESIAN_POINT ( 'NONE',  ( -5.999999999999956479, -0.8619312979532001151, -5.102805207349841332 ) ) ;
#102302 = ORIENTED_EDGE ( 'NONE', *, *, #11518, .T. ) ;
#102303 = DIRECTION ( 'NONE',  ( 1.000000000000000000, 0.000000000000000000, 0.000000000000000000 ) ) ;
#102304 = AXIS2_PLACEMENT_3D ( 'NONE', #3868, #49600, #59750 ) ;
#102305 = VECTOR ( 'NONE', #132099, 1000.000000000000000 ) ;
#102306 = CARTESIAN_POINT ( 'NONE',  ( -9.299744871391588674, -27.71228299555212971, 4.000000000000000000 ) ) ;
#102307 = VECTOR ( 'NONE', #140443, 1000.000000000000000 ) ;
#102308 = VECTOR ( 'NONE', #52327, 999.9999999999998863 ) ;
#102309 = DIRECTION ( 'NONE',  ( -1.000000000000000000, -1.224606353822377258E-16, -0.000000000000000000 ) ) ;
#102310 = DIRECTION ( 'NONE',  ( -0.7071067811865487940, 0.7071067811865463515, -0.000000000000000000 ) ) ;
#102311 = DIRECTION ( 'NONE',  ( 0.000000000000000000, -1.000000000000000000, 0.000000000000000000 ) ) ;
#102312 = VERTEX_POINT ( 'NONE', #37270 ) ;
#102313 = EDGE_CURVE ( 'NONE', #130580, #83276, #129248, .T. ) ;
#102314 = VERTEX_POINT ( 'NONE', #98072 ) ;
#102315 = VECTOR ( 'NONE', #59787, 1000.000000000000227 ) ;
#102316 = ORIENTED_EDGE ( 'NONE', *, *, #30820, .F. ) ;
#102317 = VECTOR ( 'NONE', #519, 999.9999999999998863 ) ;
#102318 = ORIENTED_EDGE ( 'NONE', *, *, #16872, .F. ) ;
#102319 = AXIS2_PLACEMENT_3D ( 'NONE', #59819, #38767, #4637 ) ;
#102320 = CARTESIAN_POINT ( 'NONE',  ( 25.82816939922335209, 3.759292476615676559, 4.000000000000000000 ) ) ;
#102321 = VERTEX_POINT ( 'NONE', #141581 ) ;
#102322 = ORIENTED_EDGE ( 'NONE', *, *, #110741, .F. ) ;
#102323 = DIRECTION ( 'NONE',  ( -0.3543493200069163240, -0.000000000000000000, -0.9351131265310288487 ) ) ;
#102324 = DIRECTION ( 'NONE',  ( -0.7071067811865487940, 0.7071067811865463515, -0.000000000000000000 ) ) ;
#102325 = VERTEX_POINT ( 'NONE', #116958 ) ;
#102326 = DIRECTION ( 'NONE',  ( 3.166071393695993333E-32, -1.016133275908817741E-16, 1.000000000000000000 ) ) ;
#102327 = ORIENTED_EDGE ( 'NONE', *, *, #112583, .F. ) ;
#102328 = ADVANCED_FACE ( 'NONE', ( #142307 ), #95920, .F. ) ;
#102329 = DIRECTION ( 'NONE',  ( 0.6830127018922180770, -0.6830127018922204085, -0.2588190451025214056 ) ) ;
#102330 = CARTESIAN_POINT ( 'NONE',  ( 28.35873647476855197, 5.808823158059031044, -5.808823158059038150 ) ) ;
#102331 = CARTESIAN_POINT ( 'NONE',  ( 4.442069808101886785, 7.934999999999993392, 2.126176841940951689 ) ) ;
#102332 = ORIENTED_EDGE ( 'NONE', *, *, #45209, .T. ) ;
#102334 = CARTESIAN_POINT ( 'NONE',  ( 11.68342038867203492, -6.740707523384209310, 11.88629033278121661 ) ) ;
#102333 = CARTESIAN_POINT ( 'NONE',  ( 108.7037635252314516, 6.109999999999999432, 1.122388791418549108E-15 ) ) ;
#102336 = EDGE_CURVE ( 'NONE', #92516, #75802, #119096, .T. ) ;
#102335 = CARTESIAN_POINT ( 'NONE',  ( 3.000000000000000000, 0.9892420537897055333, 14.41609864557725729 ) ) ;
#102337 = FILL_AREA_STYLE ('',( #58139 ) ) ;
#102338 = VERTEX_POINT ( 'NONE', #74179 ) ;
#102340 = VERTEX_POINT ( 'NONE', #64725 ) ;
#102339 = FACE_OUTER_BOUND ( 'NONE', #105618, .T. ) ;
#102341 = CARTESIAN_POINT ( 'NONE',  ( -7.499999999999940492, 7.466399257802177836, 5.000000000000000000 ) ) ;
#102342 = DIRECTION ( 'NONE',  ( 0.3543493200069162685, -0.000000000000000000, -0.9351131265310288487 ) ) ;
#102343 = FILL_AREA_STYLE ('',( #5102 ) ) ;
#102344 = PLANE ( 'NONE',  #42390 ) ;
#102345 = CARTESIAN_POINT ( 'NONE',  ( -21.48921356237309155, -27.52281430457070499, 5.000000000000000000 ) ) ;
#102346 = ORIENTED_EDGE ( 'NONE', *, *, #106568, .F. ) ;
#102347 = AXIS2_PLACEMENT_3D ( 'NONE', #100672, #34702, #46323 ) ;
#102348 = CARTESIAN_POINT ( 'NONE',  ( -14.99999999999988809, 20.96639925780204905, 5.000000000000000000 ) ) ;
#102349 = VECTOR ( 'NONE', #112061, 1000.000000000000227 ) ;
#102350 = EDGE_CURVE ( 'NONE', #106377, #78830, #7462, .T. ) ;
#102351 = VECTOR ( 'NONE', #36855, 1000.000000000000000 ) ;
#102352 = DIRECTION ( 'NONE',  ( -0.7071067811865486830, -0.7071067811865464625, -0.000000000000000000 ) ) ;
#102353 = CARTESIAN_POINT ( 'NONE',  ( -12.18398860626900060, 28.73617430169795739, 5.000000000000000000 ) ) ;
#102354 = EDGE_LOOP ( 'NONE', ( #86759, #103657, #13159 ) ) ;
#102355 = PLANE ( 'NONE',  #132307 ) ;
#102356 = VECTOR ( 'NONE', #66200, 1000.000000000000114 ) ;
#102357 = DIRECTION ( 'NONE',  ( -0.7071067811865486830, -0.7071067811865464625, -0.000000000000000000 ) ) ;
#102358 = ORIENTED_EDGE ( 'NONE', *, *, #112441, .F. ) ;
#102361 = EDGE_CURVE ( 'NONE', #98488, #113103, #61896, .T. ) ;
#102360 = ORIENTED_EDGE ( 'NONE', *, *, #32505, .T. ) ;
#102359 = CARTESIAN_POINT ( 'NONE',  ( -81.18398860626899705, 28.73617430169844056, 5.000000000000000000 ) ) ;
#102362 = VERTEX_POINT ( 'NONE', #19072 ) ;
#102363 = DIRECTION ( 'NONE',  ( -2.781805975412905890E-17, 0.3543493200069152693, 0.9351131265310292928 ) ) ;
#102364 = VECTOR ( 'NONE', #45260, 1000.000000000000000 ) ;
#102365 = EDGE_LOOP ( 'NONE', ( #38598, #50411, #91947, #137558 ) ) ;
#102366 = CARTESIAN_POINT ( 'NONE',  ( 53.49999999999999289, 0.000000000000000000, -7.950000000000000178 ) ) ;
#102367 = SURFACE_SIDE_STYLE ('',( #90023 ) ) ;
#102368 = ORIENTED_EDGE ( 'NONE', *, *, #94737, .F. ) ;
#102369 = DIRECTION ( 'NONE',  ( -0.7071067811865487940, 0.7071067811865463515, -0.000000000000000000 ) ) ;
#102370 = DIRECTION ( 'NONE',  ( 0.6830127018922180770, -0.6830127018922204085, -0.2588190451025213501 ) ) ;
#102371 = VECTOR ( 'NONE', #62852, 1000.000000000000000 ) ;
#102372 = CARTESIAN_POINT ( 'NONE',  ( 31.00193056682077142, -22.22500000000000142, 4.500000000000000888 ) ) ;
#102373 = CARTESIAN_POINT ( 'NONE',  ( -63.18398860626900415, 28.73617430169831621, 5.000000000000000000 ) ) ;
#102374 = AXIS2_PLACEMENT_3D ( 'NONE', #13706, #11560, #12301 ) ;
#102375 = LINE ( 'NONE', #58907, #2007 ) ;
#102376 = CARTESIAN_POINT ( 'NONE',  ( -2.671830600776452069, 20.25929247661551713, 4.000000000000000000 ) ) ;
#102377 = EDGE_CURVE ( 'NONE', #49015, #29472, #63337, .T. ) ;
#102378 = DIRECTION ( 'NONE',  ( -0.7071067811865487940, 0.7071067811865463515, -0.000000000000000000 ) ) ;
#102379 = ORIENTED_EDGE ( 'NONE', *, *, #110139, .T. ) ;
#102380 = ORIENTED_EDGE ( 'NONE', *, *, #54500, .T. ) ;
#102381 = ORIENTED_EDGE ( 'NONE', *, *, #112541, .T. ) ;
#102382 = CARTESIAN_POINT ( 'NONE',  ( 122.0416666666666714, -3.975000000000002753, 6.884901960086286188 ) ) ;
#102383 = EDGE_CURVE ( 'NONE', #34231, #80772, #51725, .T. ) ;
#102384 = EDGE_LOOP ( 'NONE', ( #34868, #115626, #124460, #97909 ) ) ;
#102385 = ORIENTED_EDGE ( 'NONE', *, *, #44867, .F. ) ;
#102386 = VERTEX_POINT ( 'NONE', #40158 ) ;
#102387 = VECTOR ( 'NONE', #36197, 1000.000000000000000 ) ;
#102388 = CARTESIAN_POINT ( 'NONE',  ( 23.99451991528749062, 28.92564299267954908, 4.000000000000000000 ) ) ;
#102389 = CARTESIAN_POINT ( 'NONE',  ( -32.99999999999976552, -19.22509904557639615, 1.855685503482101595 ) ) ;
#102390 = ORIENTED_EDGE ( 'NONE', *, *, #101241, .F. ) ;
#102391 = FACE_OUTER_BOUND ( 'NONE', #129817, .T. ) ;
#102392 = LINE ( 'NONE', #69044, #97619 ) ;
#102393 = DIRECTION ( 'NONE',  ( -1.000000000000000000, -0.000000000000000000, -0.000000000000000000 ) ) ;
#102394 = DIRECTION ( 'NONE',  ( 0.7071067811865487940, 0.7071067811865463515, 0.000000000000000000 ) ) ;
#102395 = CARTESIAN_POINT ( 'NONE',  ( 116.5212635252314328, -4.472830434245839371, -4.472830434245840259 ) ) ;
#102396 = EDGE_LOOP ( 'NONE', ( #117551, #37928, #21549, #75189, #137399 ) ) ;
#102397 = EDGE_CURVE ( 'NONE', #91589, #100881, #129986, .T. ) ;
#102398 = DIRECTION ( 'NONE',  ( -0.3543493200069162685, -0.000000000000000000, -0.9351131265310288487 ) ) ;
#102399 = CARTESIAN_POINT ( 'NONE',  ( -66.18398860626901126, 28.73617430169833753, 5.000000000000000000 ) ) ;
#102401 = VECTOR ( 'NONE', #44253, 1000.000000000000000 ) ;
#102400 = DIRECTION ( 'NONE',  ( 0.7071067811865487940, 0.7071067811865463515, 0.000000000000000000 ) ) ;
#102402 = CARTESIAN_POINT ( 'NONE',  ( -26.99451991528749417, 28.92564299267956685, 4.000000000000000000 ) ) ;
#102403 = DIRECTION ( 'NONE',  ( -0.7071067811865487940, 0.7071067811865463515, -0.000000000000000000 ) ) ;
#102404 = DIRECTION ( 'NONE',  ( -0.000000000000000000, 0.000000000000000000, 1.000000000000000000 ) ) ;
#102405 = PLANE ( 'NONE',  #31938 ) ;
#102406 = PRODUCT_RELATED_PRODUCT_CATEGORY ( 'part', '', ( #110337 ) ) ;
#102407 = CARTESIAN_POINT ( 'NONE',  ( 43.24586038379622721, 3.974999999999996980, 6.884901960086287964 ) ) ;
#102408 = CARTESIAN_POINT ( 'NONE',  ( -56.99451991528749062, 28.92564299267978001, 4.000000000000000000 ) ) ;
#102409 = DIRECTION ( 'NONE',  ( -0.3543493200069162685, -0.000000000000000000, -0.9351131265310288487 ) ) ;
#102410 = ORIENTED_EDGE ( 'NONE', *, *, #31343, .F. ) ;
#102411 = EDGE_LOOP ( 'NONE', ( #103807, #103903, #49915, #67373 ) ) ;
#102412 = CARTESIAN_POINT ( 'NONE',  ( 38.04166666666665719, -3.975000000000002753, 6.884901960086286188 ) ) ;
#102413 = ORIENTED_EDGE ( 'NONE', *, *, #54675, .T. ) ;
#102414 = ORIENTED_EDGE ( 'NONE', *, *, #52725, .T. ) ;
#102415 = CARTESIAN_POINT ( 'NONE',  ( -34.92500000000001137, 7.711264365774168184, -0.4997969837368162471 ) ) ;
#102416 = CARTESIAN_POINT ( 'NONE',  ( 45.48921356237309510, -27.52281430457087197, 5.000000000000000000 ) ) ;
#102417 = VERTEX_POINT ( 'NONE', #117638 ) ;
#102418 = VECTOR ( 'NONE', #70985, 999.9999999999998863 ) ;
#102419 = AXIS2_PLACEMENT_3D ( 'NONE', #11902, #109076, #77903 ) ;
#102420 = VECTOR ( 'NONE', #122364, 1000.000000000000000 ) ;
#102421 = CARTESIAN_POINT ( 'NONE',  ( 1.499999999999990896, -19.53360074219753884, 5.000000000000000000 ) ) ;
#102422 = CARTESIAN_POINT ( 'NONE',  ( -14.24139925780194105, 21.72500000000000142, 5.000000000000000000 ) ) ;
#102423 = VECTOR ( 'NONE', #6154, 1000.000000000000000 ) ;
#102424 = COLOUR_RGB ( '', 0.08235294, 0.09019608, 0.10196078) ;
#102425 = CARTESIAN_POINT ( 'NONE',  ( 33.68793019189809712, 6.110000000000002984, -1.637169565754156730 ) ) ;
#102426 = ORIENTED_EDGE ( 'NONE', *, *, #53610, .F. ) ;
#102427 = LINE ( 'NONE', #2332, #50297 ) ;
#102428 = ORIENTED_EDGE ( 'NONE', *, *, #61199, .F. ) ;
#102429 =( GEOMETRIC_REPRESENTATION_CONTEXT ( 3 ) GLOBAL_UNCERTAINTY_ASSIGNED_CONTEXT ( ( #88281 ) ) GLOBAL_UNIT_ASSIGNED_CONTEXT ( ( #66192, #56049, #43010 ) ) REPRESENTATION_CONTEXT ( 'NONE', 'WORKASPACE' ) );
#102430 = DIRECTION ( 'NONE',  ( -0.000000000000000000, -0.3543493200069152138, 0.9351131265310292928 ) ) ;
#102431 = LINE ( 'NONE', #3079, #70895 ) ;
#102432 = FILL_AREA_STYLE ('',( #48045 ) ) ;
#102433 = DIRECTION ( 'NONE',  ( 0.7071067811865487940, -0.7071067811865463515, 0.000000000000000000 ) ) ;
#102434 = ORIENTED_EDGE ( 'NONE', *, *, #107169, .F. ) ;
#102435 = ORIENTED_EDGE ( 'NONE', *, *, #131399, .T. ) ;
#102436 = CARTESIAN_POINT ( 'NONE',  ( 38.28752705046288440, 0.000000000000000000, -7.949999999999998401 ) ) ;
#102437 = DIRECTION ( 'NONE',  ( 0.7071067811865486830, -0.7071067811865464625, -0.000000000000000000 ) ) ;
#102438 = CARTESIAN_POINT ( 'NONE',  ( -29.29289321881324426, -3.740707523384243505, 5.000000000000000000 ) ) ;
#102439 = CARTESIAN_POINT ( 'NONE',  ( -42.18398860626899705, 28.73617430169816700, 5.000000000000000000 ) ) ;
#102440 = LINE ( 'NONE', #135762, #127223 ) ;
#102441 = EDGE_CURVE ( 'NONE', #125750, #114249, #108188, .T. ) ;
#102442 = CARTESIAN_POINT ( 'NONE',  ( 55.03709685856478018, -3.054999999999998828, -5.291415217122919401 ) ) ;
#102443 = EDGE_CURVE ( 'NONE', #105448, #75123, #85044, .T. ) ;
#102444 = CARTESIAN_POINT ( 'NONE',  ( 1.199999999999999956, 0.5999999999999987566, 4.749999999999999112 ) ) ;
#102446 = ADVANCED_FACE ( 'NONE', ( #29232 ), #42280, .T. ) ;
#102445 = CYLINDRICAL_SURFACE ( 'NONE', #50080, 0.5000000000000004441 ) ;
#102447 = ORIENTED_EDGE ( 'NONE', *, *, #141914, .T. ) ;
#102448 = VERTEX_POINT ( 'NONE', #8848 ) ;
#102449 = FACE_OUTER_BOUND ( 'NONE', #76043, .T. ) ;
#102450 = ORIENTED_EDGE ( 'NONE', *, *, #44544, .F. ) ;
#102451 = EDGE_CURVE ( 'NONE', #137006, #71833, #14868, .T. ) ;
#102452 = CONICAL_SURFACE ( 'NONE', #577, 2.055000000000001048, 0.9599310885968758145 ) ;
#102453 = CARTESIAN_POINT ( 'NONE',  ( 32.09873525369289382, 22.27000000000000668, -14.71147562388300045 ) ) ;
#102454 = ORIENTED_EDGE ( 'NONE', *, *, #1767, .T. ) ;
#102455 = AXIS2_PLACEMENT_3D ( 'NONE', #70782, #38143, #79546 ) ;
#102456 = CYLINDRICAL_SURFACE ( 'NONE', #21471, 0.5000000000000004441 ) ;
#102457 = AXIS2_PLACEMENT_3D ( 'NONE', #81193, #92742, #68895 ) ;
#102458 = CARTESIAN_POINT ( 'NONE',  ( -34.42500000000001137, 22.22500000000000142, 4.165035510187088619 ) ) ;
#102459 = EDGE_CURVE ( 'NONE', #28383, #36162, #75611, .T. ) ;
#102460 = FACE_BOUND ( 'NONE', #75318, .T. ) ;
#102461 = ADVANCED_FACE ( 'NONE', ( #9598 ), #34245, .F. ) ;
#102462 = DIRECTION ( 'NONE',  ( -0.7071067811865487940, 0.7071067811865463515, -0.000000000000000000 ) ) ;
#102463 = DIRECTION ( 'NONE',  ( 0.000000000000000000, 1.000000000000000000, 0.000000000000000000 ) ) ;
#102464 = CARTESIAN_POINT ( 'NONE',  ( 25.82816939922335564, 0.7592924766157207461, 4.000000000000000000 ) ) ;
#102466 = ORIENTED_EDGE ( 'NONE', *, *, #6083, .F. ) ;
#102465 = CARTESIAN_POINT ( 'NONE',  ( -20.99999999999984723, -19.06887692260762179, 4.000000000000000000 ) ) ;
#102467 = CARTESIAN_POINT ( 'NONE',  ( 23.29289321881329755, -6.740707523384216415, 5.000000000000000000 ) ) ;
#102468 = EDGE_CURVE ( 'NONE', #84739, #20850, #77057, .T. ) ;
#102469 = ORIENTED_EDGE ( 'NONE', *, *, #140396, .F. ) ;
#102470 = ORIENTED_EDGE ( 'NONE', *, *, #32806, .F. ) ;
#102471 = CARTESIAN_POINT ( 'NONE',  ( 62.91209685856477307, 5.291415217122921177, -3.054999999999994831 ) ) ;
#102472 = ORIENTED_EDGE ( 'NONE', *, *, #121237, .T. ) ;
#102473 = DIRECTION ( 'NONE',  ( -0.6830127018922181881, 0.6830127018922202975, -0.2588190451025214056 ) ) ;
#102474 = ORIENTED_EDGE ( 'NONE', *, *, #47864, .F. ) ;
#102475 = LINE ( 'NONE', #14728, #11984 ) ;
#102476 = EDGE_CURVE ( 'NONE', #78949, #27927, #111048, .T. ) ;
#102477 = AXIS2_PLACEMENT_3D ( 'NONE', #28750, #117145, #17826 ) ;
#102478 = CARTESIAN_POINT ( 'NONE',  ( 30.78162688292473348, 21.74787736706807095, 4.999607392498048419 ) ) ;
#102479 = DIRECTION ( 'NONE',  ( -0.7071067811865487940, 0.7071067811865463515, -0.000000000000000000 ) ) ;
#102480 = DIRECTION ( 'NONE',  ( 1.000000000000000000, 0.000000000000000000, 0.000000000000000000 ) ) ;
#102482 = CARTESIAN_POINT ( 'NONE',  ( -10.49999999999992184, -10.53360074219763121, 5.000000000000000000 ) ) ;
#102481 = LINE ( 'NONE', #36489, #64341 ) ;
#102483 = CARTESIAN_POINT ( 'NONE',  ( -14.81601139373099585, 28.73617430169776910, 5.000000000000000000 ) ) ;
#102484 = DIRECTION ( 'NONE',  ( 0.7071067811865487940, -0.7071067811865463515, 0.000000000000000000 ) ) ;
#102485 = ORIENTED_EDGE ( 'NONE', *, *, #72582, .T. ) ;
#102486 = EDGE_CURVE ( 'NONE', #118739, #97187, #12469, .T. ) ;
#102487 = VECTOR ( 'NONE', #7153, 1000.000000000000227 ) ;
#102488 = VERTEX_POINT ( 'NONE', #112510 ) ;
#102489 = CARTESIAN_POINT ( 'NONE',  ( 0.4000000000000001887, 0.000000000000000000, 0.000000000000000000 ) ) ;
#102490 = LINE ( 'NONE', #47428, #39700 ) ;
#102491 = ORIENTED_EDGE ( 'NONE', *, *, #40880, .F. ) ;
#102492 = ORIENTED_EDGE ( 'NONE', *, *, #20708, .T. ) ;
#102493 = ORIENTED_EDGE ( 'NONE', *, *, #38930, .F. ) ;
#102494 = LINE ( 'NONE', #5971, #67021 ) ;
#102495 = CIRCLE ( 'NONE', #114057, 2.500000000000000444 ) ;
#102496 = ORIENTED_EDGE ( 'NONE', *, *, #52460, .F. ) ;
#102497 = DIRECTION ( 'NONE',  ( -1.000000000000000000, -0.000000000000000000, -0.000000000000000000 ) ) ;
#102498 = EDGE_CURVE ( 'NONE', #44877, #26527, #81851, .T. ) ;
#102499 = LINE ( 'NONE', #68459, #14534 ) ;
#102500 = CARTESIAN_POINT ( 'NONE',  ( 1.379569808101885897, 3.967499999999998916, 6.871911579029510442 ) ) ;
#102501 = DIRECTION ( 'NONE',  ( -0.7071067811865486830, -0.7071067811865464625, 0.000000000000000000 ) ) ;
#102502 = VERTEX_POINT ( 'NONE', #133562 ) ;
#102503 = DIRECTION ( 'NONE',  ( -0.000000000000000000, -1.000000000000000000, -0.000000000000000000 ) ) ;
#102504 = CARTESIAN_POINT ( 'NONE',  ( 33.15612307739218778, -22.22500000000000142, 4.000000000000000000 ) ) ;
#102505 = LINE ( 'NONE', #133695, #142400 ) ;
#102506 = VECTOR ( 'NONE', #29918, 1000.000000000000227 ) ;
#102508 = ORIENTED_EDGE ( 'NONE', *, *, #61456, .T. ) ;
#102507 = LINE ( 'NONE', #111194, #30934 ) ;
#102509 = AXIS2_PLACEMENT_3D ( 'NONE', #34678, #78912, #57170 ) ;
#102510 = ORIENTED_EDGE ( 'NONE', *, *, #85776, .F. ) ;
#102511 = DIRECTION ( 'NONE',  ( 0.000000000000000000, 1.000000000000000000, 0.000000000000000000 ) ) ;
#102512 = CARTESIAN_POINT ( 'NONE',  ( 26.40000000000000568, -18.48000000000005372, 34.92499999999998295 ) ) ;
#102513 = VECTOR ( 'NONE', #29730, 1000.000000000000000 ) ;
#102514 = FACE_OUTER_BOUND ( 'NONE', #88228, .T. ) ;
#102516 = ORIENTED_EDGE ( 'NONE', *, *, #140086, .T. ) ;
#102515 = VECTOR ( 'NONE', #32214, 999.9999999999998863 ) ;
#102517 = DIRECTION ( 'NONE',  ( -0.7071067811865487940, 0.7071067811865463515, 0.000000000000000000 ) ) ;
#102518 = EDGE_CURVE ( 'NONE', #53303, #79366, #133, .T. ) ;
#102519 = DIRECTION ( 'NONE',  ( 0.5735764363510444941, 0.8191520442889929088, 0.000000000000000000 ) ) ;
#102520 = CARTESIAN_POINT ( 'NONE',  ( 0.6664792200040612347, -22.22500000000000142, 18.48694195581934352 ) ) ;
#102521 = FACE_OUTER_BOUND ( 'NONE', #24306, .T. ) ;
#102522 = VECTOR ( 'NONE', #1253, 1000.000000000000000 ) ;
#102523 = ORIENTED_EDGE ( 'NONE', *, *, #59737, .T. ) ;
#102524 = COLOUR_RGB ( '', 0.72549020, 0.75294118, 0.79215686) ;
#102525 = DIRECTION ( 'NONE',  ( -1.000000000000000000, -1.224606353822377258E-16, -0.000000000000000000 ) ) ;
#102526 = DIRECTION ( 'NONE',  ( -0.7071067811865487940, 0.7071067811865463515, 0.000000000000000000 ) ) ;
#102527 = CARTESIAN_POINT ( 'NONE',  ( 6.462472949537106715, -7.464222240803106570E-16, -6.094999999999989981 ) ) ;
#102528 = DIRECTION ( 'NONE',  ( 0.7071067811865486830, -0.7071067811865464625, -0.000000000000000000 ) ) ;
#102529 = CARTESIAN_POINT ( 'NONE',  ( -22.49999999999983658, 13.46639925780212721, 5.000000000000000000 ) ) ;
#102531 = EDGE_CURVE ( 'NONE', #76190, #66627, #57441, .T. ) ;
#102530 = ORIENTED_EDGE ( 'NONE', *, *, #45534, .F. ) ;
#102532 = ORIENTED_EDGE ( 'NONE', *, *, #101129, .F. ) ;
#102533 = PLANE ( 'NONE',  #17792 ) ;
#102534 = DIRECTION ( 'NONE',  ( 0.7071067811865486830, -0.7071067811865464625, -0.000000000000000000 ) ) ;
#102535 = DIRECTION ( 'NONE',  ( 1.000000000000000000, 0.000000000000000000, 0.000000000000000000 ) ) ;
#102536 = CARTESIAN_POINT ( 'NONE',  ( 65.12086038379621300, -6.884901960086286188, 3.974999999999997424 ) ) ;
#102537 = VECTOR ( 'NONE', #29400, 1000.000000000000227 ) ;
#102538 = PLANE ( 'NONE',  #43842 ) ;
#102539 = CARTESIAN_POINT ( 'NONE',  ( -32.99999999999976552, -4.447814304570784749, 5.000000000000000000 ) ) ;
#102540 = CARTESIAN_POINT ( 'NONE',  ( -29.29289321881324781, -12.74070752338415780, 5.000000000000000000 ) ) ;
#102541 = EDGE_LOOP ( 'NONE', ( #131431, #7994, #76915, #34552, #82441 ) ) ;
#102542 = CARTESIAN_POINT ( 'NONE',  ( -9.707106781186471522, 5.259292476615662792, 5.000000000000000000 ) ) ;
#102543 = DIRECTION ( 'NONE',  ( 0.3543493200069162685, -0.000000000000000000, -0.9351131265310288487 ) ) ;
#102544 = DIRECTION ( 'NONE',  ( -0.7071067811865486830, -0.7071067811865464625, 0.000000000000000000 ) ) ;
#102545 = CARTESIAN_POINT ( 'NONE',  ( 57.66209685856478728, -5.291415217122919401, 3.054999999999998384 ) ) ;
#102546 = VECTOR ( 'NONE', #14390, 1000.000000000000227 ) ;
#102547 = CARTESIAN_POINT ( 'NONE',  ( 184.1500000000000057, -49.85820393249935023, -34.92499999999998295 ) ) ;
#102548 = PLANE ( 'NONE',  #44208 ) ;
#102549 = EDGE_CURVE ( 'NONE', #41843, #56470, #76324, .T. ) ;
#102550 = AXIS2_PLACEMENT_3D ( 'NONE', #123577, #80075, #68479 ) ;
#102551 = ORIENTED_EDGE ( 'NONE', *, *, #143300, .F. ) ;
#102552 = DIRECTION ( 'NONE',  ( 0.7071067811865487940, 0.7071067811865463515, 0.000000000000000000 ) ) ;
#102553 = ORIENTED_EDGE ( 'NONE', *, *, #55818, .T. ) ;
#102554 = DIRECTION ( 'NONE',  ( -0.7071067811865487940, 0.7071067811865463515, -0.000000000000000000 ) ) ;
#102555 = STYLED_ITEM ( 'NONE', ( #91863 ), #62426 ) ;
#102556 = DIRECTION ( 'NONE',  ( -0.7071067811865486830, -0.7071067811865464625, 0.000000000000000000 ) ) ;
#102557 = FACE_OUTER_BOUND ( 'NONE', #53066, .T. ) ;
#102558 = DIRECTION ( 'NONE',  ( -0.7071067811865486830, -0.7071067811865464625, 0.000000000000000000 ) ) ;
#102559 = ADVANCED_FACE ( 'NONE', ( #1567 ), #77756, .F. ) ;
#102560 = DIRECTION ( 'NONE',  ( 0.000000000000000000, -1.000000000000000000, 0.000000000000000000 ) ) ;
#102561 = DIRECTION ( 'NONE',  ( 0.3543493200069162685, -0.000000000000000000, -0.9351131265310288487 ) ) ;
#102562 = ORIENTED_EDGE ( 'NONE', *, *, #117813, .F. ) ;
#102563 = EDGE_CURVE ( 'NONE', #43110, #9868, #54008, .T. ) ;
#102564 = EDGE_LOOP ( 'NONE', ( #23967, #57344, #119477, #23472 ) ) ;
#102565 = CARTESIAN_POINT ( 'NONE',  ( -6.489213562373093325, -27.52281430457059841, 5.000000000000000000 ) ) ;
#102566 = LINE ( 'NONE', #135887, #95455 ) ;
#102567 = UNCERTAINTY_MEASURE_WITH_UNIT (LENGTH_MEASURE( 1.000000000000000082E-05 ), #21150, 'distance_accuracy_value', 'NONE');
#102568 = DIRECTION ( 'NONE',  ( 0.6830127018922180770, -0.6830127018922204085, -0.2588190451025213501 ) ) ;
#102569 = DIRECTION ( 'NONE',  ( -0.6830127018922180770, -0.6830127018922202975, -0.2588190451025213501 ) ) ;
#102570 = AXIS2_PLACEMENT_3D ( 'NONE', #47134, #60107, #47823 ) ;
#102571 = CARTESIAN_POINT ( 'NONE',  ( 74.74586038379622721, 3.974999999999996980, 6.884901960086287964 ) ) ;
#102572 = FACE_OUTER_BOUND ( 'NONE', #104621, .T. ) ;
#102573 = CARTESIAN_POINT ( 'NONE',  ( 51.18398860626899705, 28.73617430169823095, 5.000000000000000000 ) ) ;
#102574 = VERTEX_POINT ( 'NONE', #32836 ) ;
#102575 = CARTESIAN_POINT ( 'NONE',  ( 71.29166666666667140, 3.975000000000003642, -6.884901960086285300 ) ) ;
#102576 = CARTESIAN_POINT ( 'NONE',  ( 0.005480084712502889671, 28.92564299267938210, 4.000000000000000000 ) ) ;
#102577 = CARTESIAN_POINT ( 'NONE',  ( 14.29289321881336150, 11.25929247661560773, 5.000000000000000000 ) ) ;
#102579 = VECTOR ( 'NONE', #88189, 1000.000000000000000 ) ;
#102578 = DIRECTION ( 'NONE',  ( -1.000000000000000000, -0.000000000000000000, -0.000000000000000000 ) ) ;
#102580 = VECTOR ( 'NONE', #2491, 999.9999999999998863 ) ;
#102581 = ORIENTED_EDGE ( 'NONE', *, *, #111669, .T. ) ;
#102582 = ADVANCED_FACE ( 'NONE', ( #24080 ), #23340, .F. ) ;
#102583 = DIRECTION ( 'NONE',  ( -0.000000000000000000, 0.000000000000000000, 1.000000000000000000 ) ) ;
#102584 = LINE ( 'NONE', #114146, #306 ) ;
#102585 = CARTESIAN_POINT ( 'NONE',  ( 65.33376352523143282, 6.110000000000001208, 1.122388791418549305E-15 ) ) ;
#102586 = CARTESIAN_POINT ( 'NONE',  ( -72.29974487139158157, -27.71228299555256669, 4.000000000000000000 ) ) ;
#102587 = ORIENTED_EDGE ( 'NONE', *, *, #102129, .T. ) ;
#102588 = ORIENTED_EDGE ( 'NONE', *, *, #72046, .F. ) ;
#102589 = VECTOR ( 'NONE', #25748, 1000.000000000000000 ) ;
#102590 = CARTESIAN_POINT ( 'NONE',  ( 32.99451991528749062, 28.92564299267960948, 4.000000000000000000 ) ) ;
#102591 = CARTESIAN_POINT ( 'NONE',  ( 22.49999999999985079, -1.912538124160733766, 4.000000000000000000 ) ) ;
#102592 = CARTESIAN_POINT ( 'NONE',  ( 10.46799328145038821, 4.202752102959690472E-16, 0.000000000000000000 ) ) ;
#102593 = CARTESIAN_POINT ( 'NONE',  ( 1.171830600776468945, 6.759292476615660128, 4.000000000000000000 ) ) ;
#102595 = ORIENTED_EDGE ( 'NONE', *, *, #101966, .F. ) ;
#102594 = CARTESIAN_POINT ( 'NONE',  ( 85.14583333333334281, 2.130196079827394229, -7.950000000000021494 ) ) ;
#102596 = LINE ( 'NONE', #67854, #134126 ) ;
#102597 = FACE_OUTER_BOUND ( 'NONE', #77482, .T. ) ;
#102598 = AXIS2_PLACEMENT_3D ( 'NONE', #50679, #28928, #127524 ) ;
#102599 = DIRECTION ( 'NONE',  ( 0.000000000000000000, 0.6666666666666630769, -0.7453559924999331177 ) ) ;
#102600 = DIRECTION ( 'NONE',  ( -0.7071067811865486830, 0.7071067811865464625, 0.000000000000000000 ) ) ;
#102601 = EDGE_LOOP ( 'NONE', ( #105612, #109385, #34570, #14366 ) ) ;
#102602 = ORIENTED_EDGE ( 'NONE', *, *, #104229, .T. ) ;
#102603 = EDGE_CURVE ( 'NONE', #23998, #59778, #67613, .T. ) ;
#102604 = EDGE_LOOP ( 'NONE', ( #132877, #136340, #73154, #16066, #119553 ) ) ;
#102605 = EDGE_CURVE ( 'NONE', #74021, #52888, #22606, .T. ) ;
#102606 = DIRECTION ( 'NONE',  ( 0.7071067811865487940, 0.7071067811865463515, 0.000000000000000000 ) ) ;
#102607 = CARTESIAN_POINT ( 'NONE',  ( 0.000000000000000000, 7.776507174585697093E-16, -6.350000000000004086 ) ) ;
#102608 = CARTESIAN_POINT ( 'NONE',  ( 53.49999999999999289, 0.000000000000000000, -7.950000000000000178 ) ) ;
#102609 = ORIENTED_EDGE ( 'NONE', *, *, #31880, .T. ) ;
#102610 = EDGE_LOOP ( 'NONE', ( #91971, #93185, #135066, #33650 ) ) ;
#102611 = VECTOR ( 'NONE', #118166, 1000.000000000000000 ) ;
#102612 = CARTESIAN_POINT ( 'NONE',  ( 0.000000000000000000, 0.000000000000000000, 5.000000000000000000 ) ) ;
#102613 = CARTESIAN_POINT ( 'NONE',  ( -19.39435030839552709, 0.5803129815428644811, -30.75302245446138727 ) ) ;
#102614 = EDGE_CURVE ( 'NONE', #137076, #46388, #121232, .T. ) ;
#102615 = EDGE_CURVE ( 'NONE', #115197, #4933, #2277, .T. ) ;
#102616 = CIRCLE ( 'NONE', #118825, 9.500000000000000000 ) ;
#102617 = VERTEX_POINT ( 'NONE', #66171 ) ;
#102618 = DIRECTION ( 'NONE',  ( 0.000000000000000000, 0.000000000000000000, 1.000000000000000000 ) ) ;
#102619 = ORIENTED_EDGE ( 'NONE', *, *, #122358, .F. ) ;
#102620 = CARTESIAN_POINT ( 'NONE',  ( -15.29974487139158867, -27.71228299555216879, 4.000000000000000000 ) ) ;
#102621 = PLANE ( 'NONE',  #116531 ) ;
#102622 = AXIS2_PLACEMENT_3D ( 'NONE', #125682, #95884, #26362 ) ;
#102623 = ORIENTED_EDGE ( 'NONE', *, *, #88951, .F. ) ;
#102624 = EDGE_CURVE ( 'NONE', #56866, #136190, #46596, .T. ) ;
#102625 = FACE_BOUND ( 'NONE', #26701, .T. ) ;
#102626 = EDGE_CURVE ( 'NONE', #138219, #107914, #65470, .T. ) ;
#102627 = CARTESIAN_POINT ( 'NONE',  ( 9.017348362375173565, 22.22500000000000142, 21.65139844574516914 ) ) ;
#102628 = CARTESIAN_POINT ( 'NONE',  ( 21.32816939922337696, -3.740707523384241728, 4.000000000000000000 ) ) ;
#102629 = DIRECTION ( 'NONE',  ( -0.7071067811865486830, -0.7071067811865464625, 0.000000000000000000 ) ) ;
#102630 = DIRECTION ( 'NONE',  ( 0.7071067811865487940, 0.7071067811865463515, -0.000000000000000000 ) ) ;
#102631 = ORIENTED_EDGE ( 'NONE', *, *, #109213, .T. ) ;
#102632 = VECTOR ( 'NONE', #74919, 1000.000000000000000 ) ;
#102633 = VERTEX_POINT ( 'NONE', #98760 ) ;
#102634 = CARTESIAN_POINT ( 'NONE',  ( 105.0579301918981230, 6.110000000000000320, -1.637169565754156064 ) ) ;
#102635 = ORIENTED_EDGE ( 'NONE', *, *, #69725, .T. ) ;
#102636 = EDGE_CURVE ( 'NONE', #76093, #270, #45156, .T. ) ;
#102637 = CARTESIAN_POINT ( 'NONE',  ( 15.48921356237309510, -27.52281430457066236, 5.000000000000000000 ) ) ;
#102638 = ORIENTED_EDGE ( 'NONE', *, *, #19515, .T. ) ;
#102639 = DIRECTION ( 'NONE',  ( 0.3543493200069163240, -0.000000000000000000, 0.9351131265310288487 ) ) ;
#102640 = ADVANCED_FACE ( 'NONE', ( #69757 ), #5136, .F. ) ;
#102641 = AXIS2_PLACEMENT_3D ( 'NONE', #59190, #135311, #70768 ) ;
#102642 = LINE ( 'NONE', #123690, #94111 ) ;
#102643 = CARTESIAN_POINT ( 'NONE',  ( -22.49999999999984368, -13.53360074219759746, 5.000000000000000000 ) ) ;
#102644 = ORIENTED_EDGE ( 'NONE', *, *, #23951, .F. ) ;
#102645 = FACE_OUTER_BOUND ( 'NONE', #19435, .T. ) ;
#102646 = FACE_OUTER_BOUND ( 'NONE', #114744, .T. ) ;
#102647 = VECTOR ( 'NONE', #80761, 1000.000000000000000 ) ;
#102648 = SURFACE_STYLE_USAGE ( .BOTH. , #35266 ) ;
#102649 = CARTESIAN_POINT ( 'NONE',  ( 41.99451991528749062, 28.92564299267967343, 4.000000000000000000 ) ) ;
#102650 = FACE_OUTER_BOUND ( 'NONE', #40426, .T. ) ;
#102651 = ADVANCED_FACE ( 'NONE', ( #103068 ), #61040, .T. ) ;
#102652 = DIRECTION ( 'NONE',  ( 0.3543493200069162685, -0.000000000000000000, -0.9351131265310288487 ) ) ;
#102653 = VERTEX_POINT ( 'NONE', #102372 ) ;
#102654 = CARTESIAN_POINT ( 'NONE',  ( 0.2997448713915885632, -27.71228299555206220, 4.000000000000000000 ) ) ;
#102655 = CARTESIAN_POINT ( 'NONE',  ( -6.299744871391586898, -27.71228299555210484, 4.000000000000000000 ) ) ;
#102656 = VECTOR ( 'NONE', #113527, 1000.000000000000227 ) ;
#102657 = ORIENTED_EDGE ( 'NONE', *, *, #57353, .F. ) ;
#102658 = ORIENTED_EDGE ( 'NONE', *, *, #71691, .T. ) ;
#102659 = ORIENTED_EDGE ( 'NONE', *, *, #71521, .F. ) ;
#102660 = EDGE_CURVE ( 'NONE', #132295, #84209, #25481, .T. ) ;
#102661 = CARTESIAN_POINT ( 'NONE',  ( 53.52126352523143993, -4.472830434245838482, -4.472830434245840259 ) ) ;
#102662 = EDGE_CURVE ( 'NONE', #134058, #118870, #47995, .T. ) ;
#102663 = VERTEX_POINT ( 'NONE', #137125 ) ;
#102664 = EDGE_CURVE ( 'NONE', #35075, #135973, #126248, .T. ) ;
#102665 = CARTESIAN_POINT ( 'NONE',  ( 4.274972949537106715, 4.461849672132300881, 4.461849672132299105 ) ) ;
#102666 =( BOUNDED_CURVE ( )  B_SPLINE_CURVE ( 3, ( #30188, #128105, #83902, #95445 ),
 .UNSPECIFIED., .F., .T. ) 
 B_SPLINE_CURVE_WITH_KNOTS ( ( 4, 4 ),
 ( 5.143245962375964986, 6.645403452391246191 ),
 .UNSPECIFIED. ) 
 CURVE ( )  GEOMETRIC_REPRESENTATION_ITEM ( )  RATIONAL_B_SPLINE_CURVE ( ( 1.000000000000000000, 0.8206354192515240564, 0.8206354192515240564, 1.000000000000000000 ) ) 
 REPRESENTATION_ITEM ( '' )  );
#102667 = LINE ( 'NONE', #46159, #77268 ) ;
#102668 = EDGE_LOOP ( 'NONE', ( #43982, #126571, #123202, #123406 ) ) ;
#102669 = CARTESIAN_POINT ( 'NONE',  ( 3.299744871391591339, -27.71228299555208352, 4.000000000000000000 ) ) ;
#102670 = ORIENTED_EDGE ( 'NONE', *, *, #54339, .T. ) ;
#102671 = DIRECTION ( 'NONE',  ( 0.7071067811865487940, -0.7071067811865463515, 0.000000000000000000 ) ) ;
#102672 = CONICAL_SURFACE ( 'NONE', #19351, 2.055000000000000604, 0.9599310885968764806 ) ;
#102674 = EDGE_LOOP ( 'NONE', ( #40817, #29459, #87682, #43436 ) ) ;
#102673 = CARTESIAN_POINT ( 'NONE',  ( -33.79289321881321229, 12.75929247661558641, 5.000000000000000000 ) ) ;
#102675 = ORIENTED_EDGE ( 'NONE', *, *, #56518, .F. ) ;
#102676 = CARTESIAN_POINT ( 'NONE',  ( 10.49999999999992895, 3.653845994658403651, -4.504631822206392577 ) ) ;
#102677 = CYLINDRICAL_SURFACE ( 'NONE', #97024, 2.500000000000000444 ) ;
#102678 = CARTESIAN_POINT ( 'NONE',  ( -1.069960254864079419, -0.7407075233842770334, 13.87443053587611175 ) ) ;
#102679 = ORIENTED_EDGE ( 'NONE', *, *, #86316, .T. ) ;
#102680 = LINE ( 'NONE', #12775, #6422 ) ;
#102681 = EDGE_LOOP ( 'NONE', ( #28872, #2626, #42667, #34485 ) ) ;
#102682 = ORIENTED_EDGE ( 'NONE', *, *, #133759, .F. ) ;
#102683 = EDGE_LOOP ( 'NONE', ( #103449, #94179, #80560, #40554, #135588 ) ) ;
#102684 = FACE_OUTER_BOUND ( 'NONE', #102082, .T. ) ;
#102685 = VECTOR ( 'NONE', #92893, 1000.000000000000000 ) ;
#102686 = SURFACE_STYLE_FILL_AREA ( #37422 ) ;
#102687 = DIRECTION ( 'NONE',  ( -0.7071067811865487940, 0.7071067811865463515, 0.000000000000000000 ) ) ;
#102688 = LINE ( 'NONE', #14230, #44037 ) ;
#102689 = CARTESIAN_POINT ( 'NONE',  ( 33.48921356237309510, -27.52281430457078670, 5.000000000000000000 ) ) ;
#102690 = ORIENTED_EDGE ( 'NONE', *, *, #96349, .T. ) ;
#102691 = LINE ( 'NONE', #125133, #139730 ) ;
#102692 = CARTESIAN_POINT ( 'NONE',  ( 25.93706980810189222, 2.126176841940952134, -7.934999999999993392 ) ) ;
#102693 = DIRECTION ( 'NONE',  ( 0.7071067811865487940, 0.7071067811865463515, 0.000000000000000000 ) ) ;
#102694 = LINE ( 'NONE', #22936, #57627 ) ;
#102695 = DIRECTION ( 'NONE',  ( -0.7071067811865486830, -0.7071067811865464625, 0.000000000000000000 ) ) ;
#102696 = EDGE_LOOP ( 'NONE', ( #74752, #50323, #51866, #25476 ) ) ;
#102697 = ORIENTED_EDGE ( 'NONE', *, *, #139990, .T. ) ;
#102698 = ADVANCED_FACE ( 'NONE', ( #15300 ), #125545, .F. ) ;
#102699 = ORIENTED_EDGE ( 'NONE', *, *, #74466, .T. ) ;
#102700 = CARTESIAN_POINT ( 'NONE',  ( 95.16252705046289861, 7.949999999999998401, 1.460391307983218338E-15 ) ) ;
#102701 = DIRECTION ( 'NONE',  ( -0.000000000000000000, -0.000000000000000000, -1.000000000000000000 ) ) ;
#102702 = DIRECTION ( 'NONE',  ( 0.3543493200069162685, -0.000000000000000000, -0.9351131265310288487 ) ) ;
#102703 = CARTESIAN_POINT ( 'NONE',  ( 5.949829201373897369, 9.500078657251188829, -0.2878427395703713754 ) ) ;
#102704 = AXIS2_PLACEMENT_3D ( 'NONE', #133308, #78933, #23059 ) ;
#102705 = FACE_OUTER_BOUND ( 'NONE', #27708, .T. ) ;
#102706 = FACE_OUTER_BOUND ( 'NONE', #52614, .T. ) ;
#102707 = CARTESIAN_POINT ( 'NONE',  ( 12.75860074219786711, 21.72500000000000142, 5.000000000000000000 ) ) ;
#102708 = CARTESIAN_POINT ( 'NONE',  ( -8.999999999999937828, 7.007997736742436423, -8.085015511992134307 ) ) ;
#102709 = DIRECTION ( 'NONE',  ( -0.7071067811865487940, 0.7071067811865463515, -0.000000000000000000 ) ) ;
#102711 = VERTEX_POINT ( 'NONE', #4387 ) ;
#102710 = PRODUCT_DEFINITION_FORMATION_WITH_SPECIFIED_SOURCE ( 'ANY', '', #72462, .NOT_KNOWN. ) ;
#102712 = CARTESIAN_POINT ( 'NONE',  ( 6.302772524220206840, -22.22500000000000142, -10.62274418449467284 ) ) ;
#102713 = ORIENTED_EDGE ( 'NONE', *, *, #32210, .F. ) ;
#102714 = LINE ( 'NONE', #2654, #76173 ) ;
#102716 = EDGE_LOOP ( 'NONE', ( #114845, #70435, #3752, #55761, #45839, #19727 ) ) ;
#102715 = CYLINDRICAL_SURFACE ( 'NONE', #88133, 0.5000000000000001110 ) ;
#102717 = ADVANCED_FACE ( 'NONE', ( #48688 ), #92892, .F. ) ;
#102718 = DIRECTION ( 'NONE',  ( 0.000000000000000000, 0.000000000000000000, 1.000000000000000000 ) ) ;
#102719 = LINE ( 'NONE', #6203, #130624 ) ;
#102720 = ORIENTED_EDGE ( 'NONE', *, *, #49271, .F. ) ;
#102721 = EDGE_CURVE ( 'NONE', #102268, #115069, #113934, .T. ) ;
#102722 = CARTESIAN_POINT ( 'NONE',  ( 26.90840764549667696, 9.139736423841732040E-16, 0.000000000000000000 ) ) ;
#102723 = ORIENTED_EDGE ( 'NONE', *, *, #57982, .F. ) ;
#102724 = FILL_AREA_STYLE ('',( #38187 ) ) ;
#102725 = VERTEX_POINT ( 'NONE', #24778 ) ;
#102726 = CARTESIAN_POINT ( 'NONE',  ( -2.999999999999981792, 8.966399257802175171, 5.000000000000000000 ) ) ;
#102727 = CARTESIAN_POINT ( 'NONE',  ( 105.8083603837962414, 7.949999999999997513, 2.130196079827431088 ) ) ;
#102728 = CARTESIAN_POINT ( 'NONE',  ( -27.48921356237309155, -27.52281430457074762, 5.000000000000000000 ) ) ;
#102729 = AXIS2_PLACEMENT_3D ( 'NONE', #54953, #131069, #53513 ) ;
#102730 = CARTESIAN_POINT ( 'NONE',  ( 13.92145407031093818, -2.500000000000000444, 3.061616997868384127E-16 ) ) ;
#102731 = ORIENTED_EDGE ( 'NONE', *, *, #129943, .T. ) ;
#102732 = EDGE_CURVE ( 'NONE', #74042, #99982, #69026, .T. ) ;
#102733 = DIRECTION ( 'NONE',  ( -0.000000000000000000, 0.3543493200069153248, 0.9351131265310292928 ) ) ;
#102734 = CARTESIAN_POINT ( 'NONE',  ( 30.48921356237309510, -27.52281430457076894, 5.000000000000000000 ) ) ;
#102735 = LINE ( 'NONE', #123787, #143318 ) ;
#102736 = CARTESIAN_POINT ( 'NONE',  ( 25.08333333333333570, -5.278424836066144543, 3.047499999999995879 ) ) ;
#102737 = CARTESIAN_POINT ( 'NONE',  ( 6.489213562373093325, -27.52281430457059841, 5.000000000000000000 ) ) ;
#102738 = LINE ( 'NONE', #114310, #9581 ) ;
#102739 = ORIENTED_EDGE ( 'NONE', *, *, #67966, .F. ) ;
#102740 = VECTOR ( 'NONE', #110305, 1000.000000000000227 ) ;
#102741 = EDGE_CURVE ( 'NONE', #39763, #99698, #82065, .T. ) ;
#102742 = DIRECTION ( 'NONE',  ( 0.5735764363510448272, -0.8191520442889927978, 1.003171929053526103E-16 ) ) ;
#102743 = VERTEX_POINT ( 'NONE', #126934 ) ;
#102744 = VECTOR ( 'NONE', #108161, 1000.000000000000227 ) ;
#102745 = CARTESIAN_POINT ( 'NONE',  ( 92.16709685856477563, -3.055000000000000160, -5.291415217122921177 ) ) ;
#102746 = CARTESIAN_POINT ( 'NONE',  ( -3.299744871391591339, -27.71228299555208352, 4.000000000000000000 ) ) ;
#102747 = CYLINDRICAL_SURFACE ( 'NONE', #53250, 0.5000000000000004441 ) ;
#102748 = CARTESIAN_POINT ( 'NONE',  ( -12.69999999999998153, 0.000000000000000000, 2.500000000000000444 ) ) ;
#102749 = CARTESIAN_POINT ( 'NONE',  ( 125.0591050317621011, -46.71325913968131260, -35.40428284070993215 ) ) ;
#102750 = ORIENTED_EDGE ( 'NONE', *, *, #105471, .T. ) ;
#102751 = EDGE_CURVE ( 'NONE', #77866, #102292, #135698, .T. ) ;
#102752 = CARTESIAN_POINT ( 'NONE',  ( -34.92500000000001137, -13.29806943317885448, 4.500000000000000888 ) ) ;
#102753 = AXIS2_PLACEMENT_3D ( 'NONE', #72792, #116945, #43674 ) ;
#102754 = LINE ( 'NONE', #56436, #62807 ) ;
#102755 = ORIENTED_EDGE ( 'NONE', *, *, #130646, .T. ) ;
#102756 = CARTESIAN_POINT ( 'NONE',  ( -34.42499999999997584, 22.27000000000000668, 0.000000000000000000 ) ) ;
#102757 = FACE_OUTER_BOUND ( 'NONE', #36332, .T. ) ;
#102759 = ORIENTED_EDGE ( 'NONE', *, *, #79321, .F. ) ;
#102758 = CARTESIAN_POINT ( 'NONE',  ( -34.75611968250420603, -1.294349301475922642, 4.955485411084897152 ) ) ;
#102760 = DIRECTION ( 'NONE',  ( -0.000000000000000000, -0.3543493200069152693, 0.9351131265310292928 ) ) ;
#102761 = EDGE_CURVE ( 'NONE', #66673, #69645, #29072, .T. ) ;
#102762 = CARTESIAN_POINT ( 'NONE',  ( 102.7458603837962272, 3.974999999999996980, 6.884901960086287964 ) ) ;
#102763 = DIRECTION ( 'NONE',  ( 0.7071067811865486830, -0.7071067811865464625, -0.000000000000000000 ) ) ;
#102764 = VECTOR ( 'NONE', #77410, 999.9999999999998863 ) ;
#102765 = PLANE ( 'NONE',  #116402 ) ;
#102766 = VECTOR ( 'NONE', #47763, 1000.000000000000227 ) ;
#102767 = VERTEX_POINT ( 'NONE', #31226 ) ;
#102768 = ORIENTED_EDGE ( 'NONE', *, *, #75675, .T. ) ;
#102769 = VERTEX_POINT ( 'NONE', #74743 ) ;
#102770 = CARTESIAN_POINT ( 'NONE',  ( 81.66709685856477563, -3.055000000000000160, -5.291415217122921177 ) ) ;
#102771 = VECTOR ( 'NONE', #5632, 1000.000000000000000 ) ;
#102772 = VERTEX_POINT ( 'NONE', #19613 ) ;
#102773 = LINE ( 'NONE', #12169, #85659 ) ;
#102774 = EDGE_CURVE ( 'NONE', #134932, #46795, #105884, .T. ) ;
#102775 = CARTESIAN_POINT ( 'NONE',  ( 15.18398860626900237, 28.73617430169797871, 5.000000000000000000 ) ) ;
#102776 = AXIS2_PLACEMENT_3D ( 'NONE', #101274, #1222, #55650 ) ;
#102777 = CARTESIAN_POINT ( 'NONE',  ( 27.48921356237309155, -27.52281430457074762, 5.000000000000000000 ) ) ;
#102778 = DIRECTION ( 'NONE',  ( -0.7071067811865487940, 0.7071067811865463515, -0.000000000000000000 ) ) ;
#102779 = ORIENTED_EDGE ( 'NONE', *, *, #43583, .T. ) ;
#102780 = CARTESIAN_POINT ( 'NONE',  ( 102.7916666666666714, 3.975000000000003642, -6.884901960086285300 ) ) ;
#102781 = LINE ( 'NONE', #2725, #49022 ) ;
#102782 = EDGE_CURVE ( 'NONE', #75896, #68092, #64551, .T. ) ;
#102783 = EDGE_CURVE ( 'NONE', #78277, #24426, #6546, .T. ) ;
#102784 = CARTESIAN_POINT ( 'NONE',  ( 28.00193056682079273, -22.22500000000000142, 4.500000000000000888 ) ) ;
#102785 = CARTESIAN_POINT ( 'NONE',  ( 80.70376352523145158, 6.109999999999998543, 1.122388791418548911E-15 ) ) ;
#102786 = ORIENTED_EDGE ( 'NONE', *, *, #41876, .F. ) ;
#102787 = CARTESIAN_POINT ( 'NONE',  ( 14.50183651486034364, -17.24070752338410628, 8.407044977365188743 ) ) ;
#102788 = DIRECTION ( 'NONE',  ( 1.000000000000000000, 0.000000000000000000, 0.000000000000000000 ) ) ;
#102789 = AXIS2_PLACEMENT_3D ( 'NONE', #40984, #84505, #117090 ) ;
#102790 = CARTESIAN_POINT ( 'NONE',  ( -18.29974487139159223, -27.71228299555219010, 4.000000000000000000 ) ) ;
#102791 = EDGE_CURVE ( 'NONE', #101876, #7107, #70275, .T. ) ;
#102792 = VERTEX_POINT ( 'NONE', #8685 ) ;
#102793 = VERTEX_POINT ( 'NONE', #40671 ) ;
#102794 = PLANE ( 'NONE',  #35361 ) ;
#102795 = EDGE_CURVE ( 'NONE', #108674, #11065, #118924, .T. ) ;
#102796 = EDGE_CURVE ( 'NONE', #65481, #31173, #107255, .T. ) ;
#102797 = FILL_AREA_STYLE_COLOUR ( '', #96355 ) ;
#102798 = CARTESIAN_POINT ( 'NONE',  ( 22.67123647476855552, 0.000000000000000000, 7.934999999999990727 ) ) ;
#102799 = LINE ( 'NONE', #91894, #95131 ) ;
#102800 = PLANE ( 'NONE',  #37236 ) ;
#102801 = LINE ( 'NONE', #88358, #140028 ) ;
#102802 = VECTOR ( 'NONE', #59712, 1000.000000000000000 ) ;
#102803 = ORIENTED_EDGE ( 'NONE', *, *, #117526, .T. ) ;
#102804 = ORIENTED_EDGE ( 'NONE', *, *, #83176, .F. ) ;
#102805 = EDGE_CURVE ( 'NONE', #33459, #54679, #106589, .T. ) ;
#102806 = DIRECTION ( 'NONE',  ( -0.6830127018922180770, -0.6830127018922204085, -0.2588190451025213501 ) ) ;
#102807 = ORIENTED_EDGE ( 'NONE', *, *, #75384, .F. ) ;
#102808 = EDGE_CURVE ( 'NONE', #67882, #118195, #29761, .T. ) ;
#102809 = AXIS2_PLACEMENT_3D ( 'NONE', #110616, #133143, #93003 ) ;
#102810 = CARTESIAN_POINT ( 'NONE',  ( 4.911592354503321545, 9.902892378096218942E-16, 0.000000000000000000 ) ) ;
#102811 = VERTEX_POINT ( 'NONE', #96425 ) ;
#102812 = DIRECTION ( 'NONE',  ( -0.000000000000000000, 0.000000000000000000, 1.000000000000000000 ) ) ;
#102813 = CARTESIAN_POINT ( 'NONE',  ( 32.99451991528749062, 28.92564299267960948, 4.000000000000000000 ) ) ;
#102814 = DIRECTION ( 'NONE',  ( -0.6830127018922181881, 0.6830127018922202975, -0.2588190451025214056 ) ) ;
#102815 = DIRECTION ( 'NONE',  ( 0.000000000000000000, 0.000000000000000000, 1.000000000000000000 ) ) ;
#102816 = LINE ( 'NONE', #3458, #63029 ) ;
#102817 = EDGE_LOOP ( 'NONE', ( #82559, #140967, #58770, #91315 ) ) ;
#102818 = LINE ( 'NONE', #3460, #61070 ) ;
#102819 = CARTESIAN_POINT ( 'NONE',  ( 7.139999999999956160, -60.26999999999998892, -12.10072711459626227 ) ) ;
#102820 = ORIENTED_EDGE ( 'NONE', *, *, #101647, .T. ) ;
#102821 = DIRECTION ( 'NONE',  ( 0.000000000000000000, 0.000000000000000000, 1.000000000000000000 ) ) ;
#102822 = ORIENTED_EDGE ( 'NONE', *, *, #21103, .T. ) ;
#102823 = ORIENTED_EDGE ( 'NONE', *, *, #52871, .T. ) ;
#102824 = LINE ( 'NONE', #3466, #52825 ) ;
#102825 = ORIENTED_EDGE ( 'NONE', *, *, #113747, .T. ) ;
#102826 = ORIENTED_EDGE ( 'NONE', *, *, #94202, .F. ) ;
#102827 = PLANE ( 'NONE',  #39498 ) ;
#102828 = VECTOR ( 'NONE', #121348, 1000.000000000000000 ) ;
#102829 = EDGE_LOOP ( 'NONE', ( #35451, #71956, #25501, #7597 ) ) ;
#102830 = EDGE_CURVE ( 'NONE', #127404, #94791, #30509, .T. ) ;
#102831 = DIRECTION ( 'NONE',  ( 0.7071067811865486830, -0.7071067811865464625, -0.000000000000000000 ) ) ;
#102832 = EDGE_CURVE ( 'NONE', #92449, #55968, #59365, .T. ) ;
#102833 = AXIS2_PLACEMENT_3D ( 'NONE', #98097, #95223, #30717 ) ;
#102834 = CARTESIAN_POINT ( 'NONE',  ( 45.48921356237309510, -27.52281430457087197, 5.000000000000000000 ) ) ;
#102835 = CARTESIAN_POINT ( 'NONE',  ( 118.2712635252314470, 4.472830434245838482, 4.472830434245842035 ) ) ;
#102836 = CARTESIAN_POINT ( 'NONE',  ( -39.51168605928408084, 6.759292476615653023, 16.35960578974478707 ) ) ;
#102837 = EDGE_CURVE ( 'NONE', #137801, #70973, #86322, .T. ) ;
#102838 = LINE ( 'NONE', #2036, #124610 ) ;
#102839 = LINE ( 'NONE', #52018, #16547 ) ;
#102840 = FACE_BOUND ( 'NONE', #119968, .T. ) ;
#102841 = EDGE_CURVE ( 'NONE', #108986, #114269, #95748, .T. ) ;
#102842 = CARTESIAN_POINT ( 'NONE',  ( -34.92500000000001137, 22.22500000000000142, 4.000000000000000000 ) ) ;
#102843 =( NAMED_UNIT ( * ) PLANE_ANGLE_UNIT ( ) SI_UNIT ( $, .RADIAN. ) );
#102844 = ORIENTED_EDGE ( 'NONE', *, *, #48686, .T. ) ;
#102845 = FACE_OUTER_BOUND ( 'NONE', #68188, .T. ) ;
#102846 = VECTOR ( 'NONE', #79739, 1000.000000000000000 ) ;
#102847 = AXIS2_PLACEMENT_3D ( 'NONE', #90078, #23395, #24131 ) ;
#102848 = ORIENTED_EDGE ( 'NONE', *, *, #25938, .F. ) ;
#102849 = ORIENTED_EDGE ( 'NONE', *, *, #9549, .T. ) ;
#102850 = FACE_OUTER_BOUND ( 'NONE', #53561, .T. ) ;
#102851 = ORIENTED_EDGE ( 'NONE', *, *, #118777, .F. ) ;
#102852 = CARTESIAN_POINT ( 'NONE',  ( 22.17183060077632817, 15.75929247661557042, 4.000000000000000000 ) ) ;
#102853 = DIRECTION ( 'NONE',  ( 0.000000000000000000, 0.000000000000000000, -1.000000000000000000 ) ) ;
#102854 = DIRECTION ( 'NONE',  ( -1.000000000000000000, -0.000000000000000000, -0.000000000000000000 ) ) ;
#102855 = AXIS2_PLACEMENT_3D ( 'NONE', #113169, #94, #57404 ) ;
#102856 = CARTESIAN_POINT ( 'NONE',  ( -63.29974487139158867, -27.71228299555250274, 4.000000000000000000 ) ) ;
#102857 = DIRECTION ( 'NONE',  ( -0.5735764363510503783, -0.8191520442889886899, 0.000000000000000000 ) ) ;
#102858 = ORIENTED_EDGE ( 'NONE', *, *, #76639, .T. ) ;
#102859 = PLANE ( 'NONE',  #83556 ) ;
#102860 = ORIENTED_EDGE ( 'NONE', *, *, #31773, .T. ) ;
#102862 = VECTOR ( 'NONE', #93573, 1000.000000000000000 ) ;
#102861 = CARTESIAN_POINT ( 'NONE',  ( -16.46004848586580493, -22.22500000000000142, -1.997060384840000369 ) ) ;
#102863 = AXIS2_PLACEMENT_3D ( 'NONE', #3837, #138706, #37232 ) ;
#102864 = CARTESIAN_POINT ( 'NONE',  ( 26.90040314143521627, -7.934999999999989839, 2.126176841940957907 ) ) ;
#102865 = ORIENTED_EDGE ( 'NONE', *, *, #91631, .F. ) ;
#102866 = DIRECTION ( 'NONE',  ( 0.000000000000000000, -1.000000000000000000, 0.000000000000000000 ) ) ;
#102867 = CARTESIAN_POINT ( 'NONE',  ( -34.49999999999975842, -5.945670655168998842, 4.994342998332166772 ) ) ;
#102868 = ORIENTED_EDGE ( 'NONE', *, *, #33163, .T. ) ;
#102869 = VERTEX_POINT ( 'NONE', #28370 ) ;
#102870 = ORIENTED_EDGE ( 'NONE', *, *, #129155, .T. ) ;
#102871 = CARTESIAN_POINT ( 'NONE',  ( 8.816011393731004731, 28.73617430169781173, 5.000000000000000000 ) ) ;
#102872 = CARTESIAN_POINT ( 'NONE',  ( 2.207106781186534139, 6.759292476615653023, 5.000000000000000000 ) ) ;
#102873 = DIRECTION ( 'NONE',  ( 1.000000000000000000, 0.000000000000000000, 0.000000000000000000 ) ) ;
#102874 = FACE_OUTER_BOUND ( 'NONE', #59870, .T. ) ;
#102875 = ORIENTED_EDGE ( 'NONE', *, *, #44003, .T. ) ;
#102876 = DIRECTION ( 'NONE',  ( -0.000000000000000000, -0.3543493200069152693, 0.9351131265310292928 ) ) ;
#102877 = DIRECTION ( 'NONE',  ( -0.7071067811865486830, -0.7071067811865464625, -0.000000000000000000 ) ) ;
#102878 = VECTOR ( 'NONE', #109762, 1000.000000000000227 ) ;
#102879 = FACE_OUTER_BOUND ( 'NONE', #121018, .T. ) ;
#102880 = DIRECTION ( 'NONE',  ( 1.000000000000000000, 0.000000000000000000, 0.000000000000000000 ) ) ;
#102881 = ORIENTED_EDGE ( 'NONE', *, *, #107582, .F. ) ;
#102882 = CARTESIAN_POINT ( 'NONE',  ( 0.000000000000000000, -34.64999999999999147, 17.49210858042621908 ) ) ;
#102883 = ORIENTED_EDGE ( 'NONE', *, *, #124042, .T. ) ;
#102884 = ADVANCED_FACE ( 'NONE', ( #72628 ), #129084, .F. ) ;
#102885 = EDGE_LOOP ( 'NONE', ( #42330, #40247, #126539, #3497 ) ) ;
#102886 = ORIENTED_EDGE ( 'NONE', *, *, #50354, .F. ) ;
#102887 = EDGE_CURVE ( 'NONE', #10395, #13638, #118185, .T. ) ;
#102888 = EDGE_CURVE ( 'NONE', #23831, #60214, #35600, .T. ) ;
#102889 = CARTESIAN_POINT ( 'NONE',  ( 34.42499999999998295, 21.72500000000000142, 4.000000000000000000 ) ) ;
#102890 = DIRECTION ( 'NONE',  ( 0.7071067811865486830, -0.7071067811865464625, -0.000000000000000000 ) ) ;
#102891 = VERTEX_POINT ( 'NONE', #54423 ) ;
#102892 = LINE ( 'NONE', #34786, #74478 ) ;
#102893 = UNCERTAINTY_MEASURE_WITH_UNIT (LENGTH_MEASURE( 1.000000000000000082E-05 ), #116752, 'distance_accuracy_value', 'NONE');
#102894 = VERTEX_POINT ( 'NONE', #10850 ) ;
#102895 = EDGE_CURVE ( 'NONE', #74472, #126742, #31927, .T. ) ;
#102896 = EDGE_CURVE ( 'NONE', #88917, #3869, #53697, .T. ) ;
#102897 = LINE ( 'NONE', #14450, #135551 ) ;
#102898 = LINE ( 'NONE', #100746, #80950 ) ;
#102899 = CARTESIAN_POINT ( 'NONE',  ( -42.18398860626899705, 28.73617430169816700, 5.000000000000000000 ) ) ;
#102900 = DIRECTION ( 'NONE',  ( -0.000000000000000000, -0.3543493200069152693, 0.9351131265310292928 ) ) ;
#102901 = CARTESIAN_POINT ( 'NONE',  ( -30.51665438641024153, 22.22500000000000142, 4.500000000000000888 ) ) ;
#102902 = EDGE_CURVE ( 'NONE', #108896, #85524, #32653, .T. ) ;
#102903 = DIRECTION ( 'NONE',  ( -4.681814790819591790E-17, -0.3543493200069152693, 0.9351131265310292928 ) ) ;
#102904 = DIRECTION ( 'NONE',  ( -0.7071067811865487940, 0.7071067811865463515, -0.000000000000000000 ) ) ;
#102905 = CARTESIAN_POINT ( 'NONE',  ( 30.02040314143521726, 7.934999999999989839, -2.126176841940961904 ) ) ;
#102906 = CARTESIAN_POINT ( 'NONE',  ( -6.792893218813400580, -20.24070752338406720, 5.000000000000000000 ) ) ;
#102907 = DIRECTION ( 'NONE',  ( 1.000000000000000000, 0.000000000000000000, 0.000000000000000000 ) ) ;
#102908 = PLANE ( 'NONE',  #83743 ) ;
#102909 = DIRECTION ( 'NONE',  ( -0.6830127018922180770, -0.6830127018922204085, -0.2588190451025213501 ) ) ;
#102910 = ORIENTED_EDGE ( 'NONE', *, *, #36850, .T. ) ;
#102911 = CIRCLE ( 'NONE', #93696, 2.500000000000000888 ) ;
#102912 = EDGE_LOOP ( 'NONE', ( #127011, #77828, #124269, #112752 ) ) ;
#102914 = EDGE_CURVE ( 'NONE', #114916, #100722, #143537, .T. ) ;
#102913 = CARTESIAN_POINT ( 'NONE',  ( 90.83333333333332860, -6.884901960086287964, 3.974999999999998312 ) ) ;
#102915 = EDGE_LOOP ( 'NONE', ( #14083, #3927, #92035, #116886, #68084, #65239 ) ) ;
#102916 = ORIENTED_EDGE ( 'NONE', *, *, #108372, .F. ) ;
#102917 = DIRECTION ( 'NONE',  ( -0.000000000000000000, 1.000000000000000000, 2.921639538487157626E-15 ) ) ;
#102918 = CARTESIAN_POINT ( 'NONE',  ( -31.62823445044366011, -8.240707523384200428, 11.38925528200759985 ) ) ;
#102919 = CARTESIAN_POINT ( 'NONE',  ( 14.64180977014269303, 9.473308030796305346, -0.7257954063774550990 ) ) ;
#102920 = ORIENTED_EDGE ( 'NONE', *, *, #3894, .T. ) ;
#102921 = ADVANCED_FACE ( 'NONE', ( #11561 ), #700, .F. ) ;
#102922 = CARTESIAN_POINT ( 'NONE',  ( 23.99999999999983302, -9.033600742197648970, 5.000000000000000000 ) ) ;
#102923 = DIRECTION ( 'NONE',  ( -0.7071067811865486830, 0.7071067811865464625, 0.000000000000000000 ) ) ;
#102924 = DIRECTION ( 'NONE',  ( 0.000000000000000000, 1.000000000000000000, 0.000000000000000000 ) ) ;
#102925 = CARTESIAN_POINT ( 'NONE',  ( 125.6430803969771404, -1.520810258758055200, -7.661534144229997345 ) ) ;
#102926 = FACE_OUTER_BOUND ( 'NONE', #62724, .T. ) ;
#102927 = DIRECTION ( 'NONE',  ( -0.000000000000000000, -0.000000000000000000, 1.000000000000000000 ) ) ;
#102929 = EDGE_CURVE ( 'NONE', #100675, #136109, #123241, .T. ) ;
#102928 = VECTOR ( 'NONE', #24892, 1000.000000000000114 ) ;
#102930 = CARTESIAN_POINT ( 'NONE',  ( -29.99999999999979039, -10.77435723561697856, -9.972017380717161927 ) ) ;
#102931 = CARTESIAN_POINT ( 'NONE',  ( -31.49999999999977973, -1.533600742197726463, 5.000000000000000000 ) ) ;
#102932 = DIRECTION ( 'NONE',  ( 0.7071067811865486830, -0.7071067811865464625, -0.000000000000000000 ) ) ;
#102933 = DIRECTION ( 'NONE',  ( -1.000000000000000000, -1.224606353822377258E-16, -0.000000000000000000 ) ) ;
#102934 =( NAMED_UNIT ( * ) SI_UNIT ( $, .STERADIAN. ) SOLID_ANGLE_UNIT ( ) );
#102935 = VECTOR ( 'NONE', #79792, 999.9999999999998863 ) ;
#102936 = ORIENTED_EDGE ( 'NONE', *, *, #55548, .T. ) ;
#102937 = ORIENTED_EDGE ( 'NONE', *, *, #95459, .T. ) ;
#102938 = CARTESIAN_POINT ( 'NONE',  ( 112.5837635252314470, -6.110000000000001208, -3.741295971395164515E-16 ) ) ;
#102939 = VERTEX_POINT ( 'NONE', #120315 ) ;
#102940 = CIRCLE ( 'NONE', #98285, 2.500000000000000444 ) ;
#102941 = EDGE_CURVE ( 'NONE', #70528, #14309, #131236, .T. ) ;
#102942 = PLANE ( 'NONE',  #59460 ) ;
#102943 = ORIENTED_EDGE ( 'NONE', *, *, #116243, .F. ) ;
#102944 = LINE ( 'NONE', #3589, #18943 ) ;
#102946 =( BOUNDED_CURVE ( )  B_SPLINE_CURVE ( 3, ( #126842, #27531, #71795, #16666 ),
 .UNSPECIFIED., .F., .F. ) 
 B_SPLINE_CURVE_WITH_KNOTS ( ( 4, 4 ),
 ( 2.431655599645420551, 2.488862747797045305 ),
 .UNSPECIFIED. ) 
 CURVE ( )  GEOMETRIC_REPRESENTATION_ITEM ( )  RATIONAL_B_SPLINE_CURVE ( ( 1.000000000000000000, 0.9997272971104411710, 0.9997272971104411710, 1.000000000000000000 ) ) 
 REPRESENTATION_ITEM ( '' )  );
#102945 = FACE_OUTER_BOUND ( 'NONE', #61449, .T. ) ;
#102947 = EDGE_CURVE ( 'NONE', #130461, #11776, #133397, .T. ) ;
#102948 = CARTESIAN_POINT ( 'NONE',  ( 106.9537635252314516, -6.109999999999998543, -3.741295971395162543E-16 ) ) ;
#102949 = AXIS2_PLACEMENT_3D ( 'NONE', #116057, #137116, #70480 ) ;
#102950 = ORIENTED_EDGE ( 'NONE', *, *, #110056, .F. ) ;
#102951 = EDGE_CURVE ( 'NONE', #94040, #49508, #12302, .T. ) ;
#102952 = ORIENTED_EDGE ( 'NONE', *, *, #35415, .T. ) ;
#102953 = LINE ( 'NONE', #126132, #3626 ) ;
#102954 = FACE_OUTER_BOUND ( 'NONE', #105311, .T. ) ;
#102955 =( BOUNDED_CURVE ( )  B_SPLINE_CURVE ( 3, ( #57672, #2511, #135231, #80139 ),
 .UNSPECIFIED., .F., .T. ) 
 B_SPLINE_CURVE_WITH_KNOTS ( ( 4, 4 ),
 ( 3.953918675577642539, 4.014082184732835401 ),
 .UNSPECIFIED. ) 
 CURVE ( )  GEOMETRIC_REPRESENTATION_ITEM ( )  RATIONAL_B_SPLINE_CURVE ( ( 1.000000000000000000, 0.9996983854260930169, 0.9996983854260930169, 1.000000000000000000 ) ) 
 REPRESENTATION_ITEM ( '' )  );
#102956 = EDGE_CURVE ( 'NONE', #55852, #117536, #91155, .T. ) ;
#102957 = ORIENTED_EDGE ( 'NONE', *, *, #116761, .F. ) ;
#102958 = ORIENTED_EDGE ( 'NONE', *, *, #126516, .T. ) ;
#102959 = VERTEX_POINT ( 'NONE', #22443 ) ;
#102960 = DIRECTION ( 'NONE',  ( 0.7071067811865486830, -0.7071067811865464625, -0.000000000000000000 ) ) ;
#102961 = DIRECTION ( 'NONE',  ( 0.7071067811865487940, 0.7071067811865463515, 0.000000000000000000 ) ) ;
#102962 = AXIS2_PLACEMENT_3D ( 'NONE', #67086, #123631, #24285 ) ;
#102963 = CIRCLE ( 'NONE', #40469, 0.5000000000000004441 ) ;
#102964 = VECTOR ( 'NONE', #3511, 999.9999999999998863 ) ;
#102965 = DIRECTION ( 'NONE',  ( 0.7071067811865486830, -0.7071067811865464625, -0.000000000000000000 ) ) ;
#102966 = ORIENTED_EDGE ( 'NONE', *, *, #24635, .T. ) ;
#102967 = VERTEX_POINT ( 'NONE', #122481 ) ;
#102968 = EDGE_CURVE ( 'NONE', #37148, #73565, #42823, .T. ) ;
#102969 = LINE ( 'NONE', #38422, #126620 ) ;
#102970 = ORIENTED_EDGE ( 'NONE', *, *, #24004, .F. ) ;
#102971 = ORIENTED_EDGE ( 'NONE', *, *, #58023, .F. ) ;
#102972 = CARTESIAN_POINT ( 'NONE',  ( -10.26506670282044453, 12.75929247661558996, 18.34774599283958807 ) ) ;
#102973 = DIRECTION ( 'NONE',  ( -0.6830127018922180770, -0.6830127018922204085, -0.2588190451025213501 ) ) ;
#102974 = LINE ( 'NONE', #37727, #123014 ) ;
#102975 = EDGE_CURVE ( 'NONE', #46538, #142384, #88465, .T. ) ;
#102976 = EDGE_LOOP ( 'NONE', ( #18164, #116220, #11553, #44290 ) ) ;
#102977 = CARTESIAN_POINT ( 'NONE',  ( 18.18398860626898994, 28.73617430169800002, 5.000000000000000000 ) ) ;
#102978 = PLANE ( 'NONE',  #93007 ) ;
#102979 = ADVANCED_FACE ( 'NONE', ( #109484 ), #77597, .F. ) ;
#102980 = FACE_BOUND ( 'NONE', #137736, .T. ) ;
#102981 = ORIENTED_EDGE ( 'NONE', *, *, #35545, .T. ) ;
#102982 = CARTESIAN_POINT ( 'NONE',  ( -8.510786437626906675, -27.52281430457049183, 5.000000000000000000 ) ) ;
#102983 = DIRECTION ( 'NONE',  ( -0.7071067811865487940, 0.7071067811865463515, 0.000000000000000000 ) ) ;
#102984 = CARTESIAN_POINT ( 'NONE',  ( 5.700255128608413102, -27.71228299555201957, 4.000000000000000000 ) ) ;
#102985 = ORIENTED_EDGE ( 'NONE', *, *, #91595, .T. ) ;
#102986 = FACE_OUTER_BOUND ( 'NONE', #47942, .T. ) ;
#102987 = ORIENTED_EDGE ( 'NONE', *, *, #131135, .T. ) ;
#102988 = ORIENTED_EDGE ( 'NONE', *, *, #1398, .F. ) ;
#102989 = ORIENTED_EDGE ( 'NONE', *, *, #23332, .T. ) ;
#102990 = EDGE_CURVE ( 'NONE', #15277, #111034, #67434, .T. ) ;
#102991 = CARTESIAN_POINT ( 'NONE',  ( 37.09959685856476597, -6.109999999999997655, -1.637169565754160283 ) ) ;
#102992 = ORIENTED_EDGE ( 'NONE', *, *, #1248, .T. ) ;
#102993 = FACE_OUTER_BOUND ( 'NONE', #90787, .T. ) ;
#102994 = PLANE ( 'NONE',  #2081 ) ;
#102995 = CARTESIAN_POINT ( 'NONE',  ( -0.1839886062690032631, 28.73617430169787568, 5.000000000000000000 ) ) ;
#102996 = ORIENTED_EDGE ( 'NONE', *, *, #64819, .F. ) ;
#102997 = DIRECTION ( 'NONE',  ( -0.000000000000000000, -0.3543493200069152693, 0.9351131265310292928 ) ) ;
#102998 =( LENGTH_UNIT ( ) NAMED_UNIT ( * ) SI_UNIT ( .MILLI., .METRE. ) );
#102999 = VECTOR ( 'NONE', #41128, 1000.000000000000000 ) ;
#103000 = DIRECTION ( 'NONE',  ( -0.7071067811865486830, -0.7071067811865464625, 0.000000000000000000 ) ) ;
#103001 = EDGE_CURVE ( 'NONE', #139983, #32917, #43513, .T. ) ;
#103002 = CARTESIAN_POINT ( 'NONE',  ( 63.18398860626900415, 28.73617430169831621, 5.000000000000000000 ) ) ;
#103003 = CARTESIAN_POINT ( 'NONE',  ( 26.20710678118636494, -14.24070752338413293, 5.000000000000000000 ) ) ;
#103004 = FILL_AREA_STYLE ('',( #108845 ) ) ;
#103005 = DIRECTION ( 'NONE',  ( 0.6830127018922181881, 0.6830127018922202975, -0.2588190451025214056 ) ) ;
#103006 = ORIENTED_EDGE ( 'NONE', *, *, #55281, .F. ) ;
#103007 = VERTEX_POINT ( 'NONE', #87734 ) ;
#103008 = ORIENTED_EDGE ( 'NONE', *, *, #38759, .F. ) ;
#103009 = ORIENTED_EDGE ( 'NONE', *, *, #114729, .T. ) ;
#103010 = PRESENTATION_STYLE_ASSIGNMENT (( #137068 ) ) ;
#103011 = VERTEX_POINT ( 'NONE', #34086 ) ;
#103012 = ORIENTED_EDGE ( 'NONE', *, *, #96182, .T. ) ;
#103013 = DIRECTION ( 'NONE',  ( 0.6830127018922181881, 0.6830127018922202975, -0.2588190451025214056 ) ) ;
#103014 = DIRECTION ( 'NONE',  ( 0.7071067811865487940, -0.7071067811865463515, 0.000000000000000000 ) ) ;
#103015 = ADVANCED_FACE ( 'NONE', ( #110177 ), #66702, .F. ) ;
#103016 = DIRECTION ( 'NONE',  ( 0.000000000000000000, 0.000000000000000000, -1.000000000000000000 ) ) ;
#103017 = ORIENTED_EDGE ( 'NONE', *, *, #33578, .T. ) ;
#103018 = FACE_OUTER_BOUND ( 'NONE', #30847, .T. ) ;
#103019 = EDGE_LOOP ( 'NONE', ( #120037, #3098, #97234, #86347, #84584 ) ) ;
#103020 = DIRECTION ( 'NONE',  ( 0.3543493200069162685, -0.000000000000000000, -0.9351131265310288487 ) ) ;
#103021 = CIRCLE ( 'NONE', #42818, 2.500000000000000444 ) ;
#103022 = CARTESIAN_POINT ( 'NONE',  ( -3.707106781186510602, 14.25929247661557753, 5.000000000000000000 ) ) ;
#103023 = CARTESIAN_POINT ( 'NONE',  ( 4.587903141435219823, 6.871911579029515771, 3.967499999999989146 ) ) ;
#103024 = VERTEX_POINT ( 'NONE', #136945 ) ;
#103026 = CARTESIAN_POINT ( 'NONE',  ( 31.17183060077625356, 15.75929247661555088, 4.000000000000000000 ) ) ;
#103025 = CARTESIAN_POINT ( 'NONE',  ( 99.51626352523145158, -4.472830434245839371, 4.472830434245839371 ) ) ;
#103027 = VECTOR ( 'NONE', #42676, 1000.000000000000000 ) ;
#103028 = DIRECTION ( 'NONE',  ( 0.7071067811865486830, -0.7071067811865464625, -0.000000000000000000 ) ) ;
#103029 = DIRECTION ( 'NONE',  ( 1.000000000000000000, 0.000000000000000000, 0.000000000000000000 ) ) ;
#103030 = ORIENTED_EDGE ( 'NONE', *, *, #16087, .F. ) ;
#103031 = VERTEX_POINT ( 'NONE', #115151 ) ;
#103032 = CARTESIAN_POINT ( 'NONE',  ( -23.99451991528749062, 28.92564299267954908, 4.000000000000000000 ) ) ;
#103033 = EDGE_LOOP ( 'NONE', ( #94151, #69362, #75897, #122763 ) ) ;
#103034 = PLANE ( 'NONE',  #23095 ) ;
#103035 = FACE_OUTER_BOUND ( 'NONE', #48175, .T. ) ;
#103036 = CARTESIAN_POINT ( 'NONE',  ( 61.46640106136307935, -57.15000000000010516, 40.92499999999998295 ) ) ;
#103037 = DIRECTION ( 'NONE',  ( -0.7071067811865486830, 0.7071067811865464625, 0.000000000000000000 ) ) ;
#103038 =( NAMED_UNIT ( * ) PLANE_ANGLE_UNIT ( ) SI_UNIT ( $, .RADIAN. ) );
#103039 = ORIENTED_EDGE ( 'NONE', *, *, #114794, .T. ) ;
#103040 = AXIS2_PLACEMENT_3D ( 'NONE', #63154, #9405, #131963 ) ;
#103041 = PRESENTATION_STYLE_ASSIGNMENT (( #138529 ) ) ;
#103042 = LINE ( 'NONE', #94292, #125560 ) ;
#103043 = EDGE_LOOP ( 'NONE', ( #8607, #19041, #36922, #26327 ) ) ;
#103044 = CARTESIAN_POINT ( 'NONE',  ( 34.92499999999999005, 16.51246187583931402, 4.000000000000000000 ) ) ;
#103046 = ADVANCED_FACE ( 'NONE', ( #123950 ), #38355, .F. ) ;
#103045 = DIRECTION ( 'NONE',  ( -0.000000000000000000, -0.3543493200069152693, 0.9351131265310292928 ) ) ;
#103047 = ORIENTED_EDGE ( 'NONE', *, *, #30098, .T. ) ;
#103049 = VERTEX_POINT ( 'NONE', #82570 ) ;
#103048 = LINE ( 'NONE', #113190, #97290 ) ;
#103050 = ADVANCED_FACE ( 'NONE', ( #103582 ), #126763, .F. ) ;
#103051 = ORIENTED_EDGE ( 'NONE', *, *, #142978, .F. ) ;
#103052 = DIRECTION ( 'NONE',  ( 0.7071067811865487940, 0.7071067811865463515, -0.000000000000000000 ) ) ;
#103053 = FACE_OUTER_BOUND ( 'NONE', #18042, .T. ) ;
#103054 = EDGE_LOOP ( 'NONE', ( #76726, #110855, #117019, #10648, #94100 ) ) ;
#103055 = STYLED_ITEM ( 'NONE', ( #110501 ), #120064 ) ;
#103056 = ADVANCED_FACE ( 'NONE', ( #27444 ), #15826, .F. ) ;
#103057 = EDGE_CURVE ( 'NONE', #82496, #107486, #114464, .T. ) ;
#103058 = CARTESIAN_POINT ( 'NONE',  ( 52.18749999999999289, -5.819803920172573974, 5.819803920172573086 ) ) ;
#103059 = VECTOR ( 'NONE', #87504, 1000.000000000000000 ) ;
#103060 = FACE_OUTER_BOUND ( 'NONE', #104725, .T. ) ;
#103061 = EDGE_CURVE ( 'NONE', #91612, #20734, #124640, .T. ) ;
#103062 = ORIENTED_EDGE ( 'NONE', *, *, #128918, .T. ) ;
#103063 = VECTOR ( 'NONE', #108810, 1000.000000000000000 ) ;
#103064 = FACE_OUTER_BOUND ( 'NONE', #111934, .T. ) ;
#103065 = DIRECTION ( 'NONE',  ( 0.000000000000000000, -1.000000000000000000, 0.000000000000000000 ) ) ;
#103066 = ADVANCED_FACE ( 'NONE', ( #91327 ), #125364, .T. ) ;
#103067 = LINE ( 'NONE', #115315, #118483 ) ;
#103068 = FACE_OUTER_BOUND ( 'NONE', #12910, .T. ) ;
#103069 = DIRECTION ( 'NONE',  ( -0.7071067811865486830, -0.7071067811865464625, -0.000000000000000000 ) ) ;
#103070 = CARTESIAN_POINT ( 'NONE',  ( -25.39999999999996305, 3.061616997868383141E-16, -2.500000000000000000 ) ) ;
#103071 = EDGE_CURVE ( 'NONE', #133129, #121565, #13005, .T. ) ;
#103072 = CARTESIAN_POINT ( 'NONE',  ( 27.93336038379622011, 2.130196079827431532, -7.949999999999996625 ) ) ;
#103073 = FACE_OUTER_BOUND ( 'NONE', #81774, .T. ) ;
#103074 = ORIENTED_EDGE ( 'NONE', *, *, #100282, .F. ) ;
#103075 = ORIENTED_EDGE ( 'NONE', *, *, #71154, .F. ) ;
#103076 = VERTEX_POINT ( 'NONE', #93446 ) ;
#103078 = EDGE_CURVE ( 'NONE', #113229, #17021, #25314, .T. ) ;
#103077 = CARTESIAN_POINT ( 'NONE',  ( 120.0000000000000000, 0.000000000000000000, -7.950000000000000178 ) ) ;
#103079 = ORIENTED_EDGE ( 'NONE', *, *, #77063, .T. ) ;
#103080 = ORIENTED_EDGE ( 'NONE', *, *, #136838, .F. ) ;
#103081 = VERTEX_POINT ( 'NONE', #81896 ) ;
#103082 = FACE_OUTER_BOUND ( 'NONE', #83386, .T. ) ;
#103083 = CARTESIAN_POINT ( 'NONE',  ( 23.27718569542924243, -21.72500000000000142, 5.000000000000000000 ) ) ;
#103084 = ORIENTED_EDGE ( 'NONE', *, *, #62733, .F. ) ;
#103085 = DIRECTION ( 'NONE',  ( 0.7071067811865486830, -0.7071067811865464625, -0.000000000000000000 ) ) ;
#103086 = EDGE_CURVE ( 'NONE', #110589, #103699, #104289, .T. ) ;
#103087 = LINE ( 'NONE', #114650, #143539 ) ;
#103088 = PLANE ( 'NONE',  #25579 ) ;
#103089 = CARTESIAN_POINT ( 'NONE',  ( 115.6462635252314328, -4.472830434245840259, 4.472830434245839371 ) ) ;
#103090 = ORIENTED_EDGE ( 'NONE', *, *, #53776, .F. ) ;
#103091 = FACE_OUTER_BOUND ( 'NONE', #127454, .T. ) ;
#103092 = CARTESIAN_POINT ( 'NONE',  ( -30.75860074219774631, 21.72500000000000142, 5.000000000000000000 ) ) ;
#103093 = DIRECTION ( 'NONE',  ( -0.3543493200069162685, -0.000000000000000000, -0.9351131265310288487 ) ) ;
#103094 = CARTESIAN_POINT ( 'NONE',  ( 0.6891546199041412857, 7.409644225788786009, 0.3384941017316204226 ) ) ;
#103095 = CARTESIAN_POINT ( 'NONE',  ( -39.18398860626899705, 28.73617430169814568, 5.000000000000000000 ) ) ;
#103096 = ADVANCED_FACE ( 'NONE', ( #4216 ), #113035, .T. ) ;
#103097 = DIRECTION ( 'NONE',  ( 0.7071067811865487940, 0.7071067811865463515, -0.000000000000000000 ) ) ;
#103098 = DIRECTION ( 'NONE',  ( 0.7071067811865487940, 0.7071067811865463515, 0.000000000000000000 ) ) ;
#103099 = CARTESIAN_POINT ( 'NONE',  ( 49.95419371712955581, 6.884901960086283523, 3.975000000000002753 ) ) ;
#103100 = LINE ( 'NONE', #5886, #477 ) ;
#103101 = ORIENTED_EDGE ( 'NONE', *, *, #133729, .T. ) ;
#103102 = ORIENTED_EDGE ( 'NONE', *, *, #42566, .T. ) ;
#103103 = CARTESIAN_POINT ( 'NONE',  ( 34.24999999999998579, -9.735942053221458872E-16, 7.950000000000000178 ) ) ;
#103104 = ORIENTED_EDGE ( 'NONE', *, *, #54489, .F. ) ;
#103105 = VERTEX_POINT ( 'NONE', #69582 ) ;
#103106 = CARTESIAN_POINT ( 'NONE',  ( -32.99999999999976552, -10.06887692260770883, 4.000000000000000000 ) ) ;
#103107 = CARTESIAN_POINT ( 'NONE',  ( 0.2997448713915885632, -27.71228299555206220, 4.000000000000000000 ) ) ;
#103108 = ORIENTED_EDGE ( 'NONE', *, *, #86257, .T. ) ;
#103109 = FACE_OUTER_BOUND ( 'NONE', #71576, .T. ) ;
#103110 = DIRECTION ( 'NONE',  ( 1.000000000000000000, 1.224606353822377258E-16, 0.000000000000000000 ) ) ;
#103111 = DIRECTION ( 'NONE',  ( -1.000000000000000000, -1.224606353822377258E-16, -0.000000000000000000 ) ) ;
#103112 = CARTESIAN_POINT ( 'NONE',  ( 26.83376352523143993, 6.110000000000001208, 1.122388791418549305E-15 ) ) ;
#103113 = ORIENTED_EDGE ( 'NONE', *, *, #55648, .F. ) ;
#103114 = EDGE_CURVE ( 'NONE', #17152, #4875, #26753, .T. ) ;
#103115 = CARTESIAN_POINT ( 'NONE',  ( 1.353980332882009252, 0.3999999999999995226, 2.467792535850613866 ) ) ;
#103116 = VERTEX_POINT ( 'NONE', #35536 ) ;
#103117 = DIRECTION ( 'NONE',  ( 1.734723475976806848E-16, -1.000000000000000000, 0.000000000000000000 ) ) ;
#103118 = DIRECTION ( 'NONE',  ( -0.7071067811865487940, 0.7071067811865463515, -0.000000000000000000 ) ) ;
#103119 = EDGE_CURVE ( 'NONE', #106612, #142261, #14456, .T. ) ;
#103120 = CARTESIAN_POINT ( 'NONE',  ( 75.18398860626899705, 28.73617430169839793, 5.000000000000000000 ) ) ;
#103121 = ORIENTED_EDGE ( 'NONE', *, *, #51544, .T. ) ;
#103122 = ORIENTED_EDGE ( 'NONE', *, *, #47003, .T. ) ;
#103123 = DIRECTION ( 'NONE',  ( -0.6830127018922181881, 0.6830127018922202975, -0.2588190451025214056 ) ) ;
#103124 = DIRECTION ( 'NONE',  ( -1.000000000000000000, -1.224606353822377258E-16, -0.000000000000000000 ) ) ;
#103125 = LINE ( 'NONE', #137912, #80211 ) ;
#103126 = EDGE_CURVE ( 'NONE', #118697, #137485, #101454, .T. ) ;
#103127 = VECTOR ( 'NONE', #6777, 1000.000000000000000 ) ;
#103128 = CARTESIAN_POINT ( 'NONE',  ( 47.16209685856477307, -5.291415217122919401, 3.054999999999997939 ) ) ;
#103129 = VECTOR ( 'NONE', #40385, 1000.000000000000000 ) ;
#103130 = CARTESIAN_POINT ( 'NONE',  ( 123.7916666666666714, 3.975000000000003642, -6.884901960086285300 ) ) ;
#103131 = EDGE_CURVE ( 'NONE', #125931, #1788, #2102, .T. ) ;
#103132 = LINE ( 'NONE', #59655, #117198 ) ;
#103133 = VERTEX_POINT ( 'NONE', #79768 ) ;
#103134 = EDGE_LOOP ( 'NONE', ( #76520, #76880, #17393, #104660, #63400, #4208 ) ) ;
#103135 = DIRECTION ( 'NONE',  ( 0.000000000000000000, -1.000000000000000000, 0.000000000000000000 ) ) ;
#103136 = VERTEX_POINT ( 'NONE', #13707 ) ;
#103137 = AXIS2_PLACEMENT_3D ( 'NONE', #15656, #59945, #38189 ) ;
#103138 = DIRECTION ( 'NONE',  ( 0.7071067811865487940, -0.7071067811865463515, 0.000000000000000000 ) ) ;
#103139 = ORIENTED_EDGE ( 'NONE', *, *, #34919, .T. ) ;
#103140 = PLANE ( 'NONE',  #60829 ) ;
#103141 = SURFACE_SIDE_STYLE ('',( #58986 ) ) ;
#103142 = EDGE_CURVE ( 'NONE', #134353, #132741, #58000, .T. ) ;
#103143 = FACE_BOUND ( 'NONE', #125999, .T. ) ;
#103144 = PLANE ( 'NONE',  #41036 ) ;
#103145 = FACE_OUTER_BOUND ( 'NONE', #63518, .T. ) ;
#103146 = EDGE_CURVE ( 'NONE', #14576, #34692, #30324, .T. ) ;
#103147 = SURFACE_STYLE_USAGE ( .BOTH. , #49524 ) ;
#103149 = ORIENTED_EDGE ( 'NONE', *, *, #57092, .T. ) ;
#103148 = CARTESIAN_POINT ( 'NONE',  ( -25.39999999999996305, 0.000000000000000000, 0.000000000000000000 ) ) ;
#103150 = DIRECTION ( 'NONE',  ( 0.6830127018922181881, 0.6830127018922202975, -0.2588190451025214056 ) ) ;
#103151 = VECTOR ( 'NONE', #61585, 1000.000000000000000 ) ;
#103152 = ORIENTED_EDGE ( 'NONE', *, *, #75422, .T. ) ;
#103154 = ORIENTED_EDGE ( 'NONE', *, *, #140456, .T. ) ;
#103153 = AXIS2_PLACEMENT_3D ( 'NONE', #27481, #94168, #72482 ) ;
#103155 = CARTESIAN_POINT ( 'NONE',  ( 69.76626352523143737, 4.472830434245838482, -4.472830434245837594 ) ) ;
#103156 = ORIENTED_EDGE ( 'NONE', *, *, #141765, .F. ) ;
#103157 = VECTOR ( 'NONE', #25443, 1000.000000000000000 ) ;
#103158 = CYLINDRICAL_SURFACE ( 'NONE', #97321, 0.5000000000000004441 ) ;
#103159 = ORIENTED_EDGE ( 'NONE', *, *, #109610, .F. ) ;
#103160 = LINE ( 'NONE', #80722, #79203 ) ;
#103161 = VECTOR ( 'NONE', #54074, 1000.000000000000000 ) ;
#103162 = EDGE_CURVE ( 'NONE', #42123, #118497, #130369, .T. ) ;
#103163 = FACE_OUTER_BOUND ( 'NONE', #109202, .T. ) ;
#103164 = EDGE_CURVE ( 'NONE', #50292, #23319, #128226, .T. ) ;
#103165 = DIRECTION ( 'NONE',  ( -0.3543493200069162685, -0.000000000000000000, -0.9351131265310288487 ) ) ;
#103166 = CARTESIAN_POINT ( 'NONE',  ( -12.41161490594822681, 22.22500000000000142, 4.777194822843815025 ) ) ;
#103167 = DIRECTION ( 'NONE',  ( -0.3543493200069162685, -0.000000000000000000, -0.9351131265310288487 ) ) ;
#103168 = CARTESIAN_POINT ( 'NONE',  ( -48.48921356237309510, -27.52281430457089328, 5.000000000000000000 ) ) ;
#103169 = DIRECTION ( 'NONE',  ( -0.7071067811865487940, 0.7071067811865463515, 0.000000000000000000 ) ) ;
#103170 = ORIENTED_EDGE ( 'NONE', *, *, #127229, .F. ) ;
#103171 = EDGE_LOOP ( 'NONE', ( #88753, #136273, #130403, #67508, #39727 ) ) ;
#103172 = CARTESIAN_POINT ( 'NONE',  ( 34.92499999999998295, 5.831225763041736343, -1.212213889845644488 ) ) ;
#103173 = DIRECTION ( 'NONE',  ( 0.7071067811865487940, 0.7071067811865463515, 0.000000000000000000 ) ) ;
#103174 = VERTEX_POINT ( 'NONE', #6372 ) ;
#103175 = ORIENTED_EDGE ( 'NONE', *, *, #71181, .T. ) ;
#103176 = VERTEX_POINT ( 'NONE', #19444 ) ;
#103177 = EDGE_CURVE ( 'NONE', #85323, #141546, #115872, .T. ) ;
#103178 = CARTESIAN_POINT ( 'NONE',  ( 29.29166666666666075, 3.975000000000003642, -6.884901960086285300 ) ) ;
#103179 = EDGE_LOOP ( 'NONE', ( #44420, #138506, #117282, #80666 ) ) ;
#103180 = CARTESIAN_POINT ( 'NONE',  ( 25.49999999999982236, -10.04351517176476172, -1.623559851933764175 ) ) ;
#103181 = CARTESIAN_POINT ( 'NONE',  ( 42.95419371712954870, 6.884901960086283523, 3.975000000000002753 ) ) ;
#103182 = CARTESIAN_POINT ( 'NONE',  ( 4.879569808101885897, 3.967499999999998916, 6.871911579029510442 ) ) ;
#103183 = CARTESIAN_POINT ( 'NONE',  ( 34.75611968250419181, -0.1870657452926086095, 4.955485411084880276 ) ) ;
#103184 = VERTEX_POINT ( 'NONE', #72450 ) ;
#103185 = DIRECTION ( 'NONE',  ( -0.6830127018922180770, -0.6830127018922204085, -0.2588190451025213501 ) ) ;
#103186 = CARTESIAN_POINT ( 'NONE',  ( 119.3708603837962272, 6.884901960086289741, -3.974999999999993427 ) ) ;
#103187 = DIRECTION ( 'NONE',  ( -1.734723475976806848E-16, 1.000000000000000000, 0.000000000000000000 ) ) ;
#103189 = EDGE_LOOP ( 'NONE', ( #28583, #138478, #82011, #97047 ) ) ;
#103188 = CARTESIAN_POINT ( 'NONE',  ( 26.99999999999980815, -9.033600742197647193, 5.000000000000000000 ) ) ;
#103190 = ORIENTED_EDGE ( 'NONE', *, *, #17370, .T. ) ;
#103191 = DIRECTION ( 'NONE',  ( 0.7071067811865487940, 0.7071067811865463515, 0.000000000000000000 ) ) ;
#103192 = LINE ( 'NONE', #48840, #19079 ) ;
#103193 = CARTESIAN_POINT ( 'NONE',  ( -12.20000000000000284, -40.42999999999999261, -39.50000000000000000 ) ) ;
#103194 = ORIENTED_EDGE ( 'NONE', *, *, #100458, .F. ) ;
#103195 = LINE ( 'NONE', #81488, #124660 ) ;
#103196 = DIRECTION ( 'NONE',  ( 0.6830127018922181881, 0.6830127018922202975, -0.2588190451025214056 ) ) ;
#103197 = CARTESIAN_POINT ( 'NONE',  ( -34.49999999999975842, 10.94296225409023116, -9.576120664313334530 ) ) ;
#103198 = CARTESIAN_POINT ( 'NONE',  ( 34.49999999999976552, 3.054329344830917670, 4.994342998332163219 ) ) ;
#103199 = PLANE ( 'NONE',  #99985 ) ;
#103200 = VERTEX_POINT ( 'NONE', #86140 ) ;
#103201 = CARTESIAN_POINT ( 'NONE',  ( 7.940000000000001279, -33.26999999999999602, -11.89864999999999462 ) ) ;
#103202 = PLANE ( 'NONE',  #102550 ) ;
#103203 = CARTESIAN_POINT ( 'NONE',  ( 7.337472949537107603, 6.094999999999989981, -1.119633336120465690E-15 ) ) ;
#103204 = DIRECTION ( 'NONE',  ( 1.000000000000000000, 0.000000000000000000, 0.000000000000000000 ) ) ;
#103205 = FACE_OUTER_BOUND ( 'NONE', #70906, .T. ) ;
#103206 = VERTEX_POINT ( 'NONE', #118003 ) ;
#103207 = ORIENTED_EDGE ( 'NONE', *, *, #103230, .T. ) ;
#103208 = CARTESIAN_POINT ( 'NONE',  ( -31.17183060077625711, 0.7592924766157069794, 4.000000000000000000 ) ) ;
#103209 = CARTESIAN_POINT ( 'NONE',  ( 16.49999999999989342, -7.912538124160671593, 4.000000000000000000 ) ) ;
#103210 = CARTESIAN_POINT ( 'NONE',  ( 5.520403141435220817, 7.934999999999989839, -2.126176841940961904 ) ) ;
#103211 = VECTOR ( 'NONE', #39596, 1000.000000000000000 ) ;
#103212 = CARTESIAN_POINT ( 'NONE',  ( 11.20710678118646619, -14.24070752338413648, 5.000000000000000000 ) ) ;
#103213 = ADVANCED_FACE ( 'NONE', ( #94838 ), #17300, .F. ) ;
#103214 = LINE ( 'NONE', #81507, #20636 ) ;
#103215 = LINE ( 'NONE', #58357, #69221 ) ;
#103216 = PLANE ( 'NONE',  #44471 ) ;
#103217 = EDGE_CURVE ( 'NONE', #36268, #116539, #141212, .T. ) ;
#103218 = ADVANCED_FACE ( 'NONE', ( #62984 ), #16571, .F. ) ;
#103219 = AXIS2_PLACEMENT_3D ( 'NONE', #100979, #43754, #100285 ) ;
#103220 = VERTEX_POINT ( 'NONE', #96962 ) ;
#103221 = CARTESIAN_POINT ( 'NONE',  ( -26.99999999999981171, 20.70535890316558891, 1.956823837851977332 ) ) ;
#103222 = EDGE_CURVE ( 'NONE', #72201, #24821, #95573, .T. ) ;
#103223 = DIRECTION ( 'NONE',  ( 0.000000000000000000, -1.000000000000000000, 0.000000000000000000 ) ) ;
#103224 = EDGE_CURVE ( 'NONE', #48074, #21068, #26352, .T. ) ;
#103225 = CARTESIAN_POINT ( 'NONE',  ( 50.66209685856478018, -5.291415217122919401, 3.054999999999998384 ) ) ;
#103226 = DIRECTION ( 'NONE',  ( 0.7071067811865487940, 0.7071067811865463515, 0.000000000000000000 ) ) ;
#103227 = FACE_OUTER_BOUND ( 'NONE', #17131, .T. ) ;
#103228 = VERTEX_POINT ( 'NONE', #105712 ) ;
#103230 = EDGE_CURVE ( 'NONE', #99775, #45656, #18705, .T. ) ;
#103229 = AXIS2_PLACEMENT_3D ( 'NONE', #120705, #63529, #42484 ) ;
#103231 = LINE ( 'NONE', #95749, #21076 ) ;
#103232 = ORIENTED_EDGE ( 'NONE', *, *, #129255, .T. ) ;
#103233 = CARTESIAN_POINT ( 'NONE',  ( 14.18753812416042948, -22.22500000000000142, 4.000000000000000000 ) ) ;
#103234 = CARTESIAN_POINT ( 'NONE',  ( 33.32816939922329880, 11.25929247661559529, 4.000000000000000000 ) ) ;
#103235 = DIRECTION ( 'NONE',  ( 0.3543493200069162685, -0.000000000000000000, -0.9351131265310288487 ) ) ;
#103236 = ADVANCED_FACE ( 'NONE', ( #105021 ), #47208, .T. ) ;
#103237 = DIRECTION ( 'NONE',  ( 0.7071067811865486830, -0.7071067811865464625, -0.000000000000000000 ) ) ;
#103238 = ADVANCED_FACE ( 'NONE', ( #39805 ), #119445, .T. ) ;
#103239 = DIRECTION ( 'NONE',  ( 0.6830127018922181881, 0.6830127018922202975, -0.2588190451025214056 ) ) ;
#103240 = CARTESIAN_POINT ( 'NONE',  ( 8.999999999999937828, -4.068876922607770119, 4.000000000000000000 ) ) ;
#103241 = EDGE_LOOP ( 'NONE', ( #19306, #104941, #34205, #119136 ) ) ;
#103242 = DIRECTION ( 'NONE',  ( -0.6830127018922180770, -0.6830127018922204085, -0.2588190451025213501 ) ) ;
#103243 = FACE_OUTER_BOUND ( 'NONE', #1113, .T. ) ;
#103244 = CARTESIAN_POINT ( 'NONE',  ( 29.67183060077625711, 2.259292476615694323, 4.000000000000000000 ) ) ;
#103245 = EDGE_CURVE ( 'NONE', #40200, #52853, #40244, .T. ) ;
#103246 = CONICAL_SURFACE ( 'NONE', #24498, 2.055000000000000604, 0.9599310885968764806 ) ;
#103247 = CARTESIAN_POINT ( 'NONE',  ( -34.42500000000001137, 11.97718569542929856, 5.000000000000000000 ) ) ;
#103248 = CARTESIAN_POINT ( 'NONE',  ( 72.55836038379624142, -7.949999999999997513, -2.130196079827425759 ) ) ;
#103249 = VECTOR ( 'NONE', #10372, 1000.000000000000000 ) ;
#103250 = CARTESIAN_POINT ( 'NONE',  ( 7.139999999999991687, -35.62921248010918873, -8.151379605006875195 ) ) ;
#103251 = ORIENTED_EDGE ( 'NONE', *, *, #136704, .T. ) ;
#103252 = ORIENTED_EDGE ( 'NONE', *, *, #130845, .T. ) ;
#103253 = CARTESIAN_POINT ( 'NONE',  ( 61.52083333333332149, 7.949999999999999289, 2.130196079827431532 ) ) ;
#103254 = DIRECTION ( 'NONE',  ( 0.7071067811865487940, -0.7071067811865463515, 0.000000000000000000 ) ) ;
#103255 = DIRECTION ( 'NONE',  ( 0.7071067811865487940, 0.7071067811865463515, -0.000000000000000000 ) ) ;
#103256 = DIRECTION ( 'NONE',  ( 2.173158128376833625E-16, -1.000000000000000000, 0.000000000000000000 ) ) ;
#103257 = VECTOR ( 'NONE', #96432, 1000.000000000000000 ) ;
#103258 = ORIENTED_EDGE ( 'NONE', *, *, #101343, .F. ) ;
#103259 = CARTESIAN_POINT ( 'NONE',  ( -24.18398860626899705, 28.73617430169804265, 5.000000000000000000 ) ) ;
#103260 = CARTESIAN_POINT ( 'NONE',  ( 10.94186803553636977, 3.821174125832445049E-16, 0.000000000000000000 ) ) ;
#103261 = CARTESIAN_POINT ( 'NONE',  ( 54.54209685856477563, 5.291415217122923842, -3.054999999999996163 ) ) ;
#103262 = EDGE_CURVE ( 'NONE', #99727, #125649, #67244, .T. ) ;
#103263 = LINE ( 'NONE', #48187, #110767 ) ;
#103264 = ORIENTED_EDGE ( 'NONE', *, *, #40569, .F. ) ;
#103265 = ORIENTED_EDGE ( 'NONE', *, *, #18485, .T. ) ;
#103266 = CARTESIAN_POINT ( 'NONE',  ( 25.82816939922335209, -17.24070752338409918, 4.000000000000000000 ) ) ;
#103267 = LINE ( 'NONE', #102590, #59216 ) ;
#103268 = DIRECTION ( 'NONE',  ( 0.7071067811865487940, 0.7071067811865463515, 0.000000000000000000 ) ) ;
#103269 = CARTESIAN_POINT ( 'NONE',  ( 17.99451991528748351, 28.92564299267950645, 4.000000000000000000 ) ) ;
#103270 = LINE ( 'NONE', #35921, #76373 ) ;
#103272 = ORIENTED_EDGE ( 'NONE', *, *, #47177, .T. ) ;
#103271 = DIRECTION ( 'NONE',  ( -0.000000000000000000, -0.3543493200069152693, 0.9351131265310292928 ) ) ;
#103273 = CARTESIAN_POINT ( 'NONE',  ( 21.18398860626899349, 28.73617430169802134, 5.000000000000000000 ) ) ;
#103274 = DIRECTION ( 'NONE',  ( -0.7071067811865486830, 0.7071067811865464625, 0.000000000000000000 ) ) ;
#103275 = DIRECTION ( 'NONE',  ( 0.000000000000000000, -1.000000000000000000, 0.000000000000000000 ) ) ;
#103276 = EDGE_CURVE ( 'NONE', #89141, #51035, #966, .T. ) ;
#103277 = VERTEX_POINT ( 'NONE', #121600 ) ;
#103278 = EDGE_LOOP ( 'NONE', ( #84636, #121496, #58118, #989 ) ) ;
#103279 = CARTESIAN_POINT ( 'NONE',  ( 11.81601139373100651, 28.73617430169779041, 5.000000000000000000 ) ) ;
#103280 = CARTESIAN_POINT ( 'NONE',  ( -7.628234450443801329, -8.240707523384200428, 11.38925528200754300 ) ) ;
#103281 = ADVANCED_FACE ( 'NONE', ( #141970 ), #45026, .F. ) ;
#103282 = FACE_OUTER_BOUND ( 'NONE', #119648, .T. ) ;
#103283 = DIRECTION ( 'NONE',  ( -0.6830127018922180770, -0.6830127018922204085, -0.2588190451025213501 ) ) ;
#103284 = ORIENTED_EDGE ( 'NONE', *, *, #107470, .T. ) ;
#103285 = ORIENTED_EDGE ( 'NONE', *, *, #88142, .T. ) ;
#103286 = VECTOR ( 'NONE', #73007, 1000.000000000000000 ) ;
#103287 = CARTESIAN_POINT ( 'NONE',  ( 4.499999999999972466, -10.53360074219763298, 5.000000000000000000 ) ) ;
#103288 = CARTESIAN_POINT ( 'NONE',  ( 50.99451991528749062, 28.92564299267973738, 4.000000000000000000 ) ) ;
#103289 = ORIENTED_EDGE ( 'NONE', *, *, #30964, .F. ) ;
#103290 = EDGE_CURVE ( 'NONE', #84395, #84525, #75279, .T. ) ;
#103291 = DIRECTION ( 'NONE',  ( 0.000000000000000000, 1.000000000000000000, 0.000000000000000000 ) ) ;
#103292 = ORIENTED_EDGE ( 'NONE', *, *, #1541, .T. ) ;
#103293 = DIRECTION ( 'NONE',  ( 0.000000000000000000, 1.000000000000000000, 0.000000000000000000 ) ) ;
#103295 = AXIS2_PLACEMENT_3D ( 'NONE', #104665, #60488, #6029 ) ;
#103294 = DIRECTION ( 'NONE',  ( 1.000000000000000000, 0.000000000000000000, 0.000000000000000000 ) ) ;
#103296 = ORIENTED_EDGE ( 'NONE', *, *, #62124, .T. ) ;
#103297 = EDGE_CURVE ( 'NONE', #28284, #78029, #65122, .T. ) ;
#103298 = FACE_BOUND ( 'NONE', #84886, .T. ) ;
#103299 = CARTESIAN_POINT ( 'NONE',  ( -27.48921356237309155, -27.52281430457074762, 5.000000000000000000 ) ) ;
#103300 = FACE_OUTER_BOUND ( 'NONE', #137260, .T. ) ;
#103301 = DIRECTION ( 'NONE',  ( 0.7071067811865487940, 0.7071067811865463515, 0.000000000000000000 ) ) ;
#103302 = DIRECTION ( 'NONE',  ( 9.352610917722648069E-17, 0.9242245927363030855, 0.3818493186865922207 ) ) ;
#103304 = VERTEX_POINT ( 'NONE', #120888 ) ;
#103303 = AXIS2_PLACEMENT_3D ( 'NONE', #51116, #37378, #127216 ) ;
#103305 = ORIENTED_EDGE ( 'NONE', *, *, #46163, .F. ) ;
#103306 = CARTESIAN_POINT ( 'NONE',  ( 91.05793019189812298, 6.110000000000000320, -1.637169565754156064 ) ) ;
#103307 = ORIENTED_EDGE ( 'NONE', *, *, #69726, .T. ) ;
#103308 = VECTOR ( 'NONE', #15037, 1000.000000000000000 ) ;
#103309 = CARTESIAN_POINT ( 'NONE',  ( 5.671830600776425868, -18.74070752338409207, 4.000000000000000000 ) ) ;
#103310 = CARTESIAN_POINT ( 'NONE',  ( -21.18398860626899349, 28.73617430169802134, 5.000000000000000000 ) ) ;
#103311 = SHAPE_REPRESENTATION ( '1.3 Jaw Plate', ( #127880 ), #137188 ) ;
#103312 = DIRECTION ( 'NONE',  ( 0.7071067811865487940, 0.7071067811865463515, 0.000000000000000000 ) ) ;
#103313 = EDGE_LOOP ( 'NONE', ( #45726, #1471, #134648, #143202 ) ) ;
#103314 = CARTESIAN_POINT ( 'NONE',  ( 33.32816939922331301, -21.74070752338405654, 4.000000000000000000 ) ) ;
#103315 = EDGE_CURVE ( 'NONE', #118046, #25524, #43352, .T. ) ;
#103316 = CARTESIAN_POINT ( 'NONE',  ( 25.40000000000004121, 7.384918846911211254, -2.931050874386697203 ) ) ;
#103318 = DIRECTION ( 'NONE',  ( -0.000000000000000000, -0.3543493200069152693, 0.9351131265310292928 ) ) ;
#103317 = CARTESIAN_POINT ( 'NONE',  ( -23.99451991528749062, 28.92564299267954908, 4.000000000000000000 ) ) ;
#103319 = FACE_OUTER_BOUND ( 'NONE', #119042, .T. ) ;
#103320 = CARTESIAN_POINT ( 'NONE',  ( 17.67183060077635304, 17.25929247661554200, 4.000000000000000000 ) ) ;
#103321 = VERTEX_POINT ( 'NONE', #9994 ) ;
#103322 = LINE ( 'NONE', #93186, #121327 ) ;
#103323 = LINE ( 'NONE', #3973, #37308 ) ;
#103324 = ORIENTED_EDGE ( 'NONE', *, *, #143075, .F. ) ;
#103325 = EDGE_CURVE ( 'NONE', #36965, #87041, #33226, .T. ) ;
#103327 = VERTEX_POINT ( 'NONE', #86861 ) ;
#103326 = VECTOR ( 'NONE', #106457, 999.9999999999998863 ) ;
#103328 = ADVANCED_FACE ( 'NONE', ( #12126 ), #78130, .T. ) ;
#103329 = ORIENTED_EDGE ( 'NONE', *, *, #128969, .T. ) ;
#103330 = CARTESIAN_POINT ( 'NONE',  ( 42.72959685856476142, -6.110000000000000320, -1.637169565754161393 ) ) ;
#103331 = EDGE_LOOP ( 'NONE', ( #78567, #12968, #60294, #5027 ) ) ;
#103332 = VECTOR ( 'NONE', #103973, 1000.000000000000000 ) ;
#103333 = AXIS2_PLACEMENT_3D ( 'NONE', #71241, #14697, #26295 ) ;
#103334 = AXIS2_PLACEMENT_3D ( 'NONE', #1894, #35326, #12097 ) ;
#103335 = CARTESIAN_POINT ( 'NONE',  ( 5.587472949537105826, -6.094999999999989981, 3.732111120401553285E-16 ) ) ;
#103336 = CARTESIAN_POINT ( 'NONE',  ( -14.16207406425801807, 5.380563507462931661, -29.22689065742943981 ) ) ;
#103337 = ORIENTED_EDGE ( 'NONE', *, *, #25353, .T. ) ;
#103338 = LINE ( 'NONE', #24375, #126654 ) ;
#103339 = VERTEX_POINT ( 'NONE', #87564 ) ;
#103340 = FACE_OUTER_BOUND ( 'NONE', #116436, .T. ) ;
#103341 = CIRCLE ( 'NONE', #89501, 5.968999999999998529 ) ;
#103342 = CARTESIAN_POINT ( 'NONE',  ( 34.92500000000001847, -3.269999999999991580, -36.39086428169088094 ) ) ;
#103344 = VERTEX_POINT ( 'NONE', #108553 ) ;
#103343 = LINE ( 'NONE', #23663, #58707 ) ;
#103345 = ORIENTED_EDGE ( 'NONE', *, *, #77404, .T. ) ;
#103346 = EDGE_CURVE ( 'NONE', #137915, #72729, #14848, .T. ) ;
#103347 = CARTESIAN_POINT ( 'NONE',  ( 0.000000000000000000, 0.000000000000000000, 5.000000000000000000 ) ) ;
#103348 = CARTESIAN_POINT ( 'NONE',  ( -6.299744871391586898, -27.71228299555210484, 4.000000000000000000 ) ) ;
#103349 = CARTESIAN_POINT ( 'NONE',  ( 127.0787635252314516, -7.482591942790327058E-16, 6.109999999999999432 ) ) ;
#103350 = VERTEX_POINT ( 'NONE', #133234 ) ;
#103351 = DIRECTION ( 'NONE',  ( -0.000000000000000000, -1.000000000000000000, -0.000000000000000000 ) ) ;
#103352 = VERTEX_POINT ( 'NONE', #56412 ) ;
#103353 = VERTEX_POINT ( 'NONE', #65858 ) ;
#103354 = ORIENTED_EDGE ( 'NONE', *, *, #85080, .T. ) ;
#103355 = ORIENTED_EDGE ( 'NONE', *, *, #122441, .F. ) ;
#103356 =( NAMED_UNIT ( * ) SI_UNIT ( $, .STERADIAN. ) SOLID_ANGLE_UNIT ( ) );
#103357 = DIRECTION ( 'NONE',  ( 0.7071067811865487940, -0.7071067811865463515, 0.000000000000000000 ) ) ;
#103358 = LINE ( 'NONE', #4008, #60190 ) ;
#103359 = DIRECTION ( 'NONE',  ( -0.000000000000000000, -0.3543493200069152693, 0.9351131265310292928 ) ) ;
#103360 = ORIENTED_EDGE ( 'NONE', *, *, #43739, .T. ) ;
#103361 = DIRECTION ( 'NONE',  ( -1.000000000000000000, -1.224606353822377258E-16, -0.000000000000000000 ) ) ;
#103362 = CARTESIAN_POINT ( 'NONE',  ( 22.58290314143522082, 3.967499999999992699, -6.871911579029513994 ) ) ;
#103363 = DIRECTION ( 'NONE',  ( 0.6830127018922180770, -0.6830127018922204085, -0.2588190451025213501 ) ) ;
#103364 = ADVANCED_FACE ( 'NONE', ( #110013 ), #89699, .F. ) ;
#103365 = VECTOR ( 'NONE', #85348, 999.9999999999998863 ) ;
#103366 = CARTESIAN_POINT ( 'NONE',  ( 0.000000000000000000, 0.000000000000000000, 5.000000000000000000 ) ) ;
#103367 = CARTESIAN_POINT ( 'NONE',  ( -34.92499999999996874, 22.27000000000001023, -8.436850734044138989 ) ) ;
#103368 = EDGE_LOOP ( 'NONE', ( #138274, #56595, #35287, #76216 ) ) ;
#103369 = EDGE_CURVE ( 'NONE', #66646, #17336, #44068, .T. ) ;
#103370 = VERTEX_POINT ( 'NONE', #132536 ) ;
#103371 = EDGE_LOOP ( 'NONE', ( #85942, #83752, #19385, #49203 ) ) ;
#103372 = FACE_OUTER_BOUND ( 'NONE', #108033, .T. ) ;
#103373 = CARTESIAN_POINT ( 'NONE',  ( 4.499999999999974243, 1.466399257802244893, 5.000000000000000000 ) ) ;
#103374 = PLANE ( 'NONE',  #47705 ) ;
#103375 = CIRCLE ( 'NONE', #29304, 2.500000000000000444 ) ;
#103376 = DIRECTION ( 'NONE',  ( 0.7071067811865486830, -0.7071067811865464625, -0.000000000000000000 ) ) ;
#103377 = DIRECTION ( 'NONE',  ( -0.7071067811865487940, 0.7071067811865463515, 0.000000000000000000 ) ) ;
#103378 = EDGE_CURVE ( 'NONE', #26153, #48148, #33911, .T. ) ;
#103380 = EDGE_CURVE ( 'NONE', #93894, #56990, #1237, .T. ) ;
#103379 = CARTESIAN_POINT ( 'NONE',  ( 8.372076165025809757, 8.651961987691654699, 3.925355617310125833 ) ) ;
#103381 = CARTESIAN_POINT ( 'NONE',  ( -41.99451991528749062, 28.92564299267967343, 4.000000000000000000 ) ) ;
#103382 = CARTESIAN_POINT ( 'NONE',  ( -5.999999999999954703, -21.03360074219752462, 5.000000000000000000 ) ) ;
#103383 = DIRECTION ( 'NONE',  ( -0.3543493200069162685, -0.000000000000000000, -0.9351131265310288487 ) ) ;
#103384 = CARTESIAN_POINT ( 'NONE',  ( -22.49999999999984723, -1.592773361805393417, -6.492772025301177585 ) ) ;
#103385 = DIRECTION ( 'NONE',  ( 1.000000000000000000, 0.000000000000000000, 0.000000000000000000 ) ) ;
#103386 = AXIS2_PLACEMENT_3D ( 'NONE', #142155, #140685, #108036 ) ;
#103387 = ORIENTED_EDGE ( 'NONE', *, *, #105834, .F. ) ;
#103388 = CARTESIAN_POINT ( 'NONE',  ( 16.82833281552586868, -0.2148806029953220509, -34.28722974112268673 ) ) ;
#103389 = ORIENTED_EDGE ( 'NONE', *, *, #98917, .F. ) ;
#103390 = DIRECTION ( 'NONE',  ( -0.6830127018922180770, -0.6830127018922204085, -0.2588190451025213501 ) ) ;
#103392 = ORIENTED_EDGE ( 'NONE', *, *, #53108, .F. ) ;
#103391 = CARTESIAN_POINT ( 'NONE',  ( 30.48921356237309510, -27.52281430457076894, 5.000000000000000000 ) ) ;
#103393 = EDGE_CURVE ( 'NONE', #99617, #55336, #89014, .T. ) ;
#103394 = AXIS2_PLACEMENT_3D ( 'NONE', #78372, #56662, #100825 ) ;
#103395 = EDGE_CURVE ( 'NONE', #63781, #31625, #18654, .T. ) ;
#103396 = CARTESIAN_POINT ( 'NONE',  ( -80.99451991528748351, 28.92564299267994699, 4.000000000000000000 ) ) ;
#103397 = DIRECTION ( 'NONE',  ( 0.7071067811865487940, 0.7071067811865463515, 0.000000000000000000 ) ) ;
#103398 = EDGE_LOOP ( 'NONE', ( #58515, #61465, #128961, #47063 ) ) ;
#103399 = DIRECTION ( 'NONE',  ( -0.000000000000000000, 0.3543493200069153248, 0.9351131265310292928 ) ) ;
#103400 = VERTEX_POINT ( 'NONE', #112188 ) ;
#103401 = CARTESIAN_POINT ( 'NONE',  ( -12.20000000000000462, -22.33999999999998565, 3.000000000000000000 ) ) ;
#103402 = ORIENTED_EDGE ( 'NONE', *, *, #20892, .T. ) ;
#103403 = CARTESIAN_POINT ( 'NONE',  ( -13.49999999999990408, -16.91253812416058722, 4.000000000000000000 ) ) ;
#103404 = EDGE_CURVE ( 'NONE', #103813, #52412, #69397, .T. ) ;
#103405 = PRESENTATION_LAYER_ASSIGNMENT (  '', '', ( #45615 ) ) ;
#103406 = CARTESIAN_POINT ( 'NONE',  ( 103.6208603837962272, -6.884901960086286188, 3.974999999999997424 ) ) ;
#103407 = DIRECTION ( 'NONE',  ( -0.6830127018922181881, 0.6830127018922202975, -0.2588190451025214056 ) ) ;
#103408 = DIRECTION ( 'NONE',  ( 0.7071067811865487940, -0.7071067811865463515, 0.000000000000000000 ) ) ;
#103409 = ORIENTED_EDGE ( 'NONE', *, *, #114762, .F. ) ;
#103410 =( GEOMETRIC_REPRESENTATION_CONTEXT ( 3 ) GLOBAL_UNCERTAINTY_ASSIGNED_CONTEXT ( ( #112703 ) ) GLOBAL_UNIT_ASSIGNED_CONTEXT ( ( #30024, #86583, #118466 ) ) REPRESENTATION_CONTEXT ( 'NONE', 'WORKASPACE' ) );
#103411 = CARTESIAN_POINT ( 'NONE',  ( -7.940000000000007496, -60.26999999999998892, -12.24789999999999957 ) ) ;
#103412 = LINE ( 'NONE', #123786, #132968 ) ;
#103413 = LINE ( 'NONE', #57111, #127173 ) ;
#103414 = CARTESIAN_POINT ( 'NONE',  ( 20.27083333333333570, 6.094999999999991758, 1.633150327867687102 ) ) ;
#103415 = CARTESIAN_POINT ( 'NONE',  ( 10.37159235450332062, 9.902892378096218942E-16, 0.000000000000000000 ) ) ;
#103416 = ADVANCED_FACE ( 'NONE', ( #114306 ), #13540, .F. ) ;
#103417 = CARTESIAN_POINT ( 'NONE',  ( -31.49999999999977973, -11.56887692260769640, 4.000000000000000000 ) ) ;
#103418 = VERTEX_POINT ( 'NONE', #78849 ) ;
#103419 = CYLINDRICAL_SURFACE ( 'NONE', #18875, 2.500000000000000000 ) ;
#103420 = EDGE_LOOP ( 'NONE', ( #64909, #70817, #11264, #97951 ) ) ;
#103421 = CARTESIAN_POINT ( 'NONE',  ( 97.41709685856478984, 3.054999999999998828, 5.291415217122922066 ) ) ;
#103422 = CARTESIAN_POINT ( 'NONE',  ( 7.358242975411349640, 15.75929247661555088, 19.34181609438697791 ) ) ;
#103423 = FACE_OUTER_BOUND ( 'NONE', #52183, .T. ) ;
#103424 = ADVANCED_FACE ( 'NONE', ( #3380 ), #36060, .F. ) ;
#103425 = CARTESIAN_POINT ( 'NONE',  ( 34.47516574401890921, 19.49051761211542910, 4.998110765256835286 ) ) ;
#103426 = DIRECTION ( 'NONE',  ( 1.000000000000000000, 0.000000000000000000, -0.000000000000000000 ) ) ;
#103427 = EDGE_LOOP ( 'NONE', ( #102246, #136279, #132279, #10333, #135431, #76006, #83259, #140281 ) ) ;
#103428 = LINE ( 'NONE', #48358, #35018 ) ;
#103429 = DIRECTION ( 'NONE',  ( 0.7071067811865487940, -0.7071067811865463515, 0.000000000000000000 ) ) ;
#103430 = VECTOR ( 'NONE', #70007, 1000.000000000000000 ) ;
#103431 = ORIENTED_EDGE ( 'NONE', *, *, #140576, .T. ) ;
#103432 = FACE_OUTER_BOUND ( 'NONE', #51473, .T. ) ;
#103433 = LINE ( 'NONE', #49822, #70319 ) ;
#103436 = EDGE_CURVE ( 'NONE', #22222, #65695, #90414, .T. ) ;
#103435 = EDGE_LOOP ( 'NONE', ( #8389, #79014, #47026, #53198 ) ) ;
#103434 = CARTESIAN_POINT ( 'NONE',  ( -12.69999999999999929, -59.76999999999998892, -39.50000000000000000 ) ) ;
#103437 = DIRECTION ( 'NONE',  ( 0.7071067811865487940, -0.7071067811865463515, 0.000000000000000000 ) ) ;
#103438 = DIRECTION ( 'NONE',  ( -0.000000000000000000, 0.3543493200069153248, 0.9351131265310292928 ) ) ;
#103439 = DIRECTION ( 'NONE',  ( -0.000000000000000000, 0.000000000000000000, 1.000000000000000000 ) ) ;
#103440 = VECTOR ( 'NONE', #75862, 1000.000000000000000 ) ;
#103441 =( NAMED_UNIT ( * ) PLANE_ANGLE_UNIT ( ) SI_UNIT ( $, .RADIAN. ) );
#103442 = CIRCLE ( 'NONE', #73377, 2.055000000000001048 ) ;
#103443 = ORIENTED_EDGE ( 'NONE', *, *, #104357, .F. ) ;
#103444 = ADVANCED_FACE ( 'NONE', ( #70834 ), #135381, .F. ) ;
#103445 = ORIENTED_EDGE ( 'NONE', *, *, #28891, .F. ) ;
#103446 = ORIENTED_EDGE ( 'NONE', *, *, #119971, .T. ) ;
#103447 = VECTOR ( 'NONE', #73158, 1000.000000000000000 ) ;
#103448 = CARTESIAN_POINT ( 'NONE',  ( 81.81293019189810423, -1.637169565754159617, -6.110000000000001208 ) ) ;
#103449 = ORIENTED_EDGE ( 'NONE', *, *, #110691, .F. ) ;
#103450 = DIRECTION ( 'NONE',  ( 0.000000000000000000, 0.000000000000000000, 1.000000000000000000 ) ) ;
#103451 = AXIS2_PLACEMENT_3D ( 'NONE', #8548, #54287, #110039 ) ;
#103452 = DIRECTION ( 'NONE',  ( -0.7071067811865486830, -0.7071067811865464625, -0.000000000000000000 ) ) ;
#103454 = AXIS2_PLACEMENT_3D ( 'NONE', #74799, #84249, #116839 ) ;
#103453 = LINE ( 'NONE', #82448, #135960 ) ;
#103455 = DIRECTION ( 'NONE',  ( -1.000000000000000000, 0.000000000000000000, 0.000000000000000000 ) ) ;
#103456 = VERTEX_POINT ( 'NONE', #23732 ) ;
#103457 = CARTESIAN_POINT ( 'NONE',  ( 102.9375000000000000, 5.819803920172574863, -5.819803920172573086 ) ) ;
#103458 = LINE ( 'NONE', #47020, #134724 ) ;
#103459 = CARTESIAN_POINT ( 'NONE',  ( 74.14126352523146579, 4.472830434245836706, 4.472830434245840259 ) ) ;
#103460 = VERTEX_POINT ( 'NONE', #35354 ) ;
#103461 = CARTESIAN_POINT ( 'NONE',  ( 11.99999999999992184, 10.55218569542905982, 5.000000000000000000 ) ) ;
#103462 = LINE ( 'NONE', #117186, #73376 ) ;
#103463 = DIRECTION ( 'NONE',  ( -0.7071067811865486830, 0.7071067811865464625, 0.000000000000000000 ) ) ;
#103464 = VERTEX_POINT ( 'NONE', #80982 ) ;
#103465 = ORIENTED_EDGE ( 'NONE', *, *, #47312, .T. ) ;
#103466 = CARTESIAN_POINT ( 'NONE',  ( 64.14583333333332860, 2.130196079827431976, -7.949999999999998401 ) ) ;
#103467 = SURFACE_STYLE_USAGE ( .BOTH. , #25939 ) ;
#103468 = CARTESIAN_POINT ( 'NONE',  ( 22.08790314143522338, 6.871911579029515771, 3.967499999999989146 ) ) ;
#103469 = CARTESIAN_POINT ( 'NONE',  ( 21.29159235450332233, 9.902892378096218942E-16, 0.000000000000000000 ) ) ;
#103470 = AXIS2_PLACEMENT_3D ( 'NONE', #77012, #142944, #81 ) ;
#103471 = DIRECTION ( 'NONE',  ( 0.7071067811865487940, 0.7071067811865463515, 0.000000000000000000 ) ) ;
#103472 = DIRECTION ( 'NONE',  ( -0.7071067811865486830, 0.7071067811865464625, 0.000000000000000000 ) ) ;
#103473 = VECTOR ( 'NONE', #959, 1000.000000000000000 ) ;
#103474 = ORIENTED_EDGE ( 'NONE', *, *, #113531, .F. ) ;
#103475 =( BOUNDED_SURFACE ( )  B_SPLINE_SURFACE ( 3, 2, ( 
 ( #40280, #37395, #3983 ),
 ( #48262, #117071, #17748 ),
 ( #59865, #17071, #104784 ),
 ( #26517, #6143, #39555 ),
 ( #81640, #51135, #38825 ),
 ( #92457, #103336, #6856 ),
 ( #27939, #4697, #115614 ),
 ( #136691, #48995, #114908 ),
 ( #15586, #27212, #138139 ),
 ( #137431, #28677, #82341 ),
 ( #16318, #50420, #84486 ),
 ( #71455, #93901, #70068 ),
 ( #60611, #126525, #5444 ),
 ( #49726, #62023, #83041 ),
 ( #127239, #61334, #106179 ),
 ( #114233, #94606, #59183 ),
 ( #138861, #83782, #54010 ),
 ( #64870, #108312, #19900 ),
 ( #8291, #109051, #32230 ),
 ( #96039, #40965, #107629 ),
 ( #63465, #9741, #42418 ),
 ( #120634, #98890, #143124 ),
 ( #65614, #30823, #43819 ),
 ( #88037, #8984, #119218 ),
 ( #52541, #64151, #31517 ),
 ( #74318, #98205, #109782 ),
 ( #142432, #96723, #75049 ),
 ( #53244, #140276, #85884 ),
 ( #75741, #43118, #41671 ),
 ( #97461, #29351, #141713 ),
 ( #140966, #87328, #130122 ),
 ( #131541, #86630, #130853 ),
 ( #129379, #76465, #119911 ),
 ( #20615, #85163, #21351 ),
 ( #10450, #54710, #73596 ),
 ( #30067, #117763, #18453 ),
 ( #106915, #62736, #7594 ),
 ( #51854, #118508, #19207 ),
 ( #66298, #111188, #110471 ),
 ( #33679, #89454, #56878 ),
 ( #11875, #46732, #11141 ),
 ( #3150, #113333, #133689 ),
 ( #34372, #12603, #132287 ),
 ( #78592, #88771, #56164 ),
 ( #122801, #135143, #100348 ),
 ( #101758, #13301, #23483 ) ),
 .UNSPECIFIED., .F., .F., .F. ) 
 B_SPLINE_SURFACE_WITH_KNOTS ( ( 4, 2, 2, 2, 2, 2, 2, 2, 2, 2, 2, 2, 2, 2, 2, 2, 2, 2, 2, 2, 2, 2, 4 ),
 ( 3, 3 ),
 ( 2.602085213965210642E-18, 0.003250134860695850971, 0.006500269721391699340, 0.008125337151739624175, 0.009750404582087547276, 0.01300053944278339521, 0.01462560687313131831, 0.01625067430347924141, 0.01950080916417509108, 0.02112587659452301592, 0.02275094402487094075, 0.02600107888556678695, 0.02762614631591470832, 0.02925121374626263315, 0.03250134860695848282, 0.03412641603730640766, 0.03575148346765433249, 0.03900161832835018216, 0.04225175318904603183, 0.04550188804974188150, 0.04712695548008980634, 0.04875202291043773117, 0.05200215777113357390 ),
 ( 0.000000000000000000, 1.000000000000000000 ),
 .UNSPECIFIED. ) 
 GEOMETRIC_REPRESENTATION_ITEM ( )  RATIONAL_B_SPLINE_SURFACE ( (
 ( 1.000000000000000000, 0.7366656399173064917, 1.000000000000000000),
 ( 1.000000000000000000, 0.7439429771432026772, 1.000000000000000000),
 ( 1.000000000000000000, 0.7520594078564465379, 1.000000000000000000),
 ( 1.000000000000000000, 0.7692526947351095989, 1.000000000000000000),
 ( 1.000000000000000000, 0.7783293130759435519, 1.000000000000000000),
 ( 1.000000000000000000, 0.7922221006548060274, 1.000000000000000000),
 ( 1.000000000000000000, 0.7969161081511108025, 1.000000000000000000),
 ( 1.000000000000000000, 0.8061991495951973397, 1.000000000000000000),
 ( 1.000000000000000000, 0.8107995347775716066, 1.000000000000000000),
 ( 1.000000000000000000, 0.8243916883358404224, 1.000000000000000000),
 ( 1.000000000000000000, 0.8331742881454423655, 1.000000000000000000),
 ( 1.000000000000000000, 0.8456175635000574564, 1.000000000000000000),
 ( 1.000000000000000000, 0.8496437749331391398, 1.000000000000000000),
 ( 1.000000000000000000, 0.8573989149376710639, 1.000000000000000000),
 ( 1.000000000000000000, 0.8610920168694898846, 1.000000000000000000),
 ( 1.000000000000000000, 0.8715094877776208282, 1.000000000000000000),
 ( 1.000000000000000000, 0.8775986680032793474, 1.000000000000000000),
 ( 1.000000000000000000, 0.8851898980576022868, 1.000000000000000000),
 ( 1.000000000000000000, 0.8874625043875524755, 1.000000000000000000),
 ( 1.000000000000000000, 0.8914353813151855155, 1.000000000000000000),
 ( 1.000000000000000000, 0.8931046208065658298, 1.000000000000000000),
 ( 1.000000000000000000, 0.8971318440585478449, 1.000000000000000000),
 ( 1.000000000000000000, 0.8985209499677152545, 1.000000000000000000),
 ( 1.000000000000000000, 0.8985769579961769837, 1.000000000000000000),
 ( 1.000000000000000000, 0.8982569968411678873, 1.000000000000000000),
 ( 1.000000000000000000, 0.8969164612184702401, 1.000000000000000000),
 ( 1.000000000000000000, 0.8959054417035888784, 1.000000000000000000),
 ( 1.000000000000000000, 0.8919262031741450603, 1.000000000000000000),
 ( 1.000000000000000000, 0.8880110869415998032, 1.000000000000000000),
 ( 1.000000000000000000, 0.8804381194099686336, 1.000000000000000000),
 ( 1.000000000000000000, 0.8776206763866101213, 1.000000000000000000),
 ( 1.000000000000000000, 0.8715502808905819521, 1.000000000000000000),
 ( 1.000000000000000000, 0.8682884511766901792, 1.000000000000000000),
 ( 1.000000000000000000, 0.8578980603305481623, 1.000000000000000000),
 ( 1.000000000000000000, 0.8501653997698138676, 1.000000000000000000),
 ( 1.000000000000000000, 0.8334322383353173214, 1.000000000000000000),
 ( 1.000000000000000000, 0.8246054523620813814, 1.000000000000000000),
 ( 1.000000000000000000, 0.8064801979543902988, 1.000000000000000000),
 ( 1.000000000000000000, 0.7971768814008325377, 1.000000000000000000),
 ( 1.000000000000000000, 0.7832300806951568717, 1.000000000000000000),
 ( 1.000000000000000000, 0.7785857309249303304, 1.000000000000000000),
 ( 1.000000000000000000, 0.7695076527920222675, 1.000000000000000000),
 ( 1.000000000000000000, 0.7650571017203612323, 1.000000000000000000),
 ( 1.000000000000000000, 0.7520869309904180122, 1.000000000000000000),
 ( 1.000000000000000000, 0.7439459459532327124, 1.000000000000000000),
 ( 1.000000000000000000, 0.7366656399173067138, 1.000000000000000000) ) ) 
 REPRESENTATION_ITEM ( '' )  SURFACE ( )  );
#103476 = ORIENTED_EDGE ( 'NONE', *, *, #43913, .F. ) ;
#103477 = CARTESIAN_POINT ( 'NONE',  ( 20.67183060077632462, -15.74070752338412760, 4.000000000000000000 ) ) ;
#103478 = ORIENTED_EDGE ( 'NONE', *, *, #127783, .F. ) ;
#103479 = EDGE_CURVE ( 'NONE', #113815, #20046, #103412, .T. ) ;
#103480 = VECTOR ( 'NONE', #134704, 1000.000000000000227 ) ;
#103481 = LINE ( 'NONE', #56490, #61311 ) ;
#103482 = ORIENTED_EDGE ( 'NONE', *, *, #101302, .F. ) ;
#103483 = CARTESIAN_POINT ( 'NONE',  ( 69.64169371712954160, -2.130196079827424871, -7.949999999999998401 ) ) ;
#103484 = CARTESIAN_POINT ( 'NONE',  ( 7.139999999999992575, -35.13237070076360169, 17.62370837922859934 ) ) ;
#103485 = VECTOR ( 'NONE', #124655, 1000.000000000000000 ) ;
#103486 = CARTESIAN_POINT ( 'NONE',  ( 0.2997448713915885632, -27.71228299555206220, 4.000000000000000000 ) ) ;
#103487 = FACE_OUTER_BOUND ( 'NONE', #85657, .T. ) ;
#103488 = ORIENTED_EDGE ( 'NONE', *, *, #135022, .F. ) ;
#103489 = DIRECTION ( 'NONE',  ( 1.000000000000000000, 0.000000000000000000, 0.000000000000000000 ) ) ;
#103490 = FACE_OUTER_BOUND ( 'NONE', #64161, .T. ) ;
#103492 = ORIENTED_EDGE ( 'NONE', *, *, #32301, .F. ) ;
#103491 = VECTOR ( 'NONE', #17888, 1000.000000000000000 ) ;
#103493 = ADVANCED_FACE ( 'NONE', ( #12833 ), #57109, .T. ) ;
#103494 = CARTESIAN_POINT ( 'NONE',  ( 2.999999999999976463, 10.55218569542906160, 5.000000000000000000 ) ) ;
#103495 = ORIENTED_EDGE ( 'NONE', *, *, #77486, .T. ) ;
#103496 = EDGE_LOOP ( 'NONE', ( #47221, #129411, #95528, #119519 ) ) ;
#103498 = EDGE_CURVE ( 'NONE', #41303, #119060, #79601, .T. ) ;
#103497 = LINE ( 'NONE', #126681, #78327 ) ;
#103499 = EDGE_LOOP ( 'NONE', ( #139634, #100830, #126229, #53977 ) ) ;
#103500 = ORIENTED_EDGE ( 'NONE', *, *, #66831, .F. ) ;
#103501 = CARTESIAN_POINT ( 'NONE',  ( 71.45876352523143282, 0.000000000000000000, -6.110000000000001208 ) ) ;
#103502 = ORIENTED_EDGE ( 'NONE', *, *, #39621, .F. ) ;
#103503 = CARTESIAN_POINT ( 'NONE',  ( -20.99999999999985789, -16.60178936734450872, 0.8616154019347020965 ) ) ;
#103504 = CARTESIAN_POINT ( 'NONE',  ( 21.47336096364202263, -5.240707523384221744, 16.25846745537500482 ) ) ;
#103505 = VECTOR ( 'NONE', #27008, 1000.000000000000000 ) ;
#103506 = CARTESIAN_POINT ( 'NONE',  ( 117.6879301918981042, 6.110000000000002984, -1.637169565754156730 ) ) ;
#103507 = DIRECTION ( 'NONE',  ( 0.3543493200069162685, -0.000000000000000000, -0.9351131265310288487 ) ) ;
#103508 = ADVANCED_FACE ( 'NONE', ( #14279 ), #58564, .F. ) ;
#103509 = CARTESIAN_POINT ( 'NONE',  ( 18.48921356237309510, -27.52281430457068367, 5.000000000000000000 ) ) ;
#103510 = CARTESIAN_POINT ( 'NONE',  ( -34.92500000000001137, 21.72500000000000142, 4.165035510187084178 ) ) ;
#103511 = CARTESIAN_POINT ( 'NONE',  ( 0.000000000000000000, 0.000000000000000000, 0.000000000000000000 ) ) ;
#103512 = LINE ( 'NONE', #69509, #44726 ) ;
#103513 = EDGE_CURVE ( 'NONE', #139146, #37315, #91834, .T. ) ;
#103514 = LINE ( 'NONE', #62192, #49124 ) ;
#103515 = VERTEX_POINT ( 'NONE', #51026 ) ;
#103516 = LINE ( 'NONE', #48448, #10998 ) ;
#103517 = PLANE ( 'NONE',  #33757 ) ;
#103518 = EDGE_LOOP ( 'NONE', ( #32177, #98363, #85266, #71829 ) ) ;
#103519 = ORIENTED_EDGE ( 'NONE', *, *, #22386, .F. ) ;
#103520 = DIRECTION ( 'NONE',  ( 0.000000000000000000, 0.000000000000000000, 1.000000000000000000 ) ) ;
#103521 = EDGE_CURVE ( 'NONE', #69963, #68778, #25873, .T. ) ;
#103522 = VERTEX_POINT ( 'NONE', #37483 ) ;
#103523 = CARTESIAN_POINT ( 'NONE',  ( 13.49999999999991473, -8.947814304570734123, 5.000000000000000000 ) ) ;
#103524 = DIRECTION ( 'NONE',  ( -0.6830127018922181881, 0.6830127018922202975, -0.2588190451025214056 ) ) ;
#103525 = VECTOR ( 'NONE', #88356, 999.9999999999998863 ) ;
#103526 = DIRECTION ( 'NONE',  ( 1.000000000000000000, 0.000000000000000000, 0.000000000000000000 ) ) ;
#103527 = DIRECTION ( 'NONE',  ( -0.000000000000000000, 0.000000000000000000, 1.000000000000000000 ) ) ;
#103528 = ORIENTED_EDGE ( 'NONE', *, *, #114506, .F. ) ;
#103529 = LINE ( 'NONE', #60813, #58117 ) ;
#103530 = ORIENTED_EDGE ( 'NONE', *, *, #37728, .F. ) ;
#103531 = AXIS2_PLACEMENT_3D ( 'NONE', #28631, #72883, #51088 ) ;
#103533 = DIRECTION ( 'NONE',  ( 0.6830127018922181881, 0.6830127018922202975, -0.2588190451025214056 ) ) ;
#103532 = VECTOR ( 'NONE', #81786, 1000.000000000000000 ) ;
#103534 =( BOUNDED_CURVE ( )  B_SPLINE_CURVE ( 3, ( #17691, #4629, #138074, #38761 ),
 .UNSPECIFIED., .F., .T. ) 
 B_SPLINE_CURVE_WITH_KNOTS ( ( 4, 4 ),
 ( 5.106027341939283204, 6.645403452391245303 ),
 .UNSPECIFIED. ) 
 CURVE ( )  GEOMETRIC_REPRESENTATION_ITEM ( )  RATIONAL_B_SPLINE_CURVE ( ( 1.000000000000000000, 0.8120851936182283959, 0.8120851936182283959, 1.000000000000000000 ) ) 
 REPRESENTATION_ITEM ( '' )  );
#103535 = CARTESIAN_POINT ( 'NONE',  ( 26.17123647476855908, 0.000000000000000000, 7.934999999999990727 ) ) ;
#103536 = CARTESIAN_POINT ( 'NONE',  ( 8.510786437626906675, -27.52281430457049183, 5.000000000000000000 ) ) ;
#103537 = CARTESIAN_POINT ( 'NONE',  ( 26.99451991528749417, 28.92564299267956685, 4.000000000000000000 ) ) ;
#103538 = EDGE_LOOP ( 'NONE', ( #99054, #84144, #113654, #61616, #473 ) ) ;
#103539 = EDGE_CURVE ( 'NONE', #28845, #103024, #4058, .T. ) ;
#103540 = ORIENTED_EDGE ( 'NONE', *, *, #16279, .T. ) ;
#103541 = ORIENTED_EDGE ( 'NONE', *, *, #116679, .F. ) ;
#103542 = CARTESIAN_POINT ( 'NONE',  ( -7.940000000000001279, -35.14999999999999147, -8.101350000000007157 ) ) ;
#103543 = CARTESIAN_POINT ( 'NONE',  ( 11.18753812416045434, -22.22500000000000142, 4.000000000000000000 ) ) ;
#103544 = VECTOR ( 'NONE', #138610, 1000.000000000000000 ) ;
#103545 = LINE ( 'NONE', #115120, #109890 ) ;
#103546 = SURFACE_STYLE_USAGE ( .BOTH. , #125335 ) ;
#103547 = ORIENTED_EDGE ( 'NONE', *, *, #94149, .T. ) ;
#103548 = CARTESIAN_POINT ( 'NONE',  ( 25.40000000000000568, -6.088644610809077484, -0.2782657062331916342 ) ) ;
#103549 = EDGE_CURVE ( 'NONE', #37816, #53397, #26592, .T. ) ;
#103550 = EDGE_CURVE ( 'NONE', #135328, #138961, #133925, .T. ) ;
#103551 = DIRECTION ( 'NONE',  ( 0.000000000000000000, -1.000000000000000000, 0.000000000000000000 ) ) ;
#103552 = CARTESIAN_POINT ( 'NONE',  ( 42.48921356237308800, -27.52281430457085065, 5.000000000000000000 ) ) ;
#103553 = CARTESIAN_POINT ( 'NONE',  ( -12.31657961132782297, -6.740707523384216415, 11.88629033278126990 ) ) ;
#103554 = LINE ( 'NONE', #4191, #88231 ) ;
#103555 = CARTESIAN_POINT ( 'NONE',  ( -31.36246187583881806, 22.22499999999999432, 4.000000000000000000 ) ) ;
#103556 = EDGE_LOOP ( 'NONE', ( #8867, #27753, #78857, #129903 ) ) ;
#103557 = CARTESIAN_POINT ( 'NONE',  ( 66.18398860626901126, 28.73617430169833753, 5.000000000000000000 ) ) ;
#103559 = EDGE_CURVE ( 'NONE', #11154, #106829, #32120, .T. ) ;
#103558 = DIRECTION ( 'NONE',  ( 0.7071067811865487940, 0.7071067811865463515, 0.000000000000000000 ) ) ;
#103560 = VERTEX_POINT ( 'NONE', #130007 ) ;
#103562 = VERTEX_POINT ( 'NONE', #75635 ) ;
#103561 = LINE ( 'NONE', #57983, #13896 ) ;
#103564 = ORIENTED_EDGE ( 'NONE', *, *, #40447, .F. ) ;
#103563 = ADVANCED_FACE ( 'NONE', ( #119809 ), #19801, .F. ) ;
#103565 = EDGE_CURVE ( 'NONE', #61782, #67530, #64042, .T. ) ;
#103566 = LINE ( 'NONE', #76320, #107032 ) ;
#103567 = CARTESIAN_POINT ( 'NONE',  ( 23.32000000000000028, 9.521314400968980422E-16, 0.000000000000000000 ) ) ;
#103569 = VECTOR ( 'NONE', #2576, 999.9999999999998863 ) ;
#103568 = CARTESIAN_POINT ( 'NONE',  ( -57.48921356237308800, -27.52281430457095368, 5.000000000000000000 ) ) ;
#103570 = ORIENTED_EDGE ( 'NONE', *, *, #110163, .F. ) ;
#103571 = DIRECTION ( 'NONE',  ( 0.6830127018922180770, 0.6830127018922202975, -0.2588190451025213501 ) ) ;
#103572 = ORIENTED_EDGE ( 'NONE', *, *, #1376, .F. ) ;
#103573 = CARTESIAN_POINT ( 'NONE',  ( 4.499999999999966249, -19.91253812416055169, 4.000000000000000000 ) ) ;
#103574 = CYLINDRICAL_SURFACE ( 'NONE', #20799, 2.500000000000000000 ) ;
#103575 = CARTESIAN_POINT ( 'NONE',  ( 128.7041937171295842, -6.884901960086285300, -3.975000000000000089 ) ) ;
#103576 = EDGE_CURVE ( 'NONE', #126581, #57666, #84389, .T. ) ;
#103577 = AXIS2_PLACEMENT_3D ( 'NONE', #122456, #45665, #44226 ) ;
#103578 = LINE ( 'NONE', #15822, #94827 ) ;
#103579 = ADVANCED_FACE ( 'NONE', ( #40179 ), #97341, .T. ) ;
#103580 = CARTESIAN_POINT ( 'NONE',  ( 13.26601651615776767, 1.700382741644379081, 5.000000000000000000 ) ) ;
#103581 = CARTESIAN_POINT ( 'NONE',  ( 20.20710678118641113, -14.24070752338413826, 5.000000000000000000 ) ) ;
#103582 = FACE_OUTER_BOUND ( 'NONE', #63005, .T. ) ;
#103583 =( NAMED_UNIT ( * ) PLANE_ANGLE_UNIT ( ) SI_UNIT ( $, .RADIAN. ) );
#103584 = CARTESIAN_POINT ( 'NONE',  ( 31.18706980810189222, -2.126176841940956130, 7.934999999999991616 ) ) ;
#103586 = VECTOR ( 'NONE', #109894, 1000.000000000000000 ) ;
#103585 = DIRECTION ( 'NONE',  ( -1.000000000000000000, -1.224606353822377258E-16, -0.000000000000000000 ) ) ;
#103587 = ADVANCED_FACE ( 'NONE', ( #128579 ), #109676, .F. ) ;
#103588 = DIRECTION ( 'NONE',  ( -0.000000000000000000, 0.3543493200069153248, 0.9351131265310292928 ) ) ;
#103589 = CARTESIAN_POINT ( 'NONE',  ( 0.000000000000000000, 0.000000000000000000, 5.000000000000000000 ) ) ;
#103590 = ORIENTED_EDGE ( 'NONE', *, *, #33044, .F. ) ;
#103591 = ORIENTED_EDGE ( 'NONE', *, *, #89907, .F. ) ;
#103592 = CARTESIAN_POINT ( 'NONE',  ( 88.35416666666665719, -2.130196079827425315, -7.950000000000001066 ) ) ;
#103593 = ORIENTED_EDGE ( 'NONE', *, *, #105038, .F. ) ;
#103594 = EDGE_LOOP ( 'NONE', ( #130459, #1133, #143208, #95974 ) ) ;
#103595 = LINE ( 'NONE', #84045, #71935 ) ;
#103596 = DIRECTION ( 'NONE',  ( -0.7071067811865486830, -0.7071067811865464625, 0.000000000000000000 ) ) ;
#103597 = ORIENTED_EDGE ( 'NONE', *, *, #77744, .T. ) ;
#103598 = LINE ( 'NONE', #28920, #113490 ) ;
#103599 = LINE ( 'NONE', #113789, #99647 ) ;
#103600 = CARTESIAN_POINT ( 'NONE',  ( 151.4000000000000057, -16.48000000000005016, 12.69999999999954632 ) ) ;
#103601 = DIRECTION ( 'NONE',  ( -1.000000000000000000, -0.000000000000000000, -0.000000000000000000 ) ) ;
#103602 = DIRECTION ( 'NONE',  ( -0.6830127018922181881, 0.6830127018922202975, -0.2588190451025214056 ) ) ;
#103603 = PLANE ( 'NONE',  #109857 ) ;
#103604 = DIRECTION ( 'NONE',  ( 0.7071067811865487940, -0.7071067811865463515, 0.000000000000000000 ) ) ;
#103605 = LINE ( 'NONE', #115898, #105417 ) ;
#103606 = DIRECTION ( 'NONE',  ( 0.3543493200069162685, -0.000000000000000000, -0.9351131265310288487 ) ) ;
#103607 = CARTESIAN_POINT ( 'NONE',  ( 13.60986171580761805, 4.202752102959690472E-16, 0.000000000000000000 ) ) ;
#103608 = DIRECTION ( 'NONE',  ( -0.7071067811865487940, 0.7071067811865463515, 0.000000000000000000 ) ) ;
#103609 = CARTESIAN_POINT ( 'NONE',  ( 15.48921356237309510, -27.52281430457066236, 5.000000000000000000 ) ) ;
#103610 = EDGE_CURVE ( 'NONE', #128178, #25861, #120514, .T. ) ;
#103611 = EDGE_CURVE ( 'NONE', #23390, #40720, #74940, .T. ) ;
#103612 = ORIENTED_EDGE ( 'NONE', *, *, #122637, .T. ) ;
#103613 = VERTEX_POINT ( 'NONE', #142330 ) ;
#103614 = CARTESIAN_POINT ( 'NONE',  ( 110.1045968585647756, 1.637169565754164946, -6.109999999999999432 ) ) ;
#103615 = AXIS2_PLACEMENT_3D ( 'NONE', #78746, #112785, #23639 ) ;
#103616 = ORIENTED_EDGE ( 'NONE', *, *, #69478, .F. ) ;
#103617 = CARTESIAN_POINT ( 'NONE',  ( -12.18398860626900060, 28.73617430169795739, 5.000000000000000000 ) ) ;
#103618 = DIRECTION ( 'NONE',  ( -0.7071067811865486830, -0.7071067811865464625, 0.000000000000000000 ) ) ;
#103619 = VERTEX_POINT ( 'NONE', #19097 ) ;
#103620 = EDGE_CURVE ( 'NONE', #8752, #103200, #73497, .T. ) ;
#103621 = CARTESIAN_POINT ( 'NONE',  ( -12.48921356237309155, -27.52281430457064104, 5.000000000000000000 ) ) ;
#103622 = LINE ( 'NONE', #56633, #111386 ) ;
#103623 = CIRCLE ( 'NONE', #10992, 2.500000000000000888 ) ;
#103624 = CARTESIAN_POINT ( 'NONE',  ( 101.1204301918981230, 3.055000000000001936, -5.291415217122916737 ) ) ;
#103625 = ORIENTED_EDGE ( 'NONE', *, *, #87183, .T. ) ;
#103626 = ORIENTED_EDGE ( 'NONE', *, *, #129595, .T. ) ;
#103627 = CARTESIAN_POINT ( 'NONE',  ( 15.49238828748955576, 4.584330080086930965E-16, 0.000000000000000000 ) ) ;
#103628 = DIRECTION ( 'NONE',  ( -0.6830127018922181881, 0.6830127018922202975, -0.2588190451025214056 ) ) ;
#103629 = STYLED_ITEM ( 'NONE', ( #56889 ), #125580 ) ;
#103630 = ORIENTED_EDGE ( 'NONE', *, *, #140594, .F. ) ;
#103631 = VERTEX_POINT ( 'NONE', #41553 ) ;
#103632 = AXIS2_PLACEMENT_3D ( 'NONE', #125805, #1813, #59150 ) ;
#103633 = ORIENTED_EDGE ( 'NONE', *, *, #15910, .F. ) ;
#103634 = CARTESIAN_POINT ( 'NONE',  ( -24.64327148205084583, 5.259292476615665457, 4.831541298974430632 ) ) ;
#103635 = CARTESIAN_POINT ( 'NONE',  ( 3.129569808101886341, -3.967499999999998028, -6.871911579029511330 ) ) ;
#103636 = VECTOR ( 'NONE', #20310, 1000.000000000000000 ) ;
#103637 = STYLED_ITEM ( 'NONE', ( #16864 ), #137549 ) ;
#103638 = ORIENTED_EDGE ( 'NONE', *, *, #86915, .F. ) ;
#103639 = ORIENTED_EDGE ( 'NONE', *, *, #17682, .F. ) ;
#103640 = DIRECTION ( 'NONE',  ( -0.7071067811865487940, 0.7071067811865463515, -0.000000000000000000 ) ) ;
#103641 = ORIENTED_EDGE ( 'NONE', *, *, #23155, .F. ) ;
#103642 = EDGE_LOOP ( 'NONE', ( #19959, #127629, #33567 ) ) ;
#103643 = CARTESIAN_POINT ( 'NONE',  ( 4.408325480989981671, -0.7407075233842770334, 14.76736230305381703 ) ) ;
#103644 = CARTESIAN_POINT ( 'NONE',  ( 26.67183060077628198, -0.7407075233842665973, 4.000000000000000000 ) ) ;
#103645 = ORIENTED_EDGE ( 'NONE', *, *, #76104, .F. ) ;
#103646 = CARTESIAN_POINT ( 'NONE',  ( 69.48921356237309510, -27.52281430457103895, 5.000000000000000000 ) ) ;
#103647 = DIRECTION ( 'NONE',  ( 0.7071067811865487940, 0.7071067811865463515, 0.000000000000000000 ) ) ;
#103648 = PRESENTATION_STYLE_ASSIGNMENT (( #25390 ) ) ;
#103649 = EDGE_CURVE ( 'NONE', #138500, #83589, #62623, .T. ) ;
#103650 = CARTESIAN_POINT ( 'NONE',  ( -8.999999999999941380, 1.931123077392167264, 4.000000000000000000 ) ) ;
#103651 = FACE_BOUND ( 'NONE', #141283, .T. ) ;
#103652 = ORIENTED_EDGE ( 'NONE', *, *, #31891, .T. ) ;
#103653 = CARTESIAN_POINT ( 'NONE',  ( 25.19159235450331735, -3.851859888774471706E-31, 2.500000000000001332 ) ) ;
#103654 = EDGE_CURVE ( 'NONE', #123427, #41026, #140177, .T. ) ;
#103655 = DIRECTION ( 'NONE',  ( -0.6830127018922181881, 0.6830127018922202975, -0.2588190451025214056 ) ) ;
#103656 = FILL_AREA_STYLE ('',( #83378 ) ) ;
#103657 = ORIENTED_EDGE ( 'NONE', *, *, #89284, .T. ) ;
#103658 = LINE ( 'NONE', #113848, #59808 ) ;
#103659 = VERTEX_POINT ( 'NONE', #130744 ) ;
#103660 = CIRCLE ( 'NONE', #43574, 2.500000000000000444 ) ;
#103661 = ORIENTED_EDGE ( 'NONE', *, *, #133245, .T. ) ;
#103662 = VERTEX_POINT ( 'NONE', #8189 ) ;
#103663 = ADVANCED_FACE ( 'NONE', ( #52429 ), #117661, .F. ) ;
#103664 = EDGE_CURVE ( 'NONE', #98656, #133910, #131442, .T. ) ;
#103665 = CARTESIAN_POINT ( 'NONE',  ( 35.49543019189811588, 5.291415217122916737, 3.055000000000001936 ) ) ;
#103666 = VERTEX_POINT ( 'NONE', #108209 ) ;
#103667 = PLANE ( 'NONE',  #13641 ) ;
#103668 = CARTESIAN_POINT ( 'NONE',  ( 0.000000000000000000, 0.000000000000000000, 5.000000000000000000 ) ) ;
#103669 = FACE_OUTER_BOUND ( 'NONE', #104058, .T. ) ;
#103670 = EDGE_CURVE ( 'NONE', #120796, #9583, #63183, .T. ) ;
#103671 = VERTEX_POINT ( 'NONE', #133587 ) ;
#103672 = DIRECTION ( 'NONE',  ( 0.000000000000000000, -1.286409696682840916E-16, 1.000000000000000000 ) ) ;
#103673 = CARTESIAN_POINT ( 'NONE',  ( -9.299744871391588674, -27.71228299555212971, 4.000000000000000000 ) ) ;
#103674 = EDGE_CURVE ( 'NONE', #113044, #42047, #88662, .T. ) ;
#103675 = CARTESIAN_POINT ( 'NONE',  ( 0.000000000000000000, 0.000000000000000000, 5.000000000000000000 ) ) ;
#103676 = FACE_OUTER_BOUND ( 'NONE', #138652, .T. ) ;
#103677 = LINE ( 'NONE', #136330, #4244 ) ;
#103678 = LINE ( 'NONE', #16697, #81828 ) ;
#103679 = EDGE_LOOP ( 'NONE', ( #44454, #42947, #36026, #81055, #121127, #113489, #6513, #99719, #115976, #40121 ) ) ;
#103680 = ORIENTED_EDGE ( 'NONE', *, *, #57280, .F. ) ;
#103681 = EDGE_LOOP ( 'NONE', ( #65998, #6912, #662, #114881, #77544, #122191, #125424, #111586 ) ) ;
#103682 = EDGE_LOOP ( 'NONE', ( #65631, #92994, #34622, #29278 ) ) ;
#103683 = FACE_OUTER_BOUND ( 'NONE', #83929, .T. ) ;
#103684 = ADVANCED_FACE ( 'NONE', ( #66193 ), #12495, .F. ) ;
#103685 = ORIENTED_EDGE ( 'NONE', *, *, #85773, .F. ) ;
#103686 = ORIENTED_EDGE ( 'NONE', *, *, #14020, .T. ) ;
#103687 = CARTESIAN_POINT ( 'NONE',  ( 33.48921356237309510, -27.52281430457078670, 5.000000000000000000 ) ) ;
#103688 = LINE ( 'NONE', #61672, #8649 ) ;
#103689 = CARTESIAN_POINT ( 'NONE',  ( 6.654944837453786732, 5.259292476615669010, 12.77922209995895209 ) ) ;
#103690 = VECTOR ( 'NONE', #97615, 1000.000000000000227 ) ;
#103691 = LINE ( 'NONE', #81285, #53229 ) ;
#103692 = ORIENTED_EDGE ( 'NONE', *, *, #43017, .F. ) ;
#103693 = CARTESIAN_POINT ( 'NONE',  ( 9.279999999999999361, -2.055000000000000160, 0.000000000000000000 ) ) ;
#103694 = EDGE_CURVE ( 'NONE', #19810, #7159, #35735, .T. ) ;
#103695 = VERTEX_POINT ( 'NONE', #69053 ) ;
#103696 = DIRECTION ( 'NONE',  ( 0.000000000000000000, 0.000000000000000000, -1.000000000000000000 ) ) ;
#103697 = CARTESIAN_POINT ( 'NONE',  ( -1.828169399223509517, 12.75929247661558819, 4.000000000000000000 ) ) ;
#103698 = CARTESIAN_POINT ( 'NONE',  ( -1.391263525231447584, -5.808823158059033709, 5.808823158059035485 ) ) ;
#103699 = VERTEX_POINT ( 'NONE', #87923 ) ;
#103701 = CARTESIAN_POINT ( 'NONE',  ( -19.49999999999986500, -8.568876922607721269, 4.000000000000000000 ) ) ;
#103700 = CARTESIAN_POINT ( 'NONE',  ( 97.32876352523145158, 0.000000000000000000, -6.109999999999999432 ) ) ;
#103702 = PLANE ( 'NONE',  #90625 ) ;
#103703 = DIRECTION ( 'NONE',  ( -0.000000000000000000, -0.3543493200069152693, 0.9351131265310292928 ) ) ;
#103704 = ORIENTED_EDGE ( 'NONE', *, *, #138269, .T. ) ;
#103705 = EDGE_CURVE ( 'NONE', #46538, #18761, #77084, .T. ) ;
#103706 = ORIENTED_EDGE ( 'NONE', *, *, #99829, .T. ) ;
#103707 = DIRECTION ( 'NONE',  ( -0.7071067811865487940, 0.7071067811865463515, -0.000000000000000000 ) ) ;
#103708 = ORIENTED_EDGE ( 'NONE', *, *, #79207, .F. ) ;
#103709 = PLANE ( 'NONE',  #69520 ) ;
#103710 = PLANE ( 'NONE',  #99674 ) ;
#103711 = CARTESIAN_POINT ( 'NONE',  ( 1.179999999999999716, 6.391994993740215847, 6.750000000000000888 ) ) ;
#103712 = DIRECTION ( 'NONE',  ( 0.7071067811865487940, -0.7071067811865463515, 0.000000000000000000 ) ) ;
#103713 = DIRECTION ( 'NONE',  ( 0.6830127018922181881, 0.6830127018922202975, -0.2588190451025214056 ) ) ;
#103714 = CARTESIAN_POINT ( 'NONE',  ( 180.4193221990229574, -49.14999999999999147, -40.92499999999998295 ) ) ;
#103715 = ORIENTED_EDGE ( 'NONE', *, *, #56477, .F. ) ;
#103716 = EDGE_CURVE ( 'NONE', #43122, #32117, #135041, .T. ) ;
#103717 = DIRECTION ( 'NONE',  ( 0.7071067811865487940, 0.7071067811865463515, -0.000000000000000000 ) ) ;
#103718 = EDGE_CURVE ( 'NONE', #48874, #39354, #43709, .T. ) ;
#103719 = PLANE ( 'NONE',  #67336 ) ;
#103720 = CARTESIAN_POINT ( 'NONE',  ( 12.69999999999999574, -59.76999999999998892, 24.34531699603382293 ) ) ;
#103721 = ORIENTED_EDGE ( 'NONE', *, *, #34340, .T. ) ;
#103722 = CARTESIAN_POINT ( 'NONE',  ( -33.18398860626899705, 28.73617430169810305, 5.000000000000000000 ) ) ;
#103723 = AXIS2_PLACEMENT_3D ( 'NONE', #72410, #104981, #15782 ) ;
#103725 = EDGE_CURVE ( 'NONE', #50807, #132555, #13192, .T. ) ;
#103724 = DIRECTION ( 'NONE',  ( -1.000000000000000000, -0.000000000000000000, -0.000000000000000000 ) ) ;
#103726 = ORIENTED_EDGE ( 'NONE', *, *, #100053, .F. ) ;
#103727 = VECTOR ( 'NONE', #27901, 1000.000000000000000 ) ;
#103729 = VERTEX_POINT ( 'NONE', #132168 ) ;
#103728 = DIRECTION ( 'NONE',  ( 0.000000000000000000, -1.000000000000000000, 0.000000000000000000 ) ) ;
#103730 = ORIENTED_EDGE ( 'NONE', *, *, #96770, .T. ) ;
#103731 = CARTESIAN_POINT ( 'NONE',  ( 5.068407645496677105, 9.139736423841732040E-16, 0.000000000000000000 ) ) ;
#103732 = LINE ( 'NONE', #61029, #94647 ) ;
#103733 = VECTOR ( 'NONE', #94058, 999.9999999999998863 ) ;
#103734 = EDGE_LOOP ( 'NONE', ( #3032, #38562, #93363, #108320 ) ) ;
#103735 = CARTESIAN_POINT ( 'NONE',  ( 15.20840764549667767, -3.851859888774471706E-31, 2.500000000000001332 ) ) ;
#103736 = VECTOR ( 'NONE', #133320, 1000.000000000000000 ) ;
#103737 = CARTESIAN_POINT ( 'NONE',  ( 5.510786437626906675, -27.52281430457051314, 5.000000000000000000 ) ) ;
#103738 = DIRECTION ( 'NONE',  ( 0.7071067811865487940, 0.7071067811865463515, -0.000000000000000000 ) ) ;
#103739 = ORIENTED_EDGE ( 'NONE', *, *, #94860, .T. ) ;
#103740 = ADVANCED_FACE ( 'NONE', ( #54603 ), #68361, .T. ) ;
#103741 = CARTESIAN_POINT ( 'NONE',  ( 14.67183060077638324, 20.25929247661552779, 4.000000000000000000 ) ) ;
#103742 = CARTESIAN_POINT ( 'NONE',  ( 42.29974487139158157, -27.71228299555235708, 4.000000000000000000 ) ) ;
#103743 = CARTESIAN_POINT ( 'NONE',  ( 36.29974487139159578, -27.71228299555231445, 4.000000000000000000 ) ) ;
#103744 = DIRECTION ( 'NONE',  ( -1.000000000000000000, 1.248002500702738701E-15, -3.404785525682857987E-16 ) ) ;
#103745 = CARTESIAN_POINT ( 'NONE',  ( 60.29974487139158867, -27.71228299555248142, 4.000000000000000000 ) ) ;
#103746 = CARTESIAN_POINT ( 'NONE',  ( 15.49238828748955576, 0.000000000000000000, 2.500000000000000444 ) ) ;
#103747 = EDGE_CURVE ( 'NONE', #143089, #97576, #21948, .T. ) ;
#103748 = CARTESIAN_POINT ( 'NONE',  ( 28.22502705046288440, 5.819803920172573974, -5.819803920172573086 ) ) ;
#103749 = DIRECTION ( 'NONE',  ( -0.7071067811865486830, -0.7071067811865464625, 0.000000000000000000 ) ) ;
#103750 = EDGE_LOOP ( 'NONE', ( #119316, #130752, #109616 ) ) ;
#103751 = VERTEX_POINT ( 'NONE', #57469 ) ;
#103752 = ORIENTED_EDGE ( 'NONE', *, *, #41882, .T. ) ;
#103753 = CARTESIAN_POINT ( 'NONE',  ( 121.1666666666666714, 6.884901960086285300, 3.975000000000003642 ) ) ;
#103754 = VERTEX_POINT ( 'NONE', #112534 ) ;
#103755 = VERTEX_POINT ( 'NONE', #55314 ) ;
#103756 = VERTEX_POINT ( 'NONE', #34267 ) ;
#103757 =( LENGTH_UNIT ( ) NAMED_UNIT ( * ) SI_UNIT ( .MILLI., .METRE. ) );
#103758 = AXIS2_PLACEMENT_3D ( 'NONE', #100757, #89864, #91332 ) ;
#103759 = CARTESIAN_POINT ( 'NONE',  ( -17.99451991528748351, 28.92564299267950645, 4.000000000000000000 ) ) ;
#103760 = ORIENTED_EDGE ( 'NONE', *, *, #114029, .F. ) ;
#103761 =( BOUNDED_CURVE ( )  B_SPLINE_CURVE ( 2, ( #138616, #39308, #58966, #71953, #83530, #116845, #127742, #49494, #113997, #26282, #82121, #116124, #14685 ),
 .UNSPECIFIED., .F., .T. ) 
 B_SPLINE_CURVE_WITH_KNOTS ( ( 3, 2, 2, 2, 2, 2, 3 ),
 ( 0.5999999999999999778, 0.6027777777777777457, 0.6055555555555555136, 0.6083333333333332815, 0.6111111111111111605, 0.6138888888888889284, 0.6166666666666666963 ),
 .UNSPECIFIED. ) 
 CURVE ( )  GEOMETRIC_REPRESENTATION_ITEM ( )  RATIONAL_B_SPLINE_CURVE ( ( 1.000000000000000000, 0.9659258262890683122, 1.000000000000000000, 0.9659258262890683122, 1.000000000000000000, 0.9659258262890683122, 1.000000000000000000, 0.9659258262890683122, 1.000000000000000000, 0.9659258262890683122, 1.000000000000000000, 0.9659258262890683122, 1.000000000000000000 ) ) 
 REPRESENTATION_ITEM ( '' )  );
#103762 = CARTESIAN_POINT ( 'NONE',  ( 24.48921356237309510, -27.52281430457072631, 5.000000000000000000 ) ) ;
#103763 = VECTOR ( 'NONE', #26735, 1000.000000000000114 ) ;
#103764 = CARTESIAN_POINT ( 'NONE',  ( 15.00548008471250228, 28.92564299267927552, 4.000000000000000000 ) ) ;
#103765 = DIRECTION ( 'NONE',  ( 1.000000000000000000, 0.000000000000000000, 0.000000000000000000 ) ) ;
#103766 = CARTESIAN_POINT ( 'NONE',  ( 108.7920968585647756, -5.291415217122921177, 3.054999999999999272 ) ) ;
#103767 = ORIENTED_EDGE ( 'NONE', *, *, #87166, .T. ) ;
#103768 = CARTESIAN_POINT ( 'NONE',  ( -5.098242758349162962, 11.83526629088845361, -27.40386350861210119 ) ) ;
#103769 = CARTESIAN_POINT ( 'NONE',  ( -25.49999999999982236, 15.43112307739203182, 4.000000000000000000 ) ) ;
#103770 = CARTESIAN_POINT ( 'NONE',  ( -30.70701326429283640, -21.74070752338405654, 4.999753212805224223 ) ) ;
#103771 = CARTESIAN_POINT ( 'NONE',  ( 82.62086038379624142, -6.884901960086286188, 3.974999999999997424 ) ) ;
#103772 =( NAMED_UNIT ( * ) SI_UNIT ( $, .STERADIAN. ) SOLID_ANGLE_UNIT ( ) );
#103773 = CARTESIAN_POINT ( 'NONE',  ( 17.58838509405156358, 22.22499999999999787, 4.777194822843813249 ) ) ;
#103774 = DIRECTION ( 'NONE',  ( 0.7071067811865486830, -0.7071067811865464625, -0.000000000000000000 ) ) ;
#103775 = CARTESIAN_POINT ( 'NONE',  ( 34.49586038379622011, -3.974999999999998312, -6.884901960086286188 ) ) ;
#103776 = DIRECTION ( 'NONE',  ( 0.7071067811865487940, -0.7071067811865463515, 0.000000000000000000 ) ) ;
#103777 = EDGE_CURVE ( 'NONE', #63299, #46769, #22630, .T. ) ;
#103778 = LINE ( 'NONE', #137884, #71603 ) ;
#103779 = EDGE_LOOP ( 'NONE', ( #79138, #23105, #41915, #57939, #4095 ) ) ;
#103780 = VERTEX_POINT ( 'NONE', #891 ) ;
#103781 = CARTESIAN_POINT ( 'NONE',  ( 33.81249999999999289, 5.819803920172571310, 5.819803920172575751 ) ) ;
#103782 = ORIENTED_EDGE ( 'NONE', *, *, #135199, .T. ) ;
#103783 = ORIENTED_EDGE ( 'NONE', *, *, #63946, .F. ) ;
#103784 = LINE ( 'NONE', #25526, #129336 ) ;
#103785 = LINE ( 'NONE', #82106, #47876 ) ;
#103786 = ORIENTED_EDGE ( 'NONE', *, *, #139305, .F. ) ;
#103787 = VECTOR ( 'NONE', #4313, 1000.000000000000000 ) ;
#103788 = CARTESIAN_POINT ( 'NONE',  ( 1.499999999999993561, 18.05218569542898521, 5.000000000000000000 ) ) ;
#103790 = AXIS2_PLACEMENT_3D ( 'NONE', #43163, #121407, #21401 ) ;
#103789 = FACE_OUTER_BOUND ( 'NONE', #98668, .T. ) ;
#103791 = DIRECTION ( 'NONE',  ( -0.7071067811865486830, -0.7071067811865464625, -0.000000000000000000 ) ) ;
#103792 = CARTESIAN_POINT ( 'NONE',  ( 28.29209685856476497, -5.291415217122921177, 3.054999999999999272 ) ) ;
#103793 = ORIENTED_EDGE ( 'NONE', *, *, #28449, .T. ) ;
#103794 = CARTESIAN_POINT ( 'NONE',  ( -25.17183060077629975, 6.759292476615647693, 4.000000000000000000 ) ) ;
#103795 = EDGE_LOOP ( 'NONE', ( #82409, #44933, #89686, #33121 ) ) ;
#103796 = DIRECTION ( 'NONE',  ( 0.000000000000000000, 0.000000000000000000, 1.000000000000000000 ) ) ;
#103797 = CARTESIAN_POINT ( 'NONE',  ( 2.207106781186528810, 15.75929247661555443, 5.000000000000000000 ) ) ;
#103798 = DIRECTION ( 'NONE',  ( 0.6830127018922180770, -0.6830127018922204085, -0.2588190451025213501 ) ) ;
#103799 = DIRECTION ( 'NONE',  ( 0.000000000000000000, 0.000000000000000000, -1.000000000000000000 ) ) ;
#103800 = ORIENTED_EDGE ( 'NONE', *, *, #94203, .T. ) ;
#103801 = ORIENTED_EDGE ( 'NONE', *, *, #4699, .T. ) ;
#103802 = CARTESIAN_POINT ( 'NONE',  ( 0.000000000000000000, 0.000000000000000000, 0.000000000000000000 ) ) ;
#103803 = CARTESIAN_POINT ( 'NONE',  ( 34.92460739249803225, 21.74787736706806029, 4.224371856075157972 ) ) ;
#103804 = LINE ( 'NONE', #48757, #138035 ) ;
#103805 = DIRECTION ( 'NONE',  ( -0.7071067811865487940, 0.7071067811865463515, 0.000000000000000000 ) ) ;
#103806 = CARTESIAN_POINT ( 'NONE',  ( 51.53709685856478018, -3.054999999999998828, -5.291415217122919401 ) ) ;
#103807 = ORIENTED_EDGE ( 'NONE', *, *, #108419, .T. ) ;
#103808 = DIRECTION ( 'NONE',  ( 0.000000000000000000, 0.000000000000000000, 1.000000000000000000 ) ) ;
#103809 = DIRECTION ( 'NONE',  ( 0.6830127018922180770, -0.6830127018922204085, -0.2588190451025213501 ) ) ;
#103810 = ORIENTED_EDGE ( 'NONE', *, *, #109471, .F. ) ;
#103811 = ORIENTED_EDGE ( 'NONE', *, *, #57502, .T. ) ;
#103812 = FACE_OUTER_BOUND ( 'NONE', #80432, .T. ) ;
#103813 = VERTEX_POINT ( 'NONE', #89355 ) ;
#103814 = PLANE ( 'NONE',  #72031 ) ;
#103815 = VERTEX_POINT ( 'NONE', #101651 ) ;
#103816 = PLANE ( 'NONE',  #30690 ) ;
#103817 = ADVANCED_FACE ( 'NONE', ( #160 ), #78488, .F. ) ;
#103818 = VECTOR ( 'NONE', #113482, 1000.000000000000000 ) ;
#103819 = VECTOR ( 'NONE', #7965, 1000.000000000000227 ) ;
#103820 = CIRCLE ( 'NONE', #13593, 2.500000000000000444 ) ;
#103821 = DIRECTION ( 'NONE',  ( 0.7071067811865486830, -0.7071067811865464625, -0.000000000000000000 ) ) ;
#103822 = STYLED_ITEM ( 'NONE', ( #99366 ), #113202 ) ;
#103823 = FACE_BOUND ( 'NONE', #141028, .T. ) ;
#103824 = LINE ( 'NONE', #116163, #8581 ) ;
#103825 = EDGE_CURVE ( 'NONE', #90791, #120068, #67641, .T. ) ;
#103826 = ADVANCED_FACE ( 'NONE', ( #46626 ), #134303, .F. ) ;
#103827 = CARTESIAN_POINT ( 'NONE',  ( -15.64318742751728841, -20.24070752338407075, 21.22881796311208902 ) ) ;
#103829 = ORIENTED_EDGE ( 'NONE', *, *, #70615, .T. ) ;
#103828 = CARTESIAN_POINT ( 'NONE',  ( 8.750000000000000000, -7.464222240803106570E-16, -6.094999999999989981 ) ) ;
#103830 = VECTOR ( 'NONE', #104410, 1000.000000000000000 ) ;
#103831 = VECTOR ( 'NONE', #38692, 1000.000000000000000 ) ;
#103832 = FACE_OUTER_BOUND ( 'NONE', #68153, .T. ) ;
#103833 = ORIENTED_EDGE ( 'NONE', *, *, #49089, .F. ) ;
#103834 = EDGE_CURVE ( 'NONE', #132228, #32191, #3048, .T. ) ;
#103835 = EDGE_CURVE ( 'NONE', #79341, #120024, #16789, .T. ) ;
#103836 = VERTEX_POINT ( 'NONE', #136418 ) ;
#103837 = CARTESIAN_POINT ( 'NONE',  ( 66.41209685856478018, 5.291415217122921177, -3.054999999999994831 ) ) ;
#103838 = ORIENTED_EDGE ( 'NONE', *, *, #101227, .T. ) ;
#103839 = CARTESIAN_POINT ( 'NONE',  ( -11.91685193227062101, 21.75929247661549581, 7.311836541448024640 ) ) ;
#103840 = PLANE ( 'NONE',  #65795 ) ;
#103841 = EDGE_CURVE ( 'NONE', #67478, #91367, #15327, .T. ) ;
#103842 = ORIENTED_EDGE ( 'NONE', *, *, #34574, .F. ) ;
#103843 = DIRECTION ( 'NONE',  ( -0.5150380749100710309, 0.000000000000000000, 0.8571673007021021196 ) ) ;
#103844 = VECTOR ( 'NONE', #5311, 1000.000000000000227 ) ;
#103845 = EDGE_CURVE ( 'NONE', #108755, #141993, #104506, .T. ) ;
#103846 = EDGE_CURVE ( 'NONE', #99982, #64348, #82091, .T. ) ;
#103847 = CARTESIAN_POINT ( 'NONE',  ( -21.16809626817622103, 8.755558144015518351, 4.000000000000000000 ) ) ;
#103848 = DIRECTION ( 'NONE',  ( -0.000000000000000000, 0.000000000000000000, 1.000000000000000000 ) ) ;
#103849 = FACE_OUTER_BOUND ( 'NONE', #87819, .T. ) ;
#103850 = CARTESIAN_POINT ( 'NONE',  ( 0.000000000000000000, 9.735942053221458872E-16, -7.950000000000000178 ) ) ;
#103851 = LINE ( 'NONE', #72009, #138851 ) ;
#103852 = VERTEX_POINT ( 'NONE', #26251 ) ;
#103853 = AXIS2_PLACEMENT_3D ( 'NONE', #1569, #58182, #101628 ) ;
#103854 = ORIENTED_EDGE ( 'NONE', *, *, #39678, .F. ) ;
#103855 = CIRCLE ( 'NONE', #111114, 2.055000000000000604 ) ;
#103856 = CARTESIAN_POINT ( 'NONE',  ( 14.54487008052911534, -0.7407075233842805861, 4.335043535661647240 ) ) ;
#103857 = DIRECTION ( 'NONE',  ( -0.7071067811865487940, 0.7071067811865463515, 0.000000000000000000 ) ) ;
#103858 = VERTEX_POINT ( 'NONE', #4411 ) ;
#103859 = AXIS2_PLACEMENT_3D ( 'NONE', #117829, #6910, #19267 ) ;
#103860 = EDGE_CURVE ( 'NONE', #43087, #115095, #3728, .T. ) ;
#103861 = EDGE_LOOP ( 'NONE', ( #112024, #112652, #60104, #22298 ) ) ;
#103862 = AXIS2_PLACEMENT_3D ( 'NONE', #143463, #134040, #23847 ) ;
#103863 = VERTEX_POINT ( 'NONE', #126964 ) ;
#103864 = DIRECTION ( 'NONE',  ( -0.000000000000000000, -0.000000000000000000, 1.000000000000000000 ) ) ;
#103865 = CARTESIAN_POINT ( 'NONE',  ( 29.72916666666665009, 7.950000000000001954, -2.130196079827421762 ) ) ;
#103866 = VERTEX_POINT ( 'NONE', #38551 ) ;
#103867 = VECTOR ( 'NONE', #1406, 1000.000000000000227 ) ;
#103868 = CARTESIAN_POINT ( 'NONE',  ( -8.277185695429338352, -21.72500000000000142, 5.000000000000000000 ) ) ;
#103869 = EDGE_CURVE ( 'NONE', #89522, #1245, #47343, .T. ) ;
#103870 = STYLED_ITEM ( 'NONE', ( #63786 ), #56651 ) ;
#103871 = DIRECTION ( 'NONE',  ( 0.6830127018922180770, -0.6830127018922204085, -0.2588190451025213501 ) ) ;
#103872 = CARTESIAN_POINT ( 'NONE',  ( 8.962903141435219823, -3.967499999999994476, 6.871911579029513106 ) ) ;
#103873 = PLANE ( 'NONE',  #132938 ) ;
#103874 = VERTEX_POINT ( 'NONE', #28395 ) ;
#103875 = FACE_OUTER_BOUND ( 'NONE', #22780, .T. ) ;
#103876 = CARTESIAN_POINT ( 'NONE',  ( 7.799999601179139042, 3.821174125832445049E-16, 0.000000000000000000 ) ) ;
#103877 = EDGE_CURVE ( 'NONE', #98193, #9777, #115344, .T. ) ;
#103878 = CARTESIAN_POINT ( 'NONE',  ( 25.22916666666666785, -6.094999999999989093, 1.633150327867691542 ) ) ;
#103879 = VECTOR ( 'NONE', #77907, 1000.000000000000227 ) ;
#103881 = ORIENTED_EDGE ( 'NONE', *, *, #104943, .T. ) ;
#103880 = DIRECTION ( 'NONE',  ( -0.000000000000000000, 0.3543493200069153248, 0.9351131265310292928 ) ) ;
#103882 = DIRECTION ( 'NONE',  ( 0.3543493200069162685, -0.000000000000000000, -0.9351131265310288487 ) ) ;
#103883 = VERTEX_POINT ( 'NONE', #127712 ) ;
#103884 = DIRECTION ( 'NONE',  ( 1.000000000000000000, 0.000000000000000000, 0.000000000000000000 ) ) ;
#103885 = LINE ( 'NONE', #27061, #56177 ) ;
#103886 = CARTESIAN_POINT ( 'NONE',  ( 107.7500000000000000, -9.735942053221458872E-16, 7.950000000000000178 ) ) ;
#103887 = ORIENTED_EDGE ( 'NONE', *, *, #66793, .T. ) ;
#103888 = LINE ( 'NONE', #4532, #38969 ) ;
#103889 = EDGE_CURVE ( 'NONE', #49004, #71242, #92190, .T. ) ;
#103890 = EDGE_CURVE ( 'NONE', #56792, #61837, #25511, .T. ) ;
#103891 = CARTESIAN_POINT ( 'NONE',  ( -24.48921356237309510, -27.52281430457072631, 5.000000000000000000 ) ) ;
#103892 = DIRECTION ( 'NONE',  ( -1.000000000000000000, -0.000000000000000000, -0.000000000000000000 ) ) ;
#103893 = CARTESIAN_POINT ( 'NONE',  ( -42.18398860626899705, 28.73617430169816700, 5.000000000000000000 ) ) ;
#103894 = ORIENTED_EDGE ( 'NONE', *, *, #14709, .F. ) ;
#103895 = CARTESIAN_POINT ( 'NONE',  ( -32.99999999999976552, -15.41253812416059787, 4.000000000000000000 ) ) ;
#103896 = CARTESIAN_POINT ( 'NONE',  ( 34.92499999999998295, -20.24070752338406720, 4.255531930566162302 ) ) ;
#103897 = EDGE_CURVE ( 'NONE', #117130, #84461, #53854, .T. ) ;
#103899 = EDGE_CURVE ( 'NONE', #131176, #83686, #69787, .T. ) ;
#103898 = CARTESIAN_POINT ( 'NONE',  ( 7.920806282870441528, 3.047499999999997655, 5.278424836066143655 ) ) ;
#103900 = CARTESIAN_POINT ( 'NONE',  ( -22.49999999999983302, 16.08746187583907528, 4.000000000000000000 ) ) ;
#103901 = FACE_OUTER_BOUND ( 'NONE', #108470, .T. ) ;
#103902 = ORIENTED_EDGE ( 'NONE', *, *, #41705, .T. ) ;
#103903 = ORIENTED_EDGE ( 'NONE', *, *, #37538, .F. ) ;
#103904 = DIRECTION ( 'NONE',  ( -0.7071067811865487940, 0.7071067811865463515, 0.000000000000000000 ) ) ;
#103905 = FILL_AREA_STYLE ('',( #59744 ) ) ;
#103906 = CARTESIAN_POINT ( 'NONE',  ( 1.582903141435219485, 3.967499999999992699, -6.871911579029513994 ) ) ;
#103907 = CARTESIAN_POINT ( 'NONE',  ( 38.35681257248239007, -20.24070752338406365, 21.22881796311221336 ) ) ;
#103908 = LINE ( 'NONE', #4557, #64633 ) ;
#103909 = DIRECTION ( 'NONE',  ( -0.7071067811865487940, 0.7071067811865463515, -0.000000000000000000 ) ) ;
#103910 = CARTESIAN_POINT ( 'NONE',  ( 43.53752705046289151, -9.735942053221456900E-16, 7.949999999999998401 ) ) ;
#103911 = ORIENTED_EDGE ( 'NONE', *, *, #112719, .F. ) ;
#103912 = ADVANCED_FACE ( 'NONE', ( #58931 ), #37111, .T. ) ;
#103913 = DIRECTION ( 'NONE',  ( -0.6830127018922181881, 0.6830127018922202975, -0.2588190451025214056 ) ) ;
#103914 = FACE_OUTER_BOUND ( 'NONE', #108325, .T. ) ;
#103915 = LINE ( 'NONE', #90211, #117644 ) ;
#103916 = CARTESIAN_POINT ( 'NONE',  ( 45.26626352523144448, 4.472830434245839371, -4.472830434245839371 ) ) ;
#103917 = ORIENTED_EDGE ( 'NONE', *, *, #140298, .F. ) ;
#103918 = SURFACE_SIDE_STYLE ('',( #69948 ) ) ;
#103919 = EDGE_CURVE ( 'NONE', #84037, #10400, #116092, .T. ) ;
#103920 = ORIENTED_EDGE ( 'NONE', *, *, #64758, .F. ) ;
#103921 = LINE ( 'NONE', #136568, #32701 ) ;
#103922 = ORIENTED_EDGE ( 'NONE', *, *, #107053, .F. ) ;
#103923 = PRESENTATION_LAYER_ASSIGNMENT (  '', '', ( #101672 ) ) ;
#103924 = CARTESIAN_POINT ( 'NONE',  ( -20.81601139373100295, 28.73617430169773002, 5.000000000000000000 ) ) ;
#103925 = AXIS2_PLACEMENT_3D ( 'NONE', #106159, #87303, #6830 ) ;
#103926 = AXIS2_PLACEMENT_3D ( 'NONE', #22142, #67107, #1099 ) ;
#103927 = FACE_OUTER_BOUND ( 'NONE', #132771, .T. ) ;
#103928 = LINE ( 'NONE', #4577, #97520 ) ;
#103929 = VECTOR ( 'NONE', #68944, 1000.000000000000000 ) ;
#103930 = CARTESIAN_POINT ( 'NONE',  ( 14.70025512860841133, -27.71228299555195917, 4.000000000000000000 ) ) ;
#103931 = ADVANCED_FACE ( 'NONE', ( #137154 ), #5880, .T. ) ;
#103932 = DIRECTION ( 'NONE',  ( -0.7071067811865486830, -0.7071067811865464625, -0.000000000000000000 ) ) ;
#103933 = VERTEX_POINT ( 'NONE', #50149 ) ;
#103934 = EDGE_CURVE ( 'NONE', #42625, #74781, #70514, .T. ) ;
#103935 = CARTESIAN_POINT ( 'NONE',  ( -28.49999999999979750, 5.696342897626483825, -7.587980461218466033 ) ) ;
#103936 = DIRECTION ( 'NONE',  ( -0.3543493200069162685, -0.000000000000000000, -0.9351131265310288487 ) ) ;
#103937 = UNCERTAINTY_MEASURE_WITH_UNIT (LENGTH_MEASURE( 1.000000000000000082E-05 ), #48620, 'distance_accuracy_value', 'NONE');
#103938 = VECTOR ( 'NONE', #127677, 1000.000000000000227 ) ;
#103939 = DIRECTION ( 'NONE',  ( -0.7071067811865486830, -0.7071067811865464625, 0.000000000000000000 ) ) ;
#103940 =( BOUNDED_CURVE ( )  B_SPLINE_CURVE ( 3, ( #60285, #116052, #94304, #27617 ),
 .UNSPECIFIED., .F., .T. ) 
 B_SPLINE_CURVE_WITH_KNOTS ( ( 4, 4 ),
 ( 5.920967161967927161, 7.341195215986652478 ),
 .UNSPECIFIED. ) 
 CURVE ( )  GEOMETRIC_REPRESENTATION_ITEM ( )  RATIONAL_B_SPLINE_CURVE ( ( 1.000000000000000000, 0.8388583629366581640, 0.8388583629366581640, 1.000000000000000000 ) ) 
 REPRESENTATION_ITEM ( '' )  );
#103941 = LINE ( 'NONE', #47506, #82758 ) ;
#103942 = CARTESIAN_POINT ( 'NONE',  ( 65.26669371712957002, -7.949999999999999289, 2.130196079827424427 ) ) ;
#103943 = DIRECTION ( 'NONE',  ( -1.000000000000000000, -0.000000000000000000, -0.000000000000000000 ) ) ;
#103944 = ORIENTED_EDGE ( 'NONE', *, *, #106167, .T. ) ;
#103945 = ORIENTED_EDGE ( 'NONE', *, *, #80012, .T. ) ;
#103946 = CARTESIAN_POINT ( 'NONE',  ( 62.68749999999999289, -5.819803920172573086, 5.819803920172572198 ) ) ;
#103947 = PLANE ( 'NONE',  #123497 ) ;
#103948 = PLANE ( 'NONE',  #138894 ) ;
#103949 = DIRECTION ( 'NONE',  ( -0.7071067811865487940, 0.7071067811865463515, -0.000000000000000000 ) ) ;
#103950 = AXIS2_PLACEMENT_3D ( 'NONE', #81882, #60108, #105006 ) ;
#103951 = CONICAL_SURFACE ( 'NONE', #25321, 2.055000000000001048, 0.9599310885968758145 ) ;
#103952 = ORIENTED_EDGE ( 'NONE', *, *, #64953, .F. ) ;
#103953 = EDGE_CURVE ( 'NONE', #120446, #25807, #126271, .T. ) ;
#103954 = CARTESIAN_POINT ( 'NONE',  ( 33.08333333333332860, 6.884901960086290629, -3.974999999999994316 ) ) ;
#103955 = AXIS2_PLACEMENT_3D ( 'NONE', #20505, #130013, #52436 ) ;
#103956 = EDGE_CURVE ( 'NONE', #86807, #123482, #95774, .T. ) ;
#103957 = DIRECTION ( 'NONE',  ( 0.5735764363510444941, 0.8191520442889929088, 0.000000000000000000 ) ) ;
#103958 = CARTESIAN_POINT ( 'NONE',  ( 55.12543019189811133, 5.291415217122919401, 3.055000000000002824 ) ) ;
#103959 = FACE_OUTER_BOUND ( 'NONE', #113418, .T. ) ;
#103960 = ORIENTED_EDGE ( 'NONE', *, *, #21229, .F. ) ;
#103961 = ORIENTED_EDGE ( 'NONE', *, *, #61608, .F. ) ;
#103962 = VECTOR ( 'NONE', #139696, 1000.000000000000227 ) ;
#103963 = AXIS2_PLACEMENT_3D ( 'NONE', #97528, #22786, #109840 ) ;
#103964 = CARTESIAN_POINT ( 'NONE',  ( 27.70701326429285061, -21.74070752338406365, 4.999753212805213565 ) ) ;
#103965 = FACE_OUTER_BOUND ( 'NONE', #3468, .T. ) ;
#103966 = AXIS2_PLACEMENT_3D ( 'NONE', #66509, #67215, #46209 ) ;
#103967 = DIRECTION ( 'NONE',  ( -1.000000000000000000, 0.000000000000000000, 0.000000000000000000 ) ) ;
#103968 = EDGE_CURVE ( 'NONE', #10069, #130801, #19642, .T. ) ;
#103969 = CARTESIAN_POINT ( 'NONE',  ( -17.99999999999986855, -16.60178936734450161, 0.8616154019347073145 ) ) ;
#103971 = ORIENTED_EDGE ( 'NONE', *, *, #97333, .F. ) ;
#103970 = CARTESIAN_POINT ( 'NONE',  ( -12.79289321881336683, 3.759292476615678336, 5.000000000000000000 ) ) ;
#103972 = LINE ( 'NONE', #106844, #117826 ) ;
#103973 = DIRECTION ( 'NONE',  ( -0.000000000000000000, -0.3543493200069152693, 0.9351131265310292928 ) ) ;
#103974 = CARTESIAN_POINT ( 'NONE',  ( 27.08314806772914451, 21.75929247661549581, 7.311836541448114346 ) ) ;
#103975 = VECTOR ( 'NONE', #117146, 1000.000000000000000 ) ;
#103976 = LINE ( 'NONE', #135239, #94721 ) ;
#103977 = VECTOR ( 'NONE', #72222, 1000.000000000000227 ) ;
#103978 = EDGE_LOOP ( 'NONE', ( #129705, #134243, #28260, #115884 ) ) ;
#103979 = VERTEX_POINT ( 'NONE', #119639 ) ;
#103980 = DIRECTION ( 'NONE',  ( 0.000000000000000000, -1.000000000000000000, 0.000000000000000000 ) ) ;
#103981 = DIRECTION ( 'NONE',  ( -0.7071067811865486830, 0.7071067811865464625, 0.000000000000000000 ) ) ;
#103982 = CARTESIAN_POINT ( 'NONE',  ( 150.3000000000000114, 0.000000000000000000, 0.000000000000000000 ) ) ;
#103983 = CARTESIAN_POINT ( 'NONE',  ( -18.32816939922340183, -6.740707523384207533, 4.000000000000000000 ) ) ;
#103984 = ORIENTED_EDGE ( 'NONE', *, *, #82284, .F. ) ;
#103985 = ORIENTED_EDGE ( 'NONE', *, *, #141435, .T. ) ;
#103986 = VECTOR ( 'NONE', #67598, 1000.000000000000227 ) ;
#103987 = FACE_OUTER_BOUND ( 'NONE', #38785, .T. ) ;
#103988 = FACE_OUTER_BOUND ( 'NONE', #14522, .T. ) ;
#103989 = ORIENTED_EDGE ( 'NONE', *, *, #33492, .F. ) ;
#103990 = CARTESIAN_POINT ( 'NONE',  ( 34.42499999999998295, 13.54139925780190445, 5.000000000000000000 ) ) ;
#103991 = EDGE_LOOP ( 'NONE', ( #67450, #13640, #84597, #120125 ) ) ;
#103992 = CARTESIAN_POINT ( 'NONE',  ( 0.000000000000000000, 0.000000000000000000, 5.000000000000000000 ) ) ;
#103993 = CARTESIAN_POINT ( 'NONE',  ( -3.792893218813427669, -2.240707523384264377, 5.000000000000000000 ) ) ;
#103994 = FACE_BOUND ( 'NONE', #110648, .T. ) ;
#103995 = CARTESIAN_POINT ( 'NONE',  ( -33.48921356237309510, -27.52281430457078670, 5.000000000000000000 ) ) ;
#103996 = EDGE_CURVE ( 'NONE', #100892, #90194, #105912, .T. ) ;
#103997 = DIRECTION ( 'NONE',  ( 0.7071067811865487940, -0.7071067811865463515, 0.000000000000000000 ) ) ;
#103998 = CARTESIAN_POINT ( 'NONE',  ( 44.99451991528749772, 28.92564299267969474, 4.000000000000000000 ) ) ;
#103999 = DIRECTION ( 'NONE',  ( -1.000000000000000000, -0.000000000000000000, -0.000000000000000000 ) ) ;
#104000 = CARTESIAN_POINT ( 'NONE',  ( 34.21321903303337564, 12.75929247661558641, 10.29404684609043308 ) ) ;
#104001 = PRODUCT_CONTEXT ( 'NONE', #69885, 'mechanical' ) ;
#104002 = ORIENTED_EDGE ( 'NONE', *, *, #9853, .F. ) ;
#104003 = ADVANCED_FACE ( 'NONE', ( #29098 ), #116813, .F. ) ;
#104004 = VERTEX_POINT ( 'NONE', #18178 ) ;
#104005 = CARTESIAN_POINT ( 'NONE',  ( 98.05793019189812298, 6.110000000000000320, -1.637169565754156064 ) ) ;
#104006 = EDGE_LOOP ( 'NONE', ( #70187, #121609, #139819, #3519 ) ) ;
#104007 = EDGE_CURVE ( 'NONE', #60798, #79691, #50854, .T. ) ;
#104008 = LINE ( 'NONE', #57713, #76675 ) ;
#104009 = EDGE_CURVE ( 'NONE', #30305, #63170, #85598, .T. ) ;
#104010 = DIRECTION ( 'NONE',  ( -0.7071067811865486830, -0.7071067811865464625, 0.000000000000000000 ) ) ;
#104011 = EDGE_CURVE ( 'NONE', #22459, #98793, #49756, .T. ) ;
#104012 = LINE ( 'NONE', #51112, #77223 ) ;
#104013 = ORIENTED_EDGE ( 'NONE', *, *, #120874, .F. ) ;
#104014 = DIRECTION ( 'NONE',  ( 0.7071067811865487940, 0.7071067811865463515, 0.000000000000000000 ) ) ;
#104015 = CYLINDRICAL_SURFACE ( 'NONE', #75604, 2.500000000000000444 ) ;
#104016 = EDGE_CURVE ( 'NONE', #33632, #15104, #61750, .T. ) ;
#104017 = CARTESIAN_POINT ( 'NONE',  ( -9.084913231937559175, -12.74070752338414891, 18.74364270924352027 ) ) ;
#104019 = DIRECTION ( 'NONE',  ( 0.7071067811865487940, 0.7071067811865463515, 0.000000000000000000 ) ) ;
#104018 = CARTESIAN_POINT ( 'NONE',  ( -5.293876922608010460, 22.22500000000000142, 4.000000000000000000 ) ) ;
#104020 = PLANE ( 'NONE',  #117885 ) ;
#104021 =( GEOMETRIC_REPRESENTATION_CONTEXT ( 3 ) GLOBAL_UNCERTAINTY_ASSIGNED_CONTEXT ( ( #110168 ) ) GLOBAL_UNIT_ASSIGNED_CONTEXT ( ( #92059, #58795, #36278 ) ) REPRESENTATION_CONTEXT ( 'NONE', 'WORKASPACE' ) );
#104022 = VECTOR ( 'NONE', #132280, 1000.000000000000000 ) ;
#104023 = VECTOR ( 'NONE', #33715, 1000.000000000000227 ) ;
#104024 = CARTESIAN_POINT ( 'NONE',  ( -34.92500000000001137, -9.281509562795667634, 4.759050581649335143 ) ) ;
#104025 = VECTOR ( 'NONE', #39861, 1000.000000000000000 ) ;
#104026 = VERTEX_POINT ( 'NONE', #84902 ) ;
#104027 = CARTESIAN_POINT ( 'NONE',  ( 0.000000000000000000, -14.29000000000013593, -12.70000000000045404 ) ) ;
#104028 = FACE_OUTER_BOUND ( 'NONE', #88693, .T. ) ;
#104029 = VECTOR ( 'NONE', #127394, 1000.000000000000227 ) ;
#104030 = EDGE_CURVE ( 'NONE', #70917, #135458, #108400, .T. ) ;
#104031 = EDGE_LOOP ( 'NONE', ( #26673, #121623, #53060, #137735 ) ) ;
#104032 = VERTEX_POINT ( 'NONE', #108757 ) ;
#104033 = ADVANCED_FACE ( 'NONE', ( #86350 ), #29792, .F. ) ;
#104034 = ORIENTED_EDGE ( 'NONE', *, *, #21382, .T. ) ;
#104035 = CARTESIAN_POINT ( 'NONE',  ( 40.97959685856476852, 6.109999999999999432, 1.637169565754164280 ) ) ;
#104036 = EDGE_LOOP ( 'NONE', ( #77398, #73538, #120948, #66979 ) ) ;
#104037 = VECTOR ( 'NONE', #41186, 1000.000000000000000 ) ;
#104038 = EDGE_CURVE ( 'NONE', #31242, #74888, #97164, .T. ) ;
#104039 = VECTOR ( 'NONE', #33536, 1000.000000000000000 ) ;
#104040 = CARTESIAN_POINT ( 'NONE',  ( 14.19163961620377101, 6.094999999999988205, -1.633150327867694651 ) ) ;
#104041 = VERTEX_POINT ( 'NONE', #131266 ) ;
#104042 = DIRECTION ( 'NONE',  ( -0.6830127018922181881, 0.6830127018922202975, -0.2588190451025214056 ) ) ;
#104043 = ORIENTED_EDGE ( 'NONE', *, *, #49080, .T. ) ;
#104044 = SURFACE_STYLE_FILL_AREA ( #80220 ) ;
#104045 = AXIS2_PLACEMENT_3D ( 'NONE', #44815, #131779, #99107 ) ;
#104046 = DIRECTION ( 'NONE',  ( -1.000000000000000000, 0.000000000000000000, -0.000000000000000000 ) ) ;
#104048 = VERTEX_POINT ( 'NONE', #74772 ) ;
#104047 = DIRECTION ( 'NONE',  ( -0.6830127018922180770, -0.6830127018922204085, -0.2588190451025213501 ) ) ;
#104049 = ORIENTED_EDGE ( 'NONE', *, *, #99734, .F. ) ;
#104050 = FACE_OUTER_BOUND ( 'NONE', #80808, .T. ) ;
#104051 = CARTESIAN_POINT ( 'NONE',  ( -22.17183060077632106, -11.24070752338416845, 4.000000000000000000 ) ) ;
#104052 = ORIENTED_EDGE ( 'NONE', *, *, #85357, .F. ) ;
#104053 = AXIS2_PLACEMENT_3D ( 'NONE', #60712, #93992, #117165 ) ;
#104054 = LINE ( 'NONE', #49741, #136135 ) ;
#104055 = ORIENTED_EDGE ( 'NONE', *, *, #87479, .T. ) ;
#104056 = ORIENTED_EDGE ( 'NONE', *, *, #126256, .F. ) ;
#104057 = ORIENTED_EDGE ( 'NONE', *, *, #124729, .T. ) ;
#104058 = EDGE_LOOP ( 'NONE', ( #19362, #18791, #120029, #65705 ) ) ;
#104059 = EDGE_CURVE ( 'NONE', #121778, #131245, #133446, .T. ) ;
#104060 = FACE_OUTER_BOUND ( 'NONE', #113708, .T. ) ;
#104061 = CONICAL_SURFACE ( 'NONE', #55477, 2.055000000000000604, 0.9599310885968764806 ) ;
#104062 = VECTOR ( 'NONE', #135032, 1000.000000000000000 ) ;
#104063 = FILL_AREA_STYLE_COLOUR ( '', #83937 ) ;
#104064 = VECTOR ( 'NONE', #54419, 999.9999999999998863 ) ;
#104065 = CARTESIAN_POINT ( 'NONE',  ( 12.19999999999999574, -21.76999999999999247, -40.00000000000000000 ) ) ;
#104066 = CARTESIAN_POINT ( 'NONE',  ( -84.29974487139159578, -27.71228299555264840, 4.000000000000000000 ) ) ;
#104067 = CARTESIAN_POINT ( 'NONE',  ( 33.18398860626899705, 28.73617430169810305, 5.000000000000000000 ) ) ;
#104068 = ORIENTED_EDGE ( 'NONE', *, *, #91441, .T. ) ;
#104069 = VECTOR ( 'NONE', #77963, 1000.000000000000000 ) ;
#104070 = LINE ( 'NONE', #83818, #107290 ) ;
#104071 = ADVANCED_FACE ( 'NONE', ( #140696 ), #97928, .F. ) ;
#104072 = CARTESIAN_POINT ( 'NONE',  ( 19.95790314143522437, 6.871911579029515771, 3.967499999999989146 ) ) ;
#104073 = DIRECTION ( 'NONE',  ( -0.000000000000000000, 0.000000000000000000, 1.000000000000000000 ) ) ;
#104074 = CARTESIAN_POINT ( 'NONE',  ( 96.81250000000000000, 5.819803920172571310, 5.819803920172576639 ) ) ;
#104075 = DIRECTION ( 'NONE',  ( 0.000000000000000000, -1.000000000000000000, 0.000000000000000000 ) ) ;
#104076 = ORIENTED_EDGE ( 'NONE', *, *, #13502, .T. ) ;
#104077 = ORIENTED_EDGE ( 'NONE', *, *, #108593, .F. ) ;
#104078 = ADVANCED_FACE ( 'NONE', ( #121091 ), #21060, .T. ) ;
#104079 = ORIENTED_EDGE ( 'NONE', *, *, #38682, .F. ) ;
#104080 = PRESENTATION_STYLE_ASSIGNMENT (( #125145 ) ) ;
#104081 = UNCERTAINTY_MEASURE_WITH_UNIT (LENGTH_MEASURE( 1.000000000000000082E-05 ), #83564, 'distance_accuracy_value', 'NONE');
#104082 = CIRCLE ( 'NONE', #122626, 2.500000000000000888 ) ;
#104083 = PLANE ( 'NONE',  #68583 ) ;
#104084 = B_SPLINE_CURVE_WITH_KNOTS ( 'NONE', 3,
 ( #65500, #98098, #109678, #46627, #11768, #125574, #91512, #136419, #100240, #35003, #89356, #58932, #122686, #69054, #101652, #103094, #112535, #113964, #3729, #26252, #135724, #48020, #90807, #56052, #124838, #13193, #57470, #25513, #92191, #79245, #37113, #123451, #45880, #35736, #892, #36409 ),
 .UNSPECIFIED., .F., .F.,
 ( 4, 2, 2, 2, 2, 2, 2, 2, 2, 2, 2, 2, 2, 2, 2, 2, 2, 4 ),
 ( 0.000000000000000000, 0.002483296972363799576, 0.003724945458545699147, 0.004966593944727599151, 0.005587418187818549153, 0.006208242430909499156, 0.007449890917091394824, 0.008691539403273291359, 0.009933187889455186159, 0.01117483637563708443, 0.01241648486181898096, 0.01365813334800087923, 0.01489978183418277577, 0.01614143032036467404, 0.01738307880654656884, 0.01800390304963752144, 0.01862472729272847058, 0.01986637577891036885 ),
 .UNSPECIFIED. ) ;
#104085 = CARTESIAN_POINT ( 'NONE',  ( 21.29159235450332233, -2.500000000000000444, 3.061616997868384620E-16 ) ) ;
#104086 = DIRECTION ( 'NONE',  ( 0.7071067811865487940, -0.7071067811865463515, 0.000000000000000000 ) ) ;
#104087 = CARTESIAN_POINT ( 'NONE',  ( 72.97459685856478018, 1.637169565754164280, -6.109999999999997655 ) ) ;
#104088 = DIRECTION ( 'NONE',  ( -0.7071067811865486830, -0.7071067811865464625, 0.000000000000000000 ) ) ;
#104089 = LINE ( 'NONE', #106230, #46079 ) ;
#104090 = LINE ( 'NONE', #137479, #111224 ) ;
#104091 = EDGE_CURVE ( 'NONE', #118058, #105436, #26547, .T. ) ;
#104092 = CARTESIAN_POINT ( 'NONE',  ( -17.99451991528748351, 28.92564299267950645, 4.000000000000000000 ) ) ;
#104093 = CARTESIAN_POINT ( 'NONE',  ( 29.24139925780183091, 21.72500000000000853, 5.000000000000000000 ) ) ;
#104094 = ORIENTED_EDGE ( 'NONE', *, *, #35498, .T. ) ;
#104095 = CARTESIAN_POINT ( 'NONE',  ( 83.24999999999998579, -9.735942053221458872E-16, 7.950000000000000178 ) ) ;
#104096 = VERTEX_POINT ( 'NONE', #2133 ) ;
#104097 = LINE ( 'NONE', #36044, #127062 ) ;
#104099 = ORIENTED_EDGE ( 'NONE', *, *, #64213, .F. ) ;
#104098 = CARTESIAN_POINT ( 'NONE',  ( 34.42499999999998295, -16.45860074219779889, 5.000000000000000000 ) ) ;
#104100 = EDGE_CURVE ( 'NONE', #16952, #3281, #1432, .T. ) ;
#104101 = PLANE ( 'NONE',  #95003 ) ;
#104102 = DIRECTION ( 'NONE',  ( -0.7071067811865486830, -0.7071067811865464625, 0.000000000000000000 ) ) ;
#104103 = ORIENTED_EDGE ( 'NONE', *, *, #69191, .T. ) ;
#104104 = DIRECTION ( 'NONE',  ( 0.7071067811865487940, -0.7071067811865463515, 0.000000000000000000 ) ) ;
#104105 = ORIENTED_EDGE ( 'NONE', *, *, #11729, .T. ) ;
#104106 = CARTESIAN_POINT ( 'NONE',  ( -3.005480084712505828, 28.92564299267936079, 4.000000000000000000 ) ) ;
#104107 = ORIENTED_EDGE ( 'NONE', *, *, #54153, .T. ) ;
#104108 = DIRECTION ( 'NONE',  ( -0.8571673007021110013, 1.049727191138617093E-16, 0.5150380749100563760 ) ) ;
#104109 = CARTESIAN_POINT ( 'NONE',  ( 93.70419371712957002, -6.884901960086285300, -3.975000000000000089 ) ) ;
#104110 = FACE_OUTER_BOUND ( 'NONE', #128565, .T. ) ;
#104111 = FACE_OUTER_BOUND ( 'NONE', #11607, .T. ) ;
#104112 = ORIENTED_EDGE ( 'NONE', *, *, #51855, .F. ) ;
#104113 = DIRECTION ( 'NONE',  ( -0.7071067811865486830, -0.7071067811865464625, 0.000000000000000000 ) ) ;
#104114 = LINE ( 'NONE', #126595, #34571 ) ;
#104115 = CARTESIAN_POINT ( 'NONE',  ( 27.27083333333332860, 6.094999999999991758, 1.633150327867687102 ) ) ;
#104116 =( LENGTH_UNIT ( ) NAMED_UNIT ( * ) SI_UNIT ( .MILLI., .METRE. ) );
#104117 = CARTESIAN_POINT ( 'NONE',  ( -10.49999999999992539, 3.073033219394616378, -6.593910359670993593 ) ) ;
#104118 = EDGE_LOOP ( 'NONE', ( #45334, #88180, #31313, #101699 ) ) ;
#104119 = DIRECTION ( 'NONE',  ( 0.7071067811865486830, -0.7071067811865464625, -0.000000000000000000 ) ) ;
#104120 = ORIENTED_EDGE ( 'NONE', *, *, #119329, .F. ) ;
#104121 = ADVANCED_FACE ( 'NONE', ( #121792 ), #89889, .F. ) ;
#104122 = CARTESIAN_POINT ( 'NONE',  ( 87.06293019189807580, 1.637169565754157174, 6.110000000000002984 ) ) ;
#104123 = CARTESIAN_POINT ( 'NONE',  ( -24.18398860626899705, 28.73617430169804265, 5.000000000000000000 ) ) ;
#104124 = VECTOR ( 'NONE', #55354, 1000.000000000000000 ) ;
#104125 = CARTESIAN_POINT ( 'NONE',  ( 9.183988606268997046, 28.73617430169793607, 5.000000000000000000 ) ) ;
#104126 = CARTESIAN_POINT ( 'NONE',  ( -78.29974487139158157, -27.71228299555260577, 4.000000000000000000 ) ) ;
#104127 = ORIENTED_EDGE ( 'NONE', *, *, #128123, .F. ) ;
#104128 = VECTOR ( 'NONE', #60651, 1000.000000000000000 ) ;
#104129 = CONICAL_SURFACE ( 'NONE', #132019, 2.055000000000001048, 0.9599310885968758145 ) ;
#104130 = DIRECTION ( 'NONE',  ( -0.7071067811865487940, 0.7071067811865463515, -0.000000000000000000 ) ) ;
#104131 = VECTOR ( 'NONE', #47424, 1000.000000000000000 ) ;
#104132 = DIRECTION ( 'NONE',  ( 0.5735764363510453823, -0.8191520442889923537, 1.003171929053525486E-16 ) ) ;
#104133 = DIRECTION ( 'NONE',  ( 0.7071067811865487940, 0.7071067811865463515, 0.000000000000000000 ) ) ;
#104134 = ADVANCED_FACE ( 'NONE', ( #120342 ), #65328, .T. ) ;
#104135 = CARTESIAN_POINT ( 'NONE',  ( 14.58838509405157602, 22.22500000000000142, 4.777194822843812361 ) ) ;
#104137 = ORIENTED_EDGE ( 'NONE', *, *, #27301, .T. ) ;
#104136 = CARTESIAN_POINT ( 'NONE',  ( -12.29974487139158512, -27.71228299555214747, 4.000000000000000000 ) ) ;
#104138 = CARTESIAN_POINT ( 'NONE',  ( 5.816011393731002066, 28.73617430169783304, 5.000000000000000000 ) ) ;
#104139 = DIRECTION ( 'NONE',  ( 0.6830127018922181881, 0.6830127018922202975, -0.2588190451025214056 ) ) ;
#104140 = AXIS2_PLACEMENT_3D ( 'NONE', #98279, #84555, #9065 ) ;
#104141 = LINE ( 'NONE', #4805, #16855 ) ;
#104142 = PRODUCT_DEFINITION ( 'UNKNOWN', '', #44803, #21114 ) ;
#104143 = ORIENTED_EDGE ( 'NONE', *, *, #6687, .F. ) ;
#104144 = VERTEX_POINT ( 'NONE', #78321 ) ;
#104145 = EDGE_LOOP ( 'NONE', ( #66226, #110638, #55172, #42771 ) ) ;
#104146 = CARTESIAN_POINT ( 'NONE',  ( 80.20876352523143282, -7.482591942790329030E-16, 6.110000000000001208 ) ) ;
#104147 = ORIENTED_EDGE ( 'NONE', *, *, #62326, .T. ) ;
#104148 = CARTESIAN_POINT ( 'NONE',  ( 122.6835989386367771, -1.600000000000086020, -34.92499999999998295 ) ) ;
#104149 = CARTESIAN_POINT ( 'NONE',  ( -7.940000000000001279, -33.26999999999999602, -10.00000000000000178 ) ) ;
#104150 = VECTOR ( 'NONE', #50137, 1000.000000000000000 ) ;
#104151 = DIRECTION ( 'NONE',  ( 0.3543493200069163240, 0.000000000000000000, -0.9351131265310288487 ) ) ;
#104152 = DIRECTION ( 'NONE',  ( 0.6830127018922180770, -0.6830127018922204085, -0.2588190451025213501 ) ) ;
#104153 = ORIENTED_EDGE ( 'NONE', *, *, #71640, .T. ) ;
#104154 = ADVANCED_FACE ( 'NONE', ( #10875 ), #131994, .T. ) ;
#104155 = PLANE ( 'NONE',  #97680 ) ;
#104157 = CARTESIAN_POINT ( 'NONE',  ( 13.13598696172163116, 2.500000000000000888, 0.000000000000000000 ) ) ;
#104156 = SHAPE_REPRESENTATION ( '1.4 Collar', ( #127880 ), #118637 ) ;
#104158 = VECTOR ( 'NONE', #59799, 999.9999999999998863 ) ;
#104159 = CARTESIAN_POINT ( 'NONE',  ( 75.89126352523143737, -4.472830434245839371, -4.472830434245839371 ) ) ;
#104160 = EDGE_LOOP ( 'NONE', ( #7350, #142000, #50519, #127097 ) ) ;
#104161 = CARTESIAN_POINT ( 'NONE',  ( 17.99451991528748351, 28.92564299267950645, 4.000000000000000000 ) ) ;
#104162 = CARTESIAN_POINT ( 'NONE',  ( 34.92499999999998295, -4.298069433178973497, 4.500000000000000888 ) ) ;
#104163 = VECTOR ( 'NONE', #127515, 1000.000000000000227 ) ;
#104164 = ORIENTED_EDGE ( 'NONE', *, *, #62862, .T. ) ;
#104165 = ORIENTED_EDGE ( 'NONE', *, *, #43631, .T. ) ;
#104166 = LINE ( 'NONE', #118459, #88636 ) ;
#104167 = AXIS2_PLACEMENT_3D ( 'NONE', #39033, #83256, #128886 ) ;
#104168 = DIRECTION ( 'NONE',  ( -0.7071067811865486830, 0.7071067811865464625, 0.000000000000000000 ) ) ;
#104169 = DIRECTION ( 'NONE',  ( 0.7071067811865486830, -0.7071067811865464625, -0.000000000000000000 ) ) ;
#104170 = VECTOR ( 'NONE', #26265, 1000.000000000000000 ) ;
#104171 = LINE ( 'NONE', #102072, #59605 ) ;
#104172 = DIRECTION ( 'NONE',  ( -0.7071067811865486830, -0.7071067811865464625, 0.000000000000000000 ) ) ;
#104173 = LINE ( 'NONE', #91898, #58218 ) ;
#104174 =( NAMED_UNIT ( * ) SI_UNIT ( $, .STERADIAN. ) SOLID_ANGLE_UNIT ( ) );
#104175 = EDGE_CURVE ( 'NONE', #86612, #53081, #67470, .T. ) ;
#104176 = VECTOR ( 'NONE', #64106, 1000.000000000000227 ) ;
#104177 = ORIENTED_EDGE ( 'NONE', *, *, #63147, .F. ) ;
#104178 = ORIENTED_EDGE ( 'NONE', *, *, #36836, .T. ) ;
#104179 = EDGE_CURVE ( 'NONE', #25213, #55140, #57308, .T. ) ;
#104180 = VERTEX_POINT ( 'NONE', #90633 ) ;
#104181 = ADVANCED_FACE ( 'NONE', ( #55872 ), #10185, .F. ) ;
#104182 = VECTOR ( 'NONE', #10341, 1000.000000000000000 ) ;
#104183 = EDGE_CURVE ( 'NONE', #21250, #20431, #23182, .T. ) ;
#104184 = LINE ( 'NONE', #62157, #73358 ) ;
#104185 = CARTESIAN_POINT ( 'NONE',  ( -10.49999999999993072, 15.43112307739203182, 4.000000000000000000 ) ) ;
#104186 = VERTEX_POINT ( 'NONE', #76180 ) ;
#104187 = FILL_AREA_STYLE_COLOUR ( '', #83060 ) ;
#104188 = DIRECTION ( 'NONE',  ( -0.000000000000000000, 0.3543493200069153248, 0.9351131265310292928 ) ) ;
#104189 = CARTESIAN_POINT ( 'NONE',  ( 3.989119713460488992, -22.02621442084248216, 4.990779571109224655 ) ) ;
#104190 = DIRECTION ( 'NONE',  ( 0.7071067811865487940, -0.7071067811865463515, 0.000000000000000000 ) ) ;
#104191 = VECTOR ( 'NONE', #60430, 1000.000000000000000 ) ;
#104192 = CARTESIAN_POINT ( 'NONE',  ( 2.816011393730999401, 28.73617430169785436, 5.000000000000000000 ) ) ;
#104193 = EDGE_LOOP ( 'NONE', ( #29050, #53856, #82693, #143006 ) ) ;
#104194 = DIRECTION ( 'NONE',  ( 0.6830127018922181881, 0.6830127018922202975, -0.2588190451025214056 ) ) ;
#104195 = LINE ( 'NONE', #126676, #113548 ) ;
#104196 = ADVANCED_FACE ( 'NONE', ( #66038 ), #111661, .F. ) ;
#104197 = ORIENTED_EDGE ( 'NONE', *, *, #98504, .T. ) ;
#104198 = CARTESIAN_POINT ( 'NONE',  ( 16.88727739707083231, 22.22500000000000142, 24.63360875038745235 ) ) ;
#104199 = ORIENTED_EDGE ( 'NONE', *, *, #68580, .F. ) ;
#104200 = EDGE_CURVE ( 'NONE', #129512, #25493, #68201, .T. ) ;
#104201 = ORIENTED_EDGE ( 'NONE', *, *, #23323, .F. ) ;
#104202 = CARTESIAN_POINT ( 'NONE',  ( -36.48921356237310221, -27.52281430457080802, 5.000000000000000000 ) ) ;
#104203 = ORIENTED_EDGE ( 'NONE', *, *, #98984, .T. ) ;
#104204 = VERTEX_POINT ( 'NONE', #13030 ) ;
#104205 = CARTESIAN_POINT ( 'NONE',  ( 74.22959685856477563, -6.110000000000000320, -1.637169565754161393 ) ) ;
#104207 = ORIENTED_EDGE ( 'NONE', *, *, #128914, .F. ) ;
#104206 = AXIS2_PLACEMENT_3D ( 'NONE', #72276, #39623, #61396 ) ;
#104208 = EDGE_CURVE ( 'NONE', #87694, #21974, #104315, .T. ) ;
#104209 = FACE_OUTER_BOUND ( 'NONE', #128235, .T. ) ;
#104210 = CARTESIAN_POINT ( 'NONE',  ( 27.70701326429285061, -21.74070752338406365, 4.999753212805213565 ) ) ;
#104211 = LINE ( 'NONE', #38989, #112180 ) ;
#104212 = CARTESIAN_POINT ( 'NONE',  ( 106.4587635252314328, 0.000000000000000000, -6.110000000000001208 ) ) ;
#104213 = CARTESIAN_POINT ( 'NONE',  ( 24.29974487139158867, -27.71228299555223273, 4.000000000000000000 ) ) ;
#104214 = DIRECTION ( 'NONE',  ( 0.7071067811865486830, -0.7071067811865464625, -0.000000000000000000 ) ) ;
#104215 = DIRECTION ( 'NONE',  ( 0.6830127018922180770, -0.6830127018922204085, -0.2588190451025213501 ) ) ;
#104216 = ADVANCED_FACE ( 'NONE', ( #16605 ), #113794, .F. ) ;
#104217 = VECTOR ( 'NONE', #54923, 1000.000000000000000 ) ;
#104218 = PLANE ( 'NONE',  #63243 ) ;
#104219 =( NAMED_UNIT ( * ) PLANE_ANGLE_UNIT ( ) SI_UNIT ( $, .RADIAN. ) );
#104221 = FILL_AREA_STYLE ('',( #137613 ) ) ;
#104220 = VECTOR ( 'NONE', #48595, 1000.000000000000000 ) ;
#104223 = EDGE_LOOP ( 'NONE', ( #118656, #52976, #136922, #100883 ) ) ;
#104222 = AXIS2_PLACEMENT_3D ( 'NONE', #39754, #117956, #107109 ) ;
#104224 = DIRECTION ( 'NONE',  ( -0.7071067811865486830, 0.7071067811865464625, 0.000000000000000000 ) ) ;
#104225 = CARTESIAN_POINT ( 'NONE',  ( 25.98012225071437342, -17.24070752338409918, 20.23474786156475602 ) ) ;
#104226 = VERTEX_POINT ( 'NONE', #70341 ) ;
#104227 = VERTEX_POINT ( 'NONE', #15853 ) ;
#104228 = AXIS2_PLACEMENT_3D ( 'NONE', #50896, #95090, #63234 ) ;
#104229 = EDGE_CURVE ( 'NONE', #20849, #26888, #79803, .T. ) ;
#104230 = CARTESIAN_POINT ( 'NONE',  ( 13.82816939922343558, 15.75929247661555443, 4.000000000000000000 ) ) ;
#104231 = AXIS2_PLACEMENT_3D ( 'NONE', #40463, #62211, #142450 ) ;
#104232 = AXIS2_PLACEMENT_3D ( 'NONE', #44981, #48491, #15807 ) ;
#104233 = VERTEX_POINT ( 'NONE', #69608 ) ;
#104234 = VECTOR ( 'NONE', #112153, 1000.000000000000000 ) ;
#104235 = PLANE ( 'NONE',  #16627 ) ;
#104236 = LINE ( 'NONE', #4900, #101111 ) ;
#104237 = DIRECTION ( 'NONE',  ( 0.7071067811865487940, -0.7071067811865463515, 0.000000000000000000 ) ) ;
#104238 = DIRECTION ( 'NONE',  ( -0.7071067811865487940, 0.7071067811865463515, -0.000000000000000000 ) ) ;
#104239 = EDGE_LOOP ( 'NONE', ( #2522, #21687, #45783, #123684 ) ) ;
#104240 = PRESENTATION_STYLE_ASSIGNMENT (( #68817 ) ) ;
#104242 = ORIENTED_EDGE ( 'NONE', *, *, #45082, .T. ) ;
#104241 = AXIS2_PLACEMENT_3D ( 'NONE', #11585, #63880, #31949 ) ;
#104243 = CARTESIAN_POINT ( 'NONE',  ( 34.42499999999998295, -0.02281430457060432127, 5.000000000000000000 ) ) ;
#104244 = EDGE_CURVE ( 'NONE', #18293, #123961, #92029, .T. ) ;
#104245 = CARTESIAN_POINT ( 'NONE',  ( 29.67123647476855552, 0.000000000000000000, 7.934999999999990727 ) ) ;
#104246 = CARTESIAN_POINT ( 'NONE',  ( 5.671830600776434750, -0.7407075233842735917, 4.000000000000000000 ) ) ;
#104247 = PLANE ( 'NONE',  #20524 ) ;
#104248 = CARTESIAN_POINT ( 'NONE',  ( 12.52748590975845566, -8.712603770609980813, -3.790722776764650526 ) ) ;
#104249 = VERTEX_POINT ( 'NONE', #91356 ) ;
#104250 = ORIENTED_EDGE ( 'NONE', *, *, #105092, .F. ) ;
#104251 = ORIENTED_EDGE ( 'NONE', *, *, #96503, .T. ) ;
#104253 = VECTOR ( 'NONE', #66716, 1000.000000000000227 ) ;
#104252 = FACE_OUTER_BOUND ( 'NONE', #4767, .T. ) ;
#104254 = CARTESIAN_POINT ( 'NONE',  ( 11.56505274454301357, 4.584330080086930965E-16, 0.000000000000000000 ) ) ;
#104255 = CARTESIAN_POINT ( 'NONE',  ( 45.48921356237309510, -27.52281430457087197, 5.000000000000000000 ) ) ;
#104256 = CARTESIAN_POINT ( 'NONE',  ( -8.207106781186485733, 9.759292476615620160, 5.000000000000000000 ) ) ;
#104257 = CARTESIAN_POINT ( 'NONE',  ( -6.084913231937570721, -12.74070752338414891, 18.74364270924352738 ) ) ;
#104258 = FACE_OUTER_BOUND ( 'NONE', #86714, .T. ) ;
#104259 = VECTOR ( 'NONE', #76040, 999.9999999999998863 ) ;
#104260 = AXIS2_PLACEMENT_3D ( 'NONE', #12397, #90705, #1500 ) ;
#104261 = CARTESIAN_POINT ( 'NONE',  ( 0.000000000000000000, 0.000000000000000000, 5.000000000000000000 ) ) ;
#104262 = ADVANCED_FACE ( 'NONE', ( #126111 ), #123973, .F. ) ;
#104263 = DIRECTION ( 'NONE',  ( -0.7071067811865486830, -0.7071067811865464625, 0.000000000000000000 ) ) ;
#104264 = DIRECTION ( 'NONE',  ( 0.7071067811865487940, 0.7071067811865463515, 0.000000000000000000 ) ) ;
#104265 = VECTOR ( 'NONE', #126269, 1000.000000000000000 ) ;
#104266 = ORIENTED_EDGE ( 'NONE', *, *, #76529, .F. ) ;
#104267 = LINE ( 'NONE', #84688, #53368 ) ;
#104269 = VECTOR ( 'NONE', #106964, 1000.000000000000000 ) ;
#104268 = CARTESIAN_POINT ( 'NONE',  ( 2.700255128608413990, -27.71228299555204089, 4.000000000000000000 ) ) ;
#104270 = ORIENTED_EDGE ( 'NONE', *, *, #131628, .T. ) ;
#104271 = CARTESIAN_POINT ( 'NONE',  ( -3.183988606268992161, 28.73617430169789699, 5.000000000000000000 ) ) ;
#104272 = ORIENTED_EDGE ( 'NONE', *, *, #126834, .F. ) ;
#104273 = EDGE_LOOP ( 'NONE', ( #12591, #83570, #21516, #40114 ) ) ;
#104274 = ADVANCED_FACE ( 'NONE', ( #59448 ), #82594, .T. ) ;
#104275 = AXIS2_PLACEMENT_3D ( 'NONE', #114944, #12801, #14945 ) ;
#104276 = DIRECTION ( 'NONE',  ( -1.369518533665900312E-16, 1.000000000000000000, -0.000000000000000000 ) ) ;
#104277 = DIRECTION ( 'NONE',  ( 1.000000000000000000, 0.000000000000000000, 0.000000000000000000 ) ) ;
#104278 = CARTESIAN_POINT ( 'NONE',  ( 48.48921356237309510, -27.52281430457089328, 5.000000000000000000 ) ) ;
#104279 = ORIENTED_EDGE ( 'NONE', *, *, #62813, .T. ) ;
#104280 = ORIENTED_EDGE ( 'NONE', *, *, #16166, .T. ) ;
#104281 = FACE_OUTER_BOUND ( 'NONE', #30262, .T. ) ;
#104282 = DIRECTION ( 'NONE',  ( 1.000000000000000000, 0.000000000000000000, 0.000000000000000000 ) ) ;
#104283 = CARTESIAN_POINT ( 'NONE',  ( 126.6625270504629128, 7.949999999999998401, 1.460391307983218338E-15 ) ) ;
#104284 = FACE_OUTER_BOUND ( 'NONE', #56641, .T. ) ;
#104285 = VECTOR ( 'NONE', #9797, 999.9999999999998863 ) ;
#104286 = CARTESIAN_POINT ( 'NONE',  ( 12.51665438641036054, 22.22500000000000142, 4.500000000000000888 ) ) ;
#104288 = ADVANCED_FACE ( 'NONE', ( #81184 ), #14482, .T. ) ;
#104287 = LINE ( 'NONE', #3541, #137127 ) ;
#104289 = LINE ( 'NONE', #92006, #49470 ) ;
#104290 = CARTESIAN_POINT ( 'NONE',  ( -28.49999999999979750, 9.052185695429079360, 5.000000000000000000 ) ) ;
#104292 = AXIS2_PLACEMENT_3D ( 'NONE', #119463, #77454, #76734 ) ;
#104291 = CARTESIAN_POINT ( 'NONE',  ( 32.20790314143521726, -6.871911579029513106, -3.967499999999993587 ) ) ;
#104293 = CARTESIAN_POINT ( 'NONE',  ( 10.62456980810188689, -6.871911579029512218, 3.967499999999996252 ) ) ;
#104294 = DIRECTION ( 'NONE',  ( -0.7071067811865487940, 0.7071067811865463515, -0.000000000000000000 ) ) ;
#104295 = DIRECTION ( 'NONE',  ( -0.000000000000000000, -0.3543493200069152693, 0.9351131265310292928 ) ) ;
#104296 = LINE ( 'NONE', #134113, #13010 ) ;
#104297 = ORIENTED_EDGE ( 'NONE', *, *, #42945, .F. ) ;
#104298 = ORIENTED_EDGE ( 'NONE', *, *, #50390, .T. ) ;
#104299 = CARTESIAN_POINT ( 'NONE',  ( 92.87500000000000000, 7.950000000000000178, 1.460391307983218535E-15 ) ) ;
#104300 = ORIENTED_EDGE ( 'NONE', *, *, #118546, .T. ) ;
#104301 = ORIENTED_EDGE ( 'NONE', *, *, #69015, .T. ) ;
#104302 = EDGE_CURVE ( 'NONE', #67772, #65560, #124669, .T. ) ;
#104303 = CARTESIAN_POINT ( 'NONE',  ( 19.82816939922339472, 15.75929247661555976, 4.000000000000000000 ) ) ;
#104304 = CARTESIAN_POINT ( 'NONE',  ( 2.999999999999981792, -7.447814304570750998, 5.000000000000000000 ) ) ;
#104305 = AXIS2_PLACEMENT_3D ( 'NONE', #45805, #79166, #79883 ) ;
#104306 = PLANE ( 'NONE',  #12999 ) ;
#104307 = EDGE_LOOP ( 'NONE', ( #140467, #62264, #7382, #62333 ) ) ;
#104308 = DIRECTION ( 'NONE',  ( 0.7071067811865487940, -0.7071067811865463515, 0.000000000000000000 ) ) ;
#104309 = CARTESIAN_POINT ( 'NONE',  ( 21.18398860626899349, 28.73617430169802134, 5.000000000000000000 ) ) ;
#104310 = CARTESIAN_POINT ( 'NONE',  ( 29.99999999999979039, 16.93112307739200872, 4.000000000000000000 ) ) ;
#104311 = CARTESIAN_POINT ( 'NONE',  ( 126.0567959807173679, 4.951256667972520731, -5.496178947977369944 ) ) ;
#104312 = EDGE_CURVE ( 'NONE', #50175, #29061, #81923, .T. ) ;
#104313 = EDGE_CURVE ( 'NONE', #120068, #63590, #58027, .T. ) ;
#104314 = PLANE ( 'NONE',  #116425 ) ;
#104315 = LINE ( 'NONE', #48540, #100658 ) ;
#104316 = CARTESIAN_POINT ( 'NONE',  ( 34.92500000000001847, 1.088194295437629318E-14, -37.00000000000000000 ) ) ;
#104317 = VECTOR ( 'NONE', #124289, 1000.000000000000227 ) ;
#104318 = CARTESIAN_POINT ( 'NONE',  ( 0.000000000000000000, 0.000000000000000000, 5.000000000000000000 ) ) ;
#104319 = CARTESIAN_POINT ( 'NONE',  ( 13.00193056682088688, -22.22500000000000142, 4.500000000000000888 ) ) ;
#104320 = AXIS2_PLACEMENT_3D ( 'NONE', #39951, #95717, #18860 ) ;
#104321 = DIRECTION ( 'NONE',  ( -0.7071067811865487940, 0.7071067811865463515, 0.000000000000000000 ) ) ;
#104322 = FACE_OUTER_BOUND ( 'NONE', #56626, .T. ) ;
#104323 = ORIENTED_EDGE ( 'NONE', *, *, #70717, .F. ) ;
#104324 = ORIENTED_EDGE ( 'NONE', *, *, #92402, .F. ) ;
#104325 = CARTESIAN_POINT ( 'NONE',  ( 115.5004301918981042, -3.055000000000002380, 5.291415217122920289 ) ) ;
#104326 =( BOUNDED_CURVE ( )  B_SPLINE_CURVE ( 3, ( #99536, #124172, #69097, #77820 ),
 .UNSPECIFIED., .F., .T. ) 
 B_SPLINE_CURVE_WITH_KNOTS ( ( 4, 4 ),
 ( 0.6783063634690165156, 0.7469765549618204714 ),
 .UNSPECIFIED. ) 
 CURVE ( )  GEOMETRIC_REPRESENTATION_ITEM ( )  RATIONAL_B_SPLINE_CURVE ( ( 1.000000000000000000, 0.9996070723374664846, 0.9996070723374664846, 1.000000000000000000 ) ) 
 REPRESENTATION_ITEM ( '' )  );
#104327 = ORIENTED_EDGE ( 'NONE', *, *, #136431, .F. ) ;
#104328 = EDGE_CURVE ( 'NONE', #26996, #101519, #102227, .T. ) ;
#104329 = CARTESIAN_POINT ( 'NONE',  ( -29.20710678118633652, 15.75929247661555443, 5.000000000000000000 ) ) ;
#104330 = EDGE_LOOP ( 'NONE', ( #133322, #129194 ) ) ;
#104331 = VECTOR ( 'NONE', #17119, 999.9999999999998863 ) ;
#104332 = EDGE_CURVE ( 'NONE', #21837, #119012, #135331, .T. ) ;
#104333 = DIRECTION ( 'NONE',  ( -0.3543493200069162685, -0.000000000000000000, -0.9351131265310288487 ) ) ;
#104334 = DIRECTION ( 'NONE',  ( 1.000000000000000000, 0.000000000000000000, 0.000000000000000000 ) ) ;
#104335 = MECHANICAL_DESIGN_GEOMETRIC_PRESENTATION_REPRESENTATION (  '', ( #81205 ), #95025 ) ;
#104336 = AXIS2_PLACEMENT_3D ( 'NONE', #89401, #46667, #135086 ) ;
#104337 = CARTESIAN_POINT ( 'NONE',  ( 108.4120968585647944, 5.291415217122921177, -3.054999999999994831 ) ) ;
#104338 = ORIENTED_EDGE ( 'NONE', *, *, #823, .T. ) ;
#104339 = DIRECTION ( 'NONE',  ( 0.7071067811865487940, 0.7071067811865463515, 0.000000000000000000 ) ) ;
#104340 = ORIENTED_EDGE ( 'NONE', *, *, #299, .F. ) ;
#104341 = DIRECTION ( 'NONE',  ( -0.7071067811865486830, -0.7071067811865464625, 0.000000000000000000 ) ) ;
#104342 = AXIS2_PLACEMENT_3D ( 'NONE', #8148, #130700, #9576 ) ;
#104343 = STYLED_ITEM ( 'NONE', ( #91988 ), #128132 ) ;
#104344 = CARTESIAN_POINT ( 'NONE',  ( 25.39999999999999858, 0.000000000000000000, 0.000000000000000000 ) ) ;
#104345 = VECTOR ( 'NONE', #50460, 999.9999999999998863 ) ;
#104346 = VECTOR ( 'NONE', #106646, 999.9999999999998863 ) ;
#104347 = CARTESIAN_POINT ( 'NONE',  ( -15.70679250724064246, 20.25929247661551358, 20.83292124670818524 ) ) ;
#104348 = VECTOR ( 'NONE', #15590, 1000.000000000000114 ) ;
#104349 = EDGE_LOOP ( 'NONE', ( #115993, #9546, #88858, #45402 ) ) ;
#104350 = VERTEX_POINT ( 'NONE', #47175 ) ;
#104351 = VERTEX_POINT ( 'NONE', #126789 ) ;
#104352 = CARTESIAN_POINT ( 'NONE',  ( 0.000000000000000000, -35.14999999999999147, 17.49210858042621908 ) ) ;
#104353 = CARTESIAN_POINT ( 'NONE',  ( 16.17183060077635659, 21.75929247661549937, 4.000000000000000000 ) ) ;
#104354 = CARTESIAN_POINT ( 'NONE',  ( 8.817069808101885897, -2.126176841940956130, 7.934999999999990727 ) ) ;
#104355 = AXIS2_PLACEMENT_3D ( 'NONE', #69421, #90437, #112898 ) ;
#104356 = CARTESIAN_POINT ( 'NONE',  ( 21.14583333333333925, -1.633150327867709528, 6.094999999999979323 ) ) ;
#104357 = EDGE_CURVE ( 'NONE', #79591, #142882, #36247, .T. ) ;
#104358 =( NAMED_UNIT ( * ) SI_UNIT ( $, .STERADIAN. ) SOLID_ANGLE_UNIT ( ) );
#104359 = ORIENTED_EDGE ( 'NONE', *, *, #90142, .T. ) ;
#104360 = ORIENTED_EDGE ( 'NONE', *, *, #108705, .F. ) ;
#104361 = VECTOR ( 'NONE', #37907, 1000.000000000000000 ) ;
#104362 = EDGE_CURVE ( 'NONE', #109128, #42329, #3569, .T. ) ;
#104363 = DIRECTION ( 'NONE',  ( 0.6830127018922180770, -0.6830127018922204085, -0.2588190451025213501 ) ) ;
#104364 = ORIENTED_EDGE ( 'NONE', *, *, #61436, .F. ) ;
#104365 = VERTEX_POINT ( 'NONE', #4983 ) ;
#104366 = VECTOR ( 'NONE', #133902, 1000.000000000000000 ) ;
#104367 = ADVANCED_FACE ( 'NONE', ( #114488 ), #103603, .F. ) ;
#104368 = ADVANCED_FACE ( 'NONE', ( #27474 ), #115896, .F. ) ;
#104369 = PLANE ( 'NONE',  #132779 ) ;
#104370 = AXIS2_PLACEMENT_3D ( 'NONE', #44526, #88726, #90119 ) ;
#104371 = VECTOR ( 'NONE', #926, 1000.000000000000000 ) ;
#104372 = CARTESIAN_POINT ( 'NONE',  ( -17.99451991528748351, 28.92564299267950645, 4.000000000000000000 ) ) ;
#104373 = CARTESIAN_POINT ( 'NONE',  ( 21.88339156388719431, -2.079482862307782121, 4.335713449946893228 ) ) ;
#104374 = VERTEX_POINT ( 'NONE', #6397 ) ;
#104375 = CARTESIAN_POINT ( 'NONE',  ( 26.29289321881326558, 17.25929247661554200, 5.000000000000000000 ) ) ;
#104376 = VECTOR ( 'NONE', #111545, 1000.000000000000000 ) ;
#104377 = LINE ( 'NONE', #5037, #142851 ) ;
#104378 = DIRECTION ( 'NONE',  ( -0.7071067811865486830, -0.7071067811865464625, -0.000000000000000000 ) ) ;
#104379 = VECTOR ( 'NONE', #100758, 1000.000000000000227 ) ;
#104380 = DIRECTION ( 'NONE',  ( 0.7071067811865487940, -0.7071067811865463515, 0.000000000000000000 ) ) ;
#104381 = ORIENTED_EDGE ( 'NONE', *, *, #111476, .T. ) ;
#104382 = CARTESIAN_POINT ( 'NONE',  ( -11.99999999999991296, 20.96639925780204905, 5.000000000000000000 ) ) ;
#104383 = FACE_BOUND ( 'NONE', #51131, .T. ) ;
#104384 = ADVANCED_FACE ( 'NONE', ( #41215 ), #64404, .F. ) ;
#104385 = ORIENTED_EDGE ( 'NONE', *, *, #89799, .T. ) ;
#104386 = DIRECTION ( 'NONE',  ( 0.7071067811865486830, -0.7071067811865464625, -0.000000000000000000 ) ) ;
#104387 = DIRECTION ( 'NONE',  ( 0.7071067811865487940, 0.7071067811865463515, 0.000000000000000000 ) ) ;
#104388 = MECHANICAL_DESIGN_GEOMETRIC_PRESENTATION_REPRESENTATION (  '', ( #32606 ), #58088 ) ;
#104389 = DIRECTION ( 'NONE',  ( -1.000000000000000000, -0.000000000000000000, -0.000000000000000000 ) ) ;
#104390 = EDGE_CURVE ( 'NONE', #29472, #54913, #84729, .T. ) ;
#104391 = ORIENTED_EDGE ( 'NONE', *, *, #107634, .F. ) ;
#104392 = LINE ( 'NONE', #5051, #99076 ) ;
#104393 = VERTEX_POINT ( 'NONE', #62283 ) ;
#104394 = ORIENTED_EDGE ( 'NONE', *, *, #108893, .F. ) ;
#104395 = ORIENTED_EDGE ( 'NONE', *, *, #18443, .T. ) ;
#104396 = CARTESIAN_POINT ( 'NONE',  ( 34.62043019189811588, 3.055000000000001936, -5.291415217122916737 ) ) ;
#104397 = VERTEX_POINT ( 'NONE', #9260 ) ;
#104398 = VECTOR ( 'NONE', #68346, 1000.000000000000000 ) ;
#104399 = EDGE_CURVE ( 'NONE', #109227, #129172, #86167, .T. ) ;
#104400 = FACE_OUTER_BOUND ( 'NONE', #89003, .T. ) ;
#104401 = CARTESIAN_POINT ( 'NONE',  ( 12.35051985313232237, 4.584330080086930965E-16, 0.000000000000000000 ) ) ;
#104402 = CARTESIAN_POINT ( 'NONE',  ( 31.92500000000002203, -21.76999999999999247, -37.00000000000000000 ) ) ;
#104403 = EDGE_LOOP ( 'NONE', ( #120050, #80050, #114286, #42495 ) ) ;
#104404 = CIRCLE ( 'NONE', #136812, 3.000000000000002665 ) ;
#104405 = EDGE_CURVE ( 'NONE', #77276, #110346, #140522, .T. ) ;
#104406 = AXIS2_PLACEMENT_3D ( 'NONE', #73809, #85378, #41168 ) ;
#104407 = CARTESIAN_POINT ( 'NONE',  ( 2.999999999999978240, 2.342191155542454162, -5.001666872980091938 ) ) ;
#104408 = FACE_OUTER_BOUND ( 'NONE', #58800, .T. ) ;
#104409 = CARTESIAN_POINT ( 'NONE',  ( 14.99451991528749595, 28.92564299267948513, 4.000000000000000000 ) ) ;
#104410 = DIRECTION ( 'NONE',  ( -0.7071067811865487940, 0.7071067811865463515, 0.000000000000000000 ) ) ;
#104411 = DIRECTION ( 'NONE',  ( 0.6830127018922181881, 0.6830127018922202975, -0.2588190451025214056 ) ) ;
#104412 = ORIENTED_EDGE ( 'NONE', *, *, #94025, .F. ) ;
#104413 = ORIENTED_EDGE ( 'NONE', *, *, #52476, .F. ) ;
#104415 = ORIENTED_EDGE ( 'NONE', *, *, #8085, .T. ) ;
#104414 = EDGE_CURVE ( 'NONE', #107388, #108114, #128252, .T. ) ;
#104416 = VECTOR ( 'NONE', #54213, 1000.000000000000000 ) ;
#104417 = ORIENTED_EDGE ( 'NONE', *, *, #9233, .T. ) ;
#104418 = VERTEX_POINT ( 'NONE', #18733 ) ;
#104419 = ORIENTED_EDGE ( 'NONE', *, *, #28610, .T. ) ;
#104420 = FACE_OUTER_BOUND ( 'NONE', #16614, .T. ) ;
#104421 = DIRECTION ( 'NONE',  ( 0.7071067811865487940, 0.7071067811865463515, -0.000000000000000000 ) ) ;
#104422 = ORIENTED_EDGE ( 'NONE', *, *, #26831, .T. ) ;
#104423 = EDGE_CURVE ( 'NONE', #130424, #34219, #85420, .T. ) ;
#104424 = DIRECTION ( 'NONE',  ( -0.7071067811865486830, -0.7071067811865464625, 0.000000000000000000 ) ) ;
#104425 = VECTOR ( 'NONE', #103601, 1000.000000000000000 ) ;
#104426 = ORIENTED_EDGE ( 'NONE', *, *, #131926, .F. ) ;
#104427 = CARTESIAN_POINT ( 'NONE',  ( 33.48921356237309510, -27.52281430457078670, 5.000000000000000000 ) ) ;
#104428 = EDGE_CURVE ( 'NONE', #135515, #96824, #137245, .T. ) ;
#104429 = PLANE ( 'NONE',  #119082 ) ;
#104430 = CARTESIAN_POINT ( 'NONE',  ( 1.379569808101885897, 3.967499999999998916, 6.871911579029510442 ) ) ;
#104431 = ORIENTED_EDGE ( 'NONE', *, *, #5839, .F. ) ;
#104433 = CARTESIAN_POINT ( 'NONE',  ( 8.994519915287490619, 28.92564299267944250, 4.000000000000000000 ) ) ;
#104432 = CARTESIAN_POINT ( 'NONE',  ( 103.1620968585647802, -5.291415217122919401, 3.054999999999998384 ) ) ;
#104434 = DIRECTION ( 'NONE',  ( 0.6830127018922180770, -0.6830127018922204085, -0.2588190451025213501 ) ) ;
#104435 = DIRECTION ( 'NONE',  ( 0.7071067811865486830, -0.7071067811865464625, -0.000000000000000000 ) ) ;
#104436 = VERTEX_POINT ( 'NONE', #20159 ) ;
#104437 = EDGE_LOOP ( 'NONE', ( #128669, #112720, #35844, #14072 ) ) ;
#104438 = PLANE ( 'NONE',  #72789 ) ;
#104439 = ORIENTED_EDGE ( 'NONE', *, *, #7937, .T. ) ;
#104440 = CARTESIAN_POINT ( 'NONE',  ( 42.48921356237308800, -27.52281430457085065, 5.000000000000000000 ) ) ;
#104441 = LINE ( 'NONE', #105165, #136623 ) ;
#104442 = PLANE ( 'NONE',  #70608 ) ;
#104443 = CIRCLE ( 'NONE', #132223, 2.999999999999999112 ) ;
#104444 = LINE ( 'NONE', #24755, #46981 ) ;
#104445 = CARTESIAN_POINT ( 'NONE',  ( 183.3316408629057435, -52.14999999999999147, -41.64500000000001023 ) ) ;
#104446 = ORIENTED_EDGE ( 'NONE', *, *, #104734, .F. ) ;
#104447 = VECTOR ( 'NONE', #119208, 1000.000000000000000 ) ;
#104448 = CARTESIAN_POINT ( 'NONE',  ( -28.64175702458843276, 15.75929247661555799, 19.34181609438706317 ) ) ;
#104449 = VECTOR ( 'NONE', #12895, 1000.000000000000000 ) ;
#104450 = DIRECTION ( 'NONE',  ( -0.000000000000000000, -1.000000000000000000, -0.000000000000000000 ) ) ;
#104451 = CARTESIAN_POINT ( 'NONE',  ( 12.08840764549667668, -3.851859888774471706E-31, 2.500000000000001332 ) ) ;
#104452 = VERTEX_POINT ( 'NONE', #107185 ) ;
#104453 = DIRECTION ( 'NONE',  ( -0.000000000000000000, -0.3543493200069152693, 0.9351131265310292928 ) ) ;
#104454 = VECTOR ( 'NONE', #15484, 1000.000000000000000 ) ;
#104455 = VECTOR ( 'NONE', #131833, 1000.000000000000000 ) ;
#104456 = LINE ( 'NONE', #91467, #130336 ) ;
#104458 = VERTEX_POINT ( 'NONE', #7860 ) ;
#104457 = VECTOR ( 'NONE', #97271, 1000.000000000000000 ) ;
#104460 = VERTEX_POINT ( 'NONE', #75302 ) ;
#104459 = CARTESIAN_POINT ( 'NONE',  ( 0.1839886062690032631, 28.73617430169787568, 5.000000000000000000 ) ) ;
#104461 = ORIENTED_EDGE ( 'NONE', *, *, #134261, .T. ) ;
#104462 = CARTESIAN_POINT ( 'NONE',  ( 21.18398860626899349, 28.73617430169802134, 5.000000000000000000 ) ) ;
#104463 = VECTOR ( 'NONE', #141636, 1000.000000000000000 ) ;
#104464 = FACE_OUTER_BOUND ( 'NONE', #46455, .T. ) ;
#104465 = ORIENTED_EDGE ( 'NONE', *, *, #88718, .T. ) ;
#104466 = DIRECTION ( 'NONE',  ( -1.000000000000000000, -0.000000000000000000, -0.000000000000000000 ) ) ;
#104467 = DIRECTION ( 'NONE',  ( 0.7071067811865487940, 0.7071067811865463515, 0.000000000000000000 ) ) ;
#104468 =( NAMED_UNIT ( * ) SI_UNIT ( $, .STERADIAN. ) SOLID_ANGLE_UNIT ( ) );
#104469 = ORIENTED_EDGE ( 'NONE', *, *, #1737, .F. ) ;
#104470 = VECTOR ( 'NONE', #106489, 1000.000000000000000 ) ;
#104471 = CARTESIAN_POINT ( 'NONE',  ( -12.69999999999998153, 3.061616997868383634E-16, -2.500000000000000444 ) ) ;
#104472 = DIRECTION ( 'NONE',  ( 1.000000000000000000, 0.000000000000000000, 0.000000000000000000 ) ) ;
#104473 = EDGE_CURVE ( 'NONE', #85340, #63769, #28218, .T. ) ;
#104474 = DIRECTION ( 'NONE',  ( 0.7071067811865487940, 0.7071067811865463515, 0.000000000000000000 ) ) ;
#104475 = DIRECTION ( 'NONE',  ( -0.6830127018922180770, -0.6830127018922202975, -0.2588190451025213501 ) ) ;
#104476 = DIRECTION ( 'NONE',  ( -1.000000000000000000, -0.000000000000000000, -0.000000000000000000 ) ) ;
#104477 = DIRECTION ( 'NONE',  ( 1.318980745116185161E-16, -1.000000000000000000, 0.000000000000000000 ) ) ;
#104478 = DIRECTION ( 'NONE',  ( 0.6830127018922180770, -0.6830127018922204085, -0.2588190451025213501 ) ) ;
#104479 = CARTESIAN_POINT ( 'NONE',  ( 28.95419371712955225, 6.884901960086283523, 3.975000000000002753 ) ) ;
#104480 = CARTESIAN_POINT ( 'NONE',  ( -75.48921356237309510, -27.52281430457107803, 5.000000000000000000 ) ) ;
#104481 = ORIENTED_EDGE ( 'NONE', *, *, #74417, .F. ) ;
#104482 = AXIS2_PLACEMENT_3D ( 'NONE', #94927, #5767, #94222 ) ;
#104483 = ORIENTED_EDGE ( 'NONE', *, *, #57122, .T. ) ;
#104484 = ORIENTED_EDGE ( 'NONE', *, *, #105643, .T. ) ;
#104485 = CARTESIAN_POINT ( 'NONE',  ( 120.1458333333333286, 2.130196079827431976, -7.949999999999999289 ) ) ;
#104486 = VECTOR ( 'NONE', #143412, 1000.000000000000000 ) ;
#104487 = ORIENTED_EDGE ( 'NONE', *, *, #128187, .F. ) ;
#104488 = ORIENTED_EDGE ( 'NONE', *, *, #135180, .F. ) ;
#104489 = EDGE_CURVE ( 'NONE', #102767, #50434, #51405, .T. ) ;
#104490 = AXIS2_PLACEMENT_3D ( 'NONE', #51670, #87142, #140784 ) ;
#104491 = EDGE_LOOP ( 'NONE', ( #54599, #46239, #63454, #29840 ) ) ;
#104492 = CYLINDRICAL_SURFACE ( 'NONE', #52492, 2.500000000000000000 ) ;
#104493 = LINE ( 'NONE', #5870, #71817 ) ;
#104494 = COLOUR_RGB ( '', 0.72549020, 0.75294118, 0.79215686) ;
#104495 = ORIENTED_EDGE ( 'NONE', *, *, #72936, .T. ) ;
#104496 = CARTESIAN_POINT ( 'NONE',  ( -4.251544128675727841, -11.24070752338416845, 10.39518518046010342 ) ) ;
#104497 = DIRECTION ( 'NONE',  ( -0.7071067811865486830, 0.7071067811865464625, 0.000000000000000000 ) ) ;
#104498 = CARTESIAN_POINT ( 'NONE',  ( 15.52000000000000135, 9.521314400968980422E-16, 0.000000000000000000 ) ) ;
#104499 = CARTESIAN_POINT ( 'NONE',  ( 116.9587635252314470, 0.000000000000000000, -6.110000000000001208 ) ) ;
#104500 = ADVANCED_FACE ( 'NONE', ( #17326 ), #19471, .T. ) ;
#104501 = VECTOR ( 'NONE', #80611, 1000.000000000000000 ) ;
#104502 = ORIENTED_EDGE ( 'NONE', *, *, #130310, .T. ) ;
#104503 = DIRECTION ( 'NONE',  ( -0.000000000000000000, 0.3543493200069153248, 0.9351131265310292928 ) ) ;
#104504 = DIRECTION ( 'NONE',  ( -0.6830127018922180770, -0.6830127018922204085, -0.2588190451025213501 ) ) ;
#104505 = EDGE_CURVE ( 'NONE', #22185, #10056, #52099, .T. ) ;
#104506 = LINE ( 'NONE', #135723, #35702 ) ;
#104507 = CARTESIAN_POINT ( 'NONE',  ( -18.18398860626898994, 28.73617430169800002, 5.000000000000000000 ) ) ;
#104508 = FACE_OUTER_BOUND ( 'NONE', #126498, .T. ) ;
#104509 = DIRECTION ( 'NONE',  ( 0.6830127018922181881, 0.6830127018922202975, -0.2588190451025214056 ) ) ;
#104510 = ADVANCED_FACE ( 'NONE', ( #117330 ), #106440, .T. ) ;
#104511 = CARTESIAN_POINT ( 'NONE',  ( 34.78752705046288440, 0.000000000000000000, -7.949999999999998401 ) ) ;
#104512 = DIRECTION ( 'NONE',  ( 0.000000000000000000, -1.000000000000000000, 0.000000000000000000 ) ) ;
#104513 = CARTESIAN_POINT ( 'NONE',  ( 184.1500000000000057, -14.29000000000013593, -12.70000000000045404 ) ) ;
#104514 = EDGE_LOOP ( 'NONE', ( #6363, #123135, #44031, #115159 ) ) ;
#104515 = ORIENTED_EDGE ( 'NONE', *, *, #32423, .T. ) ;
#104516 = CARTESIAN_POINT ( 'NONE',  ( 40.08333333333332860, 6.884901960086290629, -3.974999999999994316 ) ) ;
#104517 = ORIENTED_EDGE ( 'NONE', *, *, #142595, .F. ) ;
#104518 = ORIENTED_EDGE ( 'NONE', *, *, #124575, .T. ) ;
#104519 = ADVANCED_FACE ( 'NONE', ( #128943 ), #29614, .F. ) ;
#104520 = CARTESIAN_POINT ( 'NONE',  ( -7.499999999999942268, -10.91253812416064406, 4.000000000000000000 ) ) ;
#104521 = VECTOR ( 'NONE', #95793, 1000.000000000000000 ) ;
#104522 = LINE ( 'NONE', #50870, #33980 ) ;
#104523 = ORIENTED_EDGE ( 'NONE', *, *, #127989, .F. ) ;
#104524 = AXIS2_PLACEMENT_3D ( 'NONE', #121932, #102370, #23339 ) ;
#104525 = PLANE ( 'NONE',  #10915 ) ;
#104526 = PLANE ( 'NONE',  #2830 ) ;
#104527 = ADVANCED_FACE ( 'NONE', ( #118774 ), #107874, .F. ) ;
#104528 = CARTESIAN_POINT ( 'NONE',  ( -42.29974487139158157, -27.71228299555235708, 4.000000000000000000 ) ) ;
#104529 = CARTESIAN_POINT ( 'NONE',  ( 28.14626352523143638, -4.472830434245840259, 4.472830434245839371 ) ) ;
#104530 = ORIENTED_EDGE ( 'NONE', *, *, #53590, .F. ) ;
#104531 = DIRECTION ( 'NONE',  ( -0.000000000000000000, -0.3543493200069152693, 0.9351131265310292928 ) ) ;
#104532 = ORIENTED_EDGE ( 'NONE', *, *, #121780, .T. ) ;
#104533 = AXIS2_PLACEMENT_3D ( 'NONE', #53675, #142118, #140649 ) ;
#104534 = DIRECTION ( 'NONE',  ( 0.7071067811865487940, 0.7071067811865463515, 0.000000000000000000 ) ) ;
#104535 = EDGE_CURVE ( 'NONE', #16006, #17089, #100616, .T. ) ;
#104536 = CARTESIAN_POINT ( 'NONE',  ( -16.99806943317890173, -22.22500000000000142, 4.500000000000000888 ) ) ;
#104537 = PRESENTATION_STYLE_ASSIGNMENT (( #80670 ) ) ;
#104538 = DIRECTION ( 'NONE',  ( 0.6830127018922181881, 0.6830127018922202975, -0.2588190451025214056 ) ) ;
#104539 = ORIENTED_EDGE ( 'NONE', *, *, #73746, .F. ) ;
#104540 = CARTESIAN_POINT ( 'NONE',  ( 52.79209685856476852, -5.291415217122921177, 3.054999999999999272 ) ) ;
#104541 = ORIENTED_EDGE ( 'NONE', *, *, #122732, .T. ) ;
#104542 = PLANE ( 'NONE',  #17025 ) ;
#104543 = CARTESIAN_POINT ( 'NONE',  ( -0.7071067811865398012, 11.25929247661561305, 5.000000000000000000 ) ) ;
#104544 = DIRECTION ( 'NONE',  ( 0.000000000000000000, -1.000000000000000000, 0.000000000000000000 ) ) ;
#104545 = EDGE_CURVE ( 'NONE', #16928, #6491, #142682, .T. ) ;
#104546 = DIRECTION ( 'NONE',  ( 0.7071067811865486830, -0.7071067811865464625, -0.000000000000000000 ) ) ;
#104547 = VECTOR ( 'NONE', #116287, 1000.000000000000000 ) ;
#104548 = EDGE_CURVE ( 'NONE', #137243, #127621, #78152, .T. ) ;
#104549 = CARTESIAN_POINT ( 'NONE',  ( 50.37043019189811588, -3.055000000000001492, 5.291415217122917625 ) ) ;
#104550 = ORIENTED_EDGE ( 'NONE', *, *, #55334, .F. ) ;
#104551 = CARTESIAN_POINT ( 'NONE',  ( 124.3750000000000000, 7.950000000000000178, 1.460391307983218535E-15 ) ) ;
#104552 = EDGE_CURVE ( 'NONE', #117065, #83522, #49856, .T. ) ;
#104553 = CARTESIAN_POINT ( 'NONE',  ( -12.48921356237309155, -27.52281430457064104, 5.000000000000000000 ) ) ;
#104554 = ORIENTED_EDGE ( 'NONE', *, *, #54596, .T. ) ;
#104555 = ORIENTED_EDGE ( 'NONE', *, *, #89446, .F. ) ;
#104556 = FACE_OUTER_BOUND ( 'NONE', #112197, .T. ) ;
#104557 = VECTOR ( 'NONE', #80944, 1000.000000000000000 ) ;
#104558 = VECTOR ( 'NONE', #20439, 1000.000000000000000 ) ;
#104559 = ORIENTED_EDGE ( 'NONE', *, *, #36333, .F. ) ;
#104560 = EDGE_CURVE ( 'NONE', #128957, #70018, #99144, .T. ) ;
#104561 = ADVANCED_FACE ( 'NONE', ( #78877 ), #133947, .F. ) ;
#104562 = CARTESIAN_POINT ( 'NONE',  ( -12.69999999999998153, 0.000000000000000000, 0.000000000000000000 ) ) ;
#104563 = EDGE_LOOP ( 'NONE', ( #5432, #137959, #69203, #9355 ) ) ;
#104564 = CARTESIAN_POINT ( 'NONE',  ( 16.44013779566152778, -2.499999999999996447, 0.000000000000000000 ) ) ;
#104565 = VECTOR ( 'NONE', #125894, 1000.000000000000000 ) ;
#104566 = VECTOR ( 'NONE', #108201, 1000.000000000000000 ) ;
#104567 = AXIS2_PLACEMENT_3D ( 'NONE', #132700, #25304, #134095 ) ;
#104568 = VECTOR ( 'NONE', #77313, 1000.000000000000000 ) ;
#104569 = EDGE_CURVE ( 'NONE', #41530, #50028, #33936, .T. ) ;
#104570 = VECTOR ( 'NONE', #138993, 1000.000000000000000 ) ;
#104571 = CARTESIAN_POINT ( 'NONE',  ( 57.48921356237308800, -27.52281430457095368, 5.000000000000000000 ) ) ;
#104572 = FACE_BOUND ( 'NONE', #30333, .T. ) ;
#104573 = EDGE_CURVE ( 'NONE', #12969, #17742, #44097, .T. ) ;
#104574 = CARTESIAN_POINT ( 'NONE',  ( 48.25000000000000000, -9.735942053221458872E-16, 7.950000000000000178 ) ) ;
#104575 = FILL_AREA_STYLE ('',( #125634 ) ) ;
#104576 = ORIENTED_EDGE ( 'NONE', *, *, #17475, .T. ) ;
#104578 = DIRECTION ( 'NONE',  ( -1.000000000000000000, -1.224606353822377258E-16, -0.000000000000000000 ) ) ;
#104577 = AXIS2_PLACEMENT_3D ( 'NONE', #26280, #37886, #70542 ) ;
#104580 = VERTEX_POINT ( 'NONE', #120171 ) ;
#104579 = DIRECTION ( 'NONE',  ( -0.9425785261922232650, 0.3339846133601012124, 0.000000000000000000 ) ) ;
#104581 = CARTESIAN_POINT ( 'NONE',  ( 30.48921356237309510, -27.52281430457076894, 5.000000000000000000 ) ) ;
#104582 = ORIENTED_EDGE ( 'NONE', *, *, #124857, .F. ) ;
#104583 = VERTEX_POINT ( 'NONE', #131096 ) ;
#104584 = CARTESIAN_POINT ( 'NONE',  ( 63.34959685856478018, 6.109999999999996767, 1.637169565754163836 ) ) ;
#104585 = ORIENTED_EDGE ( 'NONE', *, *, #141111, .T. ) ;
#104586 = EDGE_CURVE ( 'NONE', #89926, #105060, #54975, .T. ) ;
#104587 = PLANE ( 'NONE',  #132151 ) ;
#104588 = FACE_OUTER_BOUND ( 'NONE', #19720, .T. ) ;
#104589 = EDGE_LOOP ( 'NONE', ( #17671, #126573, #120812, #131825 ) ) ;
#104590 = EDGE_CURVE ( 'NONE', #107568, #31251, #97747, .T. ) ;
#104591 = CIRCLE ( 'NONE', #97652, 2.500000000000000444 ) ;
#104592 = VECTOR ( 'NONE', #89574, 1000.000000000000227 ) ;
#104593 = LINE ( 'NONE', #5257, #40933 ) ;
#104594 = CARTESIAN_POINT ( 'NONE',  ( 25.49999999999982592, -17.56887692260762535, 4.000000000000000000 ) ) ;
#104595 = LINE ( 'NONE', #40094, #110657 ) ;
#104596 = CIRCLE ( 'NONE', #76906, 2.055000000000000604 ) ;
#104597 = CARTESIAN_POINT ( 'NONE',  ( 31.49999999999979039, -17.94781430457064531, 5.000000000000000000 ) ) ;
#104598 = EDGE_LOOP ( 'NONE', ( #105043, #131596, #69432, #125497 ) ) ;
#104599 = EDGE_LOOP ( 'NONE', ( #17885, #35274, #110000, #128321 ) ) ;
#104600 = VECTOR ( 'NONE', #140027, 1000.000000000000227 ) ;
#104601 = FACE_OUTER_BOUND ( 'NONE', #140113, .T. ) ;
#104602 = CARTESIAN_POINT ( 'NONE',  ( 26.99999999999981526, 20.96639925780204905, 5.000000000000000000 ) ) ;
#104603 = ORIENTED_EDGE ( 'NONE', *, *, #116514, .T. ) ;
#104604 = VERTEX_POINT ( 'NONE', #133257 ) ;
#104605 = ORIENTED_EDGE ( 'NONE', *, *, #117775, .T. ) ;
#104606 = FACE_OUTER_BOUND ( 'NONE', #102885, .T. ) ;
#104607 = LINE ( 'NONE', #4512, #122562 ) ;
#104608 = ORIENTED_EDGE ( 'NONE', *, *, #33062, .T. ) ;
#104609 = PLANE ( 'NONE',  #138916 ) ;
#104610 = COLOUR_RGB ( '', 0.66274510, 0.83137255, 0.94901961) ;
#104611 = ADVANCED_FACE ( 'NONE', ( #88316 ), #123085, .F. ) ;
#104612 = CARTESIAN_POINT ( 'NONE',  ( 2.510786437626908008, -27.52281430457053446, 5.000000000000000000 ) ) ;
#104613 = CARTESIAN_POINT ( 'NONE',  ( 10.42123647476855375, -9.717572351234235426E-16, -7.934999999999990727 ) ) ;
#104614 = PLANE ( 'NONE',  #135213 ) ;
#104615 = ORIENTED_EDGE ( 'NONE', *, *, #124511, .F. ) ;
#104616 = CARTESIAN_POINT ( 'NONE',  ( 6.516654386410396071, 22.22500000000000142, 4.500000000000000888 ) ) ;
#104617 = DIRECTION ( 'NONE',  ( 0.7071067811865487940, 0.7071067811865463515, 0.000000000000000000 ) ) ;
#104618 = CIRCLE ( 'NONE', #88506, 2.055000000000001048 ) ;
#104619 = CARTESIAN_POINT ( 'NONE',  ( 25.37500000000000000, -6.094999999999989981, 3.732111120401553285E-16 ) ) ;
#104621 = EDGE_LOOP ( 'NONE', ( #15350, #131333, #57056, #33813 ) ) ;
#104620 = LINE ( 'NONE', #138702, #105095 ) ;
#104623 = CIRCLE ( 'NONE', #81481, 2.247899999999996901 ) ;
#104622 = DIRECTION ( 'NONE',  ( 0.000000000000000000, 1.000000000000000000, 0.000000000000000000 ) ) ;
#104624 = EDGE_LOOP ( 'NONE', ( #140757, #3623, #61420, #130527, #99252 ) ) ;
#104625 = DIRECTION ( 'NONE',  ( -0.000000000000000000, 0.3543493200069153248, 0.9351131265310292928 ) ) ;
#104626 = CARTESIAN_POINT ( 'NONE',  ( -3.299744871391591339, -27.71228299555208352, 4.000000000000000000 ) ) ;
#104627 = FACE_OUTER_BOUND ( 'NONE', #121072, .T. ) ;
#104628 = ORIENTED_EDGE ( 'NONE', *, *, #85426, .T. ) ;
#104629 = LINE ( 'NONE', #114768, #47258 ) ;
#104630 = CARTESIAN_POINT ( 'NONE',  ( 125.5000000000000000, -3.441786896390352624, 7.166352137582667758 ) ) ;
#104631 = DIRECTION ( 'NONE',  ( -0.6830127018922181881, 0.6830127018922202975, -0.2588190451025214056 ) ) ;
#104632 = EDGE_LOOP ( 'NONE', ( #21811, #132023, #13401, #63312 ) ) ;
#104633 = LINE ( 'NONE', #93767, #9124 ) ;
#104634 = CARTESIAN_POINT ( 'NONE',  ( 61.46640106136302961, -57.15000000000008384, -34.92499999999998295 ) ) ;
#104635 =( BOUNDED_CURVE ( )  B_SPLINE_CURVE ( 2, ( #113121, #126846, #68948, #126164, #113844, #13791, #58086, #26835, #25394, #80530, #93531, #124725, #102287 ),
 .UNSPECIFIED., .F., .T. ) 
 B_SPLINE_CURVE_WITH_KNOTS ( ( 3, 2, 2, 2, 2, 2, 3 ),
 ( 0.6166666666666666963, 0.6194444444444444642, 0.6222222222222222321, 0.6250000000000000000, 0.6277777777777777679, 0.6305555555555555358, 0.6333333333333333037 ),
 .UNSPECIFIED. ) 
 CURVE ( )  GEOMETRIC_REPRESENTATION_ITEM ( )  RATIONAL_B_SPLINE_CURVE ( ( 1.000000000000000000, 0.9659258262890683122, 1.000000000000000000, 0.9659258262890683122, 1.000000000000000000, 0.9659258262890683122, 1.000000000000000000, 0.9659258262890683122, 1.000000000000000000, 0.9659258262890683122, 1.000000000000000000, 0.9659258262890683122, 1.000000000000000000 ) ) 
 REPRESENTATION_ITEM ( '' )  );
#104636 = CARTESIAN_POINT ( 'NONE',  ( 21.92080628287044064, 3.047499999999997655, 5.278424836066143655 ) ) ;
#104637 = DIRECTION ( 'NONE',  ( -0.3543493200069162685, -0.000000000000000000, -0.9351131265310288487 ) ) ;
#104638 = LINE ( 'NONE', #26383, #57695 ) ;
#104639 = ORIENTED_EDGE ( 'NONE', *, *, #66597, .T. ) ;
#104640 = VERTEX_POINT ( 'NONE', #32506 ) ;
#104641 = VECTOR ( 'NONE', #122484, 1000.000000000000000 ) ;
#104642 = LINE ( 'NONE', #48859, #142086 ) ;
#104643 = CARTESIAN_POINT ( 'NONE',  ( 1.437069808101885782, 2.126176841940952134, -7.934999999999993392 ) ) ;
#104644 = CARTESIAN_POINT ( 'NONE',  ( -51.18398860626899705, 28.73617430169823095, 5.000000000000000000 ) ) ;
#104645 = CARTESIAN_POINT ( 'NONE',  ( 0.000000000000000000, 0.000000000000000000, 5.000000000000000000 ) ) ;
#104646 = LINE ( 'NONE', #5319, #113159 ) ;
#104647 = LINE ( 'NONE', #69189, #51380 ) ;
#104648 = VERTEX_POINT ( 'NONE', #65147 ) ;
#104649 = DIRECTION ( 'NONE',  ( 0.3543493200069162685, -0.000000000000000000, -0.9351131265310288487 ) ) ;
#104650 = CARTESIAN_POINT ( 'NONE',  ( -75.48921356237309510, -27.52281430457107803, 5.000000000000000000 ) ) ;
#104651 = AXIS2_PLACEMENT_3D ( 'NONE', #141578, #100906, #133556 ) ;
#104652 = AXIS2_PLACEMENT_3D ( 'NONE', #74698, #118879, #11516 ) ;
#104653 = VECTOR ( 'NONE', #8573, 1000.000000000000000 ) ;
#104654 = CARTESIAN_POINT ( 'NONE',  ( 45.12043019189810877, 3.055000000000002380, -5.291415217122917625 ) ) ;
#104655 = DIRECTION ( 'NONE',  ( 1.000000000000000000, 0.000000000000000000, -0.000000000000000000 ) ) ;
#104656 = VECTOR ( 'NONE', #99406, 1000.000000000000000 ) ;
#104657 = AXIS2_PLACEMENT_3D ( 'NONE', #5935, #137219, #136482 ) ;
#104658 = VERTEX_POINT ( 'NONE', #66559 ) ;
#104659 = FACE_OUTER_BOUND ( 'NONE', #83375, .T. ) ;
#104660 = ORIENTED_EDGE ( 'NONE', *, *, #123139, .F. ) ;
#104661 = EDGE_CURVE ( 'NONE', #93122, #3321, #23003, .T. ) ;
#104662 = ORIENTED_EDGE ( 'NONE', *, *, #48932, .F. ) ;
#104663 = AXIS2_PLACEMENT_3D ( 'NONE', #33596, #76365, #30732 ) ;
#104664 = VECTOR ( 'NONE', #10670, 1000.000000000000000 ) ;
#104665 = CARTESIAN_POINT ( 'NONE',  ( -36.18398860626899705, 28.73617430169812437, 5.000000000000000000 ) ) ;
#104666 = CIRCLE ( 'NONE', #132454, 2.500000000000000444 ) ;
#104667 = FACE_OUTER_BOUND ( 'NONE', #66973, .T. ) ;
#104668 = ADVANCED_FACE ( 'NONE', ( #21621 ), #128491, .T. ) ;
#104669 = LINE ( 'NONE', #103930, #106352 ) ;
#104670 = CARTESIAN_POINT ( 'NONE',  ( -34.92500000000001137, -16.19990548397262842, 4.759050581649339584 ) ) ;
#104671 = CARTESIAN_POINT ( 'NONE',  ( 15.96626304157554266, 2.055000000000001048, 0.000000000000000000 ) ) ;
#104672 = ADVANCED_FACE ( 'NONE', ( #98458 ), #43376, .F. ) ;
#104673 = ADVANCED_FACE ( 'NONE', ( #557 ), #11411, .F. ) ;
#104674 = ORIENTED_EDGE ( 'NONE', *, *, #91289, .F. ) ;
#104675 = CARTESIAN_POINT ( 'NONE',  ( 75.48921356237309510, -27.52281430457107803, 5.000000000000000000 ) ) ;
#104676 = LINE ( 'NONE', #5343, #83914 ) ;
#104677 = DIRECTION ( 'NONE',  ( -0.000000000000000000, 0.000000000000000000, 1.000000000000000000 ) ) ;
#104678 = CARTESIAN_POINT ( 'NONE',  ( -27.70710678118635073, 11.25929247661560595, 5.000000000000000000 ) ) ;
#104679 = CARTESIAN_POINT ( 'NONE',  ( -0.2997448713915885632, -27.71228299555206220, 4.000000000000000000 ) ) ;
#104680 = EDGE_CURVE ( 'NONE', #34178, #119435, #86790, .T. ) ;
#104682 = ADVANCED_FACE ( 'NONE', ( #70854 ), #46261, .T. ) ;
#104681 = CARTESIAN_POINT ( 'NONE',  ( 62.64169371712956291, -2.130196079827424871, -7.949999999999999289 ) ) ;
#104683 = FACE_OUTER_BOUND ( 'NONE', #31521, .T. ) ;
#104684 = VERTEX_POINT ( 'NONE', #102035 ) ;
#104685 = EDGE_LOOP ( 'NONE', ( #114418, #39179, #92625, #92948 ) ) ;
#104686 = CARTESIAN_POINT ( 'NONE',  ( 61.66666666666666430, 6.884901960086285300, 3.975000000000003642 ) ) ;
#104687 = DIRECTION ( 'NONE',  ( -0.6830127018922180770, -0.6830127018922204085, -0.2588190451025213501 ) ) ;
#104688 = EDGE_CURVE ( 'NONE', #66020, #76576, #23316, .T. ) ;
#104689 = CARTESIAN_POINT ( 'NONE',  ( 45.18398860626900415, 28.73617430169818832, 5.000000000000000000 ) ) ;
#104690 = DIRECTION ( 'NONE',  ( 0.7071067811865486830, -0.7071067811865464625, -0.000000000000000000 ) ) ;
#104691 = ORIENTED_EDGE ( 'NONE', *, *, #70704, .T. ) ;
#104692 = PRESENTATION_LAYER_ASSIGNMENT (  '', '', ( #51527 ) ) ;
#104693 = PLANE ( 'NONE',  #53779 ) ;
#104694 = EDGE_CURVE ( 'NONE', #93111, #44264, #14302, .T. ) ;
#104695 = VECTOR ( 'NONE', #86400, 1000.000000000000000 ) ;
#104696 = DIRECTION ( 'NONE',  ( -0.7071067811865487940, 0.7071067811865463515, -0.000000000000000000 ) ) ;
#104697 = CARTESIAN_POINT ( 'NONE',  ( 53.22959685856475431, -6.110000000000000320, -1.637169565754161393 ) ) ;
#104698 = AXIS2_PLACEMENT_3D ( 'NONE', #34739, #21710, #78978 ) ;
#104699 = DIRECTION ( 'NONE',  ( 0.7071067811865486830, -0.7071067811865464625, -0.000000000000000000 ) ) ;
#104700 = VERTEX_POINT ( 'NONE', #126614 ) ;
#104701 = ORIENTED_EDGE ( 'NONE', *, *, #63023, .T. ) ;
#104702 = VECTOR ( 'NONE', #122334, 1000.000000000000227 ) ;
#104703 = DIRECTION ( 'NONE',  ( 1.000000000000000000, 0.000000000000000000, 0.000000000000000000 ) ) ;
#104704 = DIRECTION ( 'NONE',  ( -0.7071067811865487940, 0.7071067811865463515, -0.000000000000000000 ) ) ;
#104705 = FACE_OUTER_BOUND ( 'NONE', #59433, .T. ) ;
#104706 = DIRECTION ( 'NONE',  ( 0.7071067811865487940, 0.7071067811865463515, -0.000000000000000000 ) ) ;
#104707 = LINE ( 'NONE', #5374, #60451 ) ;
#104709 = ORIENTED_EDGE ( 'NONE', *, *, #12234, .F. ) ;
#104708 = CARTESIAN_POINT ( 'NONE',  ( 4.589909354801656072, 9.759292476615625489, 11.28811694763779627 ) ) ;
#104710 = CARTESIAN_POINT ( 'NONE',  ( 1.499999999999987566, -8.568876922607726598, 4.000000000000000000 ) ) ;
#104711 = DIRECTION ( 'NONE',  ( 0.6830127018922181881, 0.6830127018922202975, -0.2588190451025214056 ) ) ;
#104712 = FACE_OUTER_BOUND ( 'NONE', #68782, .T. ) ;
#104713 = EDGE_CURVE ( 'NONE', #83589, #130990, #103021, .T. ) ;
#104714 = MECHANICAL_DESIGN_GEOMETRIC_PRESENTATION_REPRESENTATION (  '', ( #5124 ), #116307 ) ;
#104715 = LINE ( 'NONE', #17003, #64634 ) ;
#104716 = VERTEX_POINT ( 'NONE', #69425 ) ;
#104717 = ORIENTED_EDGE ( 'NONE', *, *, #22672, .F. ) ;
#104718 = CARTESIAN_POINT ( 'NONE',  ( -39.18398860626899705, 28.73617430169814568, 5.000000000000000000 ) ) ;
#104719 = DIRECTION ( 'NONE',  ( 0.000000000000000000, -0.000000000000000000, -1.000000000000000000 ) ) ;
#104720 = VECTOR ( 'NONE', #25739, 1000.000000000000000 ) ;
#104721 = EDGE_CURVE ( 'NONE', #59049, #45425, #37509, .T. ) ;
#104722 = DIRECTION ( 'NONE',  ( -0.5735764363510501562, 0.8191520442889890230, 1.003171929053521419E-16 ) ) ;
#104723 = CARTESIAN_POINT ( 'NONE',  ( -25.49999999999982592, -20.56887692260760048, 4.000000000000000000 ) ) ;
#104724 = ORIENTED_EDGE ( 'NONE', *, *, #27255, .T. ) ;
#104725 = EDGE_LOOP ( 'NONE', ( #88757, #47247, #78973, #81510 ) ) ;
#104726 = VECTOR ( 'NONE', #92005, 1000.000000000000000 ) ;
#104727 = CARTESIAN_POINT ( 'NONE',  ( -12.69999999999998153, 0.000000000000000000, 0.000000000000000000 ) ) ;
#104728 = CARTESIAN_POINT ( 'NONE',  ( -17.99999999999986855, -4.447814304570788302, 5.000000000000000000 ) ) ;
#104729 = ORIENTED_EDGE ( 'NONE', *, *, #133107, .F. ) ;
#104730 = EDGE_CURVE ( 'NONE', #32716, #49377, #57138, .T. ) ;
#104731 = ORIENTED_EDGE ( 'NONE', *, *, #98539, .F. ) ;
#104732 = LINE ( 'NONE', #51086, #81449 ) ;
#104734 = EDGE_CURVE ( 'NONE', #99443, #109446, #58589, .T. ) ;
#104733 = VERTEX_POINT ( 'NONE', #15683 ) ;
#104735 = CARTESIAN_POINT ( 'NONE',  ( -11.70025512860841133, -27.71228299555198049, 4.000000000000000000 ) ) ;
#104736 = DIRECTION ( 'NONE',  ( 1.000000000000000000, 0.000000000000000000, 0.000000000000000000 ) ) ;
#104737 = AXIS2_PLACEMENT_3D ( 'NONE', #59562, #93598, #58885 ) ;
#104738 = AXIS2_PLACEMENT_3D ( 'NONE', #98824, #132207, #108243 ) ;
#104739 = EDGE_CURVE ( 'NONE', #9218, #81079, #4800, .T. ) ;
#104740 = FACE_BOUND ( 'NONE', #123957, .T. ) ;
#104741 = FACE_BOUND ( 'NONE', #38470, .T. ) ;
#104742 = DIRECTION ( 'NONE',  ( -0.000000000000000000, -0.3543493200069153248, -0.9351131265310291818 ) ) ;
#104743 = PLANE ( 'NONE',  #122363 ) ;
#104744 = VECTOR ( 'NONE', #136421, 999.9999999999998863 ) ;
#104746 = VERTEX_POINT ( 'NONE', #125938 ) ;
#104745 = DIRECTION ( 'NONE',  ( 0.6830127018922180770, -0.6830127018922204085, -0.2588190451025213501 ) ) ;
#104747 = EDGE_CURVE ( 'NONE', #95610, #39863, #3405, .T. ) ;
#104748 = PLANE ( 'NONE',  #2350 ) ;
#104749 = APPLICATION_PROTOCOL_DEFINITION ( 'draft international standard', 'automotive_design', 1998, #13292 ) ;
#104750 = EDGE_LOOP ( 'NONE', ( #55175, #58657, #34475, #135075 ) ) ;
#104751 = ORIENTED_EDGE ( 'NONE', *, *, #110326, .F. ) ;
#104752 = CARTESIAN_POINT ( 'NONE',  ( 95.43293019189810877, 1.637169565754156508, 6.110000000000000320 ) ) ;
#104753 = ORIENTED_EDGE ( 'NONE', *, *, #40546, .T. ) ;
#104754 = EDGE_CURVE ( 'NONE', #136233, #49064, #36083, .T. ) ;
#104755 = DIRECTION ( 'NONE',  ( 0.000000000000000000, -1.000000000000000000, 0.000000000000000000 ) ) ;
#104756 = CARTESIAN_POINT ( 'NONE',  ( -11.81601139373100651, 28.73617430169779041, 5.000000000000000000 ) ) ;
#104757 = VECTOR ( 'NONE', #90024, 1000.000000000000000 ) ;
#104758 = AXIS2_PLACEMENT_3D ( 'NONE', #13662, #70274, #123193 ) ;
#104759 = VECTOR ( 'NONE', #78545, 1000.000000000000000 ) ;
#104760 = VECTOR ( 'NONE', #16152, 1000.000000000000227 ) ;
#104761 = VECTOR ( 'NONE', #63075, 1000.000000000000000 ) ;
#104762 = DIRECTION ( 'NONE',  ( 0.6830127018922180770, -0.6830127018922204085, -0.2588190451025213501 ) ) ;
#104763 = ORIENTED_EDGE ( 'NONE', *, *, #33892, .T. ) ;
#104764 = PLANE ( 'NONE',  #29844 ) ;
#104765 = DIRECTION ( 'NONE',  ( 0.000000000000000000, 0.000000000000000000, 1.000000000000000000 ) ) ;
#104766 = DIRECTION ( 'NONE',  ( -0.6830127018922181881, 0.6830127018922202975, -0.2588190451025214056 ) ) ;
#104767 = CARTESIAN_POINT ( 'NONE',  ( -2.999999999999975131, 14.96639925780211122, 5.000000000000000000 ) ) ;
#104768 = PLANE ( 'NONE',  #125690 ) ;
#104769 = CARTESIAN_POINT ( 'NONE',  ( 180.8041599634935324, -49.02495722182847260, -39.69341335395904480 ) ) ;
#104770 = AXIS2_PLACEMENT_3D ( 'NONE', #84920, #129134, #142181 ) ;
#104771 = CARTESIAN_POINT ( 'NONE',  ( -3.706123077391934917, 22.22500000000000142, 4.000000000000000000 ) ) ;
#104772 = EDGE_LOOP ( 'NONE', ( #109302, #21757, #135025, #128953 ) ) ;
#104773 = PLANE ( 'NONE',  #114398 ) ;
#104774 = DIRECTION ( 'NONE',  ( -0.7071067811865487940, 0.7071067811865463515, -0.000000000000000000 ) ) ;
#104775 = VERTEX_POINT ( 'NONE', #103434 ) ;
#104776 = EDGE_CURVE ( 'NONE', #9288, #48047, #90444, .T. ) ;
#104777 = EDGE_LOOP ( 'NONE', ( #113947, #45991, #99282, #135901 ) ) ;
#104778 = ORIENTED_EDGE ( 'NONE', *, *, #67790, .F. ) ;
#104779 = CARTESIAN_POINT ( 'NONE',  ( 49.58376352523144703, -6.110000000000001208, -3.741295971395164515E-16 ) ) ;
#104780 = ORIENTED_EDGE ( 'NONE', *, *, #128969, .F. ) ;
#104781 = EDGE_CURVE ( 'NONE', #7366, #120044, #4079, .T. ) ;
#104782 = VECTOR ( 'NONE', #67047, 999.9999999999998863 ) ;
#104783 = CARTESIAN_POINT ( 'NONE',  ( 19.00413961620377279, -3.047499999999994547, 5.278424836066145431 ) ) ;
#104784 = CARTESIAN_POINT ( 'NONE',  ( -18.50179702988272012, 3.003944652846646690, -30.07174397188686399 ) ) ;
#104785 = ORIENTED_EDGE ( 'NONE', *, *, #143166, .T. ) ;
#104786 = DIRECTION ( 'NONE',  ( -0.7071067811865486830, 0.7071067811865464625, 0.000000000000000000 ) ) ;
#104787 = ORIENTED_EDGE ( 'NONE', *, *, #15419, .T. ) ;
#104788 = CYLINDRICAL_SURFACE ( 'NONE', #81218, 0.5000000000000004441 ) ;
#104789 = FACE_OUTER_BOUND ( 'NONE', #121646, .T. ) ;
#104791 = ORIENTED_EDGE ( 'NONE', *, *, #123913, .F. ) ;
#104790 = DIRECTION ( 'NONE',  ( 0.000000000000000000, 1.000000000000000000, 0.000000000000000000 ) ) ;
#104792 = EDGE_LOOP ( 'NONE', ( #61634, #35779, #95467, #135023 ) ) ;
#104793 = ADVANCED_FACE ( 'NONE', ( #134688 ), #124495, .F. ) ;
#104794 = DIRECTION ( 'NONE',  ( -1.000000000000000000, -0.000000000000000000, -0.000000000000000000 ) ) ;
#104795 = LINE ( 'NONE', #119741, #106346 ) ;
#104796 = ORIENTED_EDGE ( 'NONE', *, *, #47082, .T. ) ;
#104797 = EDGE_CURVE ( 'NONE', #61905, #92723, #35901, .T. ) ;
#104798 = DIRECTION ( 'NONE',  ( 0.7071067811865487940, -0.7071067811865463515, 0.000000000000000000 ) ) ;
#104799 = ORIENTED_EDGE ( 'NONE', *, *, #61687, .T. ) ;
#104800 = PRODUCT_DEFINITION_SHAPE ( 'NONE', 'NONE',  #143566 ) ;
#104801 = ORIENTED_EDGE ( 'NONE', *, *, #65513, .T. ) ;
#104802 = AXIS2_PLACEMENT_3D ( 'NONE', #9183, #53454, #96915 ) ;
#104803 = ORIENTED_EDGE ( 'NONE', *, *, #11425, .F. ) ;
#104804 = ORIENTED_EDGE ( 'NONE', *, *, #100168, .F. ) ;
#104805 = LINE ( 'NONE', #59886, #128242 ) ;
#104806 = VECTOR ( 'NONE', #143045, 1000.000000000000227 ) ;
#104807 = DIRECTION ( 'NONE',  ( -0.7071067811865486830, -0.7071067811865464625, -0.000000000000000000 ) ) ;
#104808 = CARTESIAN_POINT ( 'NONE',  ( -22.99806943317885555, -22.22500000000000142, 4.500000000000000888 ) ) ;
#104809 = LINE ( 'NONE', #15609, #113108 ) ;
#104810 = EDGE_CURVE ( 'NONE', #71320, #65251, #136797, .T. ) ;
#104811 = DIRECTION ( 'NONE',  ( 0.3543493200069162685, -0.000000000000000000, -0.9351131265310288487 ) ) ;
#104812 = VERTEX_POINT ( 'NONE', #13565 ) ;
#104813 = CARTESIAN_POINT ( 'NONE',  ( -26.99999999999980815, 18.08204922493370503, 0.9627537363045496344 ) ) ;
#104814 = CARTESIAN_POINT ( 'NONE',  ( -21.32816939922337696, -15.74070752338412049, 4.000000000000000000 ) ) ;
#104815 = FACE_OUTER_BOUND ( 'NONE', #96754, .T. ) ;
#104816 = FACE_OUTER_BOUND ( 'NONE', #111007, .T. ) ;
#104817 = CARTESIAN_POINT ( 'NONE',  ( 0.000000000000000000, -57.15000000000009095, 34.92499999999998295 ) ) ;
#104818 = VERTEX_POINT ( 'NONE', #135403 ) ;
#104819 = ORIENTED_EDGE ( 'NONE', *, *, #118057, .F. ) ;
#104820 = VECTOR ( 'NONE', #35052, 1000.000000000000000 ) ;
#104821 = ORIENTED_EDGE ( 'NONE', *, *, #35861, .F. ) ;
#104822 = CARTESIAN_POINT ( 'NONE',  ( 8.999999999999944933, -16.44781430457065952, 5.000000000000000000 ) ) ;
#104823 = CARTESIAN_POINT ( 'NONE',  ( 95.60002705046287019, 5.819803920172570422, 5.819803920172575751 ) ) ;
#104824 = PLANE ( 'NONE',  #110132 ) ;
#104825 = VECTOR ( 'NONE', #98965, 1000.000000000000000 ) ;
#104826 = DIRECTION ( 'NONE',  ( 0.000000000000000000, -1.000000000000000000, 0.000000000000000000 ) ) ;
#104827 = CARTESIAN_POINT ( 'NONE',  ( 78.07876352523145158, -7.482591942790327058E-16, 6.109999999999999432 ) ) ;
#104828 = PLANE ( 'NONE',  #102028 ) ;
#104829 = FACE_OUTER_BOUND ( 'NONE', #63460, .T. ) ;
#104830 = CARTESIAN_POINT ( 'NONE',  ( -18.18398860626898994, 28.73617430169800002, 5.000000000000000000 ) ) ;
#104831 = CARTESIAN_POINT ( 'NONE',  ( -3.489213562373097322, -27.52281430457057709, 5.000000000000000000 ) ) ;
#104832 = DIRECTION ( 'NONE',  ( -0.6830127018922180770, -0.6830127018922204085, -0.2588190451025213501 ) ) ;
#104833 = EDGE_CURVE ( 'NONE', #74280, #75139, #25170, .T. ) ;
#104834 = ORIENTED_EDGE ( 'NONE', *, *, #11226, .F. ) ;
#104835 = EDGE_CURVE ( 'NONE', #33991, #51470, #115006, .T. ) ;
#104836 = VECTOR ( 'NONE', #11272, 1000.000000000000000 ) ;
#104837 = CARTESIAN_POINT ( 'NONE',  ( -25.49999999999982947, 5.696342897626483825, -7.587980461218456263 ) ) ;
#104838 = ORIENTED_EDGE ( 'NONE', *, *, #75575, .F. ) ;
#104839 = EDGE_CURVE ( 'NONE', #34178, #99547, #54416, .T. ) ;
#104840 = LINE ( 'NONE', #59933, #36722 ) ;
#104842 = ORIENTED_EDGE ( 'NONE', *, *, #29587, .F. ) ;
#104841 = DIRECTION ( 'NONE',  ( 0.7071067811865486830, -0.7071067811865464625, -0.000000000000000000 ) ) ;
#104843 = DIRECTION ( 'NONE',  ( 0.3543493200069162685, -0.000000000000000000, -0.9351131265310288487 ) ) ;
#104844 = DIRECTION ( 'NONE',  ( 0.000000000000000000, 0.000000000000000000, 1.000000000000000000 ) ) ;
#104845 = EDGE_CURVE ( 'NONE', #119845, #95357, #83141, .T. ) ;
#104846 = ORIENTED_EDGE ( 'NONE', *, *, #56937, .T. ) ;
#104848 = VERTEX_POINT ( 'NONE', #30171 ) ;
#104847 = AXIS2_PLACEMENT_3D ( 'NONE', #8547, #76743, #143393 ) ;
#104849 = ORIENTED_EDGE ( 'NONE', *, *, #22505, .F. ) ;
#104850 = DIRECTION ( 'NONE',  ( 0.7071067811865486830, -0.7071067811865464625, -0.000000000000000000 ) ) ;
#104851 = ADVANCED_FACE ( 'NONE', ( #60714 ), #75147, .F. ) ;
#104853 = EDGE_CURVE ( 'NONE', #76593, #103400, #51949, .T. ) ;
#104852 = CARTESIAN_POINT ( 'NONE',  ( 90.35002705046287019, -5.819803920172572198, -5.819803920172572198 ) ) ;
#104854 = CARTESIAN_POINT ( 'NONE',  ( 72.75000000000000000, -9.735942053221458872E-16, 7.950000000000000178 ) ) ;
#104856 = ADVANCED_FACE ( 'NONE', ( #127344 ), #62835, .F. ) ;
#104855 = VERTEX_POINT ( 'NONE', #17843 ) ;
#104857 = DIRECTION ( 'NONE',  ( -1.000000000000000000, -1.224606353822377258E-16, -0.000000000000000000 ) ) ;
#104858 = EDGE_CURVE ( 'NONE', #77143, #113805, #61431, .T. ) ;
#104859 = PLANE ( 'NONE',  #43783 ) ;
#104860 = CARTESIAN_POINT ( 'NONE',  ( 25.66666666666666785, -5.278424836066145431, -3.047499999999993658 ) ) ;
#104861 = LINE ( 'NONE', #48346, #139459 ) ;
#104862 = VECTOR ( 'NONE', #112661, 1000.000000000000000 ) ;
#104863 = DIRECTION ( 'NONE',  ( 1.000000000000000000, -0.000000000000000000, 0.000000000000000000 ) ) ;
#104864 = EDGE_CURVE ( 'NONE', #26671, #34581, #41777, .T. ) ;
#104865 = ORIENTED_EDGE ( 'NONE', *, *, #109382, .T. ) ;
#104866 = TOROIDAL_SURFACE ( 'NONE', #7568, 8.000000000000001776, 1.500000000000000000 ) ;
#104867 = AXIS2_PLACEMENT_3D ( 'NONE', #3132, #80038, #45964 ) ;
#104868 = CARTESIAN_POINT ( 'NONE',  ( 45.28752705046289151, 0.000000000000000000, -7.949999999999998401 ) ) ;
#104870 = ORIENTED_EDGE ( 'NONE', *, *, #97667, .F. ) ;
#104869 = EDGE_CURVE ( 'NONE', #70774, #64350, #107015, .T. ) ;
#104871 = CARTESIAN_POINT ( 'NONE',  ( 85.45876352523143282, 0.000000000000000000, -6.110000000000001208 ) ) ;
#104872 = DIRECTION ( 'NONE',  ( -0.7071067811865487940, 0.7071067811865463515, 0.000000000000000000 ) ) ;
#104873 = VECTOR ( 'NONE', #72409, 1000.000000000000114 ) ;
#104874 = DIRECTION ( 'NONE',  ( -0.6830127018922181881, 0.6830127018922202975, -0.2588190451025214056 ) ) ;
#104875 = CARTESIAN_POINT ( 'NONE',  ( 0.000000000000000000, 0.000000000000000000, 5.000000000000000000 ) ) ;
#104876 = EDGE_LOOP ( 'NONE', ( #9271, #131175, #116517, #109671 ) ) ;
#104877 = LINE ( 'NONE', #26606, #58224 ) ;
#104878 = EDGE_CURVE ( 'NONE', #61060, #34133, #96065, .T. ) ;
#104879 = DIRECTION ( 'NONE',  ( 0.7071067811865486830, -0.7071067811865464625, -0.000000000000000000 ) ) ;
#104880 = CARTESIAN_POINT ( 'NONE',  ( 117.9125270504628986, -7.949999999999998401, -4.867971026610728450E-16 ) ) ;
#104882 = EDGE_LOOP ( 'NONE', ( #119836, #125459, #20160, #62758 ) ) ;
#104881 = DIRECTION ( 'NONE',  ( -1.000000000000000000, -1.224606353822377258E-16, -0.000000000000000000 ) ) ;
#104883 = CARTESIAN_POINT ( 'NONE',  ( 29.84387692260737523, -22.22500000000000142, 4.000000000000000000 ) ) ;
#104884 = DIRECTION ( 'NONE',  ( -0.3543493200069162685, -0.000000000000000000, -0.9351131265310288487 ) ) ;
#104885 = SURFACE_STYLE_USAGE ( .BOTH. , #26616 ) ;
#104886 = ADVANCED_FACE ( 'NONE', ( #105572 ), #49824, .F. ) ;
#104887 = CARTESIAN_POINT ( 'NONE',  ( 59.47916666666666430, -7.950000000000000178, 2.130196079827424427 ) ) ;
#104888 = VERTEX_POINT ( 'NONE', #93994 ) ;
#104889 = EDGE_LOOP ( 'NONE', ( #83826, #117443, #78621, #87156 ) ) ;
#104890 = ORIENTED_EDGE ( 'NONE', *, *, #62200, .T. ) ;
#104891 = CARTESIAN_POINT ( 'NONE',  ( 72.33376352523143282, 6.110000000000001208, 1.122388791418549305E-15 ) ) ;
#104892 = VECTOR ( 'NONE', #121934, 1000.000000000000000 ) ;
#104893 = ORIENTED_EDGE ( 'NONE', *, *, #61608, .T. ) ;
#104894 = DIRECTION ( 'NONE',  ( 0.6830127018922181881, 0.6830127018922202975, -0.2588190451025214056 ) ) ;
#104895 = LINE ( 'NONE', #3419, #119717 ) ;
#104896 = CARTESIAN_POINT ( 'NONE',  ( -42.29974487139158157, -27.71228299555235708, 4.000000000000000000 ) ) ;
#104897 = CARTESIAN_POINT ( 'NONE',  ( 19.89359858452208130, 2.055000000000001048, 0.000000000000000000 ) ) ;
#104898 = EDGE_LOOP ( 'NONE', ( #71128, #108109, #78952, #72756 ) ) ;
#104899 = LINE ( 'NONE', #140384, #44543 ) ;
#104900 = DIRECTION ( 'NONE',  ( 0.000000000000000000, 0.000000000000000000, 1.000000000000000000 ) ) ;
#104901 = VECTOR ( 'NONE', #88402, 1000.000000000000000 ) ;
#104902 = ORIENTED_EDGE ( 'NONE', *, *, #123570, .T. ) ;
#104903 = AXIS2_PLACEMENT_3D ( 'NONE', #137995, #116937, #62579 ) ;
#104904 = CARTESIAN_POINT ( 'NONE',  ( -24.84463820744543838, 1.742823668393624903, 4.000000000000000000 ) ) ;
#104905 = EDGE_CURVE ( 'NONE', #100977, #99513, #39658, .T. ) ;
#104906 = CARTESIAN_POINT ( 'NONE',  ( 33.76669371712954870, -7.949999999999998401, 2.130196079827423983 ) ) ;
#104907 = LINE ( 'NONE', #128797, #107104 ) ;
#104908 = EDGE_CURVE ( 'NONE', #97859, #124430, #43664, .T. ) ;
#104909 = ORIENTED_EDGE ( 'NONE', *, *, #41190, .T. ) ;
#104911 = EDGE_LOOP ( 'NONE', ( #2505, #119551, #23004, #74493 ) ) ;
#104910 = VECTOR ( 'NONE', #99628, 999.9999999999998863 ) ;
#104912 = FACE_OUTER_BOUND ( 'NONE', #27520, .T. ) ;
#104913 = LINE ( 'NONE', #62868, #3742 ) ;
#104914 = CARTESIAN_POINT ( 'NONE',  ( -7.940000000000001279, -33.26999999999999602, -10.00000000000000178 ) ) ;
#104915 = LINE ( 'NONE', #28803, #67448 ) ;
#104916 = DIRECTION ( 'NONE',  ( -0.3543493200069162685, -0.000000000000000000, -0.9351131265310288487 ) ) ;
#104917 = ADVANCED_FACE ( 'NONE', ( #29450 ), #62112, .F. ) ;
#104918 = VECTOR ( 'NONE', #24594, 1000.000000000000227 ) ;
#104919 = CARTESIAN_POINT ( 'NONE',  ( -11.67183060077638679, -15.74070752338412049, 4.000000000000000000 ) ) ;
#104920 = ORIENTED_EDGE ( 'NONE', *, *, #87587, .F. ) ;
#104921 = ORIENTED_EDGE ( 'NONE', *, *, #100455, .F. ) ;
#104922 = ORIENTED_EDGE ( 'NONE', *, *, #46556, .T. ) ;
#104923 = EDGE_CURVE ( 'NONE', #57507, #102158, #96130, .T. ) ;
#104924 = ORIENTED_EDGE ( 'NONE', *, *, #110139, .F. ) ;
#104925 = VECTOR ( 'NONE', #64053, 1000.000000000000000 ) ;
#104926 = DIRECTION ( 'NONE',  ( -0.6830127018922181881, 0.6830127018922202975, -0.2588190451025214056 ) ) ;
#104927 =( LENGTH_UNIT ( ) NAMED_UNIT ( * ) SI_UNIT ( .MILLI., .METRE. ) );
#104928 = ORIENTED_EDGE ( 'NONE', *, *, #102968, .T. ) ;
#104929 = CARTESIAN_POINT ( 'NONE',  ( 81.48921356237309510, -27.52281430457112066, 5.000000000000000000 ) ) ;
#104930 = FACE_OUTER_BOUND ( 'NONE', #135227, .T. ) ;
#104931 = CARTESIAN_POINT ( 'NONE',  ( 51.18398860626899705, 28.73617430169823095, 5.000000000000000000 ) ) ;
#104932 = CARTESIAN_POINT ( 'NONE',  ( -29.99999999999979750, -2.904428200921339354, -6.989807076074876946 ) ) ;
#104933 = CIRCLE ( 'NONE', #65675, 1.000000000000000000 ) ;
#104934 = CARTESIAN_POINT ( 'NONE',  ( 3.183988606268992161, 28.73617430169789699, 5.000000000000000000 ) ) ;
#104935 = ORIENTED_EDGE ( 'NONE', *, *, #80719, .T. ) ;
#104936 = DIRECTION ( 'NONE',  ( -0.000000000000000000, 0.000000000000000000, 1.000000000000000000 ) ) ;
#104937 = CARTESIAN_POINT ( 'NONE',  ( -19.62719212111867151, -2.766370489448051195, 4.185522593092492194 ) ) ;
#104938 = EDGE_LOOP ( 'NONE', ( #110776, #110557, #59645, #75303, #105249 ) ) ;
#104940 = EDGE_CURVE ( 'NONE', #85226, #98208, #61462, .T. ) ;
#104939 = LINE ( 'NONE', #125277, #133879 ) ;
#104941 = ORIENTED_EDGE ( 'NONE', *, *, #134713, .F. ) ;
#104942 = ORIENTED_EDGE ( 'NONE', *, *, #5244, .T. ) ;
#104943 = EDGE_CURVE ( 'NONE', #135502, #81560, #128774, .T. ) ;
#104944 = VERTEX_POINT ( 'NONE', #8383 ) ;
#104945 = ORIENTED_EDGE ( 'NONE', *, *, #121863, .F. ) ;
#104946 = CARTESIAN_POINT ( 'NONE',  ( 69.70876352523144703, -7.482591942790329030E-16, 6.110000000000001208 ) ) ;
#104947 = ORIENTED_EDGE ( 'NONE', *, *, #88335, .F. ) ;
#104948 = CARTESIAN_POINT ( 'NONE',  ( 50.99451991528749062, 28.92564299267973738, 4.000000000000000000 ) ) ;
#104949 = LINE ( 'NONE', #30245, #26480 ) ;
#104950 = CARTESIAN_POINT ( 'NONE',  ( 106.8962635252314328, 4.472830434245840259, -4.472830434245838482 ) ) ;
#104951 = DIRECTION ( 'NONE',  ( -0.7071067811865486830, -0.7071067811865464625, 0.000000000000000000 ) ) ;
#104952 = DIRECTION ( 'NONE',  ( -0.7071067811865487940, 0.7071067811865463515, -0.000000000000000000 ) ) ;
#104953 = AXIS2_PLACEMENT_3D ( 'NONE', #108002, #121747, #684 ) ;
#104954 = DIRECTION ( 'NONE',  ( -0.000000000000000000, 0.000000000000000000, 1.000000000000000000 ) ) ;
#104955 = FACE_OUTER_BOUND ( 'NONE', #10725, .T. ) ;
#104957 = ADVANCED_FACE ( 'NONE', ( #117859 ), #54805, .F. ) ;
#104956 = VECTOR ( 'NONE', #24718, 1000.000000000000000 ) ;
#104958 = FACE_OUTER_BOUND ( 'NONE', #23217, .T. ) ;
#104959 = ORIENTED_EDGE ( 'NONE', *, *, #136444, .T. ) ;
#104960 = ADVANCED_FACE ( 'NONE', ( #56267 ), #22137, .F. ) ;
#104961 = DIRECTION ( 'NONE',  ( 0.000000000000000000, 0.000000000000000000, 1.000000000000000000 ) ) ;
#104962 = ORIENTED_EDGE ( 'NONE', *, *, #21911, .F. ) ;
#104963 = ORIENTED_EDGE ( 'NONE', *, *, #52012, .F. ) ;
#104964 = AXIS2_PLACEMENT_3D ( 'NONE', #132027, #18965, #54476 ) ;
#104965 = PRODUCT_DEFINITION_FORMATION_WITH_SPECIFIED_SOURCE ( 'ANY', '', #142759, .NOT_KNOWN. ) ;
#104966 = DIRECTION ( 'NONE',  ( 0.7071067811865487940, 0.7071067811865463515, 0.000000000000000000 ) ) ;
#104967 = EDGE_LOOP ( 'NONE', ( #122250, #134760, #118595, #68760 ) ) ;
#104968 = FACE_OUTER_BOUND ( 'NONE', #29856, .T. ) ;
#104969 = DIRECTION ( 'NONE',  ( 0.7071067811865486830, -0.7071067811865464625, -0.000000000000000000 ) ) ;
#104970 = DIRECTION ( 'NONE',  ( -0.7071067811865486830, -0.7071067811865464625, 0.000000000000000000 ) ) ;
#104971 = EDGE_CURVE ( 'NONE', #107217, #86260, #123298, .T. ) ;
#104972 = DIRECTION ( 'NONE',  ( 0.000000000000000000, -1.000000000000000000, 0.000000000000000000 ) ) ;
#104973 = APPLICATION_CONTEXT ( 'automotive_design' ) ;
#104974 = ORIENTED_EDGE ( 'NONE', *, *, #20260, .T. ) ;
#104975 = CARTESIAN_POINT ( 'NONE',  ( 0.03269009325358174928, -47.89015928896881036, 37.22465919495169118 ) ) ;
#104976 = ORIENTED_EDGE ( 'NONE', *, *, #50246, .T. ) ;
#104977 = VECTOR ( 'NONE', #22532, 1000.000000000000000 ) ;
#104978 = VECTOR ( 'NONE', #100753, 1000.000000000000227 ) ;
#104979 = CARTESIAN_POINT ( 'NONE',  ( 31.71290314143522693, 3.967499999999992699, -6.871911579029513994 ) ) ;
#104980 = DIRECTION ( 'NONE',  ( 0.7071067811865487940, 0.7071067811865463515, 0.000000000000000000 ) ) ;
#104981 = DIRECTION ( 'NONE',  ( 1.000000000000000000, 0.000000000000000000, 0.000000000000000000 ) ) ;
#104982 = DIRECTION ( 'NONE',  ( 0.6830127018922180770, -0.6830127018922204085, -0.2588190451025213501 ) ) ;
#104983 = ORIENTED_EDGE ( 'NONE', *, *, #76417, .F. ) ;
#104984 = ORIENTED_EDGE ( 'NONE', *, *, #79328, .F. ) ;
#104985 = VERTEX_POINT ( 'NONE', #98303 ) ;
#104986 = LINE ( 'NONE', #94801, #72814 ) ;
#104987 = LINE ( 'NONE', #70963, #83483 ) ;
#104988 = CARTESIAN_POINT ( 'NONE',  ( -8.292986735706895374, -21.74070752338406010, 4.999753212805224223 ) ) ;
#104989 = CARTESIAN_POINT ( 'NONE',  ( -15.70710678118643422, 11.25929247661561128, 5.000000000000000000 ) ) ;
#104990 = AXIS2_PLACEMENT_3D ( 'NONE', #116385, #17078, #83792 ) ;
#104991 = LINE ( 'NONE', #124613, #131923 ) ;
#104992 = PLANE ( 'NONE',  #64280 ) ;
#104993 = LINE ( 'NONE', #94109, #71735 ) ;
#104994 = AXIS2_PLACEMENT_3D ( 'NONE', #97474, #64881, #54722 ) ;
#104995 = CARTESIAN_POINT ( 'NONE',  ( -18.29974487139159223, -27.71228299555219010, 4.000000000000000000 ) ) ;
#104996 = DIRECTION ( 'NONE',  ( 0.7071067811865486830, -0.7071067811865464625, -0.000000000000000000 ) ) ;
#104997 = ORIENTED_EDGE ( 'NONE', *, *, #142417, .F. ) ;
#104998 = CARTESIAN_POINT ( 'NONE',  ( 72.75000000000000000, -9.735942053221458872E-16, 7.950000000000000178 ) ) ;
#104999 = DIRECTION ( 'NONE',  ( -0.000000000000000000, 0.3543493200069152138, -0.9351131265310292928 ) ) ;
#105000 = ORIENTED_EDGE ( 'NONE', *, *, #28848, .T. ) ;
#105001 = VECTOR ( 'NONE', #127847, 1000.000000000000000 ) ;
#105002 = DIRECTION ( 'NONE',  ( 0.6830127018922181881, 0.6830127018922202975, -0.2588190451025214056 ) ) ;
#105004 = ORIENTED_EDGE ( 'NONE', *, *, #45777, .F. ) ;
#105003 = FACE_OUTER_BOUND ( 'NONE', #113847, .T. ) ;
#105005 = DIRECTION ( 'NONE',  ( 0.000000000000000000, -1.000000000000000000, 0.000000000000000000 ) ) ;
#105006 = DIRECTION ( 'NONE',  ( -0.7071067811865486830, -0.7071067811865464625, 0.000000000000000000 ) ) ;
#105007 = ORIENTED_EDGE ( 'NONE', *, *, #122212, .T. ) ;
#105008 = CARTESIAN_POINT ( 'NONE',  ( 34.92499999999998295, 4.444556126563224296, 11.73767485154041523 ) ) ;
#105009 = VERTEX_POINT ( 'NONE', #131648 ) ;
#105010 = VECTOR ( 'NONE', #3963, 1000.000000000000227 ) ;
#105011 = CARTESIAN_POINT ( 'NONE',  ( -30.48921356237309510, -27.52281430457076894, 5.000000000000000000 ) ) ;
#105012 = CARTESIAN_POINT ( 'NONE',  ( -12.69999999999998153, 3.061616997868383634E-16, -2.500000000000000444 ) ) ;
#105014 = EDGE_CURVE ( 'NONE', #47828, #81835, #110565, .T. ) ;
#105013 = CARTESIAN_POINT ( 'NONE',  ( 123.1625270504628986, 7.949999999999998401, 1.460391307983218338E-15 ) ) ;
#105016 = VECTOR ( 'NONE', #17411, 1000.000000000000227 ) ;
#105015 = DIRECTION ( 'NONE',  ( -0.7071067811865487940, 0.7071067811865463515, 0.000000000000000000 ) ) ;
#105017 = CARTESIAN_POINT ( 'NONE',  ( 51.48921356237309510, -27.52281430457091460, 5.000000000000000000 ) ) ;
#105018 = EDGE_CURVE ( 'NONE', #8091, #83438, #19523, .T. ) ;
#105019 = EDGE_CURVE ( 'NONE', #10533, #51668, #55518, .T. ) ;
#105020 = DIRECTION ( 'NONE',  ( -0.7071067811865487940, 0.7071067811865463515, 0.000000000000000000 ) ) ;
#105021 = FACE_OUTER_BOUND ( 'NONE', #43620, .T. ) ;
#105022 = EDGE_CURVE ( 'NONE', #5639, #30178, #64974, .T. ) ;
#105023 = DIRECTION ( 'NONE',  ( -1.000000000000000000, -0.000000000000000000, -0.000000000000000000 ) ) ;
#105024 = CARTESIAN_POINT ( 'NONE',  ( 28.99956980810188867, -3.967499999999998028, -6.871911579029511330 ) ) ;
#105025 = CARTESIAN_POINT ( 'NONE',  ( 4.645403141435220817, -2.126176841940958351, -7.934999999999988951 ) ) ;
#105026 = VECTOR ( 'NONE', #25169, 1000.000000000000000 ) ;
#105027 = CARTESIAN_POINT ( 'NONE',  ( -31.82816939922330235, 3.759292476615678336, 4.000000000000000000 ) ) ;
#105028 = LINE ( 'NONE', #28197, #102251 ) ;
#105030 = ADVANCED_FACE ( 'NONE', ( #133781 ), #87429, .T. ) ;
#105029 = FACE_OUTER_BOUND ( 'NONE', #23676, .T. ) ;
#105031 = ORIENTED_EDGE ( 'NONE', *, *, #74636, .F. ) ;
#105032 =( BOUNDED_CURVE ( )  B_SPLINE_CURVE ( 2, ( #61974, #125796, #38075, #138087, #6808, #15543, #93152, #116330, #105437, #70721, #27890, #82999, #38775 ),
 .UNSPECIFIED., .F., .F. ) 
 B_SPLINE_CURVE_WITH_KNOTS ( ( 3, 2, 2, 2, 2, 2, 3 ),
 ( 0.6333333333333333037, 0.6361111111111110716, 0.6388888888888888395, 0.6416666666666667185, 0.6444444444444444864, 0.6472222222222222543, 0.6500000000000000222 ),
 .UNSPECIFIED. ) 
 CURVE ( )  GEOMETRIC_REPRESENTATION_ITEM ( )  RATIONAL_B_SPLINE_CURVE ( ( 1.000000000000000000, 0.9659258262890683122, 1.000000000000000000, 0.9659258262890683122, 1.000000000000000000, 0.9659258262890683122, 1.000000000000000000, 0.9659258262890683122, 1.000000000000000000, 0.9659258262890683122, 1.000000000000000000, 0.9659258262890683122, 1.000000000000000000 ) ) 
 REPRESENTATION_ITEM ( '' )  );
#105033 = VERTEX_POINT ( 'NONE', #88868 ) ;
#105034 = CARTESIAN_POINT ( 'NONE',  ( 84.12500000000000000, -7.950000000000000178, -4.867971026610729436E-16 ) ) ;
#105036 = ORIENTED_EDGE ( 'NONE', *, *, #80690, .T. ) ;
#105035 = FILL_AREA_STYLE ('',( #60874 ) ) ;
#105037 = ORIENTED_EDGE ( 'NONE', *, *, #136284, .F. ) ;
#105038 = EDGE_CURVE ( 'NONE', #97236, #6765, #132388, .T. ) ;
#105039 = DIRECTION ( 'NONE',  ( 0.000000000000000000, 0.000000000000000000, 1.000000000000000000 ) ) ;
#105040 = DIRECTION ( 'NONE',  ( 0.7071067811865487940, 0.7071067811865463515, 0.000000000000000000 ) ) ;
#105041 = CIRCLE ( 'NONE', #3202, 2.500000000000000444 ) ;
#105042 = LINE ( 'NONE', #61578, #94038 ) ;
#105043 = ORIENTED_EDGE ( 'NONE', *, *, #24180, .T. ) ;
#105044 = CARTESIAN_POINT ( 'NONE',  ( -18.29974487139159223, -27.71228299555219010, 4.000000000000000000 ) ) ;
#105045 = FACE_OUTER_BOUND ( 'NONE', #44659, .T. ) ;
#105046 = EDGE_CURVE ( 'NONE', #1660, #139966, #89258, .T. ) ;
#105047 = CARTESIAN_POINT ( 'NONE',  ( 1.499999999999996225, -4.533600742197694267, 5.000000000000000000 ) ) ;
#105048 = CARTESIAN_POINT ( 'NONE',  ( 126.9298449394060668, 2.838896997467642791, 5.891538070402098981 ) ) ;
#105049 = EDGE_CURVE ( 'NONE', #46912, #43233, #98988, .T. ) ;
#105050 = CARTESIAN_POINT ( 'NONE',  ( 0.000000000000000000, 0.000000000000000000, 5.000000000000000000 ) ) ;
#105052 = MECHANICAL_DESIGN_GEOMETRIC_PRESENTATION_REPRESENTATION (  '', ( #100414 ), #30983 ) ;
#105051 = DIRECTION ( 'NONE',  ( 1.000000000000000000, 0.000000000000000000, 0.000000000000000000 ) ) ;
#105053 =( LENGTH_UNIT ( ) NAMED_UNIT ( * ) SI_UNIT ( .MILLI., .METRE. ) );
#105054 = DIRECTION ( 'NONE',  ( -0.7071067811865486830, -0.7071067811865464625, -0.000000000000000000 ) ) ;
#105055 = CARTESIAN_POINT ( 'NONE',  ( 28.49999999999980105, -2.173586137069114521, -4.605770156576045160 ) ) ;
#105056 = DIRECTION ( 'NONE',  ( -0.6830127018922180770, -0.6830127018922204085, -0.2588190451025213501 ) ) ;
#105057 = CARTESIAN_POINT ( 'NONE',  ( -34.92500000000001137, -0.1833456135895722428, 4.500000000000000888 ) ) ;
#105058 = EDGE_CURVE ( 'NONE', #32075, #19121, #86228, .T. ) ;
#105059 = PRESENTATION_STYLE_ASSIGNMENT (( #38386 ) ) ;
#105060 = VERTEX_POINT ( 'NONE', #9845 ) ;
#105061 = VERTEX_POINT ( 'NONE', #9088 ) ;
#105062 = CARTESIAN_POINT ( 'NONE',  ( 110.3962635252314328, 4.472830434245840259, -4.472830434245839371 ) ) ;
#105063 = VECTOR ( 'NONE', #131716, 1000.000000000000227 ) ;
#105064 = ORIENTED_EDGE ( 'NONE', *, *, #3261, .F. ) ;
#105065 = ADVANCED_FACE ( 'NONE', ( #53353 ), #120006, .F. ) ;
#105066 = CARTESIAN_POINT ( 'NONE',  ( 7.583333333333333925, -5.278424836066144543, 3.047499999999995879 ) ) ;
#105067 = ORIENTED_EDGE ( 'NONE', *, *, #43304, .T. ) ;
#105068 = CARTESIAN_POINT ( 'NONE',  ( 76.10416666666667140, 2.130196079827422206, 7.950000000000001954 ) ) ;
#105070 = AXIS2_PLACEMENT_3D ( 'NONE', #125993, #94748, #49865 ) ;
#105069 = FACE_OUTER_BOUND ( 'NONE', #95636, .T. ) ;
#105071 = CARTESIAN_POINT ( 'NONE',  ( 106.5162635252314658, -4.472830434245839371, 4.472830434245839371 ) ) ;
#105072 = VERTEX_POINT ( 'NONE', #75840 ) ;
#105073 = DIRECTION ( 'NONE',  ( 0.7071067811865486830, -0.7071067811865464625, -0.000000000000000000 ) ) ;
#105074 = ORIENTED_EDGE ( 'NONE', *, *, #49283, .T. ) ;
#105076 = EDGE_CURVE ( 'NONE', #135397, #89639, #54115, .T. ) ;
#105075 = LINE ( 'NONE', #36269, #40737 ) ;
#105077 = LINE ( 'NONE', #41239, #56148 ) ;
#105078 = LINE ( 'NONE', #127553, #83263 ) ;
#105079 = ORIENTED_EDGE ( 'NONE', *, *, #16835, .T. ) ;
#105080 = VERTEX_POINT ( 'NONE', #381 ) ;
#105081 = VERTEX_POINT ( 'NONE', #133095 ) ;
#105082 = LINE ( 'NONE', #114525, #135128 ) ;
#105083 = LINE ( 'NONE', #139170, #68588 ) ;
#105084 = CARTESIAN_POINT ( 'NONE',  ( 8.233736474768550195, 5.808823158059035485, 5.808823158059032821 ) ) ;
#105085 = AXIS2_PLACEMENT_3D ( 'NONE', #40950, #65600, #53233 ) ;
#105086 = CARTESIAN_POINT ( 'NONE',  ( -12.69999999999998153, 0.000000000000000000, 0.000000000000000000 ) ) ;
#105087 = ADVANCED_FACE ( 'NONE', ( #122162 ), #22832, .T. ) ;
#105088 = VECTOR ( 'NONE', #79954, 1000.000000000000227 ) ;
#105089 = ORIENTED_EDGE ( 'NONE', *, *, #70300, .T. ) ;
#105090 = ORIENTED_EDGE ( 'NONE', *, *, #70339, .F. ) ;
#105091 = DIRECTION ( 'NONE',  ( 0.7071067811865486830, -0.7071067811865464625, -0.000000000000000000 ) ) ;
#105093 = ORIENTED_EDGE ( 'NONE', *, *, #83351, .T. ) ;
#105092 = EDGE_CURVE ( 'NONE', #143140, #57564, #23581, .T. ) ;
#105094 = EDGE_LOOP ( 'NONE', ( #54051, #80230, #97210, #82806 ) ) ;
#105095 = VECTOR ( 'NONE', #16906, 1000.000000000000000 ) ;
#105096 = CARTESIAN_POINT ( 'NONE',  ( 110.5995968585647802, -6.109999999999997655, -1.637169565754160283 ) ) ;
#105097 = LINE ( 'NONE', #84102, #67358 ) ;
#105098 = CARTESIAN_POINT ( 'NONE',  ( 18.95159235450331892, 2.500000000000001332, 0.000000000000000000 ) ) ;
#105099 = VERTEX_POINT ( 'NONE', #122902 ) ;
#105100 = VECTOR ( 'NONE', #97104, 1000.000000000000227 ) ;
#105101 = DIRECTION ( 'NONE',  ( 0.6830127018922181881, 0.6830127018922202975, -0.2588190451025214056 ) ) ;
#105102 = EDGE_CURVE ( 'NONE', #71184, #103011, #56961, .T. ) ;
#105103 = LINE ( 'NONE', #7182, #96447 ) ;
#105104 = CARTESIAN_POINT ( 'NONE',  ( -19.49999999999986500, -17.91344420646044711, 1.358650452708419776 ) ) ;
#105105 = DIRECTION ( 'NONE',  ( -0.3543493200069162685, -0.000000000000000000, -0.9351131265310288487 ) ) ;
#105106 = ORIENTED_EDGE ( 'NONE', *, *, #42234, .T. ) ;
#105107 = VECTOR ( 'NONE', #103052, 1000.000000000000000 ) ;
#105108 = DIRECTION ( 'NONE',  ( 0.7071067811865486830, -0.7071067811865464625, -0.000000000000000000 ) ) ;
#105109 = FACE_BOUND ( 'NONE', #60062, .T. ) ;
#105111 = EDGE_LOOP ( 'NONE', ( #83927, #138209, #134599, #16975 ) ) ;
#105110 = MECHANICAL_DESIGN_GEOMETRIC_PRESENTATION_REPRESENTATION (  '', ( #112067 ), #884 ) ;
#105112 = LINE ( 'NONE', #71798, #50454 ) ;
#105114 = EDGE_CURVE ( 'NONE', #80628, #9882, #112038, .T. ) ;
#105113 = CARTESIAN_POINT ( 'NONE',  ( -54.18398860626899705, 28.73617430169825226, 5.000000000000000000 ) ) ;
#105115 = CARTESIAN_POINT ( 'NONE',  ( 57.18398860626899705, 28.73617430169827358, 5.000000000000000000 ) ) ;
#105116 = ORIENTED_EDGE ( 'NONE', *, *, #95485, .T. ) ;
#105117 = EDGE_CURVE ( 'NONE', #79775, #94854, #54510, .T. ) ;
#105118 = CARTESIAN_POINT ( 'NONE',  ( -19.01987774928536723, -17.24070752338410273, 20.23474786156464944 ) ) ;
#105119 = VERTEX_POINT ( 'NONE', #92386 ) ;
#105120 = ORIENTED_EDGE ( 'NONE', *, *, #73593, .T. ) ;
#105121 = ORIENTED_EDGE ( 'NONE', *, *, #85540, .F. ) ;
#105122 = AXIS2_PLACEMENT_3D ( 'NONE', #86247, #130470, #64481 ) ;
#105123 = CARTESIAN_POINT ( 'NONE',  ( 41.47459685856478018, 1.637169565754164280, -6.109999999999996767 ) ) ;
#105125 = ORIENTED_EDGE ( 'NONE', *, *, #139305, .T. ) ;
#105124 = COLOUR_RGB ( '', 0.40784314, 0.44705882, 0.49803922) ;
#105126 = CYLINDRICAL_SURFACE ( 'NONE', #22839, 0.5000000000000004441 ) ;
#105127 = DIRECTION ( 'NONE',  ( 0.000000000000000000, 0.000000000000000000, -1.000000000000000000 ) ) ;
#105128 = DIRECTION ( 'NONE',  ( 0.000000000000000000, 0.000000000000000000, 1.000000000000000000 ) ) ;
#105129 = LINE ( 'NONE', #7207, #36638 ) ;
#105130 = LINE ( 'NONE', #72561, #6467 ) ;
#105131 = DIRECTION ( 'NONE',  ( 0.3543493200069162685, -0.000000000000000000, -0.9351131265310288487 ) ) ;
#105132 = PRESENTATION_STYLE_ASSIGNMENT (( #6482 ) ) ;
#105133 = DIRECTION ( 'NONE',  ( -0.7071067811865486830, 0.7071067811865464625, 0.000000000000000000 ) ) ;
#105134 = ADVANCED_FACE ( 'NONE', ( #12689 ), #134506, .F. ) ;
#105135 = CARTESIAN_POINT ( 'NONE',  ( -33.48921356237309510, -27.52281430457078670, 5.000000000000000000 ) ) ;
#105136 = CARTESIAN_POINT ( 'NONE',  ( 18.18398860626898994, 28.73617430169800002, 5.000000000000000000 ) ) ;
#105137 = ORIENTED_EDGE ( 'NONE', *, *, #55831, .F. ) ;
#105138 = ORIENTED_EDGE ( 'NONE', *, *, #125170, .T. ) ;
#105140 = VERTEX_POINT ( 'NONE', #24993 ) ;
#105139 = AXIS2_PLACEMENT_3D ( 'NONE', #12270, #78998, #143498 ) ;
#105141 = ORIENTED_EDGE ( 'NONE', *, *, #138047, .F. ) ;
#105142 = CARTESIAN_POINT ( 'NONE',  ( 9.707013264292969623, -21.74070752338406365, 4.999753212805217117 ) ) ;
#105143 = ORIENTED_EDGE ( 'NONE', *, *, #102941, .T. ) ;
#105144 = ORIENTED_EDGE ( 'NONE', *, *, #139079, .T. ) ;
#105145 = CARTESIAN_POINT ( 'NONE',  ( -34.92500000000001137, 22.22500000000000142, 4.000000000000000000 ) ) ;
#105146 = DIRECTION ( 'NONE',  ( -0.7071067811865486830, -0.7071067811865464625, 0.000000000000000000 ) ) ;
#105147 = EDGE_CURVE ( 'NONE', #114717, #72085, #25720, .T. ) ;
#105148 = EDGE_CURVE ( 'NONE', #45162, #49422, #137358, .T. ) ;
#105149 = FACE_OUTER_BOUND ( 'NONE', #93693, .T. ) ;
#105150 = ORIENTED_EDGE ( 'NONE', *, *, #57734, .T. ) ;
#105151 = DIRECTION ( 'NONE',  ( 0.000000000000000000, 1.000000000000000000, 0.000000000000000000 ) ) ;
#105152 = VERTEX_POINT ( 'NONE', #69249 ) ;
#105153 = CARTESIAN_POINT ( 'NONE',  ( -2.999999999999983569, 7.931123077392109977, 4.000000000000000000 ) ) ;
#105154 = FACE_OUTER_BOUND ( 'NONE', #130982, .T. ) ;
#105155 = SURFACE_STYLE_FILL_AREA ( #45809 ) ;
#105156 = VERTEX_POINT ( 'NONE', #103970 ) ;
#105158 = FACE_OUTER_BOUND ( 'NONE', #109572, .T. ) ;
#105157 = CARTESIAN_POINT ( 'NONE',  ( 103.4537635252314516, -6.109999999999999432, -3.741295971395163529E-16 ) ) ;
#105159 = SURFACE_STYLE_USAGE ( .BOTH. , #37788 ) ;
#105160 =( NAMED_UNIT ( * ) PLANE_ANGLE_UNIT ( ) SI_UNIT ( $, .RADIAN. ) );
#105161 = ORIENTED_EDGE ( 'NONE', *, *, #125319, .T. ) ;
#105162 = ORIENTED_EDGE ( 'NONE', *, *, #25339, .F. ) ;
#105163 = CARTESIAN_POINT ( 'NONE',  ( 0.000000000000000000, 0.000000000000000000, 5.000000000000000000 ) ) ;
#105164 = ORIENTED_EDGE ( 'NONE', *, *, #41785, .T. ) ;
#105165 = CARTESIAN_POINT ( 'NONE',  ( -41.01844734635645295, 18.75929247661552424, 20.33588619593452762 ) ) ;
#105166 = CARTESIAN_POINT ( 'NONE',  ( 17.70025512860841488, -27.71228299555193786, 4.000000000000000000 ) ) ;
#105167 = CARTESIAN_POINT ( 'NONE',  ( 183.8247562798467527, -48.93522302958525216, -39.28544916627431149 ) ) ;
#105168 = EDGE_CURVE ( 'NONE', #67630, #27153, #91692, .T. ) ;
#105170 = ORIENTED_EDGE ( 'NONE', *, *, #98869, .F. ) ;
#105169 = VECTOR ( 'NONE', #44355, 1000.000000000000114 ) ;
#105171 = DIRECTION ( 'NONE',  ( -0.000000000000000000, -0.3543493200069152693, 0.9351131265310292928 ) ) ;
#105172 = FILL_AREA_STYLE_COLOUR ( '', #83702 ) ;
#105173 = CARTESIAN_POINT ( 'NONE',  ( -8.671830600776411657, -0.7407075233842683737, 4.000000000000000000 ) ) ;
#105174 = ORIENTED_EDGE ( 'NONE', *, *, #66223, .F. ) ;
#105175 = DIRECTION ( 'NONE',  ( 0.000000000000000000, 0.000000000000000000, 1.000000000000000000 ) ) ;
#105176 = LINE ( 'NONE', #5834, #23957 ) ;
#105177 = ORIENTED_EDGE ( 'NONE', *, *, #47870, .T. ) ;
#105179 = EDGE_LOOP ( 'NONE', ( #55188, #75810, #104662, #965 ) ) ;
#105178 = CARTESIAN_POINT ( 'NONE',  ( 13.08100000000000307, 3.174999999999998046, 4.000000000000000000 ) ) ;
#105180 = ORIENTED_EDGE ( 'NONE', *, *, #90629, .T. ) ;
#105181 = DIRECTION ( 'NONE',  ( -0.7071067811865487940, 0.7071067811865463515, 0.000000000000000000 ) ) ;
#105182 = VECTOR ( 'NONE', #33500, 1000.000000000000000 ) ;
#105183 = ORIENTED_EDGE ( 'NONE', *, *, #91318, .T. ) ;
#105184 = PLANE ( 'NONE',  #67457 ) ;
#105185 = LINE ( 'NONE', #73297, #142478 ) ;
#105186 = AXIS2_PLACEMENT_3D ( 'NONE', #34823, #22471, #79068 ) ;
#105187 = EDGE_CURVE ( 'NONE', #4701, #97256, #4614, .T. ) ;
#105188 = CARTESIAN_POINT ( 'NONE',  ( -29.99999999999979039, -3.033600742197705369, 5.000000000000000000 ) ) ;
#105189 = ORIENTED_EDGE ( 'NONE', *, *, #113518, .F. ) ;
#105190 = LINE ( 'NONE', #118182, #71615 ) ;
#105191 = EDGE_CURVE ( 'NONE', #42001, #34223, #47532, .T. ) ;
#105193 = CARTESIAN_POINT ( 'NONE',  ( -19.49999999999986500, 15.05218569542901541, 5.000000000000000000 ) ) ;
#105192 = VECTOR ( 'NONE', #30718, 999.9999999999998863 ) ;
#105194 = CARTESIAN_POINT ( 'NONE',  ( -25.82816939922334143, 21.75929247661549937, 4.000000000000000000 ) ) ;
#105195 = CARTESIAN_POINT ( 'NONE',  ( 33.48921356237309510, -27.52281430457078670, 5.000000000000000000 ) ) ;
#105196 = CARTESIAN_POINT ( 'NONE',  ( 0.000000000000000000, 0.000000000000000000, 5.000000000000000000 ) ) ;
#105197 = CARTESIAN_POINT ( 'NONE',  ( -27.18398860626900060, 28.73617430169806042, 5.000000000000000000 ) ) ;
#105198 = LINE ( 'NONE', #4390, #52952 ) ;
#105199 = DIRECTION ( 'NONE',  ( -1.000000000000000000, -0.000000000000000000, -0.000000000000000000 ) ) ;
#105201 = EDGE_CURVE ( 'NONE', #56830, #22851, #24300, .T. ) ;
#105200 = CARTESIAN_POINT ( 'NONE',  ( 31.92500000000001492, -3.269999999999992024, -40.00000000000000000 ) ) ;
#105203 = ADVANCED_FACE ( 'NONE', ( #78684 ), #46824, .F. ) ;
#105202 = EDGE_LOOP ( 'NONE', ( #102019, #14146, #41020, #30392 ) ) ;
#105204 = ORIENTED_EDGE ( 'NONE', *, *, #129354, .T. ) ;
#105205 = ORIENTED_EDGE ( 'NONE', *, *, #76119, .F. ) ;
#105206 = CARTESIAN_POINT ( 'NONE',  ( 114.3124999999999858, 5.819803920172571310, 5.819803920172575751 ) ) ;
#105207 = VERTEX_POINT ( 'NONE', #15521 ) ;
#105208 = AXIS2_PLACEMENT_3D ( 'NONE', #97686, #94804, #39772 ) ;
#105209 = ORIENTED_EDGE ( 'NONE', *, *, #137713, .F. ) ;
#105210 = ORIENTED_EDGE ( 'NONE', *, *, #80021, .F. ) ;
#105211 = FILL_AREA_STYLE ('',( #50842 ) ) ;
#105212 = CARTESIAN_POINT ( 'NONE',  ( -6.511686059284278016, 6.759292476615653023, 16.35960578974471247 ) ) ;
#105213 = ORIENTED_EDGE ( 'NONE', *, *, #42385, .T. ) ;
#105214 = DIRECTION ( 'NONE',  ( -0.7071067811865486830, -0.7071067811865464625, 0.000000000000000000 ) ) ;
#105215 = DIRECTION ( 'NONE',  ( 0.7071067811865487940, 0.7071067811865463515, 0.000000000000000000 ) ) ;
#105216 = EDGE_CURVE ( 'NONE', #40381, #136489, #58546, .T. ) ;
#105217 = FACE_OUTER_BOUND ( 'NONE', #35979, .T. ) ;
#105218 = DIRECTION ( 'NONE',  ( 0.7071067811865487940, 0.7071067811865463515, 0.000000000000000000 ) ) ;
#105219 = CARTESIAN_POINT ( 'NONE',  ( 114.3337635252314470, 6.110000000000001208, 1.122388791418549305E-15 ) ) ;
#105220 = ORIENTED_EDGE ( 'NONE', *, *, #64070, .F. ) ;
#105221 = EDGE_CURVE ( 'NONE', #133915, #76474, #73325, .T. ) ;
#105222 = CARTESIAN_POINT ( 'NONE',  ( 23.99999999999983302, -0.1606350220012988939, 4.664761815935144718 ) ) ;
#105223 = DIRECTION ( 'NONE',  ( 0.7071067811865487940, 0.7071067811865463515, 0.000000000000000000 ) ) ;
#105224 = DIRECTION ( 'NONE',  ( -0.000000000000000000, 0.3543493200069153248, 0.9351131265310292928 ) ) ;
#105225 = CARTESIAN_POINT ( 'NONE',  ( 83.64169371712955581, -2.130196079827424871, -7.949999999999998401 ) ) ;
#105226 = LINE ( 'NONE', #50150, #12765 ) ;
#105227 =( BOUNDED_CURVE ( )  B_SPLINE_CURVE ( 3, ( #93648, #105911, #8029, #84901 ),
 .UNSPECIFIED., .F., .T. ) 
 B_SPLINE_CURVE_WITH_KNOTS ( ( 4, 4 ),
 ( 4.446051736530363563, 4.712388980384695003 ),
 .UNSPECIFIED. ) 
 CURVE ( )  GEOMETRIC_REPRESENTATION_ITEM ( )  RATIONAL_B_SPLINE_CURVE ( ( 1.000000000000000000, 0.9940974367313476501, 0.9940974367313476501, 1.000000000000000000 ) ) 
 REPRESENTATION_ITEM ( '' )  );
#105228 = LINE ( 'NONE', #8718, #86242 ) ;
#105229 = AXIS2_PLACEMENT_3D ( 'NONE', #15257, #48646, #137080 ) ;
#105230 = CARTESIAN_POINT ( 'NONE',  ( 39.89169371712955581, 2.130196079827421762, 7.950000000000001066 ) ) ;
#105231 = EDGE_CURVE ( 'NONE', #133141, #15838, #8219, .T. ) ;
#105232 = DIRECTION ( 'NONE',  ( -0.6830127018922181881, 0.6830127018922202975, -0.2588190451025214056 ) ) ;
#105233 = VECTOR ( 'NONE', #133529, 1000.000000000000227 ) ;
#105234 = CARTESIAN_POINT ( 'NONE',  ( -12.69999999999998153, 0.000000000000000000, 2.500000000000000444 ) ) ;
#105235 = ORIENTED_EDGE ( 'NONE', *, *, #9452, .T. ) ;
#105236 = EDGE_LOOP ( 'NONE', ( #113940, #112147, #132410, #95278 ) ) ;
#105237 = AXIS2_PLACEMENT_3D ( 'NONE', #104255, #4920, #62225 ) ;
#105238 = CARTESIAN_POINT ( 'NONE',  ( 40.66666666666665719, 6.884901960086285300, 3.975000000000003642 ) ) ;
#105239 = ORIENTED_EDGE ( 'NONE', *, *, #128501, .F. ) ;
#105240 = AXIS2_PLACEMENT_3D ( 'NONE', #112256, #68078, #13617 ) ;
#105241 = DIRECTION ( 'NONE',  ( -1.000000000000000000, 0.000000000000000000, 0.000000000000000000 ) ) ;
#105242 = CARTESIAN_POINT ( 'NONE',  ( -48.29974487139158867, -27.71228299555239971, 4.000000000000000000 ) ) ;
#105243 = EDGE_CURVE ( 'NONE', #61782, #102663, #106105, .T. ) ;
#105244 = DIRECTION ( 'NONE',  ( 0.6830127018922180770, -0.6830127018922204085, -0.2588190451025213501 ) ) ;
#105245 = CARTESIAN_POINT ( 'NONE',  ( 0.1161069444170876042, 0.3999999999999995781, 2.220360628129161906 ) ) ;
#105246 = CARTESIAN_POINT ( 'NONE',  ( -51.48921356237309510, -27.52281430457091460, 5.000000000000000000 ) ) ;
#105247 = DIRECTION ( 'NONE',  ( -0.7071067811865486830, 0.7071067811865464625, 0.000000000000000000 ) ) ;
#105248 = CARTESIAN_POINT ( 'NONE',  ( 25.66709685856477563, -3.055000000000000160, -5.291415217122921177 ) ) ;
#105249 = ORIENTED_EDGE ( 'NONE', *, *, #83420, .F. ) ;
#105250 = LINE ( 'NONE', #5901, #43357 ) ;
#105251 = ORIENTED_EDGE ( 'NONE', *, *, #70594, .T. ) ;
#105252 = ADVANCED_FACE ( 'NONE', ( #84417 ), #73529, .F. ) ;
#105253 = CARTESIAN_POINT ( 'NONE',  ( -27.79289321881326558, -20.24070752338407431, 5.000000000000000000 ) ) ;
#105254 = FACE_OUTER_BOUND ( 'NONE', #65325, .T. ) ;
#105255 = FACE_OUTER_BOUND ( 'NONE', #5758, .T. ) ;
#105256 = PLANE ( 'NONE',  #71942 ) ;
#105257 = ORIENTED_EDGE ( 'NONE', *, *, #94279, .F. ) ;
#105258 = CARTESIAN_POINT ( 'NONE',  ( 51.33376352523143282, 6.110000000000001208, 1.122388791418549305E-15 ) ) ;
#105259 = ORIENTED_EDGE ( 'NONE', *, *, #768, .T. ) ;
#105260 = DIRECTION ( 'NONE',  ( 1.000000000000000000, 0.000000000000000000, 0.000000000000000000 ) ) ;
#105261 = LINE ( 'NONE', #84939, #57765 ) ;
#105262 = DIRECTION ( 'NONE',  ( -0.7071067811865486830, 0.7071067811865464625, 0.000000000000000000 ) ) ;
#105263 = ADVANCED_FACE ( 'NONE', ( #95257 ), #7520, .T. ) ;
#105264 = EDGE_CURVE ( 'NONE', #3523, #139938, #51781, .T. ) ;
#105265 = LINE ( 'NONE', #128461, #4645 ) ;
#105266 = EDGE_CURVE ( 'NONE', #67375, #132883, #101301, .T. ) ;
#105267 = CARTESIAN_POINT ( 'NONE',  ( 52.55793019189811588, 6.110000000000000320, -1.637169565754156064 ) ) ;
#105268 = ORIENTED_EDGE ( 'NONE', *, *, #3227, .T. ) ;
#105269 = DIRECTION ( 'NONE',  ( -0.000000000000000000, 0.000000000000000000, 1.000000000000000000 ) ) ;
#105270 = CARTESIAN_POINT ( 'NONE',  ( 34.49999999999976552, -4.535744391599457082, 4.994342998332164107 ) ) ;
#105271 = ORIENTED_EDGE ( 'NONE', *, *, #16681, .F. ) ;
#105272 = VERTEX_POINT ( 'NONE', #106842 ) ;
#105273 = CARTESIAN_POINT ( 'NONE',  ( 14.08979869950237251, -1.618973607074033705, -40.00000000000000000 ) ) ;
#105274 = ORIENTED_EDGE ( 'NONE', *, *, #114205, .T. ) ;
#105275 = VECTOR ( 'NONE', #25408, 1000.000000000000000 ) ;
#105276 = CARTESIAN_POINT ( 'NONE',  ( 60.45419371712955581, 6.884901960086283523, 3.975000000000002753 ) ) ;
#105277 = VERTEX_POINT ( 'NONE', #72855 ) ;
#105278 = CARTESIAN_POINT ( 'NONE',  ( 44.12086038379622721, -6.884901960086286188, 3.974999999999997424 ) ) ;
#105279 = CARTESIAN_POINT ( 'NONE',  ( -21.48921356237309155, -27.52281430457070499, 5.000000000000000000 ) ) ;
#105280 = FACE_BOUND ( 'NONE', #134070, .T. ) ;
#105281 = CARTESIAN_POINT ( 'NONE',  ( -18.75860074219783868, 21.72500000000000853, 5.000000000000000000 ) ) ;
#105282 = CARTESIAN_POINT ( 'NONE',  ( -54.48921356237310221, -27.52281430457093236, 5.000000000000000000 ) ) ;
#105283 = LINE ( 'NONE', #138648, #119708 ) ;
#105284 = ORIENTED_EDGE ( 'NONE', *, *, #27472, .F. ) ;
#105285 = PLANE ( 'NONE',  #20341 ) ;
#105287 = ORIENTED_EDGE ( 'NONE', *, *, #108935, .T. ) ;
#105286 = DIRECTION ( 'NONE',  ( -1.000000000000000000, 0.000000000000000000, -0.000000000000000000 ) ) ;
#105288 = ORIENTED_EDGE ( 'NONE', *, *, #127861, .T. ) ;
#105289 = CARTESIAN_POINT ( 'NONE',  ( 6.938893903907228378E-15, -16.06887692260765377, 4.000000000000000000 ) ) ;
#105290 = ORIENTED_EDGE ( 'NONE', *, *, #9673, .F. ) ;
#105291 = VECTOR ( 'NONE', #116641, 1000.000000000000000 ) ;
#105292 = ORIENTED_EDGE ( 'NONE', *, *, #4533, .F. ) ;
#105293 = CARTESIAN_POINT ( 'NONE',  ( 66.70376352523143737, 6.109999999999998543, 1.122388791418548911E-15 ) ) ;
#105294 = VERTEX_POINT ( 'NONE', #117010 ) ;
#105295 = DIRECTION ( 'NONE',  ( 0.3543493200069162685, -0.000000000000000000, -0.9351131265310288487 ) ) ;
#105296 = VECTOR ( 'NONE', #82778, 1000.000000000000000 ) ;
#105297 = DIRECTION ( 'NONE',  ( -0.7071067811865486830, -0.7071067811865464625, 0.000000000000000000 ) ) ;
#105298 = EDGE_CURVE ( 'NONE', #95984, #101438, #85099, .T. ) ;
#105299 = EDGE_LOOP ( 'NONE', ( #7561, #40464, #67163, #129933 ) ) ;
#105300 = PRESENTATION_STYLE_ASSIGNMENT (( #114037 ) ) ;
#105301 = DIRECTION ( 'NONE',  ( 0.000000000000000000, 0.3543493200069153248, 0.9351131265310291818 ) ) ;
#105302 = CARTESIAN_POINT ( 'NONE',  ( -13.49999999999990408, 15.43112307739202294, 4.000000000000000000 ) ) ;
#105303 = LINE ( 'NONE', #29175, #57430 ) ;
#105304 = DIRECTION ( 'NONE',  ( -0.6830127018922181881, 0.6830127018922202975, -0.2588190451025214056 ) ) ;
#105305 = PLANE ( 'NONE',  #108787 ) ;
#105306 = ORIENTED_EDGE ( 'NONE', *, *, #83930, .T. ) ;
#105307 = ORIENTED_EDGE ( 'NONE', *, *, #7093, .F. ) ;
#105308 = CARTESIAN_POINT ( 'NONE',  ( 24.18398860626899705, 28.73617430169804265, 5.000000000000000000 ) ) ;
#105309 = DIRECTION ( 'NONE',  ( 0.7071067811865487940, 0.7071067811865463515, 0.000000000000000000 ) ) ;
#105310 = ORIENTED_EDGE ( 'NONE', *, *, #138410, .F. ) ;
#105311 = EDGE_LOOP ( 'NONE', ( #129716, #129989, #108348, #71401 ) ) ;
#105312 = ORIENTED_EDGE ( 'NONE', *, *, #135044, .F. ) ;
#105313 = LINE ( 'NONE', #46156, #69874 ) ;
#105314 = EDGE_CURVE ( 'NONE', #25822, #57637, #71383, .T. ) ;
#105315 = ADVANCED_FACE ( 'NONE', ( #29996 ), #74235, .F. ) ;
#105316 = CARTESIAN_POINT ( 'NONE',  ( 30.16666666666666075, 6.884901960086285300, 3.975000000000003642 ) ) ;
#105317 = ORIENTED_EDGE ( 'NONE', *, *, #115701, .F. ) ;
#105318 = CARTESIAN_POINT ( 'NONE',  ( -54.18398860626899705, 28.73617430169825226, 5.000000000000000000 ) ) ;
#105319 = VECTOR ( 'NONE', #56946, 1000.000000000000000 ) ;
#105320 = CYLINDRICAL_SURFACE ( 'NONE', #30587, 3.000000000000002665 ) ;
#105321 = AXIS2_PLACEMENT_3D ( 'NONE', #37960, #49567, #25624 ) ;
#105322 = CARTESIAN_POINT ( 'NONE',  ( 6.483736474768551972, -5.808823158059035485, -5.808823158059033709 ) ) ;
#105323 = CARTESIAN_POINT ( 'NONE',  ( -21.29974487139158512, -27.71228299555221142, 4.000000000000000000 ) ) ;
#105324 = ORIENTED_EDGE ( 'NONE', *, *, #58519, .T. ) ;
#105326 = EDGE_CURVE ( 'NONE', #59374, #52592, #60533, .T. ) ;
#105325 = VECTOR ( 'NONE', #36131, 1000.000000000000000 ) ;
#105327 = CARTESIAN_POINT ( 'NONE',  ( 41.99451991528749062, 28.92564299267967343, 4.000000000000000000 ) ) ;
#105328 = FACE_OUTER_BOUND ( 'NONE', #103033, .T. ) ;
#105330 = EDGE_LOOP ( 'NONE', ( #121228, #86124, #10736, #88040 ) ) ;
#105329 = CARTESIAN_POINT ( 'NONE',  ( -5.999999999999950262, -13.44781430457068971, 5.000000000000000000 ) ) ;
#105331 = PLANE ( 'NONE',  #77177 ) ;
#105332 = ORIENTED_EDGE ( 'NONE', *, *, #142024, .T. ) ;
#105333 = LINE ( 'NONE', #126371, #126045 ) ;
#105334 = CARTESIAN_POINT ( 'NONE',  ( 0.000000000000000000, 0.000000000000000000, 5.000000000000000000 ) ) ;
#105335 = CARTESIAN_POINT ( 'NONE',  ( 107.8958333333333286, -2.130196079827407996, 7.950000000000009059 ) ) ;
#105336 = EDGE_CURVE ( 'NONE', #84329, #121662, #38747, .T. ) ;
#105337 = ORIENTED_EDGE ( 'NONE', *, *, #110521, .F. ) ;
#105338 = PLANE ( 'NONE',  #98122 ) ;
#105339 = LINE ( 'NONE', #94459, #95139 ) ;
#105340 = PLANE ( 'NONE',  #32847 ) ;
#105341 = EDGE_LOOP ( 'NONE', ( #32940, #93383, #84142 ) ) ;
#105342 = EDGE_CURVE ( 'NONE', #118163, #43549, #38348, .T. ) ;
#105343 = DIRECTION ( 'NONE',  ( -0.7071067811865486830, 0.7071067811865464625, 0.000000000000000000 ) ) ;
#105344 = CARTESIAN_POINT ( 'NONE',  ( 34.42499999999998295, 22.22500000000000142, 0.4999999999999995559 ) ) ;
#105345 = DIRECTION ( 'NONE',  ( -1.000000000000000000, 0.000000000000000000, 0.000000000000000000 ) ) ;
#105346 = DIRECTION ( 'NONE',  ( 0.6830127018922181881, 0.6830127018922202975, -0.2588190451025214056 ) ) ;
#105347 = DIRECTION ( 'NONE',  ( -0.000000000000000000, 0.3543493200069153248, 0.9351131265310292928 ) ) ;
#105348 = ORIENTED_EDGE ( 'NONE', *, *, #36805, .F. ) ;
#105349 = ORIENTED_EDGE ( 'NONE', *, *, #80473, .F. ) ;
#105350 = DIRECTION ( 'NONE',  ( 0.6830127018922180770, -0.6830127018922204085, -0.2588190451025213501 ) ) ;
#105351 = DIRECTION ( 'NONE',  ( 0.7071067811865487940, 0.7071067811865463515, -0.000000000000000000 ) ) ;
#105352 = CARTESIAN_POINT ( 'NONE',  ( 6.249569808101886892, 3.967499999999998916, 6.871911579029510442 ) ) ;
#105353 = CARTESIAN_POINT ( 'NONE',  ( 17.20710678118642534, 15.75929247661555443, 5.000000000000000000 ) ) ;
#105354 = DIRECTION ( 'NONE',  ( 1.000000000000000000, 0.000000000000000000, 0.000000000000000000 ) ) ;
#105355 = CARTESIAN_POINT ( 'NONE',  ( 51.18398860626899705, 28.73617430169823095, 5.000000000000000000 ) ) ;
#105356 = DIRECTION ( 'NONE',  ( -0.7071067811865487940, 0.7071067811865463515, -0.000000000000000000 ) ) ;
#105357 = ORIENTED_EDGE ( 'NONE', *, *, #24427, .T. ) ;
#105358 = EDGE_CURVE ( 'NONE', #12779, #56087, #64072, .T. ) ;
#105359 = FACE_OUTER_BOUND ( 'NONE', #63760, .T. ) ;
#105360 = DIRECTION ( 'NONE',  ( 0.3543493200069162685, -0.000000000000000000, -0.9351131265310288487 ) ) ;
#105361 = CARTESIAN_POINT ( 'NONE',  ( 12.48921356237309155, -27.52281430457064104, 5.000000000000000000 ) ) ;
#105362 = FACE_OUTER_BOUND ( 'NONE', #765, .T. ) ;
#105363 = CARTESIAN_POINT ( 'NONE',  ( 51.24543019189811588, -5.291415217122919401, -3.055000000000000604 ) ) ;
#105364 = CARTESIAN_POINT ( 'NONE',  ( -29.99999999999979039, 16.55218569542899587, 5.000000000000000000 ) ) ;
#105365 = EDGE_CURVE ( 'NONE', #119435, #118785, #131474, .T. ) ;
#105366 = ADVANCED_FACE ( 'NONE', ( #119839 ), #66095, .T. ) ;
#105367 = ORIENTED_EDGE ( 'NONE', *, *, #49108, .T. ) ;
#105368 = DIRECTION ( 'NONE',  ( 0.7071067811865487940, -0.7071067811865463515, 0.000000000000000000 ) ) ;
#105369 = VERTEX_POINT ( 'NONE', #90662 ) ;
#105370 = ORIENTED_EDGE ( 'NONE', *, *, #101268, .T. ) ;
#105371 = LINE ( 'NONE', #4574, #110317 ) ;
#105372 = EDGE_CURVE ( 'NONE', #8723, #43368, #77977, .T. ) ;
#105373 = DIRECTION ( 'NONE',  ( 1.000000000000000000, 0.000000000000000000, 0.000000000000000000 ) ) ;
#105374 = DIRECTION ( 'NONE',  ( 1.000000000000000000, -0.000000000000000000, -0.000000000000000000 ) ) ;
#105375 = LINE ( 'NONE', #94495, #58003 ) ;
#105376 = ADVANCED_FACE ( 'NONE', ( #41590 ), #84613, .T. ) ;
#105377 = CARTESIAN_POINT ( 'NONE',  ( -13.49999999999990408, -16.53360074219757081, 5.000000000000000000 ) ) ;
#105378 = DIRECTION ( 'NONE',  ( 0.6830127018922181881, 0.6830127018922202975, -0.2588190451025214056 ) ) ;
#105379 = ORIENTED_EDGE ( 'NONE', *, *, #120073, .F. ) ;
#105380 = ADVANCED_FACE ( 'NONE', ( #76384 ), #43742, .T. ) ;
#105381 = CARTESIAN_POINT ( 'NONE',  ( -1.171830600776462061, 3.759292476615678336, 4.000000000000000000 ) ) ;
#105382 = DIRECTION ( 'NONE',  ( -1.000000000000000000, -1.224606353822377258E-16, -0.000000000000000000 ) ) ;
#105383 = UNCERTAINTY_MEASURE_WITH_UNIT (LENGTH_MEASURE( 1.000000000000000082E-05 ), #89244, 'distance_accuracy_value', 'NONE');
#105384 = LINE ( 'NONE', #95943, #110340 ) ;
#105385 = DIRECTION ( 'NONE',  ( -0.7071067811865486830, -0.7071067811865464625, 0.000000000000000000 ) ) ;
#105386 = DIRECTION ( 'NONE',  ( 0.6830127018922181881, 0.6830127018922202975, -0.2588190451025214056 ) ) ;
#105387 = CARTESIAN_POINT ( 'NONE',  ( 66.72502705046289861, 5.819803920172573086, -5.819803920172572198 ) ) ;
#105388 = VECTOR ( 'NONE', #75667, 1000.000000000000000 ) ;
#105389 = DIRECTION ( 'NONE',  ( -0.7071067811865487940, 0.7071067811865463515, -0.000000000000000000 ) ) ;
#105390 = ORIENTED_EDGE ( 'NONE', *, *, #111033, .F. ) ;
#105391 = VERTEX_POINT ( 'NONE', #119147 ) ;
#105392 = CARTESIAN_POINT ( 'NONE',  ( 64.58333333333332860, 6.884901960086290629, -3.974999999999994316 ) ) ;
#105393 = EDGE_CURVE ( 'NONE', #85630, #68517, #11075, .T. ) ;
#105394 = LINE ( 'NONE', #17659, #26194 ) ;
#105395 = AXIS2_PLACEMENT_3D ( 'NONE', #45387, #89564, #78697 ) ;
#105396 = CARTESIAN_POINT ( 'NONE',  ( 15.18398860626900237, 28.73617430169797871, 5.000000000000000000 ) ) ;
#105397 = ORIENTED_EDGE ( 'NONE', *, *, #39277, .T. ) ;
#105398 = EDGE_CURVE ( 'NONE', #77014, #10464, #120548, .T. ) ;
#105399 = CARTESIAN_POINT ( 'NONE',  ( 32.49999999999998579, 0.000000000000000000, -7.950000000000000178 ) ) ;
#105400 = VECTOR ( 'NONE', #39239, 1000.000000000000227 ) ;
#105401 = CARTESIAN_POINT ( 'NONE',  ( 35.34328999833765295, 3.759292476615685441, 13.27625715073273582 ) ) ;
#105402 = CARTESIAN_POINT ( 'NONE',  ( 58.33376352523143993, 6.110000000000001208, 1.122388791418549305E-15 ) ) ;
#105403 = LINE ( 'NONE', #17669, #142899 ) ;
#105404 = EDGE_LOOP ( 'NONE', ( #33919, #110626, #99385, #120478, #20823, #77200, #88973, #96500 ) ) ;
#105405 = EDGE_LOOP ( 'NONE', ( #43306, #68062, #15865, #100951, #71566, #101120 ) ) ;
#105406 = PLANE ( 'NONE',  #23793 ) ;
#105407 = DIRECTION ( 'NONE',  ( -0.7071067811865486830, -0.7071067811865464625, 0.000000000000000000 ) ) ;
#105408 = DIRECTION ( 'NONE',  ( -0.6830127018922180770, -0.6830127018922204085, -0.2588190451025213501 ) ) ;
#105409 = LINE ( 'NONE', #6776, #102131 ) ;
#105411 = ORIENTED_EDGE ( 'NONE', *, *, #130115, .T. ) ;
#105410 = CARTESIAN_POINT ( 'NONE',  ( 6.005480084712508493, 28.92564299267933947, 4.000000000000000000 ) ) ;
#105412 = CARTESIAN_POINT ( 'NONE',  ( 36.29974487139159578, -27.71228299555231445, 4.000000000000000000 ) ) ;
#105413 = FACE_OUTER_BOUND ( 'NONE', #40792, .T. ) ;
#105414 = LINE ( 'NONE', #94535, #10050 ) ;
#105415 = EDGE_CURVE ( 'NONE', #27902, #131125, #13759, .T. ) ;
#105416 = CARTESIAN_POINT ( 'NONE',  ( 8.010880286539427075, -22.02621442084248571, 4.990779571109219326 ) ) ;
#105417 = VECTOR ( 'NONE', #39092, 999.9999999999998863 ) ;
#105418 = EDGE_CURVE ( 'NONE', #22337, #36162, #19831, .T. ) ;
#105419 = ORIENTED_EDGE ( 'NONE', *, *, #9579, .T. ) ;
#105420 = ADVANCED_FACE ( 'NONE', ( #141640 ), #75396, .T. ) ;
#105421 = VERTEX_POINT ( 'NONE', #87250 ) ;
#105422 = STYLED_ITEM ( 'NONE', ( #13075 ), #6157 ) ;
#105423 = FACE_OUTER_BOUND ( 'NONE', #48767, .T. ) ;
#105424 = CARTESIAN_POINT ( 'NONE',  ( 14.20710678118644665, -14.24070752338414003, 5.000000000000000000 ) ) ;
#105425 = CARTESIAN_POINT ( 'NONE',  ( -27.48921356237309155, -27.52281430457074762, 5.000000000000000000 ) ) ;
#105426 = CARTESIAN_POINT ( 'NONE',  ( 72.85002705046289861, -5.819803920172573086, -5.819803920172573086 ) ) ;
#105427 = EDGE_LOOP ( 'NONE', ( #138714, #91383, #87163, #38400 ) ) ;
#105428 = ORIENTED_EDGE ( 'NONE', *, *, #142033, .T. ) ;
#105429 = VECTOR ( 'NONE', #61543, 1000.000000000000000 ) ;
#105430 = DIRECTION ( 'NONE',  ( -1.000000000000000000, -0.000000000000000000, -0.000000000000000000 ) ) ;
#105432 = ADVANCED_FACE ( 'NONE', ( #86549 ), #108971, .T. ) ;
#105431 = DIRECTION ( 'NONE',  ( 0.000000000000000000, -1.000000000000000000, 0.000000000000000000 ) ) ;
#105433 = ORIENTED_EDGE ( 'NONE', *, *, #71221, .T. ) ;
#105434 = ORIENTED_EDGE ( 'NONE', *, *, #37144, .T. ) ;
#105435 = LINE ( 'NONE', #138085, #123141 ) ;
#105436 = VERTEX_POINT ( 'NONE', #46467 ) ;
#105437 = CARTESIAN_POINT ( 'NONE',  ( 61.62086038379622721, -6.884901960086286188, 3.974999999999997424 ) ) ;
#105438 = FACE_OUTER_BOUND ( 'NONE', #85263, .T. ) ;
#105439 = FACE_BOUND ( 'NONE', #111130, .T. ) ;
#105440 = PRESENTATION_STYLE_ASSIGNMENT (( #116335 ) ) ;
#105441 = CYLINDRICAL_SURFACE ( 'NONE', #2610, 0.5000000000000004441 ) ;
#105443 = ORIENTED_EDGE ( 'NONE', *, *, #78802, .F. ) ;
#105442 = CARTESIAN_POINT ( 'NONE',  ( 12.19999999999999574, -27.68200100598810565, 15.59110741220538188 ) ) ;
#105444 = APPLICATION_PROTOCOL_DEFINITION ( 'draft international standard', 'automotive_design', 1998, #80048 ) ;
#105445 = EDGE_LOOP ( 'NONE', ( #58103, #72320, #99230, #74176 ) ) ;
#105446 = VERTEX_POINT ( 'NONE', #79817 ) ;
#105447 = CARTESIAN_POINT ( 'NONE',  ( 96.45376352523145158, -6.109999999999998543, -3.741295971395162543E-16 ) ) ;
#105448 = VERTEX_POINT ( 'NONE', #130781 ) ;
#105449 = CARTESIAN_POINT ( 'NONE',  ( 30.18398860626900060, 28.73617430169808173, 5.000000000000000000 ) ) ;
#105450 = ADVANCED_FACE ( 'NONE', ( #53936 ), #98131, .F. ) ;
#105451 = DIRECTION ( 'NONE',  ( 0.7071067811865487940, 0.7071067811865463515, 0.000000000000000000 ) ) ;
#105452 = CARTESIAN_POINT ( 'NONE',  ( -10.49999999999992539, -2.947814304570798960, 5.000000000000000000 ) ) ;
#105453 = DIRECTION ( 'NONE',  ( -0.7071067811865487940, 0.7071067811865463515, -0.000000000000000000 ) ) ;
#105454 = ORIENTED_EDGE ( 'NONE', *, *, #118743, .F. ) ;
#105455 = DIRECTION ( 'NONE',  ( 0.000000000000000000, 1.000000000000000000, 0.000000000000000000 ) ) ;
#105456 = LINE ( 'NONE', #6120, #101032 ) ;
#105457 = FACE_OUTER_BOUND ( 'NONE', #115327, .T. ) ;
#105459 = DIRECTION ( 'NONE',  ( -0.000000000000000000, 0.000000000000000000, 1.000000000000000000 ) ) ;
#105458 = CARTESIAN_POINT ( 'NONE',  ( 5.999999999999960032, 1.931123077392165488, 4.000000000000000000 ) ) ;
#105460 =( NAMED_UNIT ( * ) SI_UNIT ( $, .STERADIAN. ) SOLID_ANGLE_UNIT ( ) );
#105461 = FACE_OUTER_BOUND ( 'NONE', #24054, .T. ) ;
#105462 = DIRECTION ( 'NONE',  ( 0.7071067811865487940, 0.7071067811865463515, 0.000000000000000000 ) ) ;
#105463 = VERTEX_POINT ( 'NONE', #69632 ) ;
#105464 = LINE ( 'NONE', #115600, #130571 ) ;
#105465 =( BOUNDED_CURVE ( )  B_SPLINE_CURVE ( 3, ( #82746, #38520, #126930, #5853 ),
 .UNSPECIFIED., .F., .T. ) 
 B_SPLINE_CURVE_WITH_KNOTS ( ( 4, 4 ),
 ( 5.043186909253407180, 5.074607125596362067 ),
 .UNSPECIFIED. ) 
 CURVE ( )  GEOMETRIC_REPRESENTATION_ITEM ( )  RATIONAL_B_SPLINE_CURVE ( ( 1.000000000000000000, 0.9999177325257868620, 0.9999177325257868620, 1.000000000000000000 ) ) 
 REPRESENTATION_ITEM ( '' )  );
#105466 = DIRECTION ( 'NONE',  ( -0.7071067811865486830, 0.7071067811865464625, 0.000000000000000000 ) ) ;
#105467 = ADVANCED_FACE ( 'NONE', ( #91379 ), #36091, .T. ) ;
#105468 = ORIENTED_EDGE ( 'NONE', *, *, #58486, .T. ) ;
#105469 = VERTEX_POINT ( 'NONE', #4266 ) ;
#105470 = EDGE_CURVE ( 'NONE', #44113, #80548, #116665, .T. ) ;
#105471 = EDGE_CURVE ( 'NONE', #23207, #69646, #25367, .T. ) ;
#105472 = VERTEX_POINT ( 'NONE', #114518 ) ;
#105473 = CARTESIAN_POINT ( 'NONE',  ( 45.06293019189811133, 1.637169565754157174, 6.110000000000002984 ) ) ;
#105474 = ORIENTED_EDGE ( 'NONE', *, *, #55099, .T. ) ;
#105475 = ADVANCED_FACE ( 'NONE', ( #82622 ), #37707, .F. ) ;
#105476 = EDGE_CURVE ( 'NONE', #80926, #43625, #2902, .T. ) ;
#105477 = VECTOR ( 'NONE', #84078, 1000.000000000000000 ) ;
#105478 = CARTESIAN_POINT ( 'NONE',  ( 12.73330628287043886, -6.094999999999989981, -1.633150327867689100 ) ) ;
#105479 =( LENGTH_UNIT ( ) NAMED_UNIT ( * ) SI_UNIT ( .MILLI., .METRE. ) );
#105480 = EDGE_LOOP ( 'NONE', ( #62923, #37949, #13362, #54488 ) ) ;
#105481 = AXIS2_PLACEMENT_3D ( 'NONE', #98490, #99926, #108617 ) ;
#105482 = EDGE_CURVE ( 'NONE', #33763, #27758, #135624, .T. ) ;
#105483 = DIRECTION ( 'NONE',  ( -0.5735764363510503783, -0.8191520442889886899, 0.000000000000000000 ) ) ;
#105484 = ORIENTED_EDGE ( 'NONE', *, *, #88597, .T. ) ;
#105485 = LINE ( 'NONE', #138865, #32564 ) ;
#105486 = PLANE ( 'NONE',  #98402 ) ;
#105488 = ORIENTED_EDGE ( 'NONE', *, *, #50014, .T. ) ;
#105487 = LINE ( 'NONE', #83047, #137402 ) ;
#105489 = ORIENTED_EDGE ( 'NONE', *, *, #128422, .F. ) ;
#105490 = CARTESIAN_POINT ( 'NONE',  ( -60.48921356237309510, -27.52281430457097500, 5.000000000000000000 ) ) ;
#105491 = DIRECTION ( 'NONE',  ( -0.7071067811865487940, 0.7071067811865463515, -0.000000000000000000 ) ) ;
#105492 = ADVANCED_FACE ( 'NONE', ( #48564 ), #27497, .F. ) ;
#105493 = EDGE_LOOP ( 'NONE', ( #116143, #157, #108916, #141873 ) ) ;
#105494 = PLANE ( 'NONE',  #15641 ) ;
#105495 = ORIENTED_EDGE ( 'NONE', *, *, #42325, .F. ) ;
#105496 = VERTEX_POINT ( 'NONE', #93496 ) ;
#105497 = VERTEX_POINT ( 'NONE', #138430 ) ;
#105498 = ORIENTED_EDGE ( 'NONE', *, *, #95589, .T. ) ;
#105499 = LINE ( 'NONE', #17768, #137450 ) ;
#105500 = EDGE_CURVE ( 'NONE', #7972, #78703, #105075, .T. ) ;
#105501 = DIRECTION ( 'NONE',  ( 0.000000000000000000, 1.000000000000000000, 0.000000000000000000 ) ) ;
#105502 = CARTESIAN_POINT ( 'NONE',  ( 27.18398860626900060, 28.73617430169806042, 5.000000000000000000 ) ) ;
#105503 = LINE ( 'NONE', #83067, #131665 ) ;
#105504 = ORIENTED_EDGE ( 'NONE', *, *, #135373, .T. ) ;
#105505 = CARTESIAN_POINT ( 'NONE',  ( 65.89583333333332860, -2.130196079827427091, 7.949999999999998401 ) ) ;
#105506 = ORIENTED_EDGE ( 'NONE', *, *, #120577, .T. ) ;
#105507 = EDGE_CURVE ( 'NONE', #140149, #37103, #92048, .T. ) ;
#105508 = DIRECTION ( 'NONE',  ( -0.6830127018922181881, 0.6830127018922202975, -0.2588190451025214056 ) ) ;
#105509 = AXIS2_PLACEMENT_3D ( 'NONE', #20000, #109166, #76570 ) ;
#105510 = CARTESIAN_POINT ( 'NONE',  ( 27.97873647476855297, -5.808823158059033709, 5.808823158059035485 ) ) ;
#105511 = CARTESIAN_POINT ( 'NONE',  ( 8.588385094051632862, 22.22500000000001208, 4.777194822843816802 ) ) ;
#105512 = VECTOR ( 'NONE', #73364, 999.9999999999998863 ) ;
#105513 = CARTESIAN_POINT ( 'NONE',  ( 97.25000000000000000, -9.735942053221458872E-16, 7.950000000000000178 ) ) ;
#105514 = VECTOR ( 'NONE', #106885, 1000.000000000000000 ) ;
#105515 = CARTESIAN_POINT ( 'NONE',  ( 0.000000000000000000, 9.735942053221458872E-16, -7.950000000000000178 ) ) ;
#105516 = VERTEX_POINT ( 'NONE', #58787 ) ;
#105517 = VECTOR ( 'NONE', #2138, 1000.000000000000000 ) ;
#105518 = ORIENTED_EDGE ( 'NONE', *, *, #41735, .T. ) ;
#105520 = ORIENTED_EDGE ( 'NONE', *, *, #100140, .T. ) ;
#105519 = EDGE_CURVE ( 'NONE', #60169, #8640, #115198, .T. ) ;
#105521 = CARTESIAN_POINT ( 'NONE',  ( 0.000000000000000000, 1.071565949253934124E-15, 8.000000000000001776 ) ) ;
#105522 = CARTESIAN_POINT ( 'NONE',  ( 6.471592354503322042, 2.500000000000001332, 0.000000000000000000 ) ) ;
#105523 = LINE ( 'NONE', #94646, #43016 ) ;
#105524 = VECTOR ( 'NONE', #44050, 1000.000000000000000 ) ;
#105525 = CARTESIAN_POINT ( 'NONE',  ( 34.92499999999998295, -21.72500000000000142, 5.000000000000000000 ) ) ;
#105526 =( LENGTH_UNIT ( ) NAMED_UNIT ( * ) SI_UNIT ( .MILLI., .METRE. ) );
#105527 = CARTESIAN_POINT ( 'NONE',  ( 75.01626352523142316, -4.472830434245839371, 4.472830434245839371 ) ) ;
#105528 = CARTESIAN_POINT ( 'NONE',  ( 81.20833333333332860, -3.974999999999999201, -6.884901960086287964 ) ) ;
#105529 = EDGE_CURVE ( 'NONE', #92514, #127270, #102953, .T. ) ;
#105530 = CARTESIAN_POINT ( 'NONE',  ( -24.48921356237309510, -27.52281430457072631, 5.000000000000000000 ) ) ;
#105531 = DIRECTION ( 'NONE',  ( -0.000000000000000000, -0.3543493200069152693, 0.9351131265310292928 ) ) ;
#105532 = LINE ( 'NONE', #6193, #115913 ) ;
#105533 = EDGE_CURVE ( 'NONE', #18088, #31683, #34358, .T. ) ;
#105534 = DIRECTION ( 'NONE',  ( -0.7071067811865486830, -0.7071067811865464625, -0.000000000000000000 ) ) ;
#105535 = VERTEX_POINT ( 'NONE', #60170 ) ;
#105536 = DIRECTION ( 'NONE',  ( 0.7071067811865487940, 0.7071067811865463515, 0.000000000000000000 ) ) ;
#105537 = ORIENTED_EDGE ( 'NONE', *, *, #28303, .T. ) ;
#105538 = EDGE_CURVE ( 'NONE', #6466, #138961, #15194, .T. ) ;
#105539 = DIRECTION ( 'NONE',  ( 0.3543493200069162685, -0.000000000000000000, -0.9351131265310288487 ) ) ;
#105541 = ORIENTED_EDGE ( 'NONE', *, *, #12605, .F. ) ;
#105540 = CARTESIAN_POINT ( 'NONE',  ( 2.207106781186534139, 3.759292476615678336, 5.000000000000000000 ) ) ;
#105542 = CARTESIAN_POINT ( 'NONE',  ( -20.99999999999985789, -5.527737879153202805, -7.983877177622320076 ) ) ;
#105543 = ORIENTED_EDGE ( 'NONE', *, *, #47581, .T. ) ;
#105544 = ORIENTED_EDGE ( 'NONE', *, *, #27636, .F. ) ;
#105545 = FACE_OUTER_BOUND ( 'NONE', #143127, .T. ) ;
#105546 = LINE ( 'NONE', #138202, #81528 ) ;
#105547 = CARTESIAN_POINT ( 'NONE',  ( 6.229065384000522343, 3.821174125832445049E-16, 0.000000000000000000 ) ) ;
#105548 = CARTESIAN_POINT ( 'NONE',  ( 92.10002705046289861, 5.819803920172570422, 5.819803920172574863 ) ) ;
#105549 = CARTESIAN_POINT ( 'NONE',  ( 71.00000000000000000, 0.000000000000000000, -7.950000000000000178 ) ) ;
#105550 = CYLINDRICAL_SURFACE ( 'NONE', #127047, 1.320799999999990870 ) ;
#105551 = ORIENTED_EDGE ( 'NONE', *, *, #138606, .F. ) ;
#105552 = ADVANCED_FACE ( 'NONE', ( #60913 ), #5737, .F. ) ;
#105553 = LINE ( 'NONE', #139671, #132605 ) ;
#105554 = DIRECTION ( 'NONE',  ( -0.000000000000000000, -0.3543493200069152693, 0.9351131265310292928 ) ) ;
#105555 = CARTESIAN_POINT ( 'NONE',  ( 26.10416666666666430, -1.633150327867691987, -6.094999999999989093 ) ) ;
#105556 = DIRECTION ( 'NONE',  ( -0.7071067811865486830, -0.7071067811865464625, -0.000000000000000000 ) ) ;
#105557 = AXIS2_PLACEMENT_3D ( 'NONE', #92542, #93986, #127330 ) ;
#105558 = LINE ( 'NONE', #127324, #81562 ) ;
#105559 = EDGE_LOOP ( 'NONE', ( #66242, #138193, #15732, #113120, #88330 ) ) ;
#105560 = EDGE_CURVE ( 'NONE', #135168, #8423, #94186, .T. ) ;
#105561 = DIRECTION ( 'NONE',  ( -0.000000000000000000, 0.000000000000000000, 1.000000000000000000 ) ) ;
#105562 = EDGE_LOOP ( 'NONE', ( #126941, #28469, #58085, #30063 ) ) ;
#105563 = CARTESIAN_POINT ( 'NONE',  ( 88.81293019189809002, -1.637169565754159617, -6.110000000000001208 ) ) ;
#105564 = PLANE ( 'NONE',  #128757 ) ;
#105565 = DIRECTION ( 'NONE',  ( -1.000000000000000000, -1.224606353822377258E-16, -0.000000000000000000 ) ) ;
#105566 = DIRECTION ( 'NONE',  ( -1.000000000000000000, -0.000000000000000000, -0.000000000000000000 ) ) ;
#105567 = ORIENTED_EDGE ( 'NONE', *, *, #60481, .T. ) ;
#105568 = CARTESIAN_POINT ( 'NONE',  ( 24.41159235450331977, 9.902892378096218942E-16, 0.000000000000000000 ) ) ;
#105569 = FACE_OUTER_BOUND ( 'NONE', #49393, .T. ) ;
#105570 = CARTESIAN_POINT ( 'NONE',  ( 34.92499999999998295, 22.06445279868698250, 5.060837336147044674 ) ) ;
#105571 = EDGE_CURVE ( 'NONE', #119991, #122630, #71050, .T. ) ;
#105573 = ORIENTED_EDGE ( 'NONE', *, *, #10075, .T. ) ;
#105572 = FACE_OUTER_BOUND ( 'NONE', #107269, .T. ) ;
#105574 = FACE_OUTER_BOUND ( 'NONE', #113675, .T. ) ;
#105575 = LINE ( 'NONE', #128092, #3656 ) ;
#105576 = CARTESIAN_POINT ( 'NONE',  ( 1.862596602551424896, -5.584750846682028147, 2.792454972228691989 ) ) ;
#105577 = PLANE ( 'NONE',  #37675 ) ;
#105578 = EDGE_LOOP ( 'NONE', ( #62096, #57518, #81101, #71425 ) ) ;
#105579 = VECTOR ( 'NONE', #23638, 1000.000000000000000 ) ;
#105580 = EDGE_CURVE ( 'NONE', #45800, #123719, #118802, .T. ) ;
#105581 = ORIENTED_EDGE ( 'NONE', *, *, #53298, .T. ) ;
#105582 = CARTESIAN_POINT ( 'NONE',  ( 77.43793019189810423, -6.110000000000001208, 1.637169565754158951 ) ) ;
#105583 = VERTEX_POINT ( 'NONE', #128968 ) ;
#105584 = AXIS2_PLACEMENT_3D ( 'NONE', #130427, #10738, #64435 ) ;
#105585 = FILL_AREA_STYLE_COLOUR ( '', #86793 ) ;
#105586 = DIRECTION ( 'NONE',  ( -1.000000000000000000, -0.000000000000000000, -0.000000000000000000 ) ) ;
#105587 = CARTESIAN_POINT ( 'NONE',  ( -34.92500000000001137, 22.22500000000000142, 4.000000000000000000 ) ) ;
#105588 = ORIENTED_EDGE ( 'NONE', *, *, #27709, .T. ) ;
#105589 = CARTESIAN_POINT ( 'NONE',  ( -39.48921356237310221, -27.52281430457082934, 5.000000000000000000 ) ) ;
#105590 = LINE ( 'NONE', #59987, #97621 ) ;
#105591 = EDGE_CURVE ( 'NONE', #71076, #124824, #139157, .T. ) ;
#105592 = VERTEX_POINT ( 'NONE', #51431 ) ;
#105593 = VECTOR ( 'NONE', #32116, 1000.000000000000000 ) ;
#105594 = LINE ( 'NONE', #140389, #76792 ) ;
#105595 = CARTESIAN_POINT ( 'NONE',  ( 52.60764783923754351, -49.05583548141699168, -39.86617647058817937 ) ) ;
#105596 = FACE_OUTER_BOUND ( 'NONE', #75344, .T. ) ;
#105597 = VERTEX_POINT ( 'NONE', #20182 ) ;
#105598 = VERTEX_POINT ( 'NONE', #39858 ) ;
#105599 = VECTOR ( 'NONE', #123103, 1000.000000000000000 ) ;
#105600 = EDGE_CURVE ( 'NONE', #3235, #22619, #18027, .T. ) ;
#105601 = LINE ( 'NONE', #94728, #47795 ) ;
#105602 = CARTESIAN_POINT ( 'NONE',  ( -9.489213562373095101, -27.52281430457062328, 5.000000000000000000 ) ) ;
#105603 = CARTESIAN_POINT ( 'NONE',  ( 7.139999999999956160, -35.56014942880460694, -11.72188031596273206 ) ) ;
#105604 = FACE_OUTER_BOUND ( 'NONE', #78529, .T. ) ;
#105605 = VECTOR ( 'NONE', #13947, 1000.000000000000000 ) ;
#105606 = AXIS2_PLACEMENT_3D ( 'NONE', #112584, #21293, #13242 ) ;
#105607 = DIRECTION ( 'NONE',  ( -1.000000000000000000, 0.000000000000000000, 0.000000000000000000 ) ) ;
#105608 = PRESENTATION_STYLE_ASSIGNMENT (( #41092 ) ) ;
#105609 = ORIENTED_EDGE ( 'NONE', *, *, #97649, .F. ) ;
#105610 = MECHANICAL_DESIGN_GEOMETRIC_PRESENTATION_REPRESENTATION (  '', ( #135656 ), #80213 ) ;
#105611 = ORIENTED_EDGE ( 'NONE', *, *, #91690, .T. ) ;
#105612 = ORIENTED_EDGE ( 'NONE', *, *, #105833, .T. ) ;
#105613 = ORIENTED_EDGE ( 'NONE', *, *, #42467, .F. ) ;
#105614 = AXIS2_PLACEMENT_3D ( 'NONE', #97908, #98606, #33402 ) ;
#105615 = FILL_AREA_STYLE_COLOUR ( '', #40843 ) ;
#105616 = FILL_AREA_STYLE_COLOUR ( '', #72899 ) ;
#105617 = EDGE_CURVE ( 'NONE', #5654, #63020, #107212, .T. ) ;
#105618 = EDGE_LOOP ( 'NONE', ( #133409, #4996, #77322, #21370, #70718, #47572 ) ) ;
#105619 = CARTESIAN_POINT ( 'NONE',  ( 0.000000000000000000, 0.000000000000000000, 0.000000000000000000 ) ) ;
#105621 = EDGE_CURVE ( 'NONE', #92540, #22430, #64426, .T. ) ;
#105620 = CARTESIAN_POINT ( 'NONE',  ( 12.19999999999999574, -60.26999999999998892, 25.00000000000000000 ) ) ;
#105622 = DIRECTION ( 'NONE',  ( -0.000000000000000000, 0.3543493200069153248, 0.9351131265310292928 ) ) ;
#105623 = CARTESIAN_POINT ( 'NONE',  ( 33.29974487139158867, -27.71228299555229313, 4.000000000000000000 ) ) ;
#105624 = ORIENTED_EDGE ( 'NONE', *, *, #38437, .T. ) ;
#105625 = CARTESIAN_POINT ( 'NONE',  ( 4.499999999999968914, 5.696342897626504254, -7.587980461218388761 ) ) ;
#105626 = CARTESIAN_POINT ( 'NONE',  ( -57.48921356237308800, -27.52281430457095368, 5.000000000000000000 ) ) ;
#105627 = EDGE_LOOP ( 'NONE', ( #91594, #115232, #101213, #52003 ) ) ;
#105628 = CARTESIAN_POINT ( 'NONE',  ( 0.000000000000000000, -5.000000000000000000, -6.123233995736766282E-16 ) ) ;
#105629 = EDGE_LOOP ( 'NONE', ( #19408, #31069, #85342, #58742 ) ) ;
#105630 = ADVANCED_FACE ( 'NONE', ( #29639 ), #7885, .T. ) ;
#105631 = EDGE_CURVE ( 'NONE', #672, #5240, #26843, .T. ) ;
#105632 = CYLINDRICAL_SURFACE ( 'NONE', #133880, 0.5000000000000004441 ) ;
#105633 = ORIENTED_EDGE ( 'NONE', *, *, #28848, .F. ) ;
#105634 = EDGE_LOOP ( 'NONE', ( #2323, #127431, #93095, #74494 ) ) ;
#105635 = CARTESIAN_POINT ( 'NONE',  ( 68.97959685856477563, 6.109999999999999432, 1.637169565754164280 ) ) ;
#105636 = ORIENTED_EDGE ( 'NONE', *, *, #16970, .F. ) ;
#105637 =( BOUNDED_CURVE ( )  B_SPLINE_CURVE ( 3, ( #45409, #122941, #65751, #143258 ),
 .UNSPECIFIED., .F., .T. ) 
 B_SPLINE_CURVE_WITH_KNOTS ( ( 4, 4 ),
 ( 1.901594255663603183, 1.933014472006537199 ),
 .UNSPECIFIED. ) 
 CURVE ( )  GEOMETRIC_REPRESENTATION_ITEM ( )  RATIONAL_B_SPLINE_CURVE ( ( 1.000000000000000000, 0.9999177325257868620, 0.9999177325257868620, 1.000000000000000000 ) ) 
 REPRESENTATION_ITEM ( '' )  );
#105638 = EDGE_CURVE ( 'NONE', #29342, #43549, #97010, .T. ) ;
#105639 = ADVANCED_FACE ( 'NONE', ( #140550 ), #61611, .F. ) ;
#105640 = PLANE ( 'NONE',  #37353 ) ;
#105641 = CIRCLE ( 'NONE', #31685, 2.500000000000000000 ) ;
#105643 = EDGE_CURVE ( 'NONE', #119665, #137509, #105761, .T. ) ;
#105642 = LINE ( 'NONE', #140435, #72891 ) ;
#105644 = CARTESIAN_POINT ( 'NONE',  ( 106.6045968585647614, 1.637169565754164946, -6.109999999999999432 ) ) ;
#105645 = FACE_OUTER_BOUND ( 'NONE', #10570, .T. ) ;
#105646 = EDGE_CURVE ( 'NONE', #88426, #67057, #28953, .T. ) ;
#105647 = DIRECTION ( 'NONE',  ( 0.7071067811865487940, -0.7071067811865463515, 0.000000000000000000 ) ) ;
#105648 = CARTESIAN_POINT ( 'NONE',  ( -22.49999999999984368, -10.91253812416064228, 4.000000000000000000 ) ) ;
#105649 = VECTOR ( 'NONE', #109154, 1000.000000000000000 ) ;
#105650 = EDGE_CURVE ( 'NONE', #71933, #14462, #62307, .T. ) ;
#105651 = DIRECTION ( 'NONE',  ( 0.000000000000000000, -1.000000000000000000, 0.000000000000000000 ) ) ;
#105652 = FILL_AREA_STYLE ('',( #15760 ) ) ;
#105653 = CARTESIAN_POINT ( 'NONE',  ( 77.80836038379622721, 7.949999999999996625, 2.130196079827431088 ) ) ;
#105654 = EDGE_CURVE ( 'NONE', #93928, #46809, #74614, .T. ) ;
#105655 = ORIENTED_EDGE ( 'NONE', *, *, #140456, .F. ) ;
#105656 =( LENGTH_UNIT ( ) NAMED_UNIT ( * ) SI_UNIT ( .MILLI., .METRE. ) );
#105657 = ORIENTED_EDGE ( 'NONE', *, *, #89884, .T. ) ;
#105658 = ORIENTED_EDGE ( 'NONE', *, *, #133816, .F. ) ;
#105659 = CONICAL_SURFACE ( 'NONE', #124215, 2.055000000000001048, 0.9599310885968758145 ) ;
#105660 = DIRECTION ( 'NONE',  ( 0.7071067811865487940, 0.7071067811865463515, 0.000000000000000000 ) ) ;
#105661 = VERTEX_POINT ( 'NONE', #119492 ) ;
#105662 = CARTESIAN_POINT ( 'NONE',  ( 9.183988606268997046, 28.73617430169793607, 5.000000000000000000 ) ) ;
#105663 = FACE_OUTER_BOUND ( 'NONE', #8973, .T. ) ;
#105664 = EDGE_CURVE ( 'NONE', #47526, #20459, #50704, .T. ) ;
#105665 = DIRECTION ( 'NONE',  ( -0.7071067811865486830, -0.7071067811865464625, 0.000000000000000000 ) ) ;
#105666 = CARTESIAN_POINT ( 'NONE',  ( 34.92499999999998295, -5.993876922607981328, 4.000000000000000000 ) ) ;
#105667 = EDGE_LOOP ( 'NONE', ( #37212, #119106, #127383, #38089 ) ) ;
#105668 = EDGE_LOOP ( 'NONE', ( #124932, #64443, #75809, #87059 ) ) ;
#105669 = EDGE_CURVE ( 'NONE', #22078, #115783, #94893, .T. ) ;
#105670 = CIRCLE ( 'NONE', #124131, 2.500000000000000888 ) ;
#105671 = CARTESIAN_POINT ( 'NONE',  ( 0.7079031414352193741, -6.871911579029513106, -3.967499999999993587 ) ) ;
#105672 = CARTESIAN_POINT ( 'NONE',  ( 12.98155265364323085, 18.75929247661552424, 20.33588619593440328 ) ) ;
#105673 = DIRECTION ( 'NONE',  ( 0.7071067811865487940, 0.7071067811865463515, -0.000000000000000000 ) ) ;
#105674 = VECTOR ( 'NONE', #18587, 1000.000000000000114 ) ;
#105675 = CARTESIAN_POINT ( 'NONE',  ( -19.49999999999985434, 16.46639925780209168, 5.000000000000000000 ) ) ;
#105676 = VERTEX_POINT ( 'NONE', #115662 ) ;
#105677 = VERTEX_POINT ( 'NONE', #16356 ) ;
#105678 = ORIENTED_EDGE ( 'NONE', *, *, #138411, .T. ) ;
#105679 = CARTESIAN_POINT ( 'NONE',  ( 31.19018167574429157, -18.74070752338409207, 7.910009926591434315 ) ) ;
#105680 = LINE ( 'NONE', #48472, #62683 ) ;
#105681 = CARTESIAN_POINT ( 'NONE',  ( 159.7320121765528711, 26.96999999999993847, 34.92499999999998295 ) ) ;
#105682 = CARTESIAN_POINT ( 'NONE',  ( 48.18398860626899705, 28.73617430169820608, 5.000000000000000000 ) ) ;
#105683 = CARTESIAN_POINT ( 'NONE',  ( 36.48921356237310221, -27.52281430457080802, 5.000000000000000000 ) ) ;
#105684 = EDGE_CURVE ( 'NONE', #83015, #90172, #50461, .T. ) ;
#105685 = LINE ( 'NONE', #103553, #64793 ) ;
#105686 = AXIS2_PLACEMENT_3D ( 'NONE', #34510, #78739, #122954 ) ;
#105687 = PLANE ( 'NONE',  #88343 ) ;
#105688 = EDGE_CURVE ( 'NONE', #2187, #58967, #105523, .T. ) ;
#105689 = VERTEX_POINT ( 'NONE', #37445 ) ;
#105690 = LINE ( 'NONE', #117980, #62597 ) ;
#105691 = CARTESIAN_POINT ( 'NONE',  ( -34.92500000000001137, -10.65190338184902252, -7.458287694568772608 ) ) ;
#105692 = ORIENTED_EDGE ( 'NONE', *, *, #135087, .T. ) ;
#105693 = EDGE_CURVE ( 'NONE', #10862, #102959, #70801, .T. ) ;
#105694 = DIRECTION ( 'NONE',  ( 0.000000000000000000, 0.000000000000000000, -1.000000000000000000 ) ) ;
#105696 = ORIENTED_EDGE ( 'NONE', *, *, #98791, .F. ) ;
#105695 = LINE ( 'NONE', #73126, #99700 ) ;
#105697 = VECTOR ( 'NONE', #141654, 999.9999999999998863 ) ;
#105698 = CARTESIAN_POINT ( 'NONE',  ( -33.48921356237309510, -27.52281430457078670, 5.000000000000000000 ) ) ;
#105699 = LINE ( 'NONE', #17967, #129517 ) ;
#105700 = ORIENTED_EDGE ( 'NONE', *, *, #20735, .F. ) ;
#105701 = CARTESIAN_POINT ( 'NONE',  ( -22.49999999999982947, 13.08746187583911080, 4.000000000000000000 ) ) ;
#105702 = EDGE_LOOP ( 'NONE', ( #11748, #81326, #77991, #124581 ) ) ;
#105703 = CIRCLE ( 'NONE', #6139, 2.500000000000000444 ) ;
#105704 = VECTOR ( 'NONE', #10225, 1000.000000000000227 ) ;
#105705 = CARTESIAN_POINT ( 'NONE',  ( 5.848407645496676466, 9.139736423841732040E-16, 0.000000000000000000 ) ) ;
#105707 = CARTESIAN_POINT ( 'NONE',  ( 121.2666937171295700, -7.949999999999999289, 2.130196079827424427 ) ) ;
#105706 = AXIS2_PLACEMENT_3D ( 'NONE', #77100, #78502, #32134 ) ;
#105708 = DIRECTION ( 'NONE',  ( -1.000000000000000000, -1.224606353822377258E-16, -0.000000000000000000 ) ) ;
#105709 = LINE ( 'NONE', #96254, #131635 ) ;
#105710 = EDGE_CURVE ( 'NONE', #106925, #71937, #48304, .T. ) ;
#105711 = LINE ( 'NONE', #93445, #14389 ) ;
#105712 = CARTESIAN_POINT ( 'NONE',  ( 11.29289321881338282, -6.740707523384211086, 5.000000000000000000 ) ) ;
#105713 = DIRECTION ( 'NONE',  ( -0.7071067811865486830, 0.7071067811865464625, 0.000000000000000000 ) ) ;
#105714 = CARTESIAN_POINT ( 'NONE',  ( 26.22873647476855652, 5.808823158059031044, -5.808823158059038150 ) ) ;
#105715 = CARTESIAN_POINT ( 'NONE',  ( 6.395403141435219929, 2.126176841940962348, 7.934999999999988951 ) ) ;
#105716 = CARTESIAN_POINT ( 'NONE',  ( 26.29289321881326913, 2.259292476615694323, 5.000000000000000000 ) ) ;
#105717 = AXIS2_PLACEMENT_3D ( 'NONE', #77441, #54263, #98443 ) ;
#105718 = DIRECTION ( 'NONE',  ( -0.7071067811865487940, 0.7071067811865463515, -0.000000000000000000 ) ) ;
#105719 = DIRECTION ( 'NONE',  ( 0.6830127018922180770, -0.6830127018922204085, -0.2588190451025213501 ) ) ;
#105720 = ORIENTED_EDGE ( 'NONE', *, *, #42734, .T. ) ;
#105721 = ORIENTED_EDGE ( 'NONE', *, *, #73695, .T. ) ;
#105722 = CARTESIAN_POINT ( 'NONE',  ( 78.43750000000000000, 5.819803920172573974, -5.819803920172572198 ) ) ;
#105723 = CARTESIAN_POINT ( 'NONE',  ( -31.92499999999997584, -6.270000000000012896, -40.00000000000000000 ) ) ;
#105724 = EDGE_LOOP ( 'NONE', ( #101883, #44109, #115995, #51197 ) ) ;
#105725 = ADVANCED_FACE ( 'NONE', ( #28718 ), #103374, .T. ) ;
#105726 = CARTESIAN_POINT ( 'NONE',  ( -7.140000000000001457, -35.14999999999999147, -8.278119684037250181 ) ) ;
#105727 = DIRECTION ( 'NONE',  ( 0.7071067811865486830, -0.7071067811865464625, -0.000000000000000000 ) ) ;
#105728 = PLANE ( 'NONE',  #10812 ) ;
#105729 = ORIENTED_EDGE ( 'NONE', *, *, #31283, .T. ) ;
#105730 = DIRECTION ( 'NONE',  ( 0.7071067811865487940, 0.7071067811865463515, 0.000000000000000000 ) ) ;
#105731 = CARTESIAN_POINT ( 'NONE',  ( 24.39999999999999858, -2.600000000000012079, -20.40202195861969159 ) ) ;
#105732 = LINE ( 'NONE', #84726, #136653 ) ;
#105733 = CARTESIAN_POINT ( 'NONE',  ( -34.92500000000001137, 6.006123077391876564, 4.000000000000000000 ) ) ;
#105734 = ADVANCED_FACE ( 'NONE', ( #117117 ), #59914, .F. ) ;
#105735 = FACE_OUTER_BOUND ( 'NONE', #85212, .T. ) ;
#105736 = CARTESIAN_POINT ( 'NONE',  ( -21.29974487139158512, -27.71228299555221142, 4.000000000000000000 ) ) ;
#105737 = VECTOR ( 'NONE', #90341, 1000.000000000000000 ) ;
#105738 = LINE ( 'NONE', #104316, #42949 ) ;
#105739 = PLANE ( 'NONE',  #74773 ) ;
#105740 = DIRECTION ( 'NONE',  ( -0.3543493200069162685, -0.000000000000000000, -0.9351131265310288487 ) ) ;
#105741 = CARTESIAN_POINT ( 'NONE',  ( 0.000000000000000000, 21.72500000000000142, 0.000000000000000000 ) ) ;
#105742 = DIRECTION ( 'NONE',  ( -0.6830127018922180770, -0.6830127018922204085, -0.2588190451025213501 ) ) ;
#105743 = EDGE_CURVE ( 'NONE', #47934, #3210, #125147, .T. ) ;
#105744 = ORIENTED_EDGE ( 'NONE', *, *, #142856, .F. ) ;
#105745 = EDGE_LOOP ( 'NONE', ( #47821, #5742, #81312, #40842, #95243, #78691 ) ) ;
#105746 = CARTESIAN_POINT ( 'NONE',  ( 103.1045968585647756, 1.637169565754164946, -6.109999999999999432 ) ) ;
#105747 = VECTOR ( 'NONE', #70003, 999.9999999999998863 ) ;
#105748 = ORIENTED_EDGE ( 'NONE', *, *, #41116, .T. ) ;
#105749 = PLANE ( 'NONE',  #27026 ) ;
#105750 = CIRCLE ( 'NONE', #91800, 1.000000000000000888 ) ;
#105751 = DIRECTION ( 'NONE',  ( -0.000000000000000000, -0.3543493200069152693, 0.9351131265310292928 ) ) ;
#105752 = ORIENTED_EDGE ( 'NONE', *, *, #115461, .F. ) ;
#105753 = CARTESIAN_POINT ( 'NONE',  ( -12.20000000000000284, -40.42999999999999261, -40.00000000000000000 ) ) ;
#105755 = ADVANCED_FACE ( 'NONE', ( #92503 ), #104083, .F. ) ;
#105754 = DIRECTION ( 'NONE',  ( -0.7071067811865486830, 0.7071067811865464625, 0.000000000000000000 ) ) ;
#105756 = CARTESIAN_POINT ( 'NONE',  ( 91.34959685856478018, 6.109999999999996767, 1.637169565754163836 ) ) ;
#105757 = ADVANCED_FACE ( 'NONE', ( #136729 ), #70112, .F. ) ;
#105758 = VERTEX_POINT ( 'NONE', #93946 ) ;
#105759 = DIRECTION ( 'NONE',  ( 0.6830127018922180770, -0.6830127018922204085, -0.2588190451025213501 ) ) ;
#105760 = EDGE_LOOP ( 'NONE', ( #142064, #71494, #93136, #22814 ) ) ;
#105761 = LINE ( 'NONE', #95623, #19897 ) ;
#105762 = AXIS2_PLACEMENT_3D ( 'NONE', #119629, #87750, #129100 ) ;
#105763 = LINE ( 'NONE', #50705, #74646 ) ;
#105764 = PLANE ( 'NONE',  #82471 ) ;
#105765 = DIRECTION ( 'NONE',  ( 0.7071067811865487940, 0.7071067811865463515, 0.000000000000000000 ) ) ;
#105766 = EDGE_LOOP ( 'NONE', ( #19316, #138494, #74145, #82418 ) ) ;
#105767 = ORIENTED_EDGE ( 'NONE', *, *, #89668, .F. ) ;
#105768 = VECTOR ( 'NONE', #16854, 1000.000000000000000 ) ;
#105769 = VERTEX_POINT ( 'NONE', #38864 ) ;
#105770 = CARTESIAN_POINT ( 'NONE',  ( -18.83829387547368484, -6.740707523384205757, 16.75550250614862691 ) ) ;
#105771 = ADVANCED_FACE ( 'NONE', ( #4737 ), #104824, .F. ) ;
#105772 = DIRECTION ( 'NONE',  ( 0.6830127018922181881, 0.6830127018922202975, -0.2588190451025214056 ) ) ;
#105773 = CARTESIAN_POINT ( 'NONE',  ( 12.60873647476855197, -5.808823158059033709, 5.808823158059035485 ) ) ;
#105774 = DIRECTION ( 'NONE',  ( -0.7071067811865487940, 0.7071067811865463515, -0.000000000000000000 ) ) ;
#105775 = VECTOR ( 'NONE', #34348, 999.9999999999998863 ) ;
#105776 = ORIENTED_EDGE ( 'NONE', *, *, #111786, .T. ) ;
#105777 = VECTOR ( 'NONE', #135942, 1000.000000000000000 ) ;
#105778 = ORIENTED_EDGE ( 'NONE', *, *, #49147, .F. ) ;
#105779 = DIRECTION ( 'NONE',  ( 0.3543493200069163240, 0.000000000000000000, -0.9351131265310288487 ) ) ;
#105780 = ORIENTED_EDGE ( 'NONE', *, *, #91930, .F. ) ;
#105781 = ORIENTED_EDGE ( 'NONE', *, *, #130879, .T. ) ;
#105782 = CARTESIAN_POINT ( 'NONE',  ( 115.4120968585647944, 5.291415217122921177, -3.054999999999994831 ) ) ;
#105783 = DIRECTION ( 'NONE',  ( -0.000000000000000000, -0.3543493200069152693, 0.9351131265310292928 ) ) ;
#105784 = DIRECTION ( 'NONE',  ( -0.7071067811865486830, -0.7071067811865464625, -0.000000000000000000 ) ) ;
#105785 = ORIENTED_EDGE ( 'NONE', *, *, #75065, .F. ) ;
#105786 = CARTESIAN_POINT ( 'NONE',  ( 6.270833333333333925, 6.094999999999991758, 1.633150327867686880 ) ) ;
#105787 = ADVANCED_FACE ( 'NONE', ( #116424 ), #17111, .F. ) ;
#105788 = DIRECTION ( 'NONE',  ( -0.7071067811865486830, -0.7071067811865464625, -0.000000000000000000 ) ) ;
#105789 = CARTESIAN_POINT ( 'NONE',  ( -54.18398860626899705, 28.73617430169825226, 5.000000000000000000 ) ) ;
#105790 = LINE ( 'NONE', #84110, #4888 ) ;
#105791 = ORIENTED_EDGE ( 'NONE', *, *, #31961, .T. ) ;
#105792 = CARTESIAN_POINT ( 'NONE',  ( -12.29974487139158512, -27.71228299555214747, 4.000000000000000000 ) ) ;
#105794 = CARTESIAN_POINT ( 'NONE',  ( 36.87499999999999289, 7.950000000000000178, 1.460391307983218535E-15 ) ) ;
#105793 = VECTOR ( 'NONE', #37543, 999.9999999999998863 ) ;
#105795 = VERTEX_POINT ( 'NONE', #6185 ) ;
#105796 = DIRECTION ( 'NONE',  ( -0.000000000000000000, 0.3543493200069153248, 0.9351131265310292928 ) ) ;
#105797 = FACE_OUTER_BOUND ( 'NONE', #24153, .T. ) ;
#105799 = EDGE_LOOP ( 'NONE', ( #5097, #115586, #11909, #61285 ) ) ;
#105798 = EDGE_CURVE ( 'NONE', #126032, #142844, #81683, .T. ) ;
#105800 = LINE ( 'NONE', #50746, #50578 ) ;
#105801 = ORIENTED_EDGE ( 'NONE', *, *, #116396, .T. ) ;
#105802 = VERTEX_POINT ( 'NONE', #93236 ) ;
#105803 = VECTOR ( 'NONE', #109186, 1000.000000000000000 ) ;
#105804 = ORIENTED_EDGE ( 'NONE', *, *, #16345, .F. ) ;
#105805 = VECTOR ( 'NONE', #44897, 1000.000000000000000 ) ;
#105807 = EDGE_CURVE ( 'NONE', #48148, #121857, #33806, .T. ) ;
#105806 = CIRCLE ( 'NONE', #43347, 0.9999999999999997780 ) ;
#105808 = DIRECTION ( 'NONE',  ( -1.000000000000000000, -1.224606353822377258E-16, -0.000000000000000000 ) ) ;
#105809 = CARTESIAN_POINT ( 'NONE',  ( -8.999999999999937828, 17.96639925780208102, 5.000000000000000000 ) ) ;
#105811 = ADVANCED_FACE ( 'NONE', ( #26558 ), #106223, .F. ) ;
#105810 = CARTESIAN_POINT ( 'NONE',  ( 7.139999999999985469, -39.92999999999999972, -39.50000000000000000 ) ) ;
#105812 = DIRECTION ( 'NONE',  ( -0.7071067811865487940, 0.7071067811865463515, -0.000000000000000000 ) ) ;
#105813 = CARTESIAN_POINT ( 'NONE',  ( 0.005480084712502889671, 28.92564299267938210, 4.000000000000000000 ) ) ;
#105814 = EDGE_CURVE ( 'NONE', #18168, #93700, #63592, .T. ) ;
#105815 = PLANE ( 'NONE',  #6479 ) ;
#105816 = DIRECTION ( 'NONE',  ( 1.000000000000000000, 0.000000000000000000, 0.000000000000000000 ) ) ;
#105817 = VECTOR ( 'NONE', #52289, 1000.000000000000114 ) ;
#105818 = EDGE_CURVE ( 'NONE', #106471, #37562, #33115, .T. ) ;
#105819 = LINE ( 'NONE', #86254, #116285 ) ;
#105820 = DIRECTION ( 'NONE',  ( 0.6830127018922180770, -0.6830127018922204085, -0.2588190451025213501 ) ) ;
#105821 = LINE ( 'NONE', #117410, #133985 ) ;
#105822 = DIRECTION ( 'NONE',  ( -0.7071067811865486830, -0.7071067811865464625, 0.000000000000000000 ) ) ;
#105823 = ADVANCED_FACE ( 'NONE', ( #121488 ), #130259, .F. ) ;
#105824 = ORIENTED_EDGE ( 'NONE', *, *, #78055, .T. ) ;
#105825 = ORIENTED_EDGE ( 'NONE', *, *, #116835, .F. ) ;
#105826 = ORIENTED_EDGE ( 'NONE', *, *, #60228, .F. ) ;
#105827 = VERTEX_POINT ( 'NONE', #96154 ) ;
#105828 = CARTESIAN_POINT ( 'NONE',  ( 8.423184310185783730, 4.584330080086930965E-16, 0.000000000000000000 ) ) ;
#105829 = EDGE_LOOP ( 'NONE', ( #26640, #83729, #97603, #53494 ) ) ;
#105830 = ORIENTED_EDGE ( 'NONE', *, *, #40251, .T. ) ;
#105831 = LINE ( 'NONE', #86271, #12070 ) ;
#105832 = DIRECTION ( 'NONE',  ( -0.7071067811865487940, 0.7071067811865463515, -0.000000000000000000 ) ) ;
#105833 = EDGE_CURVE ( 'NONE', #5100, #56149, #65006, .T. ) ;
#105834 = EDGE_CURVE ( 'NONE', #87449, #12661, #41806, .T. ) ;
#105835 = CARTESIAN_POINT ( 'NONE',  ( -24.70701326429287903, -21.74070752338406365, 4.999753212805221558 ) ) ;
#105836 = ORIENTED_EDGE ( 'NONE', *, *, #55482, .T. ) ;
#105837 = AXIS2_PLACEMENT_3D ( 'NONE', #55972, #121181, #66821 ) ;
#105838 = CARTESIAN_POINT ( 'NONE',  ( -10.78678096696635436, 12.75929247661558996, 10.29404684609032827 ) ) ;
#105839 = ORIENTED_EDGE ( 'NONE', *, *, #80588, .T. ) ;
#105840 = ADVANCED_FACE ( 'NONE', ( #41084 ), #10571, .F. ) ;
#105841 = DIRECTION ( 'NONE',  ( 0.7071067811865486830, -0.7071067811865464625, -0.000000000000000000 ) ) ;
#105842 = DIRECTION ( 'NONE',  ( -0.7071067811865486830, 0.7071067811865464625, 0.000000000000000000 ) ) ;
#105843 = MECHANICAL_DESIGN_GEOMETRIC_PRESENTATION_REPRESENTATION (  '', ( #66572 ), #41094 ) ;
#105844 = CARTESIAN_POINT ( 'NONE',  ( 11.29623647476855375, 7.934999999999990727, -1.457635852685135314E-15 ) ) ;
#105845 = ORIENTED_EDGE ( 'NONE', *, *, #136588, .F. ) ;
#105846 = CARTESIAN_POINT ( 'NONE',  ( 106.0787635252314516, -7.482591942790327058E-16, 6.109999999999999432 ) ) ;
#105847 = DIRECTION ( 'NONE',  ( 0.000000000000000000, -1.000000000000000000, 0.000000000000000000 ) ) ;
#105848 = DIRECTION ( 'NONE',  ( 0.000000000000000000, 0.000000000000000000, -1.000000000000000000 ) ) ;
#105849 = ORIENTED_EDGE ( 'NONE', *, *, #30753, .T. ) ;
#105850 = ORIENTED_EDGE ( 'NONE', *, *, #77287, .F. ) ;
#105851 = PLANE ( 'NONE',  #991 ) ;
#105852 = ORIENTED_EDGE ( 'NONE', *, *, #97999, .T. ) ;
#105853 = AXIS2_PLACEMENT_3D ( 'NONE', #102049, #47015, #113623 ) ;
#105854 = DIRECTION ( 'NONE',  ( -0.7071067811865487940, 0.7071067811865463515, -0.000000000000000000 ) ) ;
#105855 = DIRECTION ( 'NONE',  ( 0.7071067811865486830, -0.7071067811865464625, -0.000000000000000000 ) ) ;
#105856 = DIRECTION ( 'NONE',  ( 1.000000000000000000, 0.000000000000000000, 0.000000000000000000 ) ) ;
#105857 = CARTESIAN_POINT ( 'NONE',  ( 183.5369301914234086, -49.19053253528003466, -40.77637019028070853 ) ) ;
#105859 = ORIENTED_EDGE ( 'NONE', *, *, #43851, .F. ) ;
#105858 =( BOUNDED_CURVE ( )  B_SPLINE_CURVE ( 3, ( #86780, #140425, #111922, #96882 ),
 .UNSPECIFIED., .F., .F. ) 
 B_SPLINE_CURVE_WITH_KNOTS ( ( 4, 4 ),
 ( 3.996889577052295195, 4.025035655492697373 ),
 .UNSPECIFIED. ) 
 CURVE ( )  GEOMETRIC_REPRESENTATION_ITEM ( )  RATIONAL_B_SPLINE_CURVE ( ( 1.000000000000000000, 0.9999339842785831545, 0.9999339842785831545, 1.000000000000000000 ) ) 
 REPRESENTATION_ITEM ( '' )  );
#105860 = CARTESIAN_POINT ( 'NONE',  ( 1.516262732464673579, 0.3999999999999995226, 2.467792535850613866 ) ) ;
#105861 = DIRECTION ( 'NONE',  ( 0.7071067811865486830, -0.7071067811865464625, -0.000000000000000000 ) ) ;
#105862 = CARTESIAN_POINT ( 'NONE',  ( -17.70025512860841488, -27.71228299555193786, 4.000000000000000000 ) ) ;
#105863 = ADVANCED_FACE ( 'NONE', ( #43246 ), #62866, .F. ) ;
#105864 = MECHANICAL_DESIGN_GEOMETRIC_PRESENTATION_REPRESENTATION (  '', ( #20183 ), #43400 ) ;
#105865 = EDGE_LOOP ( 'NONE', ( #24675, #36729, #97988, #2116 ) ) ;
#105866 = CARTESIAN_POINT ( 'NONE',  ( 24.18398860626899705, 28.73617430169804265, 5.000000000000000000 ) ) ;
#105867 = LINE ( 'NONE', #40654, #9862 ) ;
#105868 = ORIENTED_EDGE ( 'NONE', *, *, #50463, .T. ) ;
#105870 = ORIENTED_EDGE ( 'NONE', *, *, #84406, .F. ) ;
#105869 = CARTESIAN_POINT ( 'NONE',  ( 0.3872656504351221218, -51.96230815476842224, -39.57541490114649463 ) ) ;
#105871 = VERTEX_POINT ( 'NONE', #99015 ) ;
#105872 = CARTESIAN_POINT ( 'NONE',  ( 34.92499999999998295, -12.18334561358941137, 4.500000000000000888 ) ) ;
#105873 = DIRECTION ( 'NONE',  ( -0.6830127018922180770, -0.6830127018922204085, -0.2588190451025213501 ) ) ;
#105874 = ORIENTED_EDGE ( 'NONE', *, *, #134827, .T. ) ;
#105875 = FACE_OUTER_BOUND ( 'NONE', #41947, .T. ) ;
#105876 = UNCERTAINTY_MEASURE_WITH_UNIT (LENGTH_MEASURE( 1.000000000000000082E-05 ), #104927, 'distance_accuracy_value', 'NONE');
#105877 = CARTESIAN_POINT ( 'NONE',  ( 54.48921356237310221, -27.52281430457093236, 5.000000000000000000 ) ) ;
#105878 = CARTESIAN_POINT ( 'NONE',  ( -21.29974487139158512, -27.71228299555221142, 4.000000000000000000 ) ) ;
#105879 = VECTOR ( 'NONE', #61132, 1000.000000000000000 ) ;
#105880 = CARTESIAN_POINT ( 'NONE',  ( -39.18398860626899705, 28.73617430169814568, 5.000000000000000000 ) ) ;
#105881 = CARTESIAN_POINT ( 'NONE',  ( -31.82816939922330945, 21.75929247661549937, 4.000000000000000000 ) ) ;
#105882 = ADVANCED_FACE ( 'NONE', ( #52667, #64271, #30203, #30947, #96852, #141095, #74451, #109908, #119336, #53386, #7724, #19335, #107750, #8409, #142558, #86750, #97592, #9876, #130971, #42547, #31647, #75868, #54837, #109191, #131676, #32360, #76603, #54146, #120031, #98336, #120775, #143253, #43952, #88173, #67883, #66425, #34496, #124358, #135941, #33800, #13420, #80168, #35951, #91044, #123674, #68575, #1126, #25027, #22864, #57702, #3272, #45404, #56296, #47563, #91720, #69279, #2549, #101165, #46856, #78014, #135266, #55549, #122192, #78719, #410, #36623, #56992, #133810, #122934, #80872, #101887, #24328, #22164, #23612, #112068, #67131, #112762, #113463, #14154, #134542, #12724, #1808, #110595, #111324, #90290, #58445, #102625, #89579, #11274, #99741, #44711, #88902, #133122, #12007, #100478, #46110, #35238, #79483, #138093, #95289, #103298, #3946, #17028, #60566, #117039, #106134, #127198, #126479, #6097, #17706, #93156, #114188, #38780, #48221, #72886, #139552, #127945, #82300, #104740, #61297, #61979, #5403, #27896, #105439, #15547, #136649, #92416, #40233, #6810, #50375, #125064, #94564, #49683, #27172, #25751, #72162, #93861, #70020, #14872, #37357, #83005, #138819, #51095, #81593, #116334, #39514, #59146, #83744, #28635, #125800, #26474, #70724, #114870, #59830, #71417, #103994, #115571, #4655, #48956, #16267, #137387, #38079, #130077, #75004, #73556, #97413, #131503, #107590, #84448, #118464, #10407, #9699, #8248, #74272, #87284, #21310, #128642, #109005, #142389, #98160, #53965, #62688, #7551, #63423, #51813, #30776, #96683, #65568, #42369, #85840, #19163, #43079, #30023, #19863, #8941, #32185, #52496, #95995, #117724, #140239, #140928, #76419, #29315, #106870, #86581, #120587, #64099, #119178, #108269, #41622, #75698, #109737, #53205, #31477, #141669, #64825, #119867, #130810, #20572, #98850, #40925, #54666, #129340, #143084, #18410, #85128, #56837, #22689, #13969, #110428, #57529, #11102, #58274, #77835, #101717, #132239, #100304, #66253, #87989, #133647, #55379, #956, #22003, #89415, #34324, #32931, #100996, #90870, #66962, #43776, #122021, #90121, #111139, #80009, #99553, #78553, #122752, #77151, #1652, #135102, #11831, #121321, #56113, #134366, #45935, #23436, #67708, #225, #45238, #2367, #102460, #44527, #35068, #88727, #132957, #111893, #33637, #24867, #12556, #79308, #123509, #24162, #69110, #68418, #112600, #113292, #13257, #46688, #35788, #124186, #27719, #58987, #71976, #135780, #5234, #103143, #93704, #82144, #126322, #49520, #127023, #28459, #38610, #104572, #72719, #103823, #15383, #48066, #137929, #82841, #5933, #115403, #137217, #61131, #70566, #60386, #50208, #116162, #16858, #127770, #3783, #81432, #36468, #94397, #136479, #4475, #91563, #116872, #17545, #92249, #105280, #27007, #114711, #138645, #71253, #3109, #59668, #48781, #39339, #92988, #37174, #83558, #16094, #47397, #37914, #61808, #124899, #80702, #25572, #69847, #114021, #14710, #26309, #125632, #140079, #8767, #84960, #142222, #108104, #139384, #32003, #64638, #76236, #117556, #97223, #120398, #51637, #129166, #6634, #87106, #84285, #141488, #41444, #97983, #131321, #53027, #107421, #130637, #42908, #74092, #95110, #85656, #31305, #18236, #75521, #40067, #42194, #62517, #86408, #129892, #30603, #119690, #20391, #40756, #106684, #73392, #21122, #105968, #108819, #50919, #9505, #53786, #128479, #74832, #96511, #29151, #29850, #19693, #7378, #95830, #118282, #18990, #63255, #119011, #8081, #52324, #140750, #63933, #134926, #78376, #112426, #35616, #43592, #132052, #44339, #32741, #110961, #77671, #46506, #23244, #66784, #99372, #34884, #10930, #778, #133472, #79121, #39, #76976, #98678, #121143, #1483, #13082, #65385, #87809, #67521, #89937, #45072, #11644, #55924, #88552, #56666, #134187, #132784, #12382, #34159, #45771, #100829, #122568, #100129, #79844, #21841, #111714, #110252, #121841, #123327, #66084, #23990, #33470, #124020, #55198, #68251, #22523, #109563, #89246, #57356, #10238, #101532, #2186, #54498, #90692, #142908, #114550, #102284, #14538, #93528, #102980, #26833, #48596, #38439, #137762, #124723, #92078, #68946, #71083, #94227, #82661, #136306, #58817, #27532, #105109, #39152, #126844, #115227, #37738, #13789, #71796, #3616, #125450, #113119, #138467, #83374, #69664, #104383, #92799, #36992, #15912, #137031, #24689, #81246, #26134, #115964, #60203, #16667, #5044, #60953, #126162, #4295, #58084, #70400, #49345, #81973, #15217, #59496, #2935, #103651, #5770, #47229, #36298, #50035, #91403, #135611, #80527, #25392, #113842, #47912, #50740, #29675, #139910, #110617, #85480, #128998, #18058, #99036, #73220, #63071, #52158, #143271, #62347, #94930, #17384 ), #73915, .F. ) ;
#105883 = FACE_OUTER_BOUND ( 'NONE', #139259, .T. ) ;
#105884 = LINE ( 'NONE', #141394, #114196 ) ;
#105885 = CARTESIAN_POINT ( 'NONE',  ( 7.940000000000001279, -60.26999999999998892, -8.101350000000007157 ) ) ;
#105886 = DIRECTION ( 'NONE',  ( -0.3543493200069162685, -0.000000000000000000, -0.9351131265310288487 ) ) ;
#105887 = CARTESIAN_POINT ( 'NONE',  ( -29.99999999999979039, -16.06887692260765377, 4.000000000000000000 ) ) ;
#105888 = DIRECTION ( 'NONE',  ( -0.7071067811865487940, 0.7071067811865463515, 0.000000000000000000 ) ) ;
#105889 = VERTEX_POINT ( 'NONE', #107244 ) ;
#105890 = ORIENTED_EDGE ( 'NONE', *, *, #63957, .F. ) ;
#105891 = ORIENTED_EDGE ( 'NONE', *, *, #94539, .F. ) ;
#105892 = CARTESIAN_POINT ( 'NONE',  ( 113.8750000000000000, 7.950000000000000178, 1.460391307983218535E-15 ) ) ;
#105893 = AXIS2_PLACEMENT_3D ( 'NONE', #108940, #53142, #121263 ) ;
#105894 = ORIENTED_EDGE ( 'NONE', *, *, #35327, .T. ) ;
#105895 = EDGE_LOOP ( 'NONE', ( #126770, #10028, #87486, #126584 ) ) ;
#105896 = ADVANCED_FACE ( 'NONE', ( #74650 ), #117385, .F. ) ;
#105897 = ORIENTED_EDGE ( 'NONE', *, *, #32210, .T. ) ;
#105898 = CARTESIAN_POINT ( 'NONE',  ( 156.1499999999997783, -49.14999999999999147, -34.92499999999975557 ) ) ;
#105899 = FACE_OUTER_BOUND ( 'NONE', #76363, .T. ) ;
#105900 = ORIENTED_EDGE ( 'NONE', *, *, #45285, .T. ) ;
#105901 = VECTOR ( 'NONE', #47090, 1000.000000000000000 ) ;
#105902 = CARTESIAN_POINT ( 'NONE',  ( 63.48921356237309510, -27.52281430457099631, 5.000000000000000000 ) ) ;
#105903 = PLANE ( 'NONE',  #2462 ) ;
#105904 = VECTOR ( 'NONE', #72889, 1000.000000000000000 ) ;
#105905 = DIRECTION ( 'NONE',  ( -1.000000000000000000, -1.224606353822377258E-16, -0.000000000000000000 ) ) ;
#105906 = DIRECTION ( 'NONE',  ( -1.000000000000000000, -1.224606353822377258E-16, -0.000000000000000000 ) ) ;
#105907 = CARTESIAN_POINT ( 'NONE',  ( 107.1879301918980900, 6.110000000000002984, -1.637169565754156730 ) ) ;
#105908 = EDGE_CURVE ( 'NONE', #86644, #12213, #7188, .T. ) ;
#105909 = ORIENTED_EDGE ( 'NONE', *, *, #87695, .F. ) ;
#105910 = CARTESIAN_POINT ( 'NONE',  ( -6.391038532768485325, 11.40365449930913222, -27.77063147129241116 ) ) ;
#105911 = CARTESIAN_POINT ( 'NONE',  ( -6.728648308968876890, -34.60547875340945723, 17.99210858042622263 ) ) ;
#105912 = LINE ( 'NONE', #6578, #114498 ) ;
#105913 = CARTESIAN_POINT ( 'NONE',  ( -29.99451991528749417, 28.92564299267958816, 4.000000000000000000 ) ) ;
#105914 = LINE ( 'NONE', #10012, #40542 ) ;
#105915 = AXIS2_PLACEMENT_3D ( 'NONE', #12212, #136143, #33992 ) ;
#105916 = LINE ( 'NONE', #95054, #130229 ) ;
#105917 = LINE ( 'NONE', #5168, #82474 ) ;
#105918 = AXIS2_PLACEMENT_3D ( 'NONE', #51643, #31311, #86414 ) ;
#105919 = CARTESIAN_POINT ( 'NONE',  ( 41.49586038379622721, -3.974999999999998312, -6.884901960086286188 ) ) ;
#105920 = DIRECTION ( 'NONE',  ( 0.6830127018922181881, 0.6830127018922202975, -0.2588190451025214056 ) ) ;
#105921 = VECTOR ( 'NONE', #126633, 1000.000000000000000 ) ;
#105922 = PRESENTATION_STYLE_ASSIGNMENT (( #44093 ) ) ;
#105923 = ORIENTED_EDGE ( 'NONE', *, *, #54166, .F. ) ;
#105924 = ORIENTED_EDGE ( 'NONE', *, *, #77324, .F. ) ;
#105925 = CARTESIAN_POINT ( 'NONE',  ( 126.4379301918981042, -6.110000000000001208, 1.637169565754158951 ) ) ;
#105926 = ORIENTED_EDGE ( 'NONE', *, *, #111117, .T. ) ;
#105927 = DIRECTION ( 'NONE',  ( 1.000000000000000000, 0.000000000000000000, 0.000000000000000000 ) ) ;
#105928 = CARTESIAN_POINT ( 'NONE',  ( 36.29974487139159578, -27.71228299555231445, 4.000000000000000000 ) ) ;
#105929 = AXIS2_PLACEMENT_3D ( 'NONE', #112052, #135248, #78700 ) ;
#105930 = LINE ( 'NONE', #6593, #110469 ) ;
#105931 = CARTESIAN_POINT ( 'NONE',  ( -26.99999999999980815, 1.761378380278660227, -6.096875308897316437 ) ) ;
#105932 = DIRECTION ( 'NONE',  ( 0.7071067811865487940, -0.7071067811865463515, 0.000000000000000000 ) ) ;
#105933 = CARTESIAN_POINT ( 'NONE',  ( 33.79289321881321229, -2.240707523384267930, 5.000000000000000000 ) ) ;
#105934 = CARTESIAN_POINT ( 'NONE',  ( 27.12543019189810067, 5.291415217122919401, 3.055000000000002824 ) ) ;
#105935 = EDGE_CURVE ( 'NONE', #17123, #60821, #88137, .T. ) ;
#105936 = ORIENTED_EDGE ( 'NONE', *, *, #89496, .F. ) ;
#105937 = CARTESIAN_POINT ( 'NONE',  ( 0.1839886062690032631, 28.73617430169787568, 5.000000000000000000 ) ) ;
#105938 = EDGE_LOOP ( 'NONE', ( #61650, #8651, #130124, #69006 ) ) ;
#105939 = FACE_OUTER_BOUND ( 'NONE', #5797, .T. ) ;
#105940 = CARTESIAN_POINT ( 'NONE',  ( -1.499999999999990896, -20.56887692260760048, 4.000000000000000000 ) ) ;
#105941 = CARTESIAN_POINT ( 'NONE',  ( -33.41161490594808470, 22.22500000000000497, 4.777194822843813249 ) ) ;
#105942 = CARTESIAN_POINT ( 'NONE',  ( -12.69999999999998153, 0.000000000000000000, 0.000000000000000000 ) ) ;
#105944 = ADVANCED_FACE ( 'NONE', ( #11294 ), #33136, .F. ) ;
#105943 = VERTEX_POINT ( 'NONE', #6459 ) ;
#105945 = CARTESIAN_POINT ( 'NONE',  ( 55.85459685856475431, -1.637169565754161615, 6.110000000000000320 ) ) ;
#105946 = ORIENTED_EDGE ( 'NONE', *, *, #62356, .T. ) ;
#105947 = DIRECTION ( 'NONE',  ( -0.7071067811865486830, 0.7071067811865464625, 0.000000000000000000 ) ) ;
#105948 = EDGE_CURVE ( 'NONE', #134670, #69673, #92767, .T. ) ;
#105949 = CARTESIAN_POINT ( 'NONE',  ( 31.49999999999977973, -10.53360074219763121, 5.000000000000000000 ) ) ;
#105950 = DIRECTION ( 'NONE',  ( 0.000000000000000000, -1.000000000000000000, 0.000000000000000000 ) ) ;
#105951 = VECTOR ( 'NONE', #26500, 1000.000000000000000 ) ;
#105952 = DIRECTION ( 'NONE',  ( -0.7071067811865487940, 0.7071067811865463515, -0.000000000000000000 ) ) ;
#105953 = CARTESIAN_POINT ( 'NONE',  ( 45.55793019189811588, 6.110000000000000320, -1.637169565754156064 ) ) ;
#105954 = ORIENTED_EDGE ( 'NONE', *, *, #120521, .F. ) ;
#105955 = FACE_OUTER_BOUND ( 'NONE', #30611, .T. ) ;
#105956 = DIRECTION ( 'NONE',  ( 0.7071067811865486830, -0.7071067811865464625, -0.000000000000000000 ) ) ;
#105957 = ORIENTED_EDGE ( 'NONE', *, *, #77882, .T. ) ;
#105958 = EDGE_LOOP ( 'NONE', ( #138889, #56573, #67600, #99009 ) ) ;
#105959 = DIRECTION ( 'NONE',  ( -0.000000000000000000, 0.3543493200069153248, 0.9351131265310292928 ) ) ;
#105960 = EDGE_LOOP ( 'NONE', ( #46010, #10271, #1551, #78140 ) ) ;
#105961 = EDGE_CURVE ( 'NONE', #75676, #108628, #22188, .T. ) ;
#105962 = DIRECTION ( 'NONE',  ( -0.7071067811865486830, -0.7071067811865464625, 0.000000000000000000 ) ) ;
#105963 = VERTEX_POINT ( 'NONE', #55573 ) ;
#105964 = CARTESIAN_POINT ( 'NONE',  ( -11.67183060077638856, 11.25929247661560595, 4.000000000000000000 ) ) ;
#105965 = DIRECTION ( 'NONE',  ( -0.000000000000000000, -0.3543493200069152693, 0.9351131265310292928 ) ) ;
#105966 = FACE_OUTER_BOUND ( 'NONE', #86306, .T. ) ;
#105967 = AXIS2_PLACEMENT_3D ( 'NONE', #10598, #55575, #63611 ) ;
#105968 = FACE_BOUND ( 'NONE', #93105, .T. ) ;
#105969 = CARTESIAN_POINT ( 'NONE',  ( 0.000000000000000000, 2.375000000000000000, 1.069999999999998508 ) ) ;
#105970 = PLANE ( 'NONE',  #66469 ) ;
#105971 = VERTEX_POINT ( 'NONE', #436 ) ;
#105972 = DIRECTION ( 'NONE',  ( 0.3543493200069162685, -0.000000000000000000, -0.9351131265310288487 ) ) ;
#105974 = ORIENTED_EDGE ( 'NONE', *, *, #53086, .F. ) ;
#105973 = CARTESIAN_POINT ( 'NONE',  ( -12.48921356237309155, -27.52281430457064104, 5.000000000000000000 ) ) ;
#105975 = ORIENTED_EDGE ( 'NONE', *, *, #70412, .T. ) ;
#105976 = CYLINDRICAL_SURFACE ( 'NONE', #123546, 6.350000000000004086 ) ;
#105977 = ORIENTED_EDGE ( 'NONE', *, *, #75314, .T. ) ;
#105978 = EDGE_CURVE ( 'NONE', #95760, #135278, #44732, .T. ) ;
#105979 = CARTESIAN_POINT ( 'NONE',  ( 55.03709685856478018, -3.054999999999998828, -5.291415217122919401 ) ) ;
#105980 = EDGE_LOOP ( 'NONE', ( #43814, #73974, #126464, #26997 ) ) ;
#105981 = VECTOR ( 'NONE', #28281, 1000.000000000000000 ) ;
#105982 = DIRECTION ( 'NONE',  ( -0.6830127018922180770, -0.6830127018922204085, -0.2588190451025213501 ) ) ;
#105983 = EDGE_CURVE ( 'NONE', #139966, #1660, #31513, .T. ) ;
#105984 = CARTESIAN_POINT ( 'NONE',  ( 11.56505274454301357, 2.500000000000000888, 0.000000000000000000 ) ) ;
#105985 = ORIENTED_EDGE ( 'NONE', *, *, #134037, .T. ) ;
#105986 = CARTESIAN_POINT ( 'NONE',  ( -51.48921356237309510, -27.52281430457091460, 5.000000000000000000 ) ) ;
#105987 = EDGE_CURVE ( 'NONE', #92017, #110318, #45428, .T. ) ;
#105988 = EDGE_CURVE ( 'NONE', #75431, #43122, #57016, .T. ) ;
#105989 = CIRCLE ( 'NONE', #38870, 31.93000000000001393 ) ;
#105990 = LINE ( 'NONE', #137955, #64108 ) ;
#105991 = CARTESIAN_POINT ( 'NONE',  ( 14.59122188827396549, 7.143407583703162089, 5.000000000000000000 ) ) ;
#105992 = CYLINDRICAL_SURFACE ( 'NONE', #43543, 4.000000000000000000 ) ;
#105993 = PLANE ( 'NONE',  #65478 ) ;
#105994 = CARTESIAN_POINT ( 'NONE',  ( -30.48921356237309510, -27.52281430457076894, 5.000000000000000000 ) ) ;
#105995 = ORIENTED_EDGE ( 'NONE', *, *, #65143, .F. ) ;
#105996 = ORIENTED_EDGE ( 'NONE', *, *, #39665, .F. ) ;
#105997 = CARTESIAN_POINT ( 'NONE',  ( 9.489213562373095101, -27.52281430457062328, 5.000000000000000000 ) ) ;
#105999 = CARTESIAN_POINT ( 'NONE',  ( -3.489213562373097322, -27.52281430457057709, 5.000000000000000000 ) ) ;
#105998 = AXIS2_PLACEMENT_3D ( 'NONE', #80925, #36002, #23672 ) ;
#106000 = ORIENTED_EDGE ( 'NONE', *, *, #141757, .T. ) ;
#106001 = ORIENTED_EDGE ( 'NONE', *, *, #52298, .T. ) ;
#106002 = EDGE_LOOP ( 'NONE', ( #141884, #40476, #40885, #87548 ) ) ;
#106003 = PLANE ( 'NONE',  #18912 ) ;
#106004 = EDGE_CURVE ( 'NONE', #142848, #131756, #135287, .T. ) ;
#106005 = EDGE_CURVE ( 'NONE', #21906, #99997, #105670, .T. ) ;
#106006 = DIRECTION ( 'NONE',  ( -0.000000000000000000, 0.000000000000000000, 1.000000000000000000 ) ) ;
#106007 = ORIENTED_EDGE ( 'NONE', *, *, #52818, .T. ) ;
#106008 = DIRECTION ( 'NONE',  ( -0.000000000000000000, 0.000000000000000000, 1.000000000000000000 ) ) ;
#106009 = VECTOR ( 'NONE', #103167, 1000.000000000000227 ) ;
#106010 = VECTOR ( 'NONE', #124563, 1000.000000000000000 ) ;
#106011 = EDGE_CURVE ( 'NONE', #139983, #24621, #24350, .T. ) ;
#106012 = CARTESIAN_POINT ( 'NONE',  ( 8.233736474768550195, 5.808823158059036373, 5.808823158059032821 ) ) ;
#106013 = DIRECTION ( 'NONE',  ( -0.7071067811865486830, -0.7071067811865464625, 0.000000000000000000 ) ) ;
#106014 = ORIENTED_EDGE ( 'NONE', *, *, #103694, .F. ) ;
#106015 = CARTESIAN_POINT ( 'NONE',  ( 11.99999999999991651, -21.41253812416053748, 4.000000000000000000 ) ) ;
#106016 = CARTESIAN_POINT ( 'NONE',  ( -51.18398860626899705, 28.73617430169823095, 5.000000000000000000 ) ) ;
#106017 = FACE_OUTER_BOUND ( 'NONE', #6425, .T. ) ;
#106018 = EDGE_CURVE ( 'NONE', #122980, #30015, #67154, .T. ) ;
#106020 = ORIENTED_EDGE ( 'NONE', *, *, #139595, .T. ) ;
#106019 = LINE ( 'NONE', #50967, #100144 ) ;
#106021 = CARTESIAN_POINT ( 'NONE',  ( 11.27497294953710671, 4.461849672132300881, 4.461849672132299105 ) ) ;
#106022 = VERTEX_POINT ( 'NONE', #101191 ) ;
#106023 = DIRECTION ( 'NONE',  ( -0.000000000000000000, -0.3543493200069152693, 0.9351131265310292928 ) ) ;
#106024 = CARTESIAN_POINT ( 'NONE',  ( 66.18398860626901126, 28.73617430169833753, 5.000000000000000000 ) ) ;
#106025 = CARTESIAN_POINT ( 'NONE',  ( -12.69999999999998153, 0.000000000000000000, 2.500000000000000444 ) ) ;
#106026 = ORIENTED_EDGE ( 'NONE', *, *, #5413, .T. ) ;
#106027 = DIRECTION ( 'NONE',  ( 0.7071067811865487940, -0.7071067811865463515, 0.000000000000000000 ) ) ;
#106028 = DIRECTION ( 'NONE',  ( 0.6830127018922181881, 0.6830127018922202975, -0.2588190451025214056 ) ) ;
#106029 = DIRECTION ( 'NONE',  ( 0.7071067811865486830, -0.7071067811865464625, -0.000000000000000000 ) ) ;
#106030 = EDGE_CURVE ( 'NONE', #23774, #121207, #45514, .T. ) ;
#106031 = ORIENTED_EDGE ( 'NONE', *, *, #12820, .T. ) ;
#106032 = CARTESIAN_POINT ( 'NONE',  ( 7.734933297179447109, 12.75929247661558286, 18.34774599283954544 ) ) ;
#106033 = CARTESIAN_POINT ( 'NONE',  ( -5.207106781186502609, -11.24070752338417201, 5.000000000000000000 ) ) ;
#106035 = CIRCLE ( 'NONE', #117620, 5.968999999999998529 ) ;
#106034 = CARTESIAN_POINT ( 'NONE',  ( 42.18398860626899705, 28.73617430169816700, 5.000000000000000000 ) ) ;
#106036 = DIRECTION ( 'NONE',  ( -0.000000000000000000, 0.000000000000000000, 1.000000000000000000 ) ) ;
#106037 = DIRECTION ( 'NONE',  ( 0.000000000000000000, 0.000000000000000000, 1.000000000000000000 ) ) ;
#106038 = ORIENTED_EDGE ( 'NONE', *, *, #7755, .T. ) ;
#106039 = ADVANCED_FACE ( 'NONE', ( #102646 ), #90316, .F. ) ;
#106040 = VERTEX_POINT ( 'NONE', #22885 ) ;
#106042 = EDGE_CURVE ( 'NONE', #140110, #57808, #14180, .T. ) ;
#106041 = VECTOR ( 'NONE', #1504, 1000.000000000000000 ) ;
#106043 = DIRECTION ( 'NONE',  ( 1.734723475976806848E-16, -1.000000000000000000, 0.000000000000000000 ) ) ;
#106044 = CARTESIAN_POINT ( 'NONE',  ( 42.18398860626899705, 28.73617430169816700, 5.000000000000000000 ) ) ;
#106045 = EDGE_CURVE ( 'NONE', #110443, #24733, #100500, .T. ) ;
#106046 = CARTESIAN_POINT ( 'NONE',  ( 2.020403141435219485, 7.934999999999989839, -2.126176841940961904 ) ) ;
#106047 = PLANE ( 'NONE',  #94465 ) ;
#106048 = CARTESIAN_POINT ( 'NONE',  ( -28.17183060077627488, 6.759292476615645917, 4.000000000000000000 ) ) ;
#106049 = FACE_OUTER_BOUND ( 'NONE', #81545, .T. ) ;
#106050 = EDGE_LOOP ( 'NONE', ( #48475, #108141, #120372, #97419 ) ) ;
#106051 = FACE_OUTER_BOUND ( 'NONE', #53572, .T. ) ;
#106052 = CARTESIAN_POINT ( 'NONE',  ( 34.92499999999999005, -6.281509562795680957, 4.759050581649329814 ) ) ;
#106053 = DIRECTION ( 'NONE',  ( 0.6830127018922181881, 0.6830127018922202975, -0.2588190451025214056 ) ) ;
#106054 = AXIS2_PLACEMENT_3D ( 'NONE', #79701, #91936, #36154 ) ;
#106055 = CARTESIAN_POINT ( 'NONE',  ( 49.49543019189811588, 5.291415217122917625, 3.055000000000002380 ) ) ;
#106056 = LINE ( 'NONE', #19078, #46504 ) ;
#106057 = VECTOR ( 'NONE', #88814, 1000.000000000000000 ) ;
#106058 = EDGE_LOOP ( 'NONE', ( #122666, #73611, #75455, #48552 ) ) ;
#106059 = DIRECTION ( 'NONE',  ( 0.7071067811865487940, 0.7071067811865463515, -0.000000000000000000 ) ) ;
#106060 = VERTEX_POINT ( 'NONE', #35264 ) ;
#106061 = ADVANCED_FACE ( 'NONE', ( #114210 ), #1146, .T. ) ;
#106062 = VERTEX_POINT ( 'NONE', #91741 ) ;
#106063 = DIRECTION ( 'NONE',  ( -1.000000000000000000, 0.000000000000000000, -0.000000000000000000 ) ) ;
#106064 = CARTESIAN_POINT ( 'NONE',  ( 0.000000000000000000, 0.000000000000000000, 5.000000000000000000 ) ) ;
#106065 = CARTESIAN_POINT ( 'NONE',  ( 24.18398860626899705, 28.73617430169804265, 5.000000000000000000 ) ) ;
#106066 = DIRECTION ( 'NONE',  ( -0.3543493200069162685, -0.000000000000000000, -0.9351131265310288487 ) ) ;
#106067 = CYLINDRICAL_SURFACE ( 'NONE', #2483, 9.119999999999999218 ) ;
#106068 = EDGE_CURVE ( 'NONE', #78734, #5013, #26952, .T. ) ;
#106069 = VERTEX_POINT ( 'NONE', #124381 ) ;
#106070 = CARTESIAN_POINT ( 'NONE',  ( -13.99806943317891772, -22.22500000000000142, 4.500000000000000888 ) ) ;
#106071 = CARTESIAN_POINT ( 'NONE',  ( 6.241694584251833433, 0.7592924766157138627, 14.37146558664981555 ) ) ;
#106072 = CARTESIAN_POINT ( 'NONE',  ( -25.78678096696625843, 12.75929247661558996, 10.29404684609029275 ) ) ;
#106073 = FILL_AREA_STYLE ('',( #61921 ) ) ;
#106074 = DIRECTION ( 'NONE',  ( -0.000000000000000000, -0.3543493200069152693, 0.9351131265310292928 ) ) ;
#106075 = DIRECTION ( 'NONE',  ( 0.7071067811865486830, -0.7071067811865464625, -0.000000000000000000 ) ) ;
#106076 = CARTESIAN_POINT ( 'NONE',  ( 61.47502705046287730, -5.819803920172572198, 5.819803920172572198 ) ) ;
#106077 = DIRECTION ( 'NONE',  ( 0.7071067811865487940, 0.7071067811865463515, 0.000000000000000000 ) ) ;
#106078 = ORIENTED_EDGE ( 'NONE', *, *, #29839, .T. ) ;
#106079 = ORIENTED_EDGE ( 'NONE', *, *, #107947, .F. ) ;
#106080 = AXIS2_PLACEMENT_3D ( 'NONE', #82168, #16881, #49540 ) ;
#106081 = CARTESIAN_POINT ( 'NONE',  ( 54.08333333333332860, 6.884901960086290629, -3.974999999999994316 ) ) ;
#106082 = CARTESIAN_POINT ( 'NONE',  ( 31.92500000000001492, 2.730000000000007088, -36.39086428169088094 ) ) ;
#106083 = DIRECTION ( 'NONE',  ( -0.000000000000000000, 0.000000000000000000, 1.000000000000000000 ) ) ;
#106084 = ADVANCED_FACE ( 'NONE', ( #25049 ), #79505, .F. ) ;
#106085 = ADVANCED_FACE ( 'NONE', ( #69300 ), #122959, .F. ) ;
#106086 = ORIENTED_EDGE ( 'NONE', *, *, #55829, .F. ) ;
#106087 = DIRECTION ( 'NONE',  ( -1.000000000000000000, -3.115803279706882722E-16, -0.000000000000000000 ) ) ;
#106088 = AXIS2_PLACEMENT_3D ( 'NONE', #39214, #92861, #50098 ) ;
#106089 = CARTESIAN_POINT ( 'NONE',  ( 54.25043019189811133, 3.055000000000002824, -5.291415217122919401 ) ) ;
#106090 = EDGE_CURVE ( 'NONE', #1673, #128813, #26498, .T. ) ;
#106091 = ORIENTED_EDGE ( 'NONE', *, *, #107455, .F. ) ;
#106092 = CARTESIAN_POINT ( 'NONE',  ( 12.32816939922344446, 8.259292476615637923, 4.000000000000000000 ) ) ;
#106093 = ORIENTED_EDGE ( 'NONE', *, *, #34636, .F. ) ;
#106094 = ORIENTED_EDGE ( 'NONE', *, *, #91700, .F. ) ;
#106095 = PLANE ( 'NONE',  #53928 ) ;
#106096 = AXIS2_PLACEMENT_3D ( 'NONE', #66611, #102812, #35441 ) ;
#106097 = VECTOR ( 'NONE', #131200, 1000.000000000000000 ) ;
#106098 = LINE ( 'NONE', #118427, #1305 ) ;
#106099 = LINE ( 'NONE', #31441, #90634 ) ;
#106100 = VECTOR ( 'NONE', #82303, 999.9999999999998863 ) ;
#106101 = CARTESIAN_POINT ( 'NONE',  ( 28.49999999999979039, 16.08746187583908949, 4.000000000000000000 ) ) ;
#106102 = ADVANCED_FACE ( 'NONE', ( #28656 ), #70743, .T. ) ;
#106104 = AXIS2_PLACEMENT_3D ( 'NONE', #39773, #52056, #139802 ) ;
#106103 = CARTESIAN_POINT ( 'NONE',  ( -21.29974487139158512, -27.71228299555221142, 4.000000000000000000 ) ) ;
#106106 = ORIENTED_EDGE ( 'NONE', *, *, #76406, .F. ) ;
#106105 = LINE ( 'NONE', #104708, #100843 ) ;
#106107 = EDGE_CURVE ( 'NONE', #38833, #126622, #82319, .T. ) ;
#106108 = CARTESIAN_POINT ( 'NONE',  ( -29.99451991528749417, 28.92564299267958816, 4.000000000000000000 ) ) ;
#106109 = CARTESIAN_POINT ( 'NONE',  ( -18.10180811604841011, 9.068207373850700748, 5.000000000000000000 ) ) ;
#106110 = CARTESIAN_POINT ( 'NONE',  ( -10.49999999999992184, -16.91253812416058722, 4.000000000000000000 ) ) ;
#106112 = DIRECTION ( 'NONE',  ( 0.000000000000000000, -0.5150380749100594846, -0.8571673007021091140 ) ) ;
#106111 = AXIS2_PLACEMENT_3D ( 'NONE', #92104, #24018, #14561 ) ;
#106113 = CARTESIAN_POINT ( 'NONE',  ( -34.92500000000001137, 18.00612307739175222, 4.000000000000000000 ) ) ;
#106114 = VECTOR ( 'NONE', #68494, 1000.000000000000000 ) ;
#106115 = ORIENTED_EDGE ( 'NONE', *, *, #118068, .T. ) ;
#106116 = VERTEX_POINT ( 'NONE', #62712 ) ;
#106117 = EDGE_CURVE ( 'NONE', #75310, #30975, #98661, .T. ) ;
#106118 = CARTESIAN_POINT ( 'NONE',  ( -16.17183060077636014, 9.759292476615621936, 4.000000000000000000 ) ) ;
#106119 = CARTESIAN_POINT ( 'NONE',  ( -17.99999999999986855, -13.44781430457069149, 5.000000000000000000 ) ) ;
#106120 = CARTESIAN_POINT ( 'NONE',  ( 29.48334561358934991, 22.22500000000000142, 4.500000000000000888 ) ) ;
#106121 = VERTEX_POINT ( 'NONE', #17726 ) ;
#106122 = ORIENTED_EDGE ( 'NONE', *, *, #100448, .T. ) ;
#106123 = VECTOR ( 'NONE', #34401, 1000.000000000000000 ) ;
#106124 = DIRECTION ( 'NONE',  ( -0.7071067811865487940, 0.7071067811865463515, 0.000000000000000000 ) ) ;
#106125 = CARTESIAN_POINT ( 'NONE',  ( -34.49999999999975131, 9.054329344830845727, 4.994342998332165884 ) ) ;
#106126 = ORIENTED_EDGE ( 'NONE', *, *, #137656, .T. ) ;
#106127 = EDGE_CURVE ( 'NONE', #129488, #128836, #95310, .T. ) ;
#106128 = VERTEX_POINT ( 'NONE', #59849 ) ;
#106129 = PRESENTATION_LAYER_ASSIGNMENT (  '', '', ( #25110 ) ) ;
#106130 = DIRECTION ( 'NONE',  ( -1.000000000000000000, -0.000000000000000000, -0.000000000000000000 ) ) ;
#106131 = ORIENTED_EDGE ( 'NONE', *, *, #50684, .F. ) ;
#106132 = DIRECTION ( 'NONE',  ( -0.000000000000000000, 0.000000000000000000, 1.000000000000000000 ) ) ;
#106133 = VECTOR ( 'NONE', #25256, 999.9999999999998863 ) ;
#106134 = FACE_BOUND ( 'NONE', #137763, .T. ) ;
#106135 = DIRECTION ( 'NONE',  ( 0.7071067811865486830, -0.7071067811865464625, -0.000000000000000000 ) ) ;
#106136 = LINE ( 'NONE', #95291, #83697 ) ;
#106137 = CARTESIAN_POINT ( 'NONE',  ( -34.42500000000001137, 16.54139925780184583, 5.000000000000000000 ) ) ;
#106139 = ORIENTED_EDGE ( 'NONE', *, *, #44181, .T. ) ;
#106138 = LINE ( 'NONE', #85132, #105904 ) ;
#106140 = VECTOR ( 'NONE', #7101, 999.9999999999998863 ) ;
#106141 = LINE ( 'NONE', #41628, #9273 ) ;
#106142 = APPLICATION_PROTOCOL_DEFINITION ( 'draft international standard', 'automotive_design', 1998, #112406 ) ;
#106143 = ORIENTED_EDGE ( 'NONE', *, *, #87087, .T. ) ;
#106145 = ORIENTED_EDGE ( 'NONE', *, *, #113857, .T. ) ;
#106144 = EDGE_CURVE ( 'NONE', #58244, #92406, #83764, .T. ) ;
#106146 = CARTESIAN_POINT ( 'NONE',  ( 94.41209685856478018, 5.291415217122921177, -3.054999999999994831 ) ) ;
#106147 = ORIENTED_EDGE ( 'NONE', *, *, #3659, .F. ) ;
#106148 = DIRECTION ( 'NONE',  ( 1.000000000000000000, 0.000000000000000000, 0.000000000000000000 ) ) ;
#106149 = DIRECTION ( 'NONE',  ( 1.000000000000000000, -0.000000000000000000, -0.000000000000000000 ) ) ;
#106150 = EDGE_CURVE ( 'NONE', #87892, #65237, #126500, .T. ) ;
#106151 = PLANE ( 'NONE',  #141676 ) ;
#106152 = CONICAL_SURFACE ( 'NONE', #99223, 2.500000000000000444, 0.9599310885968830309 ) ;
#106153 = CARTESIAN_POINT ( 'NONE',  ( -30.29974487139158867, -27.71228299555227537, 4.000000000000000000 ) ) ;
#106155 = EDGE_CURVE ( 'NONE', #11479, #79851, #106160, .T. ) ;
#106154 = AXIS2_PLACEMENT_3D ( 'NONE', #84371, #138014, #6721 ) ;
#106156 = EDGE_CURVE ( 'NONE', #13538, #40966, #15333, .T. ) ;
#106157 = PLANE ( 'NONE',  #135082 ) ;
#106158 = ORIENTED_EDGE ( 'NONE', *, *, #77569, .T. ) ;
#106159 = CARTESIAN_POINT ( 'NONE',  ( -45.48921356237309510, -27.52281430457087197, 5.000000000000000000 ) ) ;
#106160 = LINE ( 'NONE', #6831, #112636 ) ;
#106161 = CARTESIAN_POINT ( 'NONE',  ( 9.183988606268997046, 28.73617430169793607, 5.000000000000000000 ) ) ;
#106162 = CARTESIAN_POINT ( 'NONE',  ( -9.489213562373095101, -27.52281430457062328, 5.000000000000000000 ) ) ;
#106163 = PLANE ( 'NONE',  #130340 ) ;
#106164 = DIRECTION ( 'NONE',  ( -0.7071067811865486830, 0.7071067811865464625, 0.000000000000000000 ) ) ;
#106165 = LINE ( 'NONE', #6128, #26061 ) ;
#106166 = EDGE_LOOP ( 'NONE', ( #18770, #93302, #129714, #88835 ) ) ;
#106167 = EDGE_CURVE ( 'NONE', #79985, #45274, #115588, .T. ) ;
#106168 = DIRECTION ( 'NONE',  ( -0.7071067811865486830, -0.7071067811865464625, 0.000000000000000000 ) ) ;
#106169 = LINE ( 'NONE', #128671, #92976 ) ;
#106170 = VERTEX_POINT ( 'NONE', #117746 ) ;
#106171 = ORIENTED_EDGE ( 'NONE', *, *, #64136, .T. ) ;
#106172 = EDGE_CURVE ( 'NONE', #112546, #63574, #125822, .T. ) ;
#106174 = ORIENTED_EDGE ( 'NONE', *, *, #58835, .F. ) ;
#106173 = ADVANCED_FACE ( 'NONE', ( #106893 ), #104015, .T. ) ;
#106175 = CARTESIAN_POINT ( 'NONE',  ( 48.70876352523144703, -7.482591942790329030E-16, 6.110000000000001208 ) ) ;
#106176 = ORIENTED_EDGE ( 'NONE', *, *, #659, .F. ) ;
#106177 = ADVANCED_FACE ( 'NONE', ( #93178 ), #72188, .F. ) ;
#106178 = CARTESIAN_POINT ( 'NONE',  ( 11.85830628287044064, -1.633150327867689988, 6.094999999999989981 ) ) ;
#106179 = CARTESIAN_POINT ( 'NONE',  ( -9.771348248178298945, 11.46486773387262126, -26.00442996100349546 ) ) ;
#106180 = EDGE_CURVE ( 'NONE', #51758, #9966, #8390, .T. ) ;
#106181 = ORIENTED_EDGE ( 'NONE', *, *, #26776, .T. ) ;
#106182 = DIRECTION ( 'NONE',  ( 0.6830127018922180770, -0.6830127018922204085, -0.2588190451025213501 ) ) ;
#106183 = VERTEX_POINT ( 'NONE', #83024 ) ;
#106184 = CARTESIAN_POINT ( 'NONE',  ( 36.48921356237310221, -27.52281430457080802, 5.000000000000000000 ) ) ;
#106185 = FACE_OUTER_BOUND ( 'NONE', #143138, .T. ) ;
#106186 = EDGE_CURVE ( 'NONE', #88846, #73668, #105456, .T. ) ;
#106188 = ORIENTED_EDGE ( 'NONE', *, *, #35678, .T. ) ;
#106187 = CARTESIAN_POINT ( 'NONE',  ( -39.18398860626899705, 28.73617430169814568, 5.000000000000000000 ) ) ;
#106189 = ORIENTED_EDGE ( 'NONE', *, *, #89128, .F. ) ;
#106190 = DIRECTION ( 'NONE',  ( 0.6830127018922181881, 0.6830127018922202975, -0.2588190451025214056 ) ) ;
#106191 = LINE ( 'NONE', #61345, #122518 ) ;
#106192 = ORIENTED_EDGE ( 'NONE', *, *, #16642, .T. ) ;
#106193 = FACE_OUTER_BOUND ( 'NONE', #59529, .T. ) ;
#106194 = ORIENTED_EDGE ( 'NONE', *, *, #77196, .F. ) ;
#106195 = ORIENTED_EDGE ( 'NONE', *, *, #62369, .T. ) ;
#106196 = ORIENTED_EDGE ( 'NONE', *, *, #16269, .T. ) ;
#106197 = ORIENTED_EDGE ( 'NONE', *, *, #2999, .F. ) ;
#106198 = FACE_OUTER_BOUND ( 'NONE', #107251, .T. ) ;
#106199 = ADVANCED_FACE ( 'NONE', ( #98182 ), #96021, .F. ) ;
#106200 = AXIS2_PLACEMENT_3D ( 'NONE', #117055, #91740, #17048 ) ;
#106201 = VECTOR ( 'NONE', #20819, 1000.000000000000000 ) ;
#106202 = AXIS2_PLACEMENT_3D ( 'NONE', #136300, #46500, #36981 ) ;
#106203 = CARTESIAN_POINT ( 'NONE',  ( -6.328169399223484426, 11.25929247661560773, 4.000000000000000000 ) ) ;
#106204 = CARTESIAN_POINT ( 'NONE',  ( -0.2997448713915885632, -27.71228299555206220, 4.000000000000000000 ) ) ;
#106205 = CARTESIAN_POINT ( 'NONE',  ( 4.828169399223496860, -11.24070752338416845, 4.000000000000000000 ) ) ;
#106206 = ORIENTED_EDGE ( 'NONE', *, *, #97627, .F. ) ;
#106207 = FACE_OUTER_BOUND ( 'NONE', #84213, .T. ) ;
#106208 = VERTEX_POINT ( 'NONE', #74296 ) ;
#106209 = EDGE_CURVE ( 'NONE', #134021, #13302, #109759, .T. ) ;
#106210 = VECTOR ( 'NONE', #98388, 999.9999999999998863 ) ;
#106211 = CYLINDRICAL_SURFACE ( 'NONE', #114230, 7.950000000000000178 ) ;
#106212 = EDGE_CURVE ( 'NONE', #137243, #2775, #53223, .T. ) ;
#106213 = CARTESIAN_POINT ( 'NONE',  ( 10.06000000000000050, -2.055000000000000160, 2.789133085058098087E-16 ) ) ;
#106214 = CARTESIAN_POINT ( 'NONE',  ( 8.206660635421465955, 21.75929247661549226, 4.998822639870702744 ) ) ;
#106215 = VERTEX_POINT ( 'NONE', #21332 ) ;
#106216 = CARTESIAN_POINT ( 'NONE',  ( 96.66666666666667140, 6.884901960086285300, 3.975000000000003642 ) ) ;
#106217 = DIRECTION ( 'NONE',  ( -0.7071067811865487940, 0.7071067811865463515, -0.000000000000000000 ) ) ;
#106218 = VERTEX_POINT ( 'NONE', #132265 ) ;
#106219 = VERTEX_POINT ( 'NONE', #130101 ) ;
#106220 = ORIENTED_EDGE ( 'NONE', *, *, #17095, .T. ) ;
#106221 = LINE ( 'NONE', #129422, #32504 ) ;
#106222 = CARTESIAN_POINT ( 'NONE',  ( -13.79551713769220811, 6.008391563887172993, 4.335713449946893228 ) ) ;
#106223 = PLANE ( 'NONE',  #114784 ) ;
#106224 = VECTOR ( 'NONE', #39233, 999.9999999999998863 ) ;
#106225 = DIRECTION ( 'NONE',  ( 1.000000000000000000, -0.000000000000000000, 0.000000000000000000 ) ) ;
#106226 = EDGE_CURVE ( 'NONE', #23170, #84791, #36179, .T. ) ;
#106227 = CARTESIAN_POINT ( 'NONE',  ( -0.7928932188134494297, 18.75929247661552068, 5.000000000000000000 ) ) ;
#106228 = CARTESIAN_POINT ( 'NONE',  ( 74.87043019189812298, -3.055000000000001936, 5.291415217122918513 ) ) ;
#106230 = CARTESIAN_POINT ( 'NONE',  ( -31.49999999999977973, -10.04351517176480257, -1.623559851933897624 ) ) ;
#106229 = VECTOR ( 'NONE', #24279, 1000.000000000000000 ) ;
#106231 = DIRECTION ( 'NONE',  ( 0.6830127018922180770, -0.6830127018922204085, -0.2588190451025213501 ) ) ;
#106232 = DIRECTION ( 'NONE',  ( 0.000000000000000000, 0.000000000000000000, 1.000000000000000000 ) ) ;
#106233 = FACE_OUTER_BOUND ( 'NONE', #38884, .T. ) ;
#106234 = ORIENTED_EDGE ( 'NONE', *, *, #32611, .T. ) ;
#106235 = CARTESIAN_POINT ( 'NONE',  ( 34.92499999999998295, -8.337538124160891684, 4.000000000000000000 ) ) ;
#106236 = ORIENTED_EDGE ( 'NONE', *, *, #111123, .F. ) ;
#106237 = VECTOR ( 'NONE', #114846, 1000.000000000000000 ) ;
#106238 = AXIS2_PLACEMENT_3D ( 'NONE', #72816, #118387, #63351 ) ;
#106239 = CARTESIAN_POINT ( 'NONE',  ( -39.18398860626899705, 28.73617430169814568, 5.000000000000000000 ) ) ;
#106241 = ORIENTED_EDGE ( 'NONE', *, *, #70605, .F. ) ;
#106240 = DIRECTION ( 'NONE',  ( 1.734723475976806848E-16, -1.000000000000000000, 0.000000000000000000 ) ) ;
#106242 = DIRECTION ( 'NONE',  ( 1.000000000000000000, 0.000000000000000000, 0.000000000000000000 ) ) ;
#106243 = DIRECTION ( 'NONE',  ( -0.7071067811865486830, -0.7071067811865463515, 0.000000000000000000 ) ) ;
#106244 = EDGE_LOOP ( 'NONE', ( #62138, #83345, #64524, #9359 ) ) ;
#106245 = ORIENTED_EDGE ( 'NONE', *, *, #101647, .F. ) ;
#106246 = DIRECTION ( 'NONE',  ( 0.7071067811865487940, 0.7071067811865463515, -0.000000000000000000 ) ) ;
#106247 = CARTESIAN_POINT ( 'NONE',  ( -21.18398860626899349, 28.73617430169802134, 5.000000000000000000 ) ) ;
#106248 = VECTOR ( 'NONE', #12127, 1000.000000000000000 ) ;
#106249 = AXIS2_PLACEMENT_3D ( 'NONE', #78956, #11486, #12931 ) ;
#106250 = CARTESIAN_POINT ( 'NONE',  ( 25.39999999999999503, 3.246059068589359775, 5.158694168414005077 ) ) ;
#106251 = CARTESIAN_POINT ( 'NONE',  ( 98.07919371712955581, 3.975000000000002753, -6.884901960086283523 ) ) ;
#106252 = LINE ( 'NONE', #6925, #83383 ) ;
#106253 = FILL_AREA_STYLE_COLOUR ( '', #99191 ) ;
#106254 = ORIENTED_EDGE ( 'NONE', *, *, #95577, .T. ) ;
#106255 = FACE_OUTER_BOUND ( 'NONE', #99047, .T. ) ;
#106256 = EDGE_CURVE ( 'NONE', #11616, #102743, #57099, .T. ) ;
#106257 = CARTESIAN_POINT ( 'NONE',  ( 33.68750000000000711, 4.461849672132297329, -4.461849672132302658 ) ) ;
#106258 = CIRCLE ( 'NONE', #127187, 6.499999999999999112 ) ;
#106259 = FACE_OUTER_BOUND ( 'NONE', #45820, .T. ) ;
#106260 = EDGE_LOOP ( 'NONE', ( #102115, #57959, #61186, #123996 ) ) ;
#106262 = EDGE_CURVE ( 'NONE', #90802, #98883, #64126, .T. ) ;
#106261 = CARTESIAN_POINT ( 'NONE',  ( 22.37177410554622980, -1.784312229707115893, 4.000000000000000000 ) ) ;
#106263 = ORIENTED_EDGE ( 'NONE', *, *, #72980, .T. ) ;
#106264 = CARTESIAN_POINT ( 'NONE',  ( 83.85459685856478984, -1.637169565754161615, 6.110000000000000320 ) ) ;
#106265 = PLANE ( 'NONE',  #43200 ) ;
#106266 = DIRECTION ( 'NONE',  ( 0.3543493200069162685, -0.000000000000000000, -0.9351131265310288487 ) ) ;
#106267 = LINE ( 'NONE', #139686, #45644 ) ;
#106268 = ORIENTED_EDGE ( 'NONE', *, *, #44984, .T. ) ;
#106269 = CARTESIAN_POINT ( 'NONE',  ( -14.99999999999987743, -16.44781430457066662, 5.000000000000000000 ) ) ;
#106270 = DIRECTION ( 'NONE',  ( 2.110369192185896011E-16, -1.000000000000000000, 0.000000000000000000 ) ) ;
#106271 = CARTESIAN_POINT ( 'NONE',  ( -3.299744871391591339, -27.71228299555208352, 4.000000000000000000 ) ) ;
#106272 = ADVANCED_FACE ( 'NONE', ( #119891 ), #107611, .F. ) ;
#106274 = ORIENTED_EDGE ( 'NONE', *, *, #92752, .F. ) ;
#106273 = CARTESIAN_POINT ( 'NONE',  ( -19.05000000000000071, 3.174999999999997158, 4.000000000000000000 ) ) ;
#106275 = CARTESIAN_POINT ( 'NONE',  ( 12.39583333333333570, 1.633150327867697316, -6.094999999999986429 ) ) ;
#106276 = LINE ( 'NONE', #17846, #91666 ) ;
#106277 = CARTESIAN_POINT ( 'NONE',  ( 1.944300147912140453, -5.919729343870397287, 1.711352533870144521 ) ) ;
#106278 = ADVANCED_FACE ( 'NONE', ( #19185 ), #30044, .F. ) ;
#106280 = EDGE_LOOP ( 'NONE', ( #100413, #56344, #102302, #68358 ) ) ;
#106279 = EDGE_CURVE ( 'NONE', #111687, #123393, #40944, .T. ) ;
#106281 = ORIENTED_EDGE ( 'NONE', *, *, #36112, .T. ) ;
#106282 = CARTESIAN_POINT ( 'NONE',  ( 75.83376352523144703, 6.110000000000001208, 1.122388791418549305E-15 ) ) ;
#106283 = ORIENTED_EDGE ( 'NONE', *, *, #30792, .T. ) ;
#106284 = EDGE_CURVE ( 'NONE', #89804, #133506, #98868, .T. ) ;
#106285 = PRESENTATION_STYLE_ASSIGNMENT (( #138247 ) ) ;
#106286 = CARTESIAN_POINT ( 'NONE',  ( 24.64327148205084939, 5.259292476615662792, 4.831541298974423526 ) ) ;
#106287 = PLANE ( 'NONE',  #50385 ) ;
#106288 = VERTEX_POINT ( 'NONE', #109030 ) ;
#106289 = PLANE ( 'NONE',  #44434 ) ;
#106290 = CARTESIAN_POINT ( 'NONE',  ( 166.8575281714868481, 26.96999999999994202, -31.92499999999998295 ) ) ;
#106291 = EDGE_CURVE ( 'NONE', #123046, #33185, #43098, .T. ) ;
#106292 = VERTEX_POINT ( 'NONE', #31496 ) ;
#106293 = CARTESIAN_POINT ( 'NONE',  ( 4.198949119135569656E-17, -1.320799999999990870, 4.000000000000000000 ) ) ;
#106294 = CARTESIAN_POINT ( 'NONE',  ( 34.78752705046288440, 0.000000000000000000, -7.949999999999998401 ) ) ;
#106295 = CARTESIAN_POINT ( 'NONE',  ( -7.499999999999942268, -7.912538124160680475, 4.000000000000000000 ) ) ;
#106297 = EDGE_CURVE ( 'NONE', #20788, #8725, #129360, .T. ) ;
#106296 = CONICAL_SURFACE ( 'NONE', #124864, 2.500000000000000444, 0.9599310885968830309 ) ;
#106298 = AXIS2_PLACEMENT_3D ( 'NONE', #13085, #23247, #25395 ) ;
#106299 = VECTOR ( 'NONE', #63398, 999.9999999999998863 ) ;
#106300 =( BOUNDED_CURVE ( )  B_SPLINE_CURVE ( 3, ( #68204, #112379, #2882, #48544 ),
 .UNSPECIFIED., .F., .F. ) 
 B_SPLINE_CURVE_WITH_KNOTS ( ( 4, 4 ),
 ( 1.901594255663624056, 1.933014472006547413 ),
 .UNSPECIFIED. ) 
 CURVE ( )  GEOMETRIC_REPRESENTATION_ITEM ( )  RATIONAL_B_SPLINE_CURVE ( ( 1.000000000000000000, 0.9999177325257868620, 0.9999177325257868620, 1.000000000000000000 ) ) 
 REPRESENTATION_ITEM ( '' )  );
#106301 = ORIENTED_EDGE ( 'NONE', *, *, #98039, .T. ) ;
#106302 = ORIENTED_EDGE ( 'NONE', *, *, #59709, .F. ) ;
#106303 = CIRCLE ( 'NONE', #76235, 5.968999999999998529 ) ;
#106304 = CARTESIAN_POINT ( 'NONE',  ( -74.99451991528749772, 28.92564299267990435, 4.000000000000000000 ) ) ;
#106305 = FACE_OUTER_BOUND ( 'NONE', #65241, .T. ) ;
#106306 = CARTESIAN_POINT ( 'NONE',  ( 9.183988606268997046, 28.73617430169793607, 5.000000000000000000 ) ) ;
#106307 = CARTESIAN_POINT ( 'NONE',  ( 24.39999999999999858, 1.399999999999986366, 20.40202195861970580 ) ) ;
#106308 = EDGE_CURVE ( 'NONE', #10836, #34731, #8963, .T. ) ;
#106309 = AXIS2_PLACEMENT_3D ( 'NONE', #131786, #119441, #75276 ) ;
#106310 = CARTESIAN_POINT ( 'NONE',  ( 28.49999999999979750, -14.56887692260765732, 4.000000000000000000 ) ) ;
#106311 = LINE ( 'NONE', #6988, #122945 ) ;
#106312 = ORIENTED_EDGE ( 'NONE', *, *, #61249, .T. ) ;
#106313 = ORIENTED_EDGE ( 'NONE', *, *, #99334, .T. ) ;
#106314 = VERTEX_POINT ( 'NONE', #30798 ) ;
#106315 = ORIENTED_EDGE ( 'NONE', *, *, #47476, .F. ) ;
#106316 = EDGE_CURVE ( 'NONE', #123911, #26035, #141692, .T. ) ;
#106317 = VECTOR ( 'NONE', #10337, 1000.000000000000000 ) ;
#106318 = AXIS2_PLACEMENT_3D ( 'NONE', #108333, #98227, #119236 ) ;
#106319 = PRESENTATION_STYLE_ASSIGNMENT (( #4849 ) ) ;
#106320 = EDGE_CURVE ( 'NONE', #105140, #68985, #68683, .T. ) ;
#106321 = ADVANCED_FACE ( 'NONE', ( #88014 ), #87305, .F. ) ;
#106322 = VECTOR ( 'NONE', #130751, 1000.000000000000227 ) ;
#106323 = CARTESIAN_POINT ( 'NONE',  ( -34.49999999999975131, -20.56887692260760758, 4.000000000000000000 ) ) ;
#106324 = VERTEX_POINT ( 'NONE', #35086 ) ;
#106325 = PLANE ( 'NONE',  #108462 ) ;
#106326 = CARTESIAN_POINT ( 'NONE',  ( 5.700255128608413102, -27.71228299555201957, 4.000000000000000000 ) ) ;
#106327 = FACE_OUTER_BOUND ( 'NONE', #11257, .T. ) ;
#106328 = LINE ( 'NONE', #28094, #80899 ) ;
#106329 = VECTOR ( 'NONE', #41593, 1000.000000000000000 ) ;
#106330 = CARTESIAN_POINT ( 'NONE',  ( 19.73159235450332005, 2.500000000000001776, 0.000000000000000000 ) ) ;
#106331 = ORIENTED_EDGE ( 'NONE', *, *, #131495, .T. ) ;
#106333 = EDGE_CURVE ( 'NONE', #33900, #50012, #123528, .T. ) ;
#106332 = VECTOR ( 'NONE', #126263, 1000.000000000000227 ) ;
#106334 = DIRECTION ( 'NONE',  ( -0.000000000000000000, 0.3543493200069153248, 0.9351131265310292928 ) ) ;
#106335 = CARTESIAN_POINT ( 'NONE',  ( -75.18398860626899705, 28.73617430169839793, 5.000000000000000000 ) ) ;
#106336 = VECTOR ( 'NONE', #41008, 1000.000000000000000 ) ;
#106337 = ORIENTED_EDGE ( 'NONE', *, *, #52904, .F. ) ;
#106338 = PLANE ( 'NONE',  #50485 ) ;
#106339 = VERTEX_POINT ( 'NONE', #111920 ) ;
#106340 = ADVANCED_FACE ( 'NONE', ( #23460 ), #35809, .F. ) ;
#106341 = CARTESIAN_POINT ( 'NONE',  ( 9.489213562373095101, -27.52281430457062328, 5.000000000000000000 ) ) ;
#106342 = ORIENTED_EDGE ( 'NONE', *, *, #68660, .T. ) ;
#106344 = VECTOR ( 'NONE', #106815, 1000.000000000000000 ) ;
#106343 = CARTESIAN_POINT ( 'NONE',  ( 77.14626352523143282, -4.472830434245840259, 4.472830434245838482 ) ) ;
#106345 = ORIENTED_EDGE ( 'NONE', *, *, #66744, .T. ) ;
#106346 = VECTOR ( 'NONE', #108863, 1000.000000000000000 ) ;
#106347 = CARTESIAN_POINT ( 'NONE',  ( -31.99806943317879515, -22.22500000000000142, 4.500000000000000888 ) ) ;
#106348 = CARTESIAN_POINT ( 'NONE',  ( 110.6879301918981184, 6.110000000000002984, -1.637169565754156730 ) ) ;
#106349 = DIRECTION ( 'NONE',  ( -0.000000000000000000, -1.000000000000000000, -0.000000000000000000 ) ) ;
#106350 = ADVANCED_FACE ( 'NONE', ( #11123 ), #135122, .F. ) ;
#106351 = CARTESIAN_POINT ( 'NONE',  ( 45.18398860626900415, 28.73617430169818832, 5.000000000000000000 ) ) ;
#106352 = VECTOR ( 'NONE', #24953, 1000.000000000000000 ) ;
#106353 = CARTESIAN_POINT ( 'NONE',  ( 20.36747333860806819, 3.821174125832445049E-16, 0.000000000000000000 ) ) ;
#106354 = ADVANCED_FACE ( 'NONE', ( #89433 ), #113312, .T. ) ;
#106355 = CARTESIAN_POINT ( 'NONE',  ( 28.49999999999980460, 0.05218569542916537407, 5.000000000000000000 ) ) ;
#106356 = DIRECTION ( 'NONE',  ( -0.000000000000000000, 0.3543493200069153248, 0.9351131265310291818 ) ) ;
#106357 = VERTEX_POINT ( 'NONE', #57550 ) ;
#106358 = DIRECTION ( 'NONE',  ( -0.000000000000000000, 0.000000000000000000, 1.000000000000000000 ) ) ;
#106359 = VERTEX_POINT ( 'NONE', #46711 ) ;
#106360 = ORIENTED_EDGE ( 'NONE', *, *, #66392, .T. ) ;
#106361 = DIRECTION ( 'NONE',  ( -0.7071067811865486830, -0.7071067811865464625, 0.000000000000000000 ) ) ;
#106362 = ORIENTED_EDGE ( 'NONE', *, *, #103262, .F. ) ;
#106363 = PLANE ( 'NONE',  #125627 ) ;
#106364 = DIRECTION ( 'NONE',  ( -0.7071067811865487940, 0.7071067811865463515, -0.000000000000000000 ) ) ;
#106365 = LINE ( 'NONE', #60068, #81095 ) ;
#106366 = DIRECTION ( 'NONE',  ( -0.3543493200069162685, -0.000000000000000000, -0.9351131265310288487 ) ) ;
#106367 = ORIENTED_EDGE ( 'NONE', *, *, #81329, .F. ) ;
#106368 = CARTESIAN_POINT ( 'NONE',  ( 2.999999998679837354, -47.86718710719786429, 37.19897551713999917 ) ) ;
#106369 = VERTEX_POINT ( 'NONE', #101739 ) ;
#106370 = EDGE_CURVE ( 'NONE', #28133, #61121, #133667, .T. ) ;
#106371 = CARTESIAN_POINT ( 'NONE',  ( 5.082903141435219041, 3.967499999999992699, -6.871911579029513994 ) ) ;
#106372 = CARTESIAN_POINT ( 'NONE',  ( 34.49999999999976552, -14.94567065516889848, 4.994342998332158778 ) ) ;
#106373 = CARTESIAN_POINT ( 'NONE',  ( 13.82816939922344091, 12.75929247661558641, 4.000000000000000000 ) ) ;
#106374 = LINE ( 'NONE', #62220, #69723 ) ;
#106375 = ORIENTED_EDGE ( 'NONE', *, *, #131252, .T. ) ;
#106376 = ORIENTED_EDGE ( 'NONE', *, *, #82858, .T. ) ;
#106377 = VERTEX_POINT ( 'NONE', #47418 ) ;
#106378 = CARTESIAN_POINT ( 'NONE',  ( -12.51665438641036410, 22.22500000000000142, 4.500000000000000888 ) ) ;
#106379 =( NAMED_UNIT ( * ) SI_UNIT ( $, .STERADIAN. ) SOLID_ANGLE_UNIT ( ) );
#106380 = DIRECTION ( 'NONE',  ( 0.7071067811865487940, 0.7071067811865463515, 0.000000000000000000 ) ) ;
#106381 = CARTESIAN_POINT ( 'NONE',  ( 181.1500000000000057, 0.000000000000000000, -31.92499999999998295 ) ) ;
#106382 = CYLINDRICAL_SURFACE ( 'NONE', #131610, 2.500000000000000000 ) ;
#106383 = DIRECTION ( 'NONE',  ( 0.7071067811865487940, 0.7071067811865463515, 0.000000000000000000 ) ) ;
#106384 = DIRECTION ( 'NONE',  ( 0.6830127018922181881, 0.6830127018922202975, -0.2588190451025214056 ) ) ;
#106385 = CARTESIAN_POINT ( 'NONE',  ( -22.11017322888195125, -22.22500000000000142, 4.785647885939353863 ) ) ;
#106386 = FILL_AREA_STYLE ('',( #108530 ) ) ;
#106387 = EDGE_LOOP ( 'NONE', ( #116890, #97841 ) ) ;
#106388 = LINE ( 'NONE', #138356, #30184 ) ;
#106389 = VECTOR ( 'NONE', #71250, 1000.000000000000000 ) ;
#106390 = VECTOR ( 'NONE', #13120, 1000.000000000000000 ) ;
#106391 = VECTOR ( 'NONE', #112831, 1000.000000000000227 ) ;
#106392 = AXIS2_PLACEMENT_3D ( 'NONE', #120556, #111116, #74981 ) ;
#106393 = DIRECTION ( 'NONE',  ( -0.6830127018922181881, 0.6830127018922202975, -0.2588190451025214056 ) ) ;
#106394 = ORIENTED_EDGE ( 'NONE', *, *, #124080, .F. ) ;
#106395 = AXIS2_PLACEMENT_3D ( 'NONE', #55404, #75722, #9722 ) ;
#106396 = CARTESIAN_POINT ( 'NONE',  ( -31.82816939922330945, -11.24070752338416490, 4.000000000000000000 ) ) ;
#106398 = EDGE_LOOP ( 'NONE', ( #135706, #93714, #89643, #131228 ) ) ;
#106397 = PLANE ( 'NONE',  #55745 ) ;
#106399 = CARTESIAN_POINT ( 'NONE',  ( -13.49999999999990763, 8.900465351122141655, -2.516491619111481892 ) ) ;
#106400 = DIRECTION ( 'NONE',  ( -0.3543493200069162685, -0.000000000000000000, -0.9351131265310288487 ) ) ;
#106401 = ORIENTED_EDGE ( 'NONE', *, *, #143155, .T. ) ;
#106402 = AXIS2_PLACEMENT_3D ( 'NONE', #95568, #92707, #39801 ) ;
#106403 = ORIENTED_EDGE ( 'NONE', *, *, #84744, .T. ) ;
#106404 = SURFACE_SIDE_STYLE ('',( #117996 ) ) ;
#106405 = CARTESIAN_POINT ( 'NONE',  ( 123.4541937171295700, 6.884901960086283523, 3.975000000000002753 ) ) ;
#106406 = DIRECTION ( 'NONE',  ( 0.7071067811865487940, 0.7071067811865463515, 0.000000000000000000 ) ) ;
#106407 = AXIS2_PLACEMENT_3D ( 'NONE', #108524, #107127, #86111 ) ;
#106408 = CARTESIAN_POINT ( 'NONE',  ( -20.99451991528748707, 28.92564299267952777, 4.000000000000000000 ) ) ;
#106409 = DIRECTION ( 'NONE',  ( -1.000000000000000000, 0.000000000000000000, 0.000000000000000000 ) ) ;
#106410 = PRESENTATION_STYLE_ASSIGNMENT (( #96257 ) ) ;
#106411 = DIRECTION ( 'NONE',  ( 0.7071067811865487940, 0.7071067811865463515, 0.000000000000000000 ) ) ;
#106412 = CARTESIAN_POINT ( 'NONE',  ( 2.041666666666666963, 3.047499999999993214, -5.278424836066146320 ) ) ;
#106414 = AXIS2_PLACEMENT_3D ( 'NONE', #13021, #90617, #55860 ) ;
#106413 = CARTESIAN_POINT ( 'NONE',  ( 6.832903141435220817, -3.967499999999994476, 6.871911579029513106 ) ) ;
#106415 = DIRECTION ( 'NONE',  ( -0.3543493200069162685, -0.000000000000000000, -0.9351131265310288487 ) ) ;
#106416 = VECTOR ( 'NONE', #100134, 1000.000000000000000 ) ;
#106417 = DIRECTION ( 'NONE',  ( 0.6830127018922181881, 0.6830127018922202975, -0.2588190451025214056 ) ) ;
#106418 = CARTESIAN_POINT ( 'NONE',  ( -12.69999999999998153, 0.000000000000000000, 0.000000000000000000 ) ) ;
#106419 = ORIENTED_EDGE ( 'NONE', *, *, #53395, .F. ) ;
#106420 = ORIENTED_EDGE ( 'NONE', *, *, #50412, .T. ) ;
#106421 = CARTESIAN_POINT ( 'NONE',  ( 87.47916666666665719, -7.950000000000001066, 2.130196079827424427 ) ) ;
#106422 = VECTOR ( 'NONE', #40706, 1000.000000000000000 ) ;
#106423 = CARTESIAN_POINT ( 'NONE',  ( 3.793339364578457662, 21.75929247661549937, 4.998822639870711626 ) ) ;
#106424 = ORIENTED_EDGE ( 'NONE', *, *, #5463, .F. ) ;
#106425 = CARTESIAN_POINT ( 'NONE',  ( 91.66252705046288440, 7.949999999999998401, 1.460391307983218338E-15 ) ) ;
#106426 = LINE ( 'NONE', #107175, #97312 ) ;
#106427 = CARTESIAN_POINT ( 'NONE',  ( 28.49999999999981171, -20.56887692260760048, 4.000000000000000000 ) ) ;
#106428 = ORIENTED_EDGE ( 'NONE', *, *, #68920, .T. ) ;
#106429 = VECTOR ( 'NONE', #86719, 1000.000000000000000 ) ;
#106430 = LINE ( 'NONE', #28213, #20876 ) ;
#106431 = VECTOR ( 'NONE', #97155, 999.9999999999998863 ) ;
#106432 = CARTESIAN_POINT ( 'NONE',  ( 3.183988606268992161, 28.73617430169789699, 5.000000000000000000 ) ) ;
#106433 = EDGE_CURVE ( 'NONE', #58071, #20334, #33658, .T. ) ;
#106434 = DIRECTION ( 'NONE',  ( -0.9707728879609256456, 0.000000000000000000, -0.2400000000000085398 ) ) ;
#106435 = CARTESIAN_POINT ( 'NONE',  ( 13.49999999999992006, -1.912538124160735542, 4.000000000000000000 ) ) ;
#106436 = EDGE_CURVE ( 'NONE', #59940, #81437, #80727, .T. ) ;
#106437 = EDGE_CURVE ( 'NONE', #43341, #91589, #68440, .T. ) ;
#106438 = AXIS2_PLACEMENT_3D ( 'NONE', #34658, #113622, #25183 ) ;
#106439 = LINE ( 'NONE', #36082, #130515 ) ;
#106440 = PLANE ( 'NONE',  #10387 ) ;
#106441 = LINE ( 'NONE', #94869, #108150 ) ;
#106442 = VECTOR ( 'NONE', #82258, 999.9999999999998863 ) ;
#106443 = LINE ( 'NONE', #116642, #128619 ) ;
#106444 = PLANE ( 'NONE',  #107221 ) ;
#106445 = CARTESIAN_POINT ( 'NONE',  ( 21.66240673564756491, 0.000000000000000000, 0.000000000000000000 ) ) ;
#106446 = CARTESIAN_POINT ( 'NONE',  ( -36.48921356237310221, -27.52281430457080802, 5.000000000000000000 ) ) ;
#106447 = DIRECTION ( 'NONE',  ( 0.7071067811865487940, -0.7071067811865463515, 0.000000000000000000 ) ) ;
#106448 = EDGE_CURVE ( 'NONE', #143191, #117668, #25592, .T. ) ;
#106449 = ADVANCED_FACE ( 'NONE', ( #100326 ), #2392, .F. ) ;
#106450 = EDGE_LOOP ( 'NONE', ( #37769, #42604, #123473, #112318 ) ) ;
#106451 = VERTEX_POINT ( 'NONE', #78573 ) ;
#106452 = CARTESIAN_POINT ( 'NONE',  ( 104.1254301918981184, 5.291415217122919401, 3.055000000000002824 ) ) ;
#106453 = ORIENTED_EDGE ( 'NONE', *, *, #129559, .F. ) ;
#106454 = EDGE_CURVE ( 'NONE', #129291, #112641, #63999, .T. ) ;
#106455 =( NAMED_UNIT ( * ) SI_UNIT ( $, .STERADIAN. ) SOLID_ANGLE_UNIT ( ) );
#106456 = CIRCLE ( 'NONE', #115761, 2.500000000000000888 ) ;
#106457 = DIRECTION ( 'NONE',  ( 0.7071067811865487940, 0.7071067811865463515, 0.000000000000000000 ) ) ;
#106458 = ORIENTED_EDGE ( 'NONE', *, *, #49699, .F. ) ;
#106459 = LINE ( 'NONE', #7140, #113933 ) ;
#106460 = FACE_OUTER_BOUND ( 'NONE', #68844, .T. ) ;
#106461 = ADVANCED_FACE ( 'NONE', ( #67727 ), #122044, .F. ) ;
#106462 = CARTESIAN_POINT ( 'NONE',  ( 93.97459685856478018, 1.637169565754164058, -6.109999999999996767 ) ) ;
#106463 = VERTEX_POINT ( 'NONE', #1668 ) ;
#106464 = CARTESIAN_POINT ( 'NONE',  ( 5.999999999999967137, -16.06887692260765377, 4.000000000000000000 ) ) ;
#106465 = EDGE_LOOP ( 'NONE', ( #14488, #122574, #102510, #28678 ) ) ;
#106466 = DIRECTION ( 'NONE',  ( 0.000000000000000000, -1.000000000000000000, 0.000000000000000000 ) ) ;
#106467 = DIRECTION ( 'NONE',  ( 0.6830127018922181881, 0.6830127018922202975, -0.2588190451025214056 ) ) ;
#106468 = AXIS2_PLACEMENT_3D ( 'NONE', #70604, #124933, #59025 ) ;
#106469 = DIRECTION ( 'NONE',  ( 0.3543493200069162685, -0.000000000000000000, -0.9351131265310288487 ) ) ;
#106470 = VERTEX_POINT ( 'NONE', #36487 ) ;
#106471 = VERTEX_POINT ( 'NONE', #22711 ) ;
#106472 = EDGE_LOOP ( 'NONE', ( #127428, #107813, #26321, #3145, #80289 ) ) ;
#106473 = CARTESIAN_POINT ( 'NONE',  ( -14.99999999999989519, 15.45873954670183537, -0.03131636524290794948 ) ) ;
#106474 = CARTESIAN_POINT ( 'NONE',  ( 5.999999999999967137, 7.588810512006220144, -3.013526669885240761 ) ) ;
#106475 = CARTESIAN_POINT ( 'NONE',  ( 13.19206980810188412, -7.934999999999990727, -2.126176841940955242 ) ) ;
#106476 = EDGE_CURVE ( 'NONE', #129269, #135619, #9317, .T. ) ;
#106477 = AXIS2_PLACEMENT_3D ( 'NONE', #44812, #55649, #122291 ) ;
#106478 = CLOSED_SHELL ( 'NONE', ( #100647, #2929, #21683, #22593, #140206, #95917, #125960, #50394 ) ) ;
#106479 = CYLINDRICAL_SURFACE ( 'NONE', #29448, 2.500000000000000444 ) ;
#106480 =( NAMED_UNIT ( * ) SI_UNIT ( $, .STERADIAN. ) SOLID_ANGLE_UNIT ( ) );
#106481 = ORIENTED_EDGE ( 'NONE', *, *, #13486, .T. ) ;
#106482 = EDGE_LOOP ( 'NONE', ( #128789, #135626, #128193, #87810 ) ) ;
#106483 = DIRECTION ( 'NONE',  ( -1.000000000000000000, -0.000000000000000000, 0.000000000000000000 ) ) ;
#106484 = ORIENTED_EDGE ( 'NONE', *, *, #16296, .T. ) ;
#106485 = EDGE_LOOP ( 'NONE', ( #12754, #31446, #62619, #79599, #15481 ) ) ;
#106486 = ADVANCED_FACE ( 'NONE', ( #111164 ), #17566, .F. ) ;
#106487 = EDGE_CURVE ( 'NONE', #69673, #77789, #38178, .T. ) ;
#106488 = VECTOR ( 'NONE', #91784, 1000.000000000000000 ) ;
#106489 = DIRECTION ( 'NONE',  ( -0.7071067811865486830, -0.7071067811865464625, -0.000000000000000000 ) ) ;
#106490 = LINE ( 'NONE', #60192, #26381 ) ;
#106491 = ORIENTED_EDGE ( 'NONE', *, *, #38277, .F. ) ;
#106492 = CARTESIAN_POINT ( 'NONE',  ( 5.510786437626906675, -27.52281430457051314, 5.000000000000000000 ) ) ;
#106493 = ADVANCED_FACE ( 'NONE', ( #39362 ), #126343, .T. ) ;
#106494 = VECTOR ( 'NONE', #53942, 999.9999999999998863 ) ;
#106495 = DIRECTION ( 'NONE',  ( 1.000000000000000000, -0.000000000000000000, -0.000000000000000000 ) ) ;
#106496 = FACE_OUTER_BOUND ( 'NONE', #38140, .T. ) ;
#106497 = VECTOR ( 'NONE', #123574, 1000.000000000000000 ) ;
#106498 = AXIS2_PLACEMENT_3D ( 'NONE', #61708, #85556, #84860 ) ;
#106499 = CONICAL_SURFACE ( 'NONE', #2295, 2.500000000000000444, 0.9599310885968830309 ) ;
#106500 = EDGE_CURVE ( 'NONE', #69962, #68424, #93009, .T. ) ;
#106501 = DIRECTION ( 'NONE',  ( -1.000000000000000000, 0.000000000000000000, -0.000000000000000000 ) ) ;
#106502 = VERTEX_POINT ( 'NONE', #15405 ) ;
#106503 = EDGE_CURVE ( 'NONE', #73610, #109637, #127797, .T. ) ;
#106504 = VECTOR ( 'NONE', #4150, 1000.000000000000227 ) ;
#106505 = CARTESIAN_POINT ( 'NONE',  ( -12.00548008471251293, 28.92564299267929684, 4.000000000000000000 ) ) ;
#106506 = DIRECTION ( 'NONE',  ( -1.000000000000000000, 0.000000000000000000, -0.000000000000000000 ) ) ;
#106507 = ORIENTED_EDGE ( 'NONE', *, *, #89673, .T. ) ;
#106508 = DIRECTION ( 'NONE',  ( -0.3543493200069162685, -0.000000000000000000, -0.9351131265310288487 ) ) ;
#106509 = PLANE ( 'NONE',  #133787 ) ;
#106510 = DIRECTION ( 'NONE',  ( -0.7071067811865487940, 0.7071067811865463515, -0.000000000000000000 ) ) ;
#106511 = VERTEX_POINT ( 'NONE', #26332 ) ;
#106512 = CARTESIAN_POINT ( 'NONE',  ( 16.49999999999988276, 10.94296225409028089, -9.576120664313215514 ) ) ;
#106513 = EDGE_LOOP ( 'NONE', ( #77946, #38362, #121519, #28673 ) ) ;
#106514 = VERTEX_POINT ( 'NONE', #71275 ) ;
#106515 = AXIS2_PLACEMENT_3D ( 'NONE', #35180, #78664, #121437 ) ;
#106516 = ADVANCED_FACE ( 'NONE', ( #139403 ), #28482, .F. ) ;
#106517 = VERTEX_POINT ( 'NONE', #70587 ) ;
#106518 = CARTESIAN_POINT ( 'NONE',  ( 32.57876352523145158, -7.482591942790325086E-16, 6.109999999999998543 ) ) ;
#106519 = DIRECTION ( 'NONE',  ( 0.6830127018922180770, -0.6830127018922204085, -0.2588190451025213501 ) ) ;
#106520 = FACE_OUTER_BOUND ( 'NONE', #88121, .T. ) ;
#106521 = FACE_OUTER_BOUND ( 'NONE', #140165, .T. ) ;
#106522 = DIRECTION ( 'NONE',  ( 0.000000000000000000, -1.000000000000000000, 0.000000000000000000 ) ) ;
#106523 = ADVANCED_FACE ( 'NONE', ( #114733 ), #61830, .F. ) ;
#106524 = CARTESIAN_POINT ( 'NONE',  ( -14.99999999999989342, -16.60178936734450161, 0.8616154019347151971 ) ) ;
#106525 = CARTESIAN_POINT ( 'NONE',  ( -24.48921356237309510, -27.52281430457072631, 5.000000000000000000 ) ) ;
#106526 = VECTOR ( 'NONE', #58749, 1000.000000000000114 ) ;
#106527 = DIRECTION ( 'NONE',  ( -0.7071067811865487940, 0.7071067811865463515, -0.000000000000000000 ) ) ;
#106528 = CIRCLE ( 'NONE', #127364, 2.500000000000000888 ) ;
#106529 = CARTESIAN_POINT ( 'NONE',  ( -7.828169399223471103, 6.759292476615647693, 4.000000000000000000 ) ) ;
#106530 = AXIS2_PLACEMENT_3D ( 'NONE', #47245, #24009, #101546 ) ;
#106531 = LINE ( 'NONE', #142763, #64437 ) ;
#106532 = CARTESIAN_POINT ( 'NONE',  ( 12.18398860626900060, 28.73617430169795739, 5.000000000000000000 ) ) ;
#106533 = VERTEX_POINT ( 'NONE', #48090 ) ;
#106534 = VECTOR ( 'NONE', #85959, 1000.000000000000000 ) ;
#106535 = ORIENTED_EDGE ( 'NONE', *, *, #73765, .T. ) ;
#106536 = VERTEX_POINT ( 'NONE', #116186 ) ;
#106537 = EDGE_LOOP ( 'NONE', ( #10767, #92235, #94656, #88079, #65466 ) ) ;
#106538 = CARTESIAN_POINT ( 'NONE',  ( -4.912274722134691121E-20, 1.320799999999990870, 4.000000000000000000 ) ) ;
#106539 = EDGE_LOOP ( 'NONE', ( #72890, #75170, #141525, #116327 ) ) ;
#106540 = VECTOR ( 'NONE', #103226, 999.9999999999998863 ) ;
#106541 = VERTEX_POINT ( 'NONE', #37936 ) ;
#106542 = DIRECTION ( 'NONE',  ( 0.7071067811865487940, -0.7071067811865463515, 0.000000000000000000 ) ) ;
#106543 = DIRECTION ( 'NONE',  ( -0.000000000000000000, -0.3543493200069152693, 0.9351131265310292928 ) ) ;
#106544 = EDGE_CURVE ( 'NONE', #9752, #93361, #78826, .T. ) ;
#106545 = AXIS2_PLACEMENT_3D ( 'NONE', #75088, #77235, #97501 ) ;
#106546 = CARTESIAN_POINT ( 'NONE',  ( -11.99999999999991829, 10.55218569542905982, 5.000000000000000000 ) ) ;
#106547 = VERTEX_POINT ( 'NONE', #61153 ) ;
#106548 = DIRECTION ( 'NONE',  ( -0.6830127018922180770, -0.6830127018922204085, -0.2588190451025213501 ) ) ;
#106549 = ORIENTED_EDGE ( 'NONE', *, *, #61035, .T. ) ;
#106550 = DIRECTION ( 'NONE',  ( -0.7071067811865487940, 0.7071067811865463515, 0.000000000000000000 ) ) ;
#106551 = CARTESIAN_POINT ( 'NONE',  ( 7.139999999999985469, -39.93000000000000682, 18.97874025153853239 ) ) ;
#106552 = AXIS2_PLACEMENT_3D ( 'NONE', #13263, #133654, #23444 ) ;
#106553 = CARTESIAN_POINT ( 'NONE',  ( 13.33790314143522160, -6.871911579029513106, -3.967499999999993587 ) ) ;
#106554 = ORIENTED_EDGE ( 'NONE', *, *, #91991, .T. ) ;
#106555 = CARTESIAN_POINT ( 'NONE',  ( 95.28709685856479439, 3.054999999999997939, 5.291415217122920289 ) ) ;
#106556 = CARTESIAN_POINT ( 'NONE',  ( -30.69326993309580587, -3.740707523384241728, 12.88036043432874678 ) ) ;
#106557 = CARTESIAN_POINT ( 'NONE',  ( -12.20000000000000107, -40.42999999999999261, 19.06900128115122328 ) ) ;
#106558 = ORIENTED_EDGE ( 'NONE', *, *, #114729, .F. ) ;
#106559 = ORIENTED_EDGE ( 'NONE', *, *, #31435, .F. ) ;
#106560 = CARTESIAN_POINT ( 'NONE',  ( 4.658131166821905644, 3.821174125832445049E-16, 0.000000000000000000 ) ) ;
#106561 = VECTOR ( 'NONE', #2872, 1000.000000000000000 ) ;
#106562 = ORIENTED_EDGE ( 'NONE', *, *, #38822, .F. ) ;
#106563 = DIRECTION ( 'NONE',  ( -0.3543493200069163240, 0.000000000000000000, -0.9351131265310288487 ) ) ;
#106564 = CARTESIAN_POINT ( 'NONE',  ( 12.69999999999999574, -60.40159979880236563, 24.51762929923639334 ) ) ;
#106565 = FACE_OUTER_BOUND ( 'NONE', #97971, .T. ) ;
#106566 = DIRECTION ( 'NONE',  ( 0.7071067811865486830, -0.7071067811865464625, -0.000000000000000000 ) ) ;
#106568 = EDGE_CURVE ( 'NONE', #14297, #2772, #105990, .T. ) ;
#106567 = ORIENTED_EDGE ( 'NONE', *, *, #58918, .T. ) ;
#106569 = DIRECTION ( 'NONE',  ( -0.7071067811865486830, -0.7071067811865464625, 0.000000000000000000 ) ) ;
#106570 = EDGE_CURVE ( 'NONE', #33281, #42329, #59687, .T. ) ;
#106571 = DIRECTION ( 'NONE',  ( 0.7071067811865486830, -0.7071067811865464625, -0.000000000000000000 ) ) ;
#106572 = LINE ( 'NONE', #140647, #88516 ) ;
#106573 = ORIENTED_EDGE ( 'NONE', *, *, #95853, .F. ) ;
#106574 = DIRECTION ( 'NONE',  ( -0.7071067811865486830, -0.7071067811865464625, -0.000000000000000000 ) ) ;
#106575 = CARTESIAN_POINT ( 'NONE',  ( 7.637717201596474048, 2.500000000000000888, 0.000000000000000000 ) ) ;
#106576 = ORIENTED_EDGE ( 'NONE', *, *, #79095, .F. ) ;
#106578 = ORIENTED_EDGE ( 'NONE', *, *, #14153, .T. ) ;
#106577 = DIRECTION ( 'NONE',  ( -0.000000000000000000, 0.000000000000000000, 1.000000000000000000 ) ) ;
#106579 = EDGE_CURVE ( 'NONE', #77379, #50386, #104593, .T. ) ;
#106580 = DIRECTION ( 'NONE',  ( 1.000000000000000000, 0.000000000000000000, 0.000000000000000000 ) ) ;
#106581 = CARTESIAN_POINT ( 'NONE',  ( -5.510786437626906675, -27.52281430457051314, 5.000000000000000000 ) ) ;
#106583 = ORIENTED_EDGE ( 'NONE', *, *, #110263, .T. ) ;
#106582 = VECTOR ( 'NONE', #135036, 1000.000000000000000 ) ;
#106584 = CARTESIAN_POINT ( 'NONE',  ( 2.999999999999980016, -6.033600742197678279, 5.000000000000000000 ) ) ;
#106585 = PLANE ( 'NONE',  #137825 ) ;
#106586 = DIRECTION ( 'NONE',  ( -1.000000000000000000, -0.000000000000000000, -0.000000000000000000 ) ) ;
#106587 = CARTESIAN_POINT ( 'NONE',  ( 0.4892135623730947680, -27.52281430457055578, 5.000000000000000000 ) ) ;
#106588 = CARTESIAN_POINT ( 'NONE',  ( 21.48921356237309155, -27.52281430457070499, 5.000000000000000000 ) ) ;
#106589 = LINE ( 'NONE', #75440, #111842 ) ;
#106590 = DIRECTION ( 'NONE',  ( -0.7071067811865486830, -0.7071067811865464625, -0.000000000000000000 ) ) ;
#106591 = CARTESIAN_POINT ( 'NONE',  ( 29.29289321881325137, -0.7407075233842770334, 5.000000000000000000 ) ) ;
#106592 = LINE ( 'NONE', #51558, #90007 ) ;
#106593 = VECTOR ( 'NONE', #142926, 1000.000000000000000 ) ;
#106594 = DIRECTION ( 'NONE',  ( -0.000000000000000000, 0.3543493200069153248, 0.9351131265310292928 ) ) ;
#106595 = LINE ( 'NONE', #94323, #40779 ) ;
#106596 = ORIENTED_EDGE ( 'NONE', *, *, #13497, .F. ) ;
#106597 = ORIENTED_EDGE ( 'NONE', *, *, #74348, .T. ) ;
#106598 = VERTEX_POINT ( 'NONE', #38632 ) ;
#106599 = VECTOR ( 'NONE', #111532, 1000.000000000000000 ) ;
#106600 = CARTESIAN_POINT ( 'NONE',  ( 109.6458333333333286, 2.130196079827431976, -7.949999999999999289 ) ) ;
#106601 = AXIS2_PLACEMENT_3D ( 'NONE', #44507, #45225, #88708 ) ;
#106602 = ORIENTED_EDGE ( 'NONE', *, *, #17022, .T. ) ;
#106603 = VERTEX_POINT ( 'NONE', #82862 ) ;
#106604 = ORIENTED_EDGE ( 'NONE', *, *, #57480, .T. ) ;
#106605 = ADVANCED_FACE ( 'NONE', ( #50231 ), #42929, .F. ) ;
#106606 = DIRECTION ( 'NONE',  ( 0.7071067811865487940, 0.7071067811865463515, -0.000000000000000000 ) ) ;
#106607 = CARTESIAN_POINT ( 'NONE',  ( -12.48921356237309155, -27.52281430457064104, 5.000000000000000000 ) ) ;
#106608 = VECTOR ( 'NONE', #122639, 1000.000000000000000 ) ;
#106609 = VECTOR ( 'NONE', #62080, 1000.000000000000000 ) ;
#106610 = VECTOR ( 'NONE', #30289, 1000.000000000000227 ) ;
#106611 =( GEOMETRIC_REPRESENTATION_CONTEXT ( 3 ) GLOBAL_UNCERTAINTY_ASSIGNED_CONTEXT ( ( #111406 ) ) GLOBAL_UNIT_ASSIGNED_CONTEXT ( ( #8051, #85616, #5190 ) ) REPRESENTATION_CONTEXT ( 'NONE', 'WORKASPACE' ) );
#106612 = VERTEX_POINT ( 'NONE', #64665 ) ;
#106613 = FACE_OUTER_BOUND ( 'NONE', #100602, .T. ) ;
#106614 = AXIS2_PLACEMENT_3D ( 'NONE', #9923, #23662, #98382 ) ;
#106615 = CARTESIAN_POINT ( 'NONE',  ( -33.48921356237309510, -27.52281430457078670, 5.000000000000000000 ) ) ;
#106616 = CARTESIAN_POINT ( 'NONE',  ( -36.18398860626899705, 28.73617430169812437, 5.000000000000000000 ) ) ;
#106617 = CARTESIAN_POINT ( 'NONE',  ( 16.03163515922181404, 2.259292476615694323, 13.77329220150640765 ) ) ;
#106618 = CARTESIAN_POINT ( 'NONE',  ( 99.02126352523144703, -4.472830434245839371, -4.472830434245840259 ) ) ;
#106619 = EDGE_LOOP ( 'NONE', ( #118242, #105312, #60931, #96190 ) ) ;
#106620 = EDGE_CURVE ( 'NONE', #119532, #27906, #54520, .T. ) ;
#106621 = CARTESIAN_POINT ( 'NONE',  ( -15.78802419517198352, 2.637730036045195625, -32.92692751918610128 ) ) ;
#106622 = FACE_OUTER_BOUND ( 'NONE', #114704, .T. ) ;
#106623 = CARTESIAN_POINT ( 'NONE',  ( 0.000000000000000000, 0.000000000000000000, -10.00000000000000000 ) ) ;
#106624 = VECTOR ( 'NONE', #52786, 999.9999999999998863 ) ;
#106625 = LINE ( 'NONE', #105913, #110659 ) ;
#106626 = CARTESIAN_POINT ( 'NONE',  ( -29.99451991528749417, 28.92564299267958816, 4.000000000000000000 ) ) ;
#106627 = DIRECTION ( 'NONE',  ( -0.7071067811865486830, 0.7071067811865464625, 0.000000000000000000 ) ) ;
#106628 = CARTESIAN_POINT ( 'NONE',  ( 30.55836038379621655, -7.949999999999997513, -2.130196079827425759 ) ) ;
#106629 = DIRECTION ( 'NONE',  ( -0.7071067811865486830, -0.7071067811865464625, -0.000000000000000000 ) ) ;
#106630 = EDGE_CURVE ( 'NONE', #34677, #97296, #98701, .T. ) ;
#106631 = ADVANCED_FACE ( 'NONE', ( #20415 ), #43612, .F. ) ;
#106632 = LINE ( 'NONE', #51587, #106422 ) ;
#106633 = VERTEX_POINT ( 'NONE', #107440 ) ;
#106634 = ORIENTED_EDGE ( 'NONE', *, *, #64932, .T. ) ;
#106635 = CARTESIAN_POINT ( 'NONE',  ( 24.77083333333332504, -7.949999999999999289, -2.130196079827426203 ) ) ;
#106636 = EDGE_CURVE ( 'NONE', #81966, #66916, #1556, .T. ) ;
#106637 = VERTEX_POINT ( 'NONE', #21149 ) ;
#106638 = CARTESIAN_POINT ( 'NONE',  ( 34.42499999999998295, 0.000000000000000000, 4.500000000000000888 ) ) ;
#106639 = EDGE_CURVE ( 'NONE', #26708, #126797, #53807, .T. ) ;
#106640 = VECTOR ( 'NONE', #90218, 999.9999999999998863 ) ;
#106641 = DIRECTION ( 'NONE',  ( -1.000000000000000000, -0.000000000000000000, -0.000000000000000000 ) ) ;
#106642 = EDGE_CURVE ( 'NONE', #79922, #137698, #120421, .T. ) ;
#106643 = CARTESIAN_POINT ( 'NONE',  ( -19.05000000000000071, 3.174999999999997158, 5.000000000000000000 ) ) ;
#106644 = LINE ( 'NONE', #105931, #141843 ) ;
#106645 = FILL_AREA_STYLE ('',( #28414 ) ) ;
#106646 = DIRECTION ( 'NONE',  ( 0.7071067811865487940, 0.7071067811865463515, 0.000000000000000000 ) ) ;
#106647 = VECTOR ( 'NONE', #33606, 999.9999999999998863 ) ;
#106648 = EDGE_CURVE ( 'NONE', #93168, #45460, #75546, .T. ) ;
#106649 = VECTOR ( 'NONE', #76381, 1000.000000000000000 ) ;
#106650 = CARTESIAN_POINT ( 'NONE',  ( 127.0787635252314516, -7.482591942790325086E-16, 6.109999999999998543 ) ) ;
#106651 = EDGE_LOOP ( 'NONE', ( #139514, #54348, #56158, #100933 ) ) ;
#106652 = AXIS2_PLACEMENT_3D ( 'NONE', #20335, #99320, #76179 ) ;
#106653 = CARTESIAN_POINT ( 'NONE',  ( 1.499999999999999556, 0.05218569542916363935, 5.000000000000000000 ) ) ;
#106654 = EDGE_LOOP ( 'NONE', ( #22592, #7753, #96303, #112733 ) ) ;
#106655 = LINE ( 'NONE', #83526, #52123 ) ;
#106656 = VECTOR ( 'NONE', #136397, 1000.000000000000000 ) ;
#106657 = FACE_OUTER_BOUND ( 'NONE', #73039, .T. ) ;
#106658 = CARTESIAN_POINT ( 'NONE',  ( 23.63159235450331863, 2.500000000000001332, 0.000000000000000000 ) ) ;
#106659 = EDGE_CURVE ( 'NONE', #94040, #2296, #129184, .T. ) ;
#106660 = DIRECTION ( 'NONE',  ( -0.000000000000000000, 0.000000000000000000, 1.000000000000000000 ) ) ;
#106661 = VERTEX_POINT ( 'NONE', #76261 ) ;
#106662 = CARTESIAN_POINT ( 'NONE',  ( 48.70876352523144703, -7.482591942790329030E-16, 6.110000000000001208 ) ) ;
#106663 = EDGE_CURVE ( 'NONE', #79589, #87542, #95854, .T. ) ;
#106664 = ORIENTED_EDGE ( 'NONE', *, *, #30240, .F. ) ;
#106665 = PLANE ( 'NONE',  #65596 ) ;
#106666 = DIRECTION ( 'NONE',  ( 0.7071067811865486830, -0.7071067811865464625, -0.000000000000000000 ) ) ;
#106667 = DIRECTION ( 'NONE',  ( -1.000000000000000000, -1.224606353822377258E-16, -0.000000000000000000 ) ) ;
#106668 = CARTESIAN_POINT ( 'NONE',  ( 5.671830600776435638, 20.25929247661551003, 4.000000000000000000 ) ) ;
#106669 = ADVANCED_FACE ( 'NONE', ( #31328 ), #106706, .F. ) ;
#106670 = CARTESIAN_POINT ( 'NONE',  ( 38.55793019189810877, 6.110000000000000320, -1.637169565754156064 ) ) ;
#106671 = ORIENTED_EDGE ( 'NONE', *, *, #59774, .F. ) ;
#106672 = CARTESIAN_POINT ( 'NONE',  ( 33.18398860626899705, 28.73617430169810305, 5.000000000000000000 ) ) ;
#106673 = DIRECTION ( 'NONE',  ( -0.7071067811865486830, 0.7071067811865464625, 0.000000000000000000 ) ) ;
#106674 = EDGE_LOOP ( 'NONE', ( #5453, #15150, #30108 ) ) ;
#106675 = ORIENTED_EDGE ( 'NONE', *, *, #120213, .T. ) ;
#106676 = AXIS2_PLACEMENT_3D ( 'NONE', #20878, #109332, #108573 ) ;
#106677 = ORIENTED_EDGE ( 'NONE', *, *, #137864, .F. ) ;
#106678 = DIRECTION ( 'NONE',  ( 0.000000000000000000, 0.000000000000000000, 1.000000000000000000 ) ) ;
#106679 = VERTEX_POINT ( 'NONE', #140100 ) ;
#106680 = CARTESIAN_POINT ( 'NONE',  ( -12.20000000000000284, -39.92999999999999261, 19.06900128115122328 ) ) ;
#106681 = ADVANCED_FACE ( 'NONE', ( #108843 ), #84983, .F. ) ;
#106682 = VECTOR ( 'NONE', #12078, 1000.000000000000000 ) ;
#106683 = CARTESIAN_POINT ( 'NONE',  ( 34.92500000000002558, -22.06289321881344634, -2.893915774544653381E-16 ) ) ;
#106684 = FACE_BOUND ( 'NONE', #97456, .T. ) ;
#106685 = LINE ( 'NONE', #7379, #59578 ) ;
#106686 = CARTESIAN_POINT ( 'NONE',  ( 3.191216777807879712, -48.83231052142029682, 38.98973348322100207 ) ) ;
#106687 = CARTESIAN_POINT ( 'NONE',  ( 66.48921356237309510, -27.52281430457101763, 5.000000000000000000 ) ) ;
#106688 = EDGE_LOOP ( 'NONE', ( #57012, #44189, #86822, #51070 ) ) ;
#106689 = ORIENTED_EDGE ( 'NONE', *, *, #48611, .F. ) ;
#106690 = ORIENTED_EDGE ( 'NONE', *, *, #91204, .T. ) ;
#106691 = AXIS2_PLACEMENT_3D ( 'NONE', #29613, #28923, #62280 ) ;
#106692 = CARTESIAN_POINT ( 'NONE',  ( -24.48921356237309510, -27.52281430457072631, 5.000000000000000000 ) ) ;
#106693 = ADVANCED_FACE ( 'NONE', ( #87130 ), #74115, .F. ) ;
#106694 = ORIENTED_EDGE ( 'NONE', *, *, #5241, .T. ) ;
#106695 = CARTESIAN_POINT ( 'NONE',  ( 54.89126352523145158, -4.472830434245838482, -4.472830434245838482 ) ) ;
#106696 = ORIENTED_EDGE ( 'NONE', *, *, #52250, .T. ) ;
#106697 = PLANE ( 'NONE',  #53377 ) ;
#106698 = CARTESIAN_POINT ( 'NONE',  ( 65.99451991528749772, 28.92564299267984396, 4.000000000000000000 ) ) ;
#106699 = EDGE_CURVE ( 'NONE', #108316, #75865, #85679, .T. ) ;
#106700 = ORIENTED_EDGE ( 'NONE', *, *, #93518, .T. ) ;
#106701 = DIRECTION ( 'NONE',  ( 0.7071067811865486830, -0.7071067811865464625, -0.000000000000000000 ) ) ;
#106702 = VECTOR ( 'NONE', #25445, 1000.000000000000227 ) ;
#106703 =( BOUNDED_CURVE ( )  B_SPLINE_CURVE ( 3, ( #81551, #93820, #125755, #26430 ),
 .UNSPECIFIED., .F., .F. ) 
 B_SPLINE_CURVE_WITH_KNOTS ( ( 4, 4 ),
 ( 3.953918675577642095, 4.014082184732835401 ),
 .UNSPECIFIED. ) 
 CURVE ( )  GEOMETRIC_REPRESENTATION_ITEM ( )  RATIONAL_B_SPLINE_CURVE ( ( 1.000000000000000000, 0.9996983854260930169, 0.9996983854260930169, 1.000000000000000000 ) ) 
 REPRESENTATION_ITEM ( '' )  );
#106704 = AXIS2_PLACEMENT_3D ( 'NONE', #22897, #447, #12752 ) ;
#106705 = CIRCLE ( 'NONE', #44263, 2.500000000000000444 ) ;
#106706 = PLANE ( 'NONE',  #135822 ) ;
#106707 = EDGE_CURVE ( 'NONE', #17447, #99025, #109585, .T. ) ;
#106708 = FACE_OUTER_BOUND ( 'NONE', #16106, .T. ) ;
#106709 = CARTESIAN_POINT ( 'NONE',  ( -17.38161509397993854, -2.240707523384264377, 13.37739548510243459 ) ) ;
#106710 = LINE ( 'NONE', #72745, #26123 ) ;
#106711 = FACE_OUTER_BOUND ( 'NONE', #126428, .T. ) ;
#106712 = EDGE_LOOP ( 'NONE', ( #76069, #137584, #1888, #70380 ) ) ;
#106713 = VECTOR ( 'NONE', #36196, 1000.000000000000000 ) ;
#106714 = AXIS2_PLACEMENT_3D ( 'NONE', #67815, #92347, #89516 ) ;
#106715 = VECTOR ( 'NONE', #74359, 1000.000000000000000 ) ;
#106716 = ORIENTED_EDGE ( 'NONE', *, *, #116968, .T. ) ;
#106717 = AXIS2_PLACEMENT_3D ( 'NONE', #2897, #125412, #136994 ) ;
#106718 = CARTESIAN_POINT ( 'NONE',  ( 19.29580628287044064, -5.278424836066144543, 3.047499999999995879 ) ) ;
#106719 =( BOUNDED_CURVE ( )  B_SPLINE_CURVE ( 3, ( #105057, #131642, #11976, #122156 ),
 .UNSPECIFIED., .F., .F. ) 
 B_SPLINE_CURVE_WITH_KNOTS ( ( 4, 4 ),
 ( 2.779374508378133601, 4.199602562396849592 ),
 .UNSPECIFIED. ) 
 CURVE ( )  GEOMETRIC_REPRESENTATION_ITEM ( )  RATIONAL_B_SPLINE_CURVE ( ( 1.000000000000000000, 0.8388583629366601624, 0.8388583629366601624, 1.000000000000000000 ) ) 
 REPRESENTATION_ITEM ( '' )  );
#106720 = DIRECTION ( 'NONE',  ( -0.7071067811865486830, -0.7071067811865464625, -0.000000000000000000 ) ) ;
#106721 = VERTEX_POINT ( 'NONE', #30625 ) ;
#106722 = AXIS2_PLACEMENT_3D ( 'NONE', #98037, #132105, #142955 ) ;
#106723 = ORIENTED_EDGE ( 'NONE', *, *, #94998, .F. ) ;
#106724 = EDGE_LOOP ( 'NONE', ( #104532, #46475, #75616, #17551 ) ) ;
#106725 = DIRECTION ( 'NONE',  ( -0.7071067811865486830, -0.7071067811865464625, 0.000000000000000000 ) ) ;
#106726 = CARTESIAN_POINT ( 'NONE',  ( 55.35002705046288440, -5.819803920172573086, -5.819803920172573086 ) ) ;
#106727 = EDGE_CURVE ( 'NONE', #55207, #136089, #74855, .T. ) ;
#106728 = CARTESIAN_POINT ( 'NONE',  ( 39.48921356237310221, -27.52281430457082934, 5.000000000000000000 ) ) ;
#106729 = VERTEX_POINT ( 'NONE', #63958 ) ;
#106730 = VECTOR ( 'NONE', #1947, 1000.000000000000000 ) ;
#106731 = LINE ( 'NONE', #52366, #20810 ) ;
#106732 = SURFACE_SIDE_STYLE ('',( #127818 ) ) ;
#106733 = CARTESIAN_POINT ( 'NONE',  ( 15.23373647476855375, 5.808823158059036373, 5.808823158059032821 ) ) ;
#106734 = DIRECTION ( 'NONE',  ( -0.6830127018922180770, -0.6830127018922204085, -0.2588190451025213501 ) ) ;
#106735 = ORIENTED_EDGE ( 'NONE', *, *, #38607, .F. ) ;
#106736 = DIRECTION ( 'NONE',  ( 0.3543493200069162685, -0.000000000000000000, -0.9351131265310288487 ) ) ;
#106737 = CIRCLE ( 'NONE', #99822, 2.055000000000001048 ) ;
#106738 = EDGE_CURVE ( 'NONE', #92199, #22742, #8479, .T. ) ;
#106739 = DIRECTION ( 'NONE',  ( 0.3543493200069162685, -0.000000000000000000, -0.9351131265310288487 ) ) ;
#106740 = VECTOR ( 'NONE', #55473, 999.9999999999998863 ) ;
#106741 = LINE ( 'NONE', #130686, #65843 ) ;
#106743 = ORIENTED_EDGE ( 'NONE', *, *, #135533, .F. ) ;
#106742 = DIRECTION ( 'NONE',  ( -0.6830127018922181881, 0.6830127018922202975, -0.2588190451025214056 ) ) ;
#106744 = DIRECTION ( 'NONE',  ( 1.000000000000000000, 0.000000000000000000, 0.000000000000000000 ) ) ;
#106745 = ORIENTED_EDGE ( 'NONE', *, *, #73311, .F. ) ;
#106746 = CARTESIAN_POINT ( 'NONE',  ( 20.51159235450331764, -2.500000000000000000, 3.061616997868384127E-16 ) ) ;
#106747 = LINE ( 'NONE', #75585, #72525 ) ;
#106748 = ADVANCED_FACE ( 'NONE', ( #45095 ), #134211, .F. ) ;
#106749 = FACE_OUTER_BOUND ( 'NONE', #11891, .T. ) ;
#106751 = EDGE_CURVE ( 'NONE', #62473, #98546, #68275, .T. ) ;
#106750 = ORIENTED_EDGE ( 'NONE', *, *, #6039, .F. ) ;
#106752 = CIRCLE ( 'NONE', #72045, 2.055000000000000604 ) ;
#106753 = CARTESIAN_POINT ( 'NONE',  ( 63.48921356237309510, -27.52281430457099631, 5.000000000000000000 ) ) ;
#106754 = AXIS2_PLACEMENT_3D ( 'NONE', #140549, #107897, #74613 ) ;
#106755 = EDGE_CURVE ( 'NONE', #61841, #126832, #15423, .T. ) ;
#106757 = DIRECTION ( 'NONE',  ( 0.3543493200069162685, -0.000000000000000000, -0.9351131265310288487 ) ) ;
#106756 = VECTOR ( 'NONE', #32579, 1000.000000000000000 ) ;
#106758 = DIRECTION ( 'NONE',  ( -0.3543493200069162685, -0.000000000000000000, -0.9351131265310288487 ) ) ;
#106759 = CARTESIAN_POINT ( 'NONE',  ( -34.42500000000001137, 20.97718569542920264, 5.000000000000000000 ) ) ;
#106760 = EDGE_LOOP ( 'NONE', ( #44608, #106902, #42290, #85115, #5321 ) ) ;
#106761 = DIRECTION ( 'NONE',  ( -0.7071067811865486830, 0.7071067811865464625, 0.000000000000000000 ) ) ;
#106762 = AXIS2_PLACEMENT_3D ( 'NONE', #100219, #88639, #133566 ) ;
#106763 = CARTESIAN_POINT ( 'NONE',  ( 63.48921356237309510, -27.52281430457099631, 5.000000000000000000 ) ) ;
#106764 = CARTESIAN_POINT ( 'NONE',  ( 0.7070132642930391231, -21.74070752338405654, 4.999753212805213565 ) ) ;
#106765 = DIRECTION ( 'NONE',  ( 1.000000000000000000, 1.224606353822377258E-16, 0.000000000000000000 ) ) ;
#106766 = LINE ( 'NONE', #64714, #9073 ) ;
#106767 = VERTEX_POINT ( 'NONE', #2213 ) ;
#106768 = VECTOR ( 'NONE', #82062, 1000.000000000000000 ) ;
#106769 = EDGE_CURVE ( 'NONE', #29345, #103464, #84907, .T. ) ;
#106770 = ORIENTED_EDGE ( 'NONE', *, *, #92911, .F. ) ;
#106771 = DIRECTION ( 'NONE',  ( -0.6830127018922181881, 0.6830127018922202975, -0.2588190451025214056 ) ) ;
#106772 = LINE ( 'NONE', #130713, #87632 ) ;
#106773 = CARTESIAN_POINT ( 'NONE',  ( 15.87456980810188867, 6.871911579029510442, -3.967499999999998916 ) ) ;
#106774 = CARTESIAN_POINT ( 'NONE',  ( -2.999999999999975575, -21.41253812416053748, 4.000000000000000000 ) ) ;
#106775 = AXIS2_PLACEMENT_3D ( 'NONE', #34983, #142314, #77763 ) ;
#106776 = CARTESIAN_POINT ( 'NONE',  ( -34.92500000000001137, -11.99387692260794047, 4.000000000000000000 ) ) ;
#106777 = DIRECTION ( 'NONE',  ( -0.6830127018922181881, 0.6830127018922202975, -0.2588190451025214056 ) ) ;
#106778 = VERTEX_POINT ( 'NONE', #57376 ) ;
#106779 = CARTESIAN_POINT ( 'NONE',  ( -30.48921356237309510, -27.52281430457076894, 5.000000000000000000 ) ) ;
#106780 = DIRECTION ( 'NONE',  ( -0.3543493200069162685, -0.000000000000000000, -0.9351131265310288487 ) ) ;
#106781 = VECTOR ( 'NONE', #64601, 1000.000000000000000 ) ;
#106782 = CARTESIAN_POINT ( 'NONE',  ( 5.879139616203772789, -5.278424836066145431, -3.047499999999993658 ) ) ;
#106783 = VECTOR ( 'NONE', #133210, 1000.000000000000000 ) ;
#106784 = PLANE ( 'NONE',  #76081 ) ;
#106785 = CARTESIAN_POINT ( 'NONE',  ( 39.72459685856478018, -1.637169565754161171, 6.109999999999998543 ) ) ;
#106786 = CARTESIAN_POINT ( 'NONE',  ( -20.99451991528748707, 28.92564299267952777, 4.000000000000000000 ) ) ;
#106787 = ORIENTED_EDGE ( 'NONE', *, *, #118147, .F. ) ;
#106788 = PLANE ( 'NONE',  #11775 ) ;
#106789 = ORIENTED_EDGE ( 'NONE', *, *, #142344, .F. ) ;
#106790 = VECTOR ( 'NONE', #21623, 1000.000000000000000 ) ;
#106791 = ORIENTED_EDGE ( 'NONE', *, *, #4720, .T. ) ;
#106792 = VECTOR ( 'NONE', #131947, 999.9999999999998863 ) ;
#106793 = CARTESIAN_POINT ( 'NONE',  ( 24.39999999999999858, 1.194621026894847171, -17.40906030209848510 ) ) ;
#106794 = CARTESIAN_POINT ( 'NONE',  ( 32.20710678118632586, 0.7592924766157052030, 5.000000000000000000 ) ) ;
#106795 = DIRECTION ( 'NONE',  ( 0.3543493200069162685, -0.000000000000000000, -0.9351131265310288487 ) ) ;
#106796 = LINE ( 'NONE', #17638, #4859 ) ;
#106797 = CARTESIAN_POINT ( 'NONE',  ( 7.408325480989960354, -0.7407075233842770334, 14.76736230305382414 ) ) ;
#106798 = DIRECTION ( 'NONE',  ( -0.7071067811865486830, -0.7071067811865464625, 0.000000000000000000 ) ) ;
#106799 = ORIENTED_EDGE ( 'NONE', *, *, #142550, .T. ) ;
#106800 = CARTESIAN_POINT ( 'NONE',  ( 21.48921356237309155, -27.52281430457070499, 5.000000000000000000 ) ) ;
#106801 = DIRECTION ( 'NONE',  ( -0.7071067811865486830, -0.7071067811865464625, 0.000000000000000000 ) ) ;
#106803 = CONICAL_SURFACE ( 'NONE', #136934, 2.055000000000000604, 0.9599310885968764806 ) ;
#106802 = DIRECTION ( 'NONE',  ( -0.7071067811865486830, -0.7071067811865464625, -0.000000000000000000 ) ) ;
#106804 = DIRECTION ( 'NONE',  ( 0.000000000000000000, 0.000000000000000000, 1.000000000000000000 ) ) ;
#106805 = FACE_OUTER_BOUND ( 'NONE', #94643, .T. ) ;
#106806 = CARTESIAN_POINT ( 'NONE',  ( 103.9125270504628844, -7.949999999999998401, -4.867971026610728450E-16 ) ) ;
#106807 = CARTESIAN_POINT ( 'NONE',  ( 64.39169371712955581, 2.130196079827421762, 7.950000000000001066 ) ) ;
#106808 = EDGE_CURVE ( 'NONE', #80619, #126257, #113136, .T. ) ;
#106809 = CARTESIAN_POINT ( 'NONE',  ( 34.42499999999998295, 13.54139925780190445, 5.000000000000000000 ) ) ;
#106810 = ORIENTED_EDGE ( 'NONE', *, *, #138477, .T. ) ;
#106811 = ORIENTED_EDGE ( 'NONE', *, *, #59265, .F. ) ;
#106812 = CARTESIAN_POINT ( 'NONE',  ( 58.89583333333332149, -2.130196079827427091, 7.949999999999999289 ) ) ;
#106813 = CARTESIAN_POINT ( 'NONE',  ( 0.000000000000000000, 0.000000000000000000, 5.000000000000000000 ) ) ;
#106814 = EDGE_CURVE ( 'NONE', #16172, #44633, #10953, .T. ) ;
#106815 = DIRECTION ( 'NONE',  ( 0.5735764363510444941, 0.8191520442889929088, 0.000000000000000000 ) ) ;
#106816 = ADVANCED_FACE ( 'NONE', ( #76997 ), #32768, .T. ) ;
#106817 = CARTESIAN_POINT ( 'NONE',  ( -8.207106781186480404, 6.759292476615647693, 5.000000000000000000 ) ) ;
#106818 = ORIENTED_EDGE ( 'NONE', *, *, #11382, .T. ) ;
#106819 = VECTOR ( 'NONE', #96927, 1000.000000000000000 ) ;
#106820 = EDGE_CURVE ( 'NONE', #42487, #72813, #88575, .T. ) ;
#106821 = CARTESIAN_POINT ( 'NONE',  ( 4.499999999999976019, 10.46639925780215208, 5.000000000000000000 ) ) ;
#106822 = VECTOR ( 'NONE', #50239, 1000.000000000000000 ) ;
#106823 = VECTOR ( 'NONE', #131506, 999.9999999999998863 ) ;
#106824 = CARTESIAN_POINT ( 'NONE',  ( 45.64626352523142572, -4.472830434245840259, 4.472830434245839371 ) ) ;
#106825 = ORIENTED_EDGE ( 'NONE', *, *, #126637, .T. ) ;
#106826 = CARTESIAN_POINT ( 'NONE',  ( -63.29974487139158867, -27.71228299555250274, 4.000000000000000000 ) ) ;
#106827 = EDGE_LOOP ( 'NONE', ( #3935, #116599, #6339, #14884 ) ) ;
#106829 = VERTEX_POINT ( 'NONE', #13812 ) ;
#106828 = AXIS2_PLACEMENT_3D ( 'NONE', #115669, #26567, #113553 ) ;
#106830 = AXIS2_PLACEMENT_3D ( 'NONE', #90424, #3390, #123793 ) ;
#106831 = VECTOR ( 'NONE', #57096, 1000.000000000000000 ) ;
#106832 =( GEOMETRIC_REPRESENTATION_CONTEXT ( 3 ) GLOBAL_UNCERTAINTY_ASSIGNED_CONTEXT ( ( #1205 ) ) GLOBAL_UNIT_ASSIGNED_CONTEXT ( ( #112057, #101157, #99729 ) ) REPRESENTATION_CONTEXT ( 'NONE', 'WORKASPACE' ) );
#106833 = DIRECTION ( 'NONE',  ( -1.000000000000000000, 0.000000000000000000, 0.000000000000000000 ) ) ;
#106835 = CARTESIAN_POINT ( 'NONE',  ( -0.7928932188134510950, 6.759292476615645917, 5.000000000000000000 ) ) ;
#106834 = AXIS2_PLACEMENT_3D ( 'NONE', #87692, #121027, #31187 ) ;
#106836 = CARTESIAN_POINT ( 'NONE',  ( 0.000000000000000000, 9.735942053221458872E-16, -7.950000000000000178 ) ) ;
#106837 = EDGE_CURVE ( 'NONE', #59938, #237, #121924, .T. ) ;
#106838 = DIRECTION ( 'NONE',  ( -0.5735764363510499342, -0.8191520442889891340, 0.000000000000000000 ) ) ;
#106840 = ADVANCED_FACE ( 'NONE', ( #101552 ), #47252, .T. ) ;
#106839 = PLANE ( 'NONE',  #107706 ) ;
#106841 = FACE_OUTER_BOUND ( 'NONE', #62631, .T. ) ;
#106843 = VERTEX_POINT ( 'NONE', #1506 ) ;
#106842 = CARTESIAN_POINT ( 'NONE',  ( -17.99999999999986855, -16.44781430457066662, 5.000000000000000000 ) ) ;
#106844 = CARTESIAN_POINT ( 'NONE',  ( 25.39999999999999858, 0.000000000000000000, 6.094999999999989093 ) ) ;
#106845 = CARTESIAN_POINT ( 'NONE',  ( -5.999999999999963585, 14.58746187583910903, 4.000000000000000000 ) ) ;
#106846 = CARTESIAN_POINT ( 'NONE',  ( 1.516262732464673579, -0.4000000000000004108, 2.467792535850613866 ) ) ;
#106847 = CARTESIAN_POINT ( 'NONE',  ( 13.49999999999991473, 8.319652575858402344, -8.582050562765800805 ) ) ;
#106848 = ADVANCED_FACE ( 'NONE', ( #66109 ), #110988, .F. ) ;
#106849 = ORIENTED_EDGE ( 'NONE', *, *, #32387, .T. ) ;
#106850 = ORIENTED_EDGE ( 'NONE', *, *, #121383, .F. ) ;
#106851 = AXIS2_PLACEMENT_3D ( 'NONE', #75713, #53979, #109753 ) ;
#106852 = CARTESIAN_POINT ( 'NONE',  ( 88.60002705046289861, 5.819803920172570422, 5.819803920172575751 ) ) ;
#106853 = CARTESIAN_POINT ( 'NONE',  ( 76.76626352523142316, 4.472830434245839371, -4.472830434245838482 ) ) ;
#106854 = DIRECTION ( 'NONE',  ( 0.000000000000000000, -1.000000000000000000, 0.000000000000000000 ) ) ;
#106855 = LINE ( 'NONE', #117025, #128809 ) ;
#106856 = ORIENTED_EDGE ( 'NONE', *, *, #135884, .T. ) ;
#106858 = EDGE_CURVE ( 'NONE', #129574, #141782, #93553, .T. ) ;
#106857 = EDGE_LOOP ( 'NONE', ( #55757, #33083, #39219, #64061 ) ) ;
#106859 = CARTESIAN_POINT ( 'NONE',  ( 30.70701326429282929, -21.74070752338406365, 4.999753212805224223 ) ) ;
#106860 = ORIENTED_EDGE ( 'NONE', *, *, #80290, .F. ) ;
#106861 = EDGE_LOOP ( 'NONE', ( #139054, #104270, #64261, #53498 ) ) ;
#106862 = VECTOR ( 'NONE', #57698, 1000.000000000000227 ) ;
#106863 = LINE ( 'NONE', #129331, #30522 ) ;
#106864 = ORIENTED_EDGE ( 'NONE', *, *, #1926, .F. ) ;
#106865 = AXIS2_PLACEMENT_3D ( 'NONE', #142258, #29184, #41481 ) ;
#106866 = CARTESIAN_POINT ( 'NONE',  ( 0.2261952378971223976, 0.5999999999999987566, 3.877637771780739318 ) ) ;
#106867 = EDGE_CURVE ( 'NONE', #129881, #117528, #80553, .T. ) ;
#106868 = STYLED_ITEM ( 'NONE', ( #98442 ), #61305 ) ;
#106869 = DIRECTION ( 'NONE',  ( 0.000000000000000000, -1.000000000000000000, 0.000000000000000000 ) ) ;
#106870 = FACE_BOUND ( 'NONE', #49730, .T. ) ;
#106871 = DIRECTION ( 'NONE',  ( -0.7071067811865487940, 0.7071067811865463515, -0.000000000000000000 ) ) ;
#106872 = APPLICATION_CONTEXT ( 'automotive_design' ) ;
#106873 = DIRECTION ( 'NONE',  ( -1.000000000000000000, -0.000000000000000000, -0.000000000000000000 ) ) ;
#106874 = DIRECTION ( 'NONE',  ( 0.3543493200069162685, -0.000000000000000000, -0.9351131265310288487 ) ) ;
#106876 = ORIENTED_EDGE ( 'NONE', *, *, #10890, .T. ) ;
#106875 = DIRECTION ( 'NONE',  ( 0.000000000000000000, -0.2631995976047557528, -0.9647414015272147703 ) ) ;
#106877 = AXIS2_PLACEMENT_3D ( 'NONE', #98865, #45955, #1666 ) ;
#106878 =( NAMED_UNIT ( * ) SI_UNIT ( $, .STERADIAN. ) SOLID_ANGLE_UNIT ( ) );
#106880 = ADVANCED_FACE ( 'NONE', ( #39173 ), #82683, .T. ) ;
#106879 = APPLICATION_PROTOCOL_DEFINITION ( 'draft international standard', 'automotive_design', 1998, #38308 ) ;
#106881 = VERTEX_POINT ( 'NONE', #5070 ) ;
#106882 = VERTEX_POINT ( 'NONE', #59519 ) ;
#106883 = CARTESIAN_POINT ( 'NONE',  ( 89.16209685856478018, -5.291415217122919401, 3.054999999999997939 ) ) ;
#106884 = ORIENTED_EDGE ( 'NONE', *, *, #8740, .F. ) ;
#106885 = DIRECTION ( 'NONE',  ( 0.000000000000000000, -1.000000000000000000, 0.000000000000000000 ) ) ;
#106886 = LINE ( 'NONE', #138831, #44293 ) ;
#106887 = EDGE_CURVE ( 'NONE', #23670, #46353, #17403, .T. ) ;
#106888 = AXIS2_PLACEMENT_3D ( 'NONE', #15187, #47879, #102241 ) ;
#106889 = FACE_OUTER_BOUND ( 'NONE', #110354, .T. ) ;
#106890 = VECTOR ( 'NONE', #74918, 1000.000000000000227 ) ;
#106891 = FACE_OUTER_BOUND ( 'NONE', #110309, .T. ) ;
#106892 = CARTESIAN_POINT ( 'NONE',  ( 34.49999999999975842, -11.94567065516892512, 4.994342998332160555 ) ) ;
#106893 = FACE_OUTER_BOUND ( 'NONE', #2857, .T. ) ;
#106894 = ADVANCED_FACE ( 'NONE', ( #61660 ), #25415, .F. ) ;
#106895 = CARTESIAN_POINT ( 'NONE',  ( 12.19999999999999574, -22.33999999999998565, 3.000000000000000000 ) ) ;
#106896 = CONICAL_SURFACE ( 'NONE', #116116, 2.055000000000000604, 0.9599310885968764806 ) ;
#106897 = CARTESIAN_POINT ( 'NONE',  ( -20.99999999999985789, -10.06887692260770883, 4.000000000000000000 ) ) ;
#106898 = FACE_OUTER_BOUND ( 'NONE', #142898, .T. ) ;
#106899 = PLANE ( 'NONE',  #101783 ) ;
#106900 = AXIS2_PLACEMENT_3D ( 'NONE', #60454, #104631, #5297 ) ;
#106901 = CARTESIAN_POINT ( 'NONE',  ( 34.92500000000002558, -21.76999999999999247, 0.000000000000000000 ) ) ;
#106902 = ORIENTED_EDGE ( 'NONE', *, *, #103996, .F. ) ;
#106903 = CARTESIAN_POINT ( 'NONE',  ( 10.49999999999991829, 22.22500000000000142, 4.362957392718799454 ) ) ;
#106904 = DIRECTION ( 'NONE',  ( 0.8571673007021110013, 0.000000000000000000, 0.5150380749100563760 ) ) ;
#106905 = ORIENTED_EDGE ( 'NONE', *, *, #27801, .T. ) ;
#106906 = ORIENTED_EDGE ( 'NONE', *, *, #43213, .F. ) ;
#106907 = ADVANCED_FACE ( 'NONE', ( #92102 ), #28305, .F. ) ;
#106908 = ORIENTED_EDGE ( 'NONE', *, *, #39718, .F. ) ;
#106909 = CARTESIAN_POINT ( 'NONE',  ( 31.64626352523143638, -4.472830434245840259, 4.472830434245838482 ) ) ;
#106910 = VECTOR ( 'NONE', #67438, 1000.000000000000227 ) ;
#106911 = VERTEX_POINT ( 'NONE', #69689 ) ;
#106912 = CARTESIAN_POINT ( 'NONE',  ( 21.29159235450332233, -2.500000000000000000, 3.061616997868384127E-16 ) ) ;
#106913 =( BOUNDED_CURVE ( )  B_SPLINE_CURVE ( 3, ( #87768, #88500, #10880, #90640 ),
 .UNSPECIFIED., .F., .T. ) 
 B_SPLINE_CURVE_WITH_KNOTS ( ( 4, 4 ),
 ( 2.001653308786165208, 3.503810798801449522 ),
 .UNSPECIFIED. ) 
 CURVE ( )  GEOMETRIC_REPRESENTATION_ITEM ( )  RATIONAL_B_SPLINE_CURVE ( ( 1.000000000000000000, 0.8206354192515235013, 0.8206354192515235013, 1.000000000000000000 ) ) 
 REPRESENTATION_ITEM ( '' )  );
#106914 = CARTESIAN_POINT ( 'NONE',  ( 16.37913961620377279, -5.278424836066145431, -3.047499999999993658 ) ) ;
#106915 = CARTESIAN_POINT ( 'NONE',  ( 11.57112785411878519, 8.234238653253980189, -30.09936050942188857 ) ) ;
#106916 = VERTEX_POINT ( 'NONE', #14559 ) ;
#106917 = ADVANCED_FACE ( 'NONE', ( #136328 ), #27551, .F. ) ;
#106918 = CARTESIAN_POINT ( 'NONE',  ( -0.3301021854726499116, 17.25929247661554555, 19.83885114516071368 ) ) ;
#106919 = VERTEX_POINT ( 'NONE', #125475 ) ;
#106920 = CARTESIAN_POINT ( 'NONE',  ( 34.92499999999998295, -13.48753812416038933, 4.000000000000000000 ) ) ;
#106921 = FACE_OUTER_BOUND ( 'NONE', #52550, .T. ) ;
#106922 = VECTOR ( 'NONE', #126397, 1000.000000000000227 ) ;
#106923 = PRESENTATION_LAYER_ASSIGNMENT (  '', '', ( #65265 ) ) ;
#106925 = VERTEX_POINT ( 'NONE', #48622 ) ;
#106924 = DIRECTION ( 'NONE',  ( 0.6830127018922181881, 0.6830127018922202975, -0.2588190451025214056 ) ) ;
#106926 = ORIENTED_EDGE ( 'NONE', *, *, #86039, .F. ) ;
#106927 = FACE_OUTER_BOUND ( 'NONE', #112462, .T. ) ;
#106928 = AXIS2_PLACEMENT_3D ( 'NONE', #128168, #81093, #72390 ) ;
#106930 = ORIENTED_EDGE ( 'NONE', *, *, #108652, .T. ) ;
#106929 = CIRCLE ( 'NONE', #14433, 2.500000000000000888 ) ;
#106931 = DIRECTION ( 'NONE',  ( 0.7071067811865487940, -0.7071067811865463515, 0.000000000000000000 ) ) ;
#106932 = VERTEX_POINT ( 'NONE', #92824 ) ;
#106934 = VERTEX_POINT ( 'NONE', #15935 ) ;
#106933 = EDGE_CURVE ( 'NONE', #91285, #17335, #72565, .T. ) ;
#106935 = ORIENTED_EDGE ( 'NONE', *, *, #104869, .T. ) ;
#106936 = VERTEX_POINT ( 'NONE', #135635 ) ;
#106937 = DIRECTION ( 'NONE',  ( 1.000000000000000000, 3.115803279706882722E-16, 0.000000000000000000 ) ) ;
#106938 = VECTOR ( 'NONE', #77278, 1000.000000000000000 ) ;
#106939 = AXIS2_PLACEMENT_3D ( 'NONE', #67073, #23554, #65689 ) ;
#106940 = CARTESIAN_POINT ( 'NONE',  ( -12.20000000000000284, -40.42999999999999261, -39.50000000000000000 ) ) ;
#106941 = LINE ( 'NONE', #115106, #72326 ) ;
#106943 = ADVANCED_FACE ( 'NONE', ( #104408 ), #49366, .F. ) ;
#106942 = CARTESIAN_POINT ( 'NONE',  ( -36.29974487139159578, -27.71228299555231445, 4.000000000000000000 ) ) ;
#106944 = CARTESIAN_POINT ( 'NONE',  ( -34.92500000000001137, 15.75929247661555088, 4.255531930566231580 ) ) ;
#106945 = ORIENTED_EDGE ( 'NONE', *, *, #104878, .T. ) ;
#106946 = ADVANCED_FACE ( 'NONE', ( #84135 ), #86256, .F. ) ;
#106947 = CARTESIAN_POINT ( 'NONE',  ( -1.499999999999987566, -20.53675388469230612, 2.352720554255888885 ) ) ;
#106948 = ORIENTED_EDGE ( 'NONE', *, *, #55659, .T. ) ;
#106949 = CARTESIAN_POINT ( 'NONE',  ( 0.2997448713915885632, -27.71228299555206220, 4.000000000000000000 ) ) ;
#106950 = CARTESIAN_POINT ( 'NONE',  ( 33.95790314143522437, 6.871911579029515771, 3.967499999999989146 ) ) ;
#106951 = DIRECTION ( 'NONE',  ( -0.7071067811865486830, -0.7071067811865464625, -0.000000000000000000 ) ) ;
#106952 = VERTEX_POINT ( 'NONE', #96363 ) ;
#106953 = CARTESIAN_POINT ( 'NONE',  ( -15.48921356237309510, -27.52281430457066236, 5.000000000000000000 ) ) ;
#106954 = ORIENTED_EDGE ( 'NONE', *, *, #102603, .F. ) ;
#106955 = ORIENTED_EDGE ( 'NONE', *, *, #5857, .F. ) ;
#106956 = VERTEX_POINT ( 'NONE', #30438 ) ;
#106957 = DIRECTION ( 'NONE',  ( -0.7071067811865486830, -0.7071067811865464625, 0.000000000000000000 ) ) ;
#106958 = CARTESIAN_POINT ( 'NONE',  ( 16.49999999999988631, -13.91253812416061564, 4.000000000000000000 ) ) ;
#106959 = CARTESIAN_POINT ( 'NONE',  ( -32.99451991528749062, 28.92564299267960948, 4.000000000000000000 ) ) ;
#106960 = DIRECTION ( 'NONE',  ( -0.7071067811865486830, -0.7071067811865464625, 0.000000000000000000 ) ) ;
#106961 = CARTESIAN_POINT ( 'NONE',  ( 75.74543019189810877, -5.291415217122919401, -3.055000000000000604 ) ) ;
#106962 = EDGE_CURVE ( 'NONE', #139225, #88478, #20967, .T. ) ;
#106963 = VECTOR ( 'NONE', #25775, 1000.000000000000000 ) ;
#106964 = DIRECTION ( 'NONE',  ( 0.7071067811865487940, 0.7071067811865463515, -0.000000000000000000 ) ) ;
#106965 = PRESENTATION_LAYER_ASSIGNMENT (  '', '', ( #51425 ) ) ;
#106966 = FACE_OUTER_BOUND ( 'NONE', #87453, .T. ) ;
#106967 = LINE ( 'NONE', #87379, #120524 ) ;
#106968 = CARTESIAN_POINT ( 'NONE',  ( 65.75000000000000000, -9.735942053221458872E-16, 7.950000000000000178 ) ) ;
#106969 = VECTOR ( 'NONE', #102323, 1000.000000000000227 ) ;
#106970 = ORIENTED_EDGE ( 'NONE', *, *, #130439, .F. ) ;
#106971 = CARTESIAN_POINT ( 'NONE',  ( 0.000000000000000000, 0.000000000000000000, 5.000000000000000000 ) ) ;
#106972 = ORIENTED_EDGE ( 'NONE', *, *, #47766, .T. ) ;
#106973 = PLANE ( 'NONE',  #81782 ) ;
#106975 = AXIS2_PLACEMENT_3D ( 'NONE', #116820, #105232, #69793 ) ;
#106974 = FACE_OUTER_BOUND ( 'NONE', #44056, .T. ) ;
#106976 = VERTEX_POINT ( 'NONE', #97831 ) ;
#106977 = CARTESIAN_POINT ( 'NONE',  ( 34.92499999999998295, -10.48753812416042308, 4.000000000000000000 ) ) ;
#106978 = ORIENTED_EDGE ( 'NONE', *, *, #73615, .F. ) ;
#106979 = CARTESIAN_POINT ( 'NONE',  ( -19.05000000000000071, 3.174999999999997158, 1.444000000000000394 ) ) ;
#106980 = LINE ( 'NONE', #75111, #88918 ) ;
#106981 = ORIENTED_EDGE ( 'NONE', *, *, #116, .T. ) ;
#106982 = EDGE_LOOP ( 'NONE', ( #100623, #125208, #107869, #24301 ) ) ;
#106983 = CARTESIAN_POINT ( 'NONE',  ( 20.99999999999985079, 18.08204922493375122, 0.9627537363044395002 ) ) ;
#106985 = EDGE_CURVE ( 'NONE', #83429, #1085, #94952, .T. ) ;
#106984 = CARTESIAN_POINT ( 'NONE',  ( 54.29974487139159578, -27.71228299555243879, 4.000000000000000000 ) ) ;
#106986 = VECTOR ( 'NONE', #135632, 999.9999999999998863 ) ;
#106987 = CYLINDRICAL_SURFACE ( 'NONE', #12884, 2.500000000000000444 ) ;
#106988 = CARTESIAN_POINT ( 'NONE',  ( 98.37086038379622721, 6.884901960086289741, -3.974999999999993427 ) ) ;
#106989 = CARTESIAN_POINT ( 'NONE',  ( 50.99451991528749062, 28.92564299267973738, 4.000000000000000000 ) ) ;
#106990 = ADVANCED_FACE ( 'NONE', ( #52868 ), #119547, .F. ) ;
#106991 = DIRECTION ( 'NONE',  ( -0.000000000000000000, -1.000000000000000000, -0.000000000000000000 ) ) ;
#106992 = ORIENTED_EDGE ( 'NONE', *, *, #19840, .F. ) ;
#106993 = CARTESIAN_POINT ( 'NONE',  ( 5.380000000000000782, -2.055000000000000160, 2.789133085058098087E-16 ) ) ;
#106994 = EDGE_CURVE ( 'NONE', #44425, #122337, #8625, .T. ) ;
#106995 = DIRECTION ( 'NONE',  ( 0.000000000000000000, 0.000000000000000000, -1.000000000000000000 ) ) ;
#106997 = AXIS2_PLACEMENT_3D ( 'NONE', #26631, #78899, #68051 ) ;
#106996 = CARTESIAN_POINT ( 'NONE',  ( -2.163471288734491349, 15.75929247661555976, 9.299976744542915341 ) ) ;
#106999 = AXIS2_PLACEMENT_3D ( 'NONE', #139100, #41189, #20858 ) ;
#106998 = LINE ( 'NONE', #32125, #113917 ) ;
#107000 = ORIENTED_EDGE ( 'NONE', *, *, #24287, .F. ) ;
#107001 = EDGE_CURVE ( 'NONE', #36869, #87685, #73938, .T. ) ;
#107002 = EDGE_CURVE ( 'NONE', #53796, #114615, #108659, .T. ) ;
#107003 = CARTESIAN_POINT ( 'NONE',  ( -32.99999999999976552, 7.552185695429097123, 5.000000000000000000 ) ) ;
#107004 = ORIENTED_EDGE ( 'NONE', *, *, #38073, .F. ) ;
#107005 = CARTESIAN_POINT ( 'NONE',  ( 83.56293019189811844, 1.637169565754157174, 6.110000000000002984 ) ) ;
#107006 = CARTESIAN_POINT ( 'NONE',  ( -34.92500000000001137, 22.22500000000000142, 4.000000000000000000 ) ) ;
#107008 = AXIS2_PLACEMENT_3D ( 'NONE', #83441, #36365, #80594 ) ;
#107007 = LINE ( 'NONE', #107717, #49339 ) ;
#107009 = ORIENTED_EDGE ( 'NONE', *, *, #58413, .T. ) ;
#107010 = DIRECTION ( 'NONE',  ( 0.7071067811865486830, -0.7071067811865464625, -0.000000000000000000 ) ) ;
#107011 = FACE_OUTER_BOUND ( 'NONE', #88247, .T. ) ;
#107012 = EDGE_CURVE ( 'NONE', #54435, #124219, #50760, .T. ) ;
#107013 = CARTESIAN_POINT ( 'NONE',  ( 2.700255128608413990, -27.71228299555204089, 4.000000000000000000 ) ) ;
#107014 = EDGE_CURVE ( 'NONE', #104818, #26316, #85499, .T. ) ;
#107016 = EDGE_LOOP ( 'NONE', ( #20889, #112741, #75129, #27752 ) ) ;
#107015 = LINE ( 'NONE', #140364, #38252 ) ;
#107017 = DIRECTION ( 'NONE',  ( -0.7071067811865486830, -0.7071067811865464625, 0.000000000000000000 ) ) ;
#107018 = CARTESIAN_POINT ( 'NONE',  ( -23.99999999999982947, -3.485240976185095096, -4.108735105802453269 ) ) ;
#107019 = VECTOR ( 'NONE', #57472, 1000.000000000000000 ) ;
#107020 = DIRECTION ( 'NONE',  ( 0.6830127018922180770, -0.6830127018922204085, -0.2588190451025213501 ) ) ;
#107021 = DIRECTION ( 'NONE',  ( -1.000000000000000000, -1.224606353822377258E-16, -0.000000000000000000 ) ) ;
#107022 = ORIENTED_EDGE ( 'NONE', *, *, #28457, .F. ) ;
#107023 = EDGE_LOOP ( 'NONE', ( #23053, #76645, #74353, #119168 ) ) ;
#107024 = CARTESIAN_POINT ( 'NONE',  ( 75.54209685856477563, 5.291415217122923842, -3.054999999999996163 ) ) ;
#107025 = ORIENTED_EDGE ( 'NONE', *, *, #137151, .T. ) ;
#107026 = EDGE_CURVE ( 'NONE', #132815, #114242, #130479, .T. ) ;
#107027 = DIRECTION ( 'NONE',  ( -0.7071067811865486830, 0.7071067811865464625, 0.000000000000000000 ) ) ;
#107028 = CYLINDRICAL_SURFACE ( 'NONE', #47970, 2.500000000000000444 ) ;
#107029 = CARTESIAN_POINT ( 'NONE',  ( 7.499999999999947597, -12.66682484999665625, -0.6294897503863775556 ) ) ;
#107030 = CARTESIAN_POINT ( 'NONE',  ( 20.51078643762690490, -27.52281430457041012, 5.000000000000000000 ) ) ;
#107031 = EDGE_LOOP ( 'NONE', ( #37592, #11285, #57785, #83762 ) ) ;
#107033 = EDGE_CURVE ( 'NONE', #34652, #142342, #142074, .T. ) ;
#107032 = VECTOR ( 'NONE', #120481, 1000.000000000000000 ) ;
#107034 =( GEOMETRIC_REPRESENTATION_CONTEXT ( 3 ) GLOBAL_UNCERTAINTY_ASSIGNED_CONTEXT ( ( #12803 ) ) GLOBAL_UNIT_ASSIGNED_CONTEXT ( ( #9369, #100001, #76847 ) ) REPRESENTATION_CONTEXT ( 'NONE', 'WORKASPACE' ) );
#107035 = VECTOR ( 'NONE', #102960, 1000.000000000000000 ) ;
#107036 = CARTESIAN_POINT ( 'NONE',  ( 184.1499999999998067, -57.14999999999999147, -34.92499999999972715 ) ) ;
#107037 = LINE ( 'NONE', #71575, #113879 ) ;
#107038 = VECTOR ( 'NONE', #19914, 1000.000000000000000 ) ;
#107039 = VECTOR ( 'NONE', #128317, 999.9999999999998863 ) ;
#107040 = VERTEX_POINT ( 'NONE', #31863 ) ;
#107041 = CARTESIAN_POINT ( 'NONE',  ( 0.08796123503190976523, -1.320799999999990648, 4.000000000000000000 ) ) ;
#107043 = DIRECTION ( 'NONE',  ( 0.7071067811865486830, -0.7071067811865464625, -0.000000000000000000 ) ) ;
#107042 = AXIS2_PLACEMENT_3D ( 'NONE', #116833, #48738, #16810 ) ;
#107044 = EDGE_CURVE ( 'NONE', #46544, #123966, #93639, .T. ) ;
#107045 = CARTESIAN_POINT ( 'NONE',  ( 19.69064382391260892, -2.759520746520534473, 4.000000000000000000 ) ) ;
#107046 = PRESENTATION_LAYER_ASSIGNMENT (  '', '', ( #2831 ) ) ;
#107047 = STYLED_ITEM ( 'NONE', ( #116680 ), #74116 ) ;
#107048 = VERTEX_POINT ( 'NONE', #106529 ) ;
#107049 = ORIENTED_EDGE ( 'NONE', *, *, #22386, .T. ) ;
#107050 = DIRECTION ( 'NONE',  ( 0.7071067811865487940, 0.7071067811865463515, 0.000000000000000000 ) ) ;
#107051 = CARTESIAN_POINT ( 'NONE',  ( -50.99451991528749062, 28.92564299267973738, 4.000000000000000000 ) ) ;
#107052 = PLANE ( 'NONE',  #108665 ) ;
#107053 = EDGE_CURVE ( 'NONE', #8350, #126973, #7213, .T. ) ;
#107054 = CARTESIAN_POINT ( 'NONE',  ( 5.700255128608413102, -27.71228299555201957, 4.000000000000000000 ) ) ;
#107055 = CARTESIAN_POINT ( 'NONE',  ( -17.99999999999986855, -6.412538124160685804, 4.000000000000000000 ) ) ;
#107056 = EDGE_CURVE ( 'NONE', #55424, #89048, #129734, .T. ) ;
#107057 = CARTESIAN_POINT ( 'NONE',  ( 53.89169371712955581, 2.130196079827421762, 7.950000000000000178 ) ) ;
#107058 = FACE_OUTER_BOUND ( 'NONE', #62803, .T. ) ;
#107060 = EDGE_CURVE ( 'NONE', #9707, #64319, #51486, .T. ) ;
#107059 = SURFACE_STYLE_USAGE ( .BOTH. , #16454 ) ;
#107061 = EDGE_LOOP ( 'NONE', ( #42784, #8735, #126623, #45273 ) ) ;
#107062 = ORIENTED_EDGE ( 'NONE', *, *, #27769, .F. ) ;
#107063 = ORIENTED_EDGE ( 'NONE', *, *, #96349, .F. ) ;
#107064 = ORIENTED_EDGE ( 'NONE', *, *, #62243, .F. ) ;
#107065 = AXIS2_PLACEMENT_3D ( 'NONE', #64853, #63449, #88021 ) ;
#107066 = CARTESIAN_POINT ( 'NONE',  ( -17.99999999999987210, 10.93112307739206912, 4.000000000000000000 ) ) ;
#107067 = CARTESIAN_POINT ( 'NONE',  ( -0.000000000000000000, -22.33999999999998565, 3.000000000000000000 ) ) ;
#107068 = ORIENTED_EDGE ( 'NONE', *, *, #90040, .F. ) ;
#107069 = CARTESIAN_POINT ( 'NONE',  ( 19.49999999999986500, 15.43112307739202826, 4.000000000000000000 ) ) ;
#107070 = CARTESIAN_POINT ( 'NONE',  ( 42.29974487139158157, -27.71228299555235708, 4.000000000000000000 ) ) ;
#107071 = AXIS2_PLACEMENT_3D ( 'NONE', #106940, #105501, #83063 ) ;
#107072 = CARTESIAN_POINT ( 'NONE',  ( 4.001930566820951718, -22.22500000000000142, 4.500000000000000888 ) ) ;
#107073 = DIRECTION ( 'NONE',  ( -1.000000000000000000, 0.000000000000000000, 0.000000000000000000 ) ) ;
#107074 = VECTOR ( 'NONE', #66736, 1000.000000000000000 ) ;
#107075 = CARTESIAN_POINT ( 'NONE',  ( -22.63753812416082667, 22.22500000000000142, 4.000000000000000000 ) ) ;
#107076 = EDGE_LOOP ( 'NONE', ( #19711, #122864, #58227, #29775 ) ) ;
#107077 = CARTESIAN_POINT ( 'NONE',  ( -78.18398860626899705, 28.73617430169841924, 5.000000000000000000 ) ) ;
#107078 = PLANE ( 'NONE',  #74367 ) ;
#107079 = ORIENTED_EDGE ( 'NONE', *, *, #31495, .F. ) ;
#107080 = FACE_OUTER_BOUND ( 'NONE', #58851, .T. ) ;
#107081 = ORIENTED_EDGE ( 'NONE', *, *, #75753, .T. ) ;
#107082 = DIRECTION ( 'NONE',  ( -0.7071067811865487940, 0.7071067811865463515, 0.000000000000000000 ) ) ;
#107083 = ORIENTED_EDGE ( 'NONE', *, *, #32906, .T. ) ;
#107084 = CARTESIAN_POINT ( 'NONE',  ( 64.60459685856477563, 1.637169565754164946, -6.109999999999999432 ) ) ;
#107085 = EDGE_LOOP ( 'NONE', ( #110166, #15130, #11475, #31696 ) ) ;
#107086 = ORIENTED_EDGE ( 'NONE', *, *, #123480, .T. ) ;
#107087 = DIRECTION ( 'NONE',  ( 0.000000000000000000, -1.000000000000000000, 0.000000000000000000 ) ) ;
#107088 = CARTESIAN_POINT ( 'NONE',  ( -23.99999999999984013, -8.151047557385094677, -8.977947279169748995 ) ) ;
#107089 = CARTESIAN_POINT ( 'NONE',  ( 111.2712635252314470, 4.472830434245838482, 4.472830434245842035 ) ) ;
#107090 = CARTESIAN_POINT ( 'NONE',  ( -48.48921356237309510, -27.52281430457089328, 5.000000000000000000 ) ) ;
#107092 = DIRECTION ( 'NONE',  ( -0.000000000000000000, 0.000000000000000000, 1.000000000000000000 ) ) ;
#107091 = VECTOR ( 'NONE', #109182, 1000.000000000000227 ) ;
#107093 = CARTESIAN_POINT ( 'NONE',  ( 30.29974487139158867, -27.71228299555227537, 4.000000000000000000 ) ) ;
#107094 = LINE ( 'NONE', #127420, #110075 ) ;
#107095 = VECTOR ( 'NONE', #102733, 1000.000000000000000 ) ;
#107096 = DIRECTION ( 'NONE',  ( -0.7071067811865486830, 0.7071067811865464625, 0.000000000000000000 ) ) ;
#107097 = DIRECTION ( 'NONE',  ( -0.7071067811865486830, -0.7071067811865464625, -0.000000000000000000 ) ) ;
#107098 = DIRECTION ( 'NONE',  ( 0.6830127018922181881, 0.6830127018922202975, -0.2588190451025214056 ) ) ;
#107099 = EDGE_LOOP ( 'NONE', ( #128266, #35939, #81258, #49742 ) ) ;
#107100 = CARTESIAN_POINT ( 'NONE',  ( -7.499999999999944045, 16.18958161055402201, -11.56426086740813197 ) ) ;
#107101 = ORIENTED_EDGE ( 'NONE', *, *, #132469, .F. ) ;
#107102 = ORIENTED_EDGE ( 'NONE', *, *, #137481, .F. ) ;
#107103 = ORIENTED_EDGE ( 'NONE', *, *, #8639, .F. ) ;
#107105 = ORIENTED_EDGE ( 'NONE', *, *, #99790, .F. ) ;
#107104 = VECTOR ( 'NONE', #140391, 1000.000000000000000 ) ;
#107106 = LINE ( 'NONE', #31009, #35197 ) ;
#107107 = CARTESIAN_POINT ( 'NONE',  ( -23.99999999999982592, -9.033600742197648970, 5.000000000000000000 ) ) ;
#107108 = ADVANCED_FACE ( 'NONE', ( #63095 ), #131170, .F. ) ;
#107109 = DIRECTION ( 'NONE',  ( 0.000000000000000000, 0.000000000000000000, 1.000000000000000000 ) ) ;
#107110 = ORIENTED_EDGE ( 'NONE', *, *, #95656, .T. ) ;
#107111 = ADVANCED_FACE ( 'NONE', ( #140605 ), #10097, .F. ) ;
#107112 = AXIS2_PLACEMENT_3D ( 'NONE', #1435, #81926, #102231 ) ;
#107113 = ORIENTED_EDGE ( 'NONE', *, *, #113061, .F. ) ;
#107114 = CARTESIAN_POINT ( 'NONE',  ( 8.145403141435220817, -2.126176841940958351, -7.934999999999989839 ) ) ;
#107115 = DIRECTION ( 'NONE',  ( -0.7071067811865486830, -0.7071067811865464625, 0.000000000000000000 ) ) ;
#107116 = CARTESIAN_POINT ( 'NONE',  ( 26.20710678118635784, -17.24070752338410628, 5.000000000000000000 ) ) ;
#107117 = EDGE_CURVE ( 'NONE', #77708, #9606, #54363, .T. ) ;
#107118 = CARTESIAN_POINT ( 'NONE',  ( 34.45011844616453800, 3.002304141593910014, 5.000000000000001776 ) ) ;
#107119 = ORIENTED_EDGE ( 'NONE', *, *, #76077, .F. ) ;
#107120 = ORIENTED_EDGE ( 'NONE', *, *, #51031, .F. ) ;
#107121 = EDGE_LOOP ( 'NONE', ( #50011, #35623, #48668, #1724, #55787 ) ) ;
#107122 = CARTESIAN_POINT ( 'NONE',  ( 27.53159235450332076, 2.500000000000001776, 0.000000000000000000 ) ) ;
#107123 = FACE_OUTER_BOUND ( 'NONE', #71677, .T. ) ;
#107125 = DIRECTION ( 'NONE',  ( -0.7071067811865487940, 0.7071067811865463515, -0.000000000000000000 ) ) ;
#107124 = VECTOR ( 'NONE', #12450, 1000.000000000000114 ) ;
#107126 = CARTESIAN_POINT ( 'NONE',  ( 0.1161069444170889225, -0.4000000000000003553, 2.220360628129160130 ) ) ;
#107127 = DIRECTION ( 'NONE',  ( 0.6830127018922180770, -0.6830127018922204085, -0.2588190451025213501 ) ) ;
#107128 = VECTOR ( 'NONE', #133530, 1000.000000000000227 ) ;
#107129 = CARTESIAN_POINT ( 'NONE',  ( 34.75611968250419181, -13.29434930147582072, 4.955485411084880276 ) ) ;
#107130 = ADVANCED_FACE ( 'NONE', ( #24546 ), #52847, .F. ) ;
#107132 = VECTOR ( 'NONE', #84310, 1000.000000000000000 ) ;
#107131 = DIRECTION ( 'NONE',  ( -0.7071067811865487940, 0.7071067811865463515, 0.000000000000000000 ) ) ;
#107133 = FACE_OUTER_BOUND ( 'NONE', #99247, .T. ) ;
#107134 = CARTESIAN_POINT ( 'NONE',  ( 26.10459685856476852, 1.637169565754164946, -6.109999999999999432 ) ) ;
#107135 = PLANE ( 'NONE',  #125383 ) ;
#107136 = ORIENTED_EDGE ( 'NONE', *, *, #6266, .T. ) ;
#107137 = LINE ( 'NONE', #63675, #46384 ) ;
#107138 = VECTOR ( 'NONE', #67746, 1000.000000000000000 ) ;
#107139 = AXIS2_PLACEMENT_3D ( 'NONE', #22991, #47687, #12146 ) ;
#107140 = EDGE_CURVE ( 'NONE', #140272, #1952, #21698, .T. ) ;
#107141 = LINE ( 'NONE', #83264, #109525 ) ;
#107142 = VERTEX_POINT ( 'NONE', #67364 ) ;
#107143 = PLANE ( 'NONE',  #138682 ) ;
#107145 = ORIENTED_EDGE ( 'NONE', *, *, #3658, .T. ) ;
#107144 = CARTESIAN_POINT ( 'NONE',  ( 52.60764783923752930, -49.05583548141699879, -39.86617647058820069 ) ) ;
#107146 = CARTESIAN_POINT ( 'NONE',  ( 0.000000000000000000, -21.72500000000000142, 4.500000000000000888 ) ) ;
#107147 = PRESENTATION_STYLE_ASSIGNMENT (( #129612 ) ) ;
#107148 = ADVANCED_FACE ( 'NONE', ( #98537 ), #22829, .T. ) ;
#107149 = VERTEX_POINT ( 'NONE', #142762 ) ;
#107150 = CARTESIAN_POINT ( 'NONE',  ( -9.183988606268997046, 28.73617430169793607, 5.000000000000000000 ) ) ;
#107151 = UNCERTAINTY_MEASURE_WITH_UNIT (LENGTH_MEASURE( 1.000000000000000082E-05 ), #51634, 'distance_accuracy_value', 'NONE');
#107152 = ORIENTED_EDGE ( 'NONE', *, *, #130263, .T. ) ;
#107153 = CARTESIAN_POINT ( 'NONE',  ( 93.55836038379622721, -7.949999999999996625, -2.130196079827426203 ) ) ;
#107154 = CARTESIAN_POINT ( 'NONE',  ( 120.1000270504628986, 5.819803920172570422, 5.819803920172574863 ) ) ;
#107155 = CARTESIAN_POINT ( 'NONE',  ( -26.67183060077628909, 14.25929247661557220, 4.000000000000000000 ) ) ;
#107156 = VECTOR ( 'NONE', #70647, 1000.000000000000227 ) ;
#107157 = DIRECTION ( 'NONE',  ( 0.3543493200069162685, -0.000000000000000000, -0.9351131265310288487 ) ) ;
#107158 = CARTESIAN_POINT ( 'NONE',  ( 3.250000000000000000, 4.999999999999997335, -7.627214432543508948 ) ) ;
#107159 = ADVANCED_FACE ( 'NONE', ( #110111 ), #88403, .F. ) ;
#107160 = CYLINDRICAL_SURFACE ( 'NONE', #15892, 2.500000000000000444 ) ;
#107161 = CARTESIAN_POINT ( 'NONE',  ( 2.770833333333333925, 6.094999999999991758, 1.633150327867687102 ) ) ;
#107162 = CARTESIAN_POINT ( 'NONE',  ( 6.687069808101886004, -2.126176841940956130, 7.934999999999990727 ) ) ;
#107163 = DIRECTION ( 'NONE',  ( -0.6830127018922181881, 0.6830127018922202975, -0.2588190451025214056 ) ) ;
#107164 = CYLINDRICAL_SURFACE ( 'NONE', #77930, 2.500000000000000444 ) ;
#107165 = ORIENTED_EDGE ( 'NONE', *, *, #24976, .F. ) ;
#107166 = AXIS2_PLACEMENT_3D ( 'NONE', #22913, #86075, #121537 ) ;
#107168 = ORIENTED_EDGE ( 'NONE', *, *, #107014, .F. ) ;
#107167 = ADVANCED_FACE ( 'NONE', ( #1342 ), #68800, .T. ) ;
#107169 = EDGE_CURVE ( 'NONE', #6884, #2746, #12939, .T. ) ;
#107170 = ORIENTED_EDGE ( 'NONE', *, *, #108072, .F. ) ;
#107171 = PRODUCT_DEFINITION_SHAPE ( 'NONE', 'NONE',  #143567 ) ;
#107172 = VECTOR ( 'NONE', #5998, 999.9999999999998863 ) ;
#107173 = LINE ( 'NONE', #19459, #27135 ) ;
#107174 = LINE ( 'NONE', #57831, #118008 ) ;
#107175 = CARTESIAN_POINT ( 'NONE',  ( 27.65494483745365173, 5.259292476615662792, 12.77922209995900182 ) ) ;
#107176 = CARTESIAN_POINT ( 'NONE',  ( 29.68336038379622366, -2.130196079827426203, 7.949999999999996625 ) ) ;
#107177 = EDGE_LOOP ( 'NONE', ( #88440, #2408, #72202, #71776 ) ) ;
#107178 = EDGE_CURVE ( 'NONE', #57246, #85199, #1909, .T. ) ;
#107179 = CARTESIAN_POINT ( 'NONE',  ( -33.29974487139158867, -27.71228299555229313, 4.000000000000000000 ) ) ;
#107180 = LINE ( 'NONE', #88312, #106624 ) ;
#107181 = LINE ( 'NONE', #8539, #16451 ) ;
#107182 = EDGE_CURVE ( 'NONE', #85826, #84933, #101393, .T. ) ;
#107183 = EDGE_CURVE ( 'NONE', #47923, #123374, #45975, .T. ) ;
#107184 = FILL_AREA_STYLE ('',( #52787 ) ) ;
#107186 = ORIENTED_EDGE ( 'NONE', *, *, #65947, .F. ) ;
#107185 = CARTESIAN_POINT ( 'NONE',  ( -29.20710678118633652, 6.759292476615654799, 5.000000000000000000 ) ) ;
#107187 = CARTESIAN_POINT ( 'NONE',  ( 40.95833333333333570, 3.974999999999997424, 6.884901960086288852 ) ) ;
#107188 = CARTESIAN_POINT ( 'NONE',  ( 19.49999999999986500, 12.43112307739205491, 4.000000000000000000 ) ) ;
#107189 = DIRECTION ( 'NONE',  ( -1.000000000000000000, -1.224606353822377258E-16, -0.000000000000000000 ) ) ;
#107190 = LINE ( 'NONE', #136981, #110380 ) ;
#107191 = CARTESIAN_POINT ( 'NONE',  ( 2.700255128608413990, -27.71228299555204089, 4.000000000000000000 ) ) ;
#107192 = CARTESIAN_POINT ( 'NONE',  ( 58.17012237851905354, -48.09441802426618295, 35.89947574910241457 ) ) ;
#107193 = VECTOR ( 'NONE', #29059, 1000.000000000000227 ) ;
#107194 = ORIENTED_EDGE ( 'NONE', *, *, #103899, .T. ) ;
#107195 = VERTEX_POINT ( 'NONE', #78235 ) ;
#107196 = ORIENTED_EDGE ( 'NONE', *, *, #27761, .T. ) ;
#107197 = CARTESIAN_POINT ( 'NONE',  ( 97.41709685856478984, 3.054999999999998828, 5.291415217122922066 ) ) ;
#107198 = ORIENTED_EDGE ( 'NONE', *, *, #1238, .T. ) ;
#107199 = EDGE_CURVE ( 'NONE', #115184, #4136, #122420, .T. ) ;
#107200 = AXIS2_PLACEMENT_3D ( 'NONE', #48972, #16287, #91736 ) ;
#107201 = CARTESIAN_POINT ( 'NONE',  ( 128.4365526510869699, -51.77943056867388805, 39.18578444878806266 ) ) ;
#107202 = VECTOR ( 'NONE', #43022, 1000.000000000000000 ) ;
#107203 = CARTESIAN_POINT ( 'NONE',  ( -12.32816939922343913, -12.74070752338415602, 4.000000000000000000 ) ) ;
#107204 = ORIENTED_EDGE ( 'NONE', *, *, #90049, .F. ) ;
#107205 = EDGE_CURVE ( 'NONE', #91285, #51446, #49186, .T. ) ;
#107206 = DIRECTION ( 'NONE',  ( -0.6830127018922181881, 0.6830127018922202975, -0.2588190451025214056 ) ) ;
#107207 = CARTESIAN_POINT ( 'NONE',  ( 4.226741607178313487, -11.24070752338416135, 18.24660765846983068 ) ) ;
#107208 = CARTESIAN_POINT ( 'NONE',  ( 92.95376352523145158, -6.109999999999998543, -3.741295971395162543E-16 ) ) ;
#107209 = ORIENTED_EDGE ( 'NONE', *, *, #86853, .T. ) ;
#107210 = DIRECTION ( 'NONE',  ( 0.7071067811865486830, -0.7071067811865464625, -0.000000000000000000 ) ) ;
#107211 = ORIENTED_EDGE ( 'NONE', *, *, #44794, .F. ) ;
#107212 = LINE ( 'NONE', #107898, #61557 ) ;
#107213 = CARTESIAN_POINT ( 'NONE',  ( 22.49999999999984723, 13.46639925780212721, 5.000000000000000000 ) ) ;
#107214 = CARTESIAN_POINT ( 'NONE',  ( 6.005480084712508493, 28.92564299267933947, 4.000000000000000000 ) ) ;
#107215 = ORIENTED_EDGE ( 'NONE', *, *, #128450, .T. ) ;
#107216 = VERTEX_POINT ( 'NONE', #93379 ) ;
#107217 = VERTEX_POINT ( 'NONE', #38293 ) ;
#107218 = CARTESIAN_POINT ( 'NONE',  ( 23.99451991528749062, 28.92564299267954908, 4.000000000000000000 ) ) ;
#107219 = FACE_OUTER_BOUND ( 'NONE', #116102, .T. ) ;
#107220 = CARTESIAN_POINT ( 'NONE',  ( 11.73373647476855197, 5.808823158059035485, 5.808823158059032821 ) ) ;
#107221 = AXIS2_PLACEMENT_3D ( 'NONE', #29618, #94872, #95601 ) ;
#107222 = CARTESIAN_POINT ( 'NONE',  ( -7.140000000000001457, -60.26999999999998892, -8.278119684037250181 ) ) ;
#107223 = EDGE_CURVE ( 'NONE', #43460, #127258, #36847, .T. ) ;
#107225 = EDGE_CURVE ( 'NONE', #38928, #103858, #24200, .T. ) ;
#107224 =( LENGTH_UNIT ( ) NAMED_UNIT ( * ) SI_UNIT ( .MILLI., .METRE. ) );
#107226 = EDGE_LOOP ( 'NONE', ( #131155, #66928, #101102, #34713 ) ) ;
#107227 = ORIENTED_EDGE ( 'NONE', *, *, #22440, .F. ) ;
#107228 = LINE ( 'NONE', #17369, #85033 ) ;
#107229 = ORIENTED_EDGE ( 'NONE', *, *, #139089, .T. ) ;
#107230 = ORIENTED_EDGE ( 'NONE', *, *, #113248, .F. ) ;
#107231 = VECTOR ( 'NONE', #15803, 1000.000000000000227 ) ;
#107232 = VECTOR ( 'NONE', #125478, 999.9999999999998863 ) ;
#107233 = CARTESIAN_POINT ( 'NONE',  ( 18.22916666666666785, -6.094999999999989093, 1.633150327867691542 ) ) ;
#107234 = LINE ( 'NONE', #27524, #130490 ) ;
#107235 = EDGE_LOOP ( 'NONE', ( #86083, #48809, #113737, #74412 ) ) ;
#107236 = CARTESIAN_POINT ( 'NONE',  ( -60.18398860626900415, 28.73617430169829490, 5.000000000000000000 ) ) ;
#107237 = CARTESIAN_POINT ( 'NONE',  ( 14.27159235450332098, 2.500000000000001332, 0.000000000000000000 ) ) ;
#107238 = CARTESIAN_POINT ( 'NONE',  ( -3.084913231937595590, -12.74070752338414891, 18.74364270924353448 ) ) ;
#107239 = AXIS2_PLACEMENT_3D ( 'NONE', #103802, #60362, #72692 ) ;
#107240 = PRESENTATION_LAYER_ASSIGNMENT (  '', '', ( #111821 ) ) ;
#107241 = PLANE ( 'NONE',  #85416 ) ;
#107242 = EDGE_LOOP ( 'NONE', ( #26203, #118202, #142551, #121750 ) ) ;
#107243 = DIRECTION ( 'NONE',  ( -1.000000000000000000, -1.224606353822377258E-16, -0.000000000000000000 ) ) ;
#107244 = CARTESIAN_POINT ( 'NONE',  ( 25.00442415654155681, 3.591886032380943838, 4.000000000000000000 ) ) ;
#107245 = ORIENTED_EDGE ( 'NONE', *, *, #46240, .F. ) ;
#107246 = LINE ( 'NONE', #63773, #15617 ) ;
#107247 = CARTESIAN_POINT ( 'NONE',  ( 19.93618820135885272, -3.269999999999997353, -36.05817462077273916 ) ) ;
#107248 = CARTESIAN_POINT ( 'NONE',  ( 10.83999999999999986, -2.055000000000000160, 2.789133085058098087E-16 ) ) ;
#107249 = ORIENTED_EDGE ( 'NONE', *, *, #42576, .T. ) ;
#107250 = CARTESIAN_POINT ( 'NONE',  ( -33.48921356237309510, -27.52281430457078670, 5.000000000000000000 ) ) ;
#107251 = EDGE_LOOP ( 'NONE', ( #7673, #36632, #52758, #29555 ) ) ;
#107252 = ORIENTED_EDGE ( 'NONE', *, *, #86407, .T. ) ;
#107253 = EDGE_LOOP ( 'NONE', ( #128155, #15160, #38848, #30637 ) ) ;
#107254 = CARTESIAN_POINT ( 'NONE',  ( 29.95376352523145158, -6.109999999999998543, -3.741295971395162543E-16 ) ) ;
#107255 = CIRCLE ( 'NONE', #30821, 5.968999999999998529 ) ;
#107256 = LINE ( 'NONE', #42756, #71530 ) ;
#107257 = DIRECTION ( 'NONE',  ( -0.7071067811865486830, -0.7071067811865464625, 0.000000000000000000 ) ) ;
#107258 = CARTESIAN_POINT ( 'NONE',  ( -7.499999999999947597, 8.900465351122141655, -2.516491619111497435 ) ) ;
#107259 = CARTESIAN_POINT ( 'NONE',  ( 10.22674160717827085, -11.24070752338416845, 18.24660765846984845 ) ) ;
#107260 = EDGE_CURVE ( 'NONE', #35412, #109145, #39000, .T. ) ;
#107261 = DIRECTION ( 'NONE',  ( 0.6830127018922180770, -0.6830127018922204085, -0.2588190451025213501 ) ) ;
#107262 = CARTESIAN_POINT ( 'NONE',  ( -30.33229681110318410, 22.22500000000000142, 6.740346922533748675 ) ) ;
#107264 = LINE ( 'NONE', #128335, #88574 ) ;
#107263 = VECTOR ( 'NONE', #9749, 999.9999999999998863 ) ;
#107265 = CARTESIAN_POINT ( 'NONE',  ( -30.48921356237309510, -27.52281430457076894, 5.000000000000000000 ) ) ;
#107266 = PLANE ( 'NONE',  #89980 ) ;
#107267 = VECTOR ( 'NONE', #32989, 999.9999999999998863 ) ;
#107268 = FACE_OUTER_BOUND ( 'NONE', #19437, .T. ) ;
#107269 = EDGE_LOOP ( 'NONE', ( #116442, #69949, #76136, #135444 ) ) ;
#107270 = VERTEX_POINT ( 'NONE', #82510 ) ;
#107271 = ORIENTED_EDGE ( 'NONE', *, *, #61697, .T. ) ;
#107272 = VERTEX_POINT ( 'NONE', #92641 ) ;
#107273 = DIRECTION ( 'NONE',  ( 0.000000000000000000, 1.000000000000000000, 0.000000000000000000 ) ) ;
#107274 = ORIENTED_EDGE ( 'NONE', *, *, #28561, .T. ) ;
#107275 = VECTOR ( 'NONE', #7616, 1000.000000000000000 ) ;
#107277 = ORIENTED_EDGE ( 'NONE', *, *, #121016, .F. ) ;
#107276 = EDGE_CURVE ( 'NONE', #141475, #134787, #81094, .T. ) ;
#107278 = DIRECTION ( 'NONE',  ( 0.7071067811865487940, 0.7071067811865463515, -0.000000000000000000 ) ) ;
#107279 = EDGE_CURVE ( 'NONE', #23962, #71803, #80389, .T. ) ;
#107280 = ADVANCED_FACE ( 'NONE', ( #125299 ), #61407, .T. ) ;
#107281 = LINE ( 'NONE', #9365, #13783 ) ;
#107282 = ORIENTED_EDGE ( 'NONE', *, *, #111719, .T. ) ;
#107283 = CARTESIAN_POINT ( 'NONE',  ( 0.000000000000000000, -0.5999999999999993117, -4.750000000000000000 ) ) ;
#107284 = ORIENTED_EDGE ( 'NONE', *, *, #141158, .F. ) ;
#107287 = EDGE_CURVE ( 'NONE', #58068, #41011, #15084, .T. ) ;
#107286 = VECTOR ( 'NONE', #96172, 1000.000000000000000 ) ;
#107285 = CARTESIAN_POINT ( 'NONE',  ( -15.72281430457048934, -21.72500000000000497, 5.000000000000000000 ) ) ;
#107288 = ADVANCED_FACE ( 'NONE', ( #2789 ), #115088, .F. ) ;
#107289 = CARTESIAN_POINT ( 'NONE',  ( -11.29298673570688649, -21.74070752338406720, 4.999753212805217117 ) ) ;
#107290 = VECTOR ( 'NONE', #17100, 1000.000000000000000 ) ;
#107291 = CARTESIAN_POINT ( 'NONE',  ( 8.817069808101885897, -2.126176841940956130, 7.934999999999991616 ) ) ;
#107292 = VERTEX_POINT ( 'NONE', #27382 ) ;
#107293 = CARTESIAN_POINT ( 'NONE',  ( 96.74543019189810877, -5.291415217122919401, -3.055000000000000604 ) ) ;
#107294 = LINE ( 'NONE', #36523, #11198 ) ;
#107295 = ADVANCED_FACE ( 'NONE', ( #71642 ), #136165, .T. ) ;
#107296 = DIRECTION ( 'NONE',  ( -0.7071067811865487940, 0.7071067811865463515, -0.000000000000000000 ) ) ;
#107297 = DIRECTION ( 'NONE',  ( -1.000000000000000000, -1.224606353822377258E-16, -0.000000000000000000 ) ) ;
#107298 = ORIENTED_EDGE ( 'NONE', *, *, #118915, .T. ) ;
#107299 = ORIENTED_EDGE ( 'NONE', *, *, #89475, .F. ) ;
#107300 = DIRECTION ( 'NONE',  ( 0.000000000000000000, -1.000000000000000000, 0.000000000000000000 ) ) ;
#107301 = EDGE_LOOP ( 'NONE', ( #91088, #68977, #41445 ) ) ;
#107303 = AXIS2_PLACEMENT_3D ( 'NONE', #296, #123575, #1708 ) ;
#107302 = CARTESIAN_POINT ( 'NONE',  ( 33.48921356237309510, -27.52281430457078670, 5.000000000000000000 ) ) ;
#107304 = DIRECTION ( 'NONE',  ( -0.7071067811865487940, 0.7071067811865463515, -0.000000000000000000 ) ) ;
#107305 = CARTESIAN_POINT ( 'NONE',  ( 36.18398860626899705, 28.73617430169812437, 5.000000000000000000 ) ) ;
#107306 = DIRECTION ( 'NONE',  ( 0.7071067811865487940, 0.7071067811865463515, 0.000000000000000000 ) ) ;
#107307 = ORIENTED_EDGE ( 'NONE', *, *, #41889, .F. ) ;
#107308 = DIRECTION ( 'NONE',  ( 0.6830127018922180770, -0.6830127018922204085, -0.2588190451025213501 ) ) ;
#107309 = ADVANCED_FACE ( 'NONE', ( #69510 ), #113700, .T. ) ;
#107310 = DIRECTION ( 'NONE',  ( -0.7071067811865487940, 0.7071067811865463515, -0.000000000000000000 ) ) ;
#107311 = CARTESIAN_POINT ( 'NONE',  ( 69.78752705046289861, 0.000000000000000000, -7.949999999999998401 ) ) ;
#107312 = ORIENTED_EDGE ( 'NONE', *, *, #59542, .F. ) ;
#107313 = LINE ( 'NONE', #139978, #25774 ) ;
#107314 = VECTOR ( 'NONE', #121381, 1000.000000000000000 ) ;
#107315 = EDGE_CURVE ( 'NONE', #108329, #96831, #114627, .T. ) ;
#107316 = FACE_OUTER_BOUND ( 'NONE', #90499, .T. ) ;
#107317 = ORIENTED_EDGE ( 'NONE', *, *, #17441, .T. ) ;
#107319 = EDGE_LOOP ( 'NONE', ( #126875, #41997, #58412, #53926 ) ) ;
#107318 = LINE ( 'NONE', #118168, #44048 ) ;
#107320 = ORIENTED_EDGE ( 'NONE', *, *, #129937, .F. ) ;
#107321 = CIRCLE ( 'NONE', #44889, 2.500000000000000888 ) ;
#107322 = CARTESIAN_POINT ( 'NONE',  ( 22.25000000000000000, 0.000000000000000000, 0.000000000000000000 ) ) ;
#107323 = DIRECTION ( 'NONE',  ( -0.7071067811865487940, 0.7071067811865463515, -0.000000000000000000 ) ) ;
#107324 = ADVANCED_FACE ( 'NONE', ( #117944 ), #140444, .F. ) ;
#107325 = ORIENTED_EDGE ( 'NONE', *, *, #114159, .F. ) ;
#107326 = LINE ( 'NONE', #119606, #81316 ) ;
#107327 = UNCERTAINTY_MEASURE_WITH_UNIT (LENGTH_MEASURE( 1.000000000000000082E-05 ), #65044, 'distance_accuracy_value', 'NONE');
#107328 = CARTESIAN_POINT ( 'NONE',  ( 0.000000000000000000, 0.000000000000000000, 5.000000000000000000 ) ) ;
#107330 = VECTOR ( 'NONE', #64317, 1000.000000000000227 ) ;
#107329 = CARTESIAN_POINT ( 'NONE',  ( -31.49999999999978684, -20.53675388469233098, 2.352720554255818275 ) ) ;
#107331 = CARTESIAN_POINT ( 'NONE',  ( 5.816011393731002066, 28.73617430169783304, 5.000000000000000000 ) ) ;
#107332 = CARTESIAN_POINT ( 'NONE',  ( 30.89583333333332860, -2.130196079827427091, 7.949999999999998401 ) ) ;
#107333 = CARTESIAN_POINT ( 'NONE',  ( 3.062499999999999556, 4.461849672132300881, 4.461849672132299105 ) ) ;
#107335 = EDGE_CURVE ( 'NONE', #120211, #133905, #121550, .T. ) ;
#107334 = CARTESIAN_POINT ( 'NONE',  ( 48.25000000000000000, -9.735942053221458872E-16, 7.950000000000000178 ) ) ;
#107336 = DIRECTION ( 'NONE',  ( -0.000000000000000000, 0.3543493200069153248, 0.9351131265310292928 ) ) ;
#107337 = CARTESIAN_POINT ( 'NONE',  ( -81.18398860626899705, 28.73617430169844056, 5.000000000000000000 ) ) ;
#107338 = DIRECTION ( 'NONE',  ( 1.000000000000000000, 0.000000000000000000, 0.000000000000000000 ) ) ;
#107339 = FACE_OUTER_BOUND ( 'NONE', #136046, .T. ) ;
#107340 = FACE_OUTER_BOUND ( 'NONE', #126299, .T. ) ;
#107341 = CARTESIAN_POINT ( 'NONE',  ( 30.18398860626900060, 28.73617430169808173, 5.000000000000000000 ) ) ;
#107342 = ORIENTED_EDGE ( 'NONE', *, *, #132747, .F. ) ;
#107343 = VECTOR ( 'NONE', #78240, 1000.000000000000000 ) ;
#107344 = VERTEX_POINT ( 'NONE', #52712 ) ;
#107345 = ORIENTED_EDGE ( 'NONE', *, *, #70258, .F. ) ;
#107346 = EDGE_CURVE ( 'NONE', #29747, #62376, #40451, .T. ) ;
#107347 = CARTESIAN_POINT ( 'NONE',  ( 113.4374999999999716, 5.819803920172573974, -5.819803920172572198 ) ) ;
#107348 = ORIENTED_EDGE ( 'NONE', *, *, #44468, .T. ) ;
#107349 = ORIENTED_EDGE ( 'NONE', *, *, #119565, .F. ) ;
#107350 = EDGE_CURVE ( 'NONE', #29747, #26803, #41861, .T. ) ;
#107351 = EDGE_LOOP ( 'NONE', ( #131022, #55912, #36049, #142238 ) ) ;
#107352 = CARTESIAN_POINT ( 'NONE',  ( 7.326124847093153925, -2.055000000000000160, 2.789133085058097101E-16 ) ) ;
#107353 = PLANE ( 'NONE',  #90209 ) ;
#107354 = EDGE_LOOP ( 'NONE', ( #15264, #18093, #51143, #110969, #5390 ) ) ;
#107355 = CARTESIAN_POINT ( 'NONE',  ( -20.29289321881331176, -15.74070752338412049, 5.000000000000000000 ) ) ;
#107356 = EDGE_CURVE ( 'NONE', #100536, #127633, #7774, .T. ) ;
#107357 = DIRECTION ( 'NONE',  ( -1.000000000000000000, 0.000000000000000000, 0.000000000000000000 ) ) ;
#107358 = LINE ( 'NONE', #8024, #141203 ) ;
#107359 = DIRECTION ( 'NONE',  ( 0.6830127018922181881, 0.6830127018922202975, -0.2588190451025214056 ) ) ;
#107360 = CARTESIAN_POINT ( 'NONE',  ( 103.2504301918981184, 3.055000000000002824, -5.291415217122919401 ) ) ;
#107361 = ORIENTED_EDGE ( 'NONE', *, *, #108905, .F. ) ;
#107362 = CARTESIAN_POINT ( 'NONE',  ( 15.78699708688048631, 2.640433550745856728, -32.92603572637591469 ) ) ;
#107363 = PLANE ( 'NONE',  #139581 ) ;
#107364 = DIRECTION ( 'NONE',  ( -0.000000000000000000, 0.3543493200069153248, 0.9351131265310292928 ) ) ;
#107365 = VECTOR ( 'NONE', #73063, 1000.000000000000227 ) ;
#107366 = DIRECTION ( 'NONE',  ( 0.7071067811865487940, 0.7071067811865463515, 0.000000000000000000 ) ) ;
#107367 = CARTESIAN_POINT ( 'NONE',  ( -30.48921356237309510, -27.52281430457076894, 5.000000000000000000 ) ) ;
#107368 = DIRECTION ( 'NONE',  ( 0.7071067811865487940, 0.7071067811865463515, 0.000000000000000000 ) ) ;
#107369 = CARTESIAN_POINT ( 'NONE',  ( 0.000000000000000000, 0.000000000000000000, 5.000000000000000000 ) ) ;
#107370 = CARTESIAN_POINT ( 'NONE',  ( -36.18398860626899705, 28.73617430169812437, 5.000000000000000000 ) ) ;
#107371 = AXIS2_PLACEMENT_3D ( 'NONE', #21030, #142138, #34794 ) ;
#107372 = ORIENTED_EDGE ( 'NONE', *, *, #31726, .T. ) ;
#107373 = ORIENTED_EDGE ( 'NONE', *, *, #17298, .T. ) ;
#107374 = CARTESIAN_POINT ( 'NONE',  ( 30.31249999999999645, 5.819803920172571310, 5.819803920172575751 ) ) ;
#107375 = ORIENTED_EDGE ( 'NONE', *, *, #13385, .T. ) ;
#107376 = EDGE_CURVE ( 'NONE', #141174, #9436, #17242, .T. ) ;
#107377 = DIRECTION ( 'NONE',  ( 0.6830127018922181881, 0.6830127018922202975, -0.2588190451025214056 ) ) ;
#107378 = CYLINDRICAL_SURFACE ( 'NONE', #61828, 7.950000000000000178 ) ;
#107379 = DIRECTION ( 'NONE',  ( -1.000000000000000000, -1.224606353822377258E-16, -0.000000000000000000 ) ) ;
#107380 = VECTOR ( 'NONE', #89992, 1000.000000000000000 ) ;
#107381 = CARTESIAN_POINT ( 'NONE',  ( 6.628407645496676714, 9.139736423841732040E-16, 0.000000000000000000 ) ) ;
#107382 =( NAMED_UNIT ( * ) SI_UNIT ( $, .STERADIAN. ) SOLID_ANGLE_UNIT ( ) );
#107383 = CARTESIAN_POINT ( 'NONE',  ( 127.2245968585647660, -1.637169565754160949, 6.109999999999997655 ) ) ;
#107384 = EDGE_CURVE ( 'NONE', #116374, #71694, #75224, .T. ) ;
#107385 = AXIS2_PLACEMENT_3D ( 'NONE', #66845, #69000, #110312 ) ;
#107386 = EDGE_LOOP ( 'NONE', ( #11446, #45106, #27219, #140634 ) ) ;
#107387 = FACE_OUTER_BOUND ( 'NONE', #65305, .T. ) ;
#107388 = VERTEX_POINT ( 'NONE', #94780 ) ;
#107389 = FACE_OUTER_BOUND ( 'NONE', #121633, .T. ) ;
#107390 = DIRECTION ( 'NONE',  ( -0.7071067811865487940, 0.7071067811865463515, 0.000000000000000000 ) ) ;
#107391 = CARTESIAN_POINT ( 'NONE',  ( 2.999999999999984457, 16.55218569542899587, 5.000000000000000000 ) ) ;
#107392 = VECTOR ( 'NONE', #128988, 999.9999999999998863 ) ;
#107393 = FACE_OUTER_BOUND ( 'NONE', #129657, .T. ) ;
#107394 = ORIENTED_EDGE ( 'NONE', *, *, #124220, .F. ) ;
#107395 = CARTESIAN_POINT ( 'NONE',  ( 50.16709685856476852, -3.055000000000000160, -5.291415217122921177 ) ) ;
#107396 = ORIENTED_EDGE ( 'NONE', *, *, #113503, .F. ) ;
#107397 = DIRECTION ( 'NONE',  ( 0.7071067811865487940, 0.7071067811865463515, 0.000000000000000000 ) ) ;
#107398 = DIRECTION ( 'NONE',  ( -0.7071067811865487940, 0.7071067811865463515, 0.000000000000000000 ) ) ;
#107399 = CARTESIAN_POINT ( 'NONE',  ( 23.99999999999984013, 8.966399257802171618, 5.000000000000000000 ) ) ;
#107400 = DIRECTION ( 'NONE',  ( 0.000000000000000000, 0.000000000000000000, 1.000000000000000000 ) ) ;
#107401 = VECTOR ( 'NONE', #23836, 999.9999999999998863 ) ;
#107402 = ADVANCED_FACE ( 'NONE', ( #86078 ), #62922, .F. ) ;
#107403 = AXIS2_PLACEMENT_3D ( 'NONE', #97072, #75382, #29703 ) ;
#107404 = CARTESIAN_POINT ( 'NONE',  ( 40.30793019189810877, -6.109999999999998543, 1.637169565754158063 ) ) ;
#107405 = ORIENTED_EDGE ( 'NONE', *, *, #124911, .T. ) ;
#107406 = DIRECTION ( 'NONE',  ( 0.7071067811865487940, 0.7071067811865463515, -0.000000000000000000 ) ) ;
#107407 = ORIENTED_EDGE ( 'NONE', *, *, #56308, .T. ) ;
#107408 = ORIENTED_EDGE ( 'NONE', *, *, #67957, .F. ) ;
#107409 = AXIS2_PLACEMENT_3D ( 'NONE', #96099, #142494, #54772 ) ;
#107410 = ORIENTED_EDGE ( 'NONE', *, *, #17869, .F. ) ;
#107411 = EDGE_CURVE ( 'NONE', #118031, #15339, #109975, .T. ) ;
#107412 = EDGE_CURVE ( 'NONE', #34779, #42914, #130313, .T. ) ;
#107413 = DIRECTION ( 'NONE',  ( -0.000000000000000000, 0.000000000000000000, 1.000000000000000000 ) ) ;
#107414 = DIRECTION ( 'NONE',  ( -0.6830127018922181881, 0.6830127018922202975, -0.2588190451025214056 ) ) ;
#107415 = ORIENTED_EDGE ( 'NONE', *, *, #64840, .F. ) ;
#107416 = CARTESIAN_POINT ( 'NONE',  ( -18.29974487139159223, -27.71228299555219010, 4.000000000000000000 ) ) ;
#107417 = LINE ( 'NONE', #138639, #105768 ) ;
#107418 = VECTOR ( 'NONE', #39768, 1000.000000000000000 ) ;
#107419 = LINE ( 'NONE', #42192, #38974 ) ;
#107420 = CARTESIAN_POINT ( 'NONE',  ( 18.63999999999999702, 9.521314400968980422E-16, 0.000000000000000000 ) ) ;
#107421 = FACE_BOUND ( 'NONE', #82755, .T. ) ;
#107423 = ADVANCED_FACE ( 'NONE', ( #17917 ), #63639, .T. ) ;
#107422 = ORIENTED_EDGE ( 'NONE', *, *, #52215, .F. ) ;
#107424 = CARTESIAN_POINT ( 'NONE',  ( 22.49999999999985789, -11.94781430457070215, 5.000000000000000000 ) ) ;
#107425 = DIRECTION ( 'NONE',  ( 0.6830127018922181881, 0.6830127018922202975, -0.2588190451025214056 ) ) ;
#107426 = CARTESIAN_POINT ( 'NONE',  ( -31.49999999999977973, -2.947814304570804289, 5.000000000000000000 ) ) ;
#107427 = ORIENTED_EDGE ( 'NONE', *, *, #69177, .F. ) ;
#107428 = CARTESIAN_POINT ( 'NONE',  ( -34.92500000000001137, 5.831225763041756771, -1.212213889845635828 ) ) ;
#107429 = ORIENTED_EDGE ( 'NONE', *, *, #52077, .F. ) ;
#107430 = ORIENTED_EDGE ( 'NONE', *, *, #72003, .T. ) ;
#107431 = CARTESIAN_POINT ( 'NONE',  ( 3.813491353976365961, -15.74070752338412049, 8.904080028138931624 ) ) ;
#107432 = EDGE_LOOP ( 'NONE', ( #101200, #10167, #139200 ) ) ;
#107433 = CARTESIAN_POINT ( 'NONE',  ( 61.01626352523143737, -4.472830434245838482, 4.472830434245838482 ) ) ;
#107435 = ORIENTED_EDGE ( 'NONE', *, *, #25353, .F. ) ;
#107434 = VECTOR ( 'NONE', #121364, 1000.000000000000000 ) ;
#107436 = FACE_OUTER_BOUND ( 'NONE', #44766, .T. ) ;
#107437 = CARTESIAN_POINT ( 'NONE',  ( -25.21498419724174767, -3.740707523384238176, 15.76143240460118200 ) ) ;
#107438 = EDGE_LOOP ( 'NONE', ( #54578, #26406, #130279, #10660, #10924 ) ) ;
#107439 = VECTOR ( 'NONE', #115420, 1000.000000000000227 ) ;
#107440 = CARTESIAN_POINT ( 'NONE',  ( -17.01299345043647548, -0.9444868035624306435, -36.99999999997771738 ) ) ;
#107441 = CARTESIAN_POINT ( 'NONE',  ( 32.27718569542918203, -21.72500000000000142, 5.000000000000000000 ) ) ;
#107442 = DIRECTION ( 'NONE',  ( 0.7071067811865486830, -0.7071067811865463515, 0.000000000000000000 ) ) ;
#107443 = CARTESIAN_POINT ( 'NONE',  ( 53.99451991528749062, 28.92564299267975869, 4.000000000000000000 ) ) ;
#107444 = ORIENTED_EDGE ( 'NONE', *, *, #94149, .F. ) ;
#107445 = VERTEX_POINT ( 'NONE', #107801 ) ;
#107446 = CARTESIAN_POINT ( 'NONE',  ( -27.75860074219777118, 21.72500000000000142, 5.000000000000000000 ) ) ;
#107447 = PLANE ( 'NONE',  #111495 ) ;
#107448 = ORIENTED_EDGE ( 'NONE', *, *, #135821, .T. ) ;
#107449 = EDGE_CURVE ( 'NONE', #95865, #135641, #9173, .T. ) ;
#107450 = EDGE_LOOP ( 'NONE', ( #4131, #102868, #102659, #20588 ) ) ;
#107451 = ORIENTED_EDGE ( 'NONE', *, *, #122414, .T. ) ;
#107452 = CARTESIAN_POINT ( 'NONE',  ( 14.99999999999990230, 11.96639925780214320, 5.000000000000000000 ) ) ;
#107453 = CARTESIAN_POINT ( 'NONE',  ( 63.18398860626900415, 28.73617430169831621, 5.000000000000000000 ) ) ;
#107454 = ADVANCED_FACE ( 'NONE', ( #30256 ), #53439, .T. ) ;
#107455 = EDGE_CURVE ( 'NONE', #71262, #102314, #46172, .T. ) ;
#107456 = DIRECTION ( 'NONE',  ( -0.7071067811865487940, 0.7071067811865463515, -0.000000000000000000 ) ) ;
#107457 = VERTEX_POINT ( 'NONE', #31695 ) ;
#107458 = CARTESIAN_POINT ( 'NONE',  ( -5.671830600776425868, -15.74070752338412049, 4.000000000000000000 ) ) ;
#107459 = AXIS2_PLACEMENT_3D ( 'NONE', #135294, #100508, #446 ) ;
#107461 = EDGE_CURVE ( 'NONE', #39522, #123360, #44762, .T. ) ;
#107460 = CARTESIAN_POINT ( 'NONE',  ( 18.29974487139159223, -27.71228299555219010, 4.000000000000000000 ) ) ;
#107462 = EDGE_CURVE ( 'NONE', #9125, #138634, #90350, .T. ) ;
#107463 = VECTOR ( 'NONE', #139496, 1000.000000000000000 ) ;
#107464 = CARTESIAN_POINT ( 'NONE',  ( 22.23373647476855197, 5.808823158059036373, 5.808823158059032821 ) ) ;
#107465 = CARTESIAN_POINT ( 'NONE',  ( 8.999999999999932498, 5.966399257802197376, 5.000000000000000000 ) ) ;
#107466 = EDGE_CURVE ( 'NONE', #134862, #10403, #12773, .T. ) ;
#107467 = ORIENTED_EDGE ( 'NONE', *, *, #61472, .F. ) ;
#107468 = CARTESIAN_POINT ( 'NONE',  ( 117.3079301918980946, -6.109999999999999432, 1.637169565754158507 ) ) ;
#107469 = STYLED_ITEM ( 'NONE', ( #52764 ), #89171 ) ;
#107470 = EDGE_CURVE ( 'NONE', #130889, #99583, #44006, .T. ) ;
#107471 = CARTESIAN_POINT ( 'NONE',  ( -12.69999999999998153, 0.000000000000000000, 0.000000000000000000 ) ) ;
#107472 = CARTESIAN_POINT ( 'NONE',  ( -34.92500000000001137, 18.85612307739224036, 4.000000000000000000 ) ) ;
#107474 = ORIENTED_EDGE ( 'NONE', *, *, #42598, .T. ) ;
#107473 = LINE ( 'NONE', #19750, #14764 ) ;
#107475 = CARTESIAN_POINT ( 'NONE',  ( 67.45419371712955581, 6.884901960086283523, 3.975000000000002753 ) ) ;
#107476 = ORIENTED_EDGE ( 'NONE', *, *, #118390, .F. ) ;
#107477 = ADVANCED_FACE ( 'NONE', ( #101221 ), #120085, .T. ) ;
#107478 = CARTESIAN_POINT ( 'NONE',  ( 76.05836038379622721, -7.949999999999996625, -2.130196079827426203 ) ) ;
#107479 = DIRECTION ( 'NONE',  ( 0.3543493200069162685, -0.000000000000000000, -0.9351131265310288487 ) ) ;
#107480 = DIRECTION ( 'NONE',  ( 0.000000000000000000, -1.000000000000000000, 0.000000000000000000 ) ) ;
#107481 = VERTEX_POINT ( 'NONE', #56352 ) ;
#107482 = EDGE_CURVE ( 'NONE', #358, #8173, #78069, .T. ) ;
#107483 = CARTESIAN_POINT ( 'NONE',  ( 8.999999999999941380, 13.55218569542903140, 5.000000000000000000 ) ) ;
#107484 = PLANE ( 'NONE',  #113558 ) ;
#107485 = DIRECTION ( 'NONE',  ( -0.6830127018922181881, 0.6830127018922202975, -0.2588190451025214056 ) ) ;
#107486 = VERTEX_POINT ( 'NONE', #143301 ) ;
#107487 = LINE ( 'NONE', #30669, #134202 ) ;
#107488 = DIRECTION ( 'NONE',  ( 0.000000000000000000, 0.000000000000000000, 1.000000000000000000 ) ) ;
#107489 = ADVANCED_FACE ( 'NONE', ( #120826 ), #54199, .F. ) ;
#107490 = CARTESIAN_POINT ( 'NONE',  ( 3.937500000000000000, -4.461849672132299105, 4.461849672132299993 ) ) ;
#107491 = DIRECTION ( 'NONE',  ( 0.3543493200069162685, -0.000000000000000000, -0.9351131265310288487 ) ) ;
#107492 = AXIS2_PLACEMENT_3D ( 'NONE', #136719, #1879, #70099 ) ;
#107493 = EDGE_LOOP ( 'NONE', ( #4000, #1577, #96601, #53771 ) ) ;
#107494 = EDGE_LOOP ( 'NONE', ( #130454, #123355 ) ) ;
#107495 = DIRECTION ( 'NONE',  ( -0.7071067811865486830, 0.7071067811865464625, 0.000000000000000000 ) ) ;
#107496 = DIRECTION ( 'NONE',  ( 0.7071067811865486830, -0.7071067811865464625, -0.000000000000000000 ) ) ;
#107497 = ADVANCED_FACE ( 'NONE', ( #67183 ), #466, .F. ) ;
#107498 = AXIS2_PLACEMENT_3D ( 'NONE', #90359, #23680, #103357 ) ;
#107499 = CARTESIAN_POINT ( 'NONE',  ( 11.49956980810188689, -3.967499999999998028, -6.871911579029511330 ) ) ;
#107500 = CARTESIAN_POINT ( 'NONE',  ( 7.940000000000001279, -60.26999999999998892, -11.89864999999999640 ) ) ;
#107501 = VECTOR ( 'NONE', #65442, 1000.000000000000000 ) ;
#107502 = AXIS2_PLACEMENT_3D ( 'NONE', #73111, #117271, #29560 ) ;
#107503 = DIRECTION ( 'NONE',  ( 0.7071067811865487940, 0.7071067811865463515, 0.000000000000000000 ) ) ;
#107504 = LINE ( 'NONE', #28541, #134806 ) ;
#107505 = EDGE_LOOP ( 'NONE', ( #130524, #127230, #6062, #63709 ) ) ;
#107506 = DIRECTION ( 'NONE',  ( 0.000000000000000000, 0.000000000000000000, -1.000000000000000000 ) ) ;
#107507 = CARTESIAN_POINT ( 'NONE',  ( 27.48921356237309155, -27.52281430457074762, 5.000000000000000000 ) ) ;
#107508 = DIRECTION ( 'NONE',  ( 0.7071067811865487940, 0.7071067811865463515, -0.000000000000000000 ) ) ;
#107509 = LINE ( 'NONE', #27094, #71431 ) ;
#107510 = CARTESIAN_POINT ( 'NONE',  ( 40.16209685856478018, -5.291415217122919401, 3.054999999999998384 ) ) ;
#107511 = CARTESIAN_POINT ( 'NONE',  ( 31.99806943317879515, -22.22500000000000142, 4.500000000000000888 ) ) ;
#107512 = AXIS2_PLACEMENT_3D ( 'NONE', #17054, #137410, #38105 ) ;
#107513 = ORIENTED_EDGE ( 'NONE', *, *, #42617, .F. ) ;
#107514 = CYLINDRICAL_SURFACE ( 'NONE', #88286, 1.000000000000000888 ) ;
#107515 = ORIENTED_EDGE ( 'NONE', *, *, #91318, .F. ) ;
#107516 = EDGE_CURVE ( 'NONE', #126734, #92516, #109245, .T. ) ;
#107517 = ORIENTED_EDGE ( 'NONE', *, *, #59895, .T. ) ;
#107518 = CARTESIAN_POINT ( 'NONE',  ( 22.49999999999985079, 13.08746187583910725, 4.000000000000000000 ) ) ;
#107519 = DIRECTION ( 'NONE',  ( 0.000000000000000000, 0.000000000000000000, -1.000000000000000000 ) ) ;
#107520 = ORIENTED_EDGE ( 'NONE', *, *, #77848, .T. ) ;
#107521 = EDGE_CURVE ( 'NONE', #113241, #12982, #121540, .T. ) ;
#107522 = DIRECTION ( 'NONE',  ( 0.000000000000000000, -1.000000000000000000, 0.000000000000000000 ) ) ;
#107523 = DIRECTION ( 'NONE',  ( 0.3543493200069162685, -0.000000000000000000, -0.9351131265310288487 ) ) ;
#107524 = DIRECTION ( 'NONE',  ( -0.6830127018922181881, 0.6830127018922202975, -0.2588190451025214056 ) ) ;
#107525 = DIRECTION ( 'NONE',  ( -0.6830127018922180770, -0.6830127018922204085, -0.2588190451025213501 ) ) ;
#107526 = LINE ( 'NONE', #51745, #57017 ) ;
#107527 = ORIENTED_EDGE ( 'NONE', *, *, #124349, .T. ) ;
#107528 = DIRECTION ( 'NONE',  ( -0.000000000000000000, 0.3543493200069153248, 0.9351131265310292928 ) ) ;
#107529 = DIRECTION ( 'NONE',  ( 0.000000000000000000, -1.000000000000000000, 0.000000000000000000 ) ) ;
#107530 = CARTESIAN_POINT ( 'NONE',  ( -36.48921356237310221, -27.52281430457080802, 5.000000000000000000 ) ) ;
#107531 = CARTESIAN_POINT ( 'NONE',  ( 0.000000000000000000, 0.000000000000000000, 5.000000000000000000 ) ) ;
#107532 = FACE_OUTER_BOUND ( 'NONE', #106674, .T. ) ;
#107533 = EDGE_CURVE ( 'NONE', #83048, #47602, #34555, .T. ) ;
#107534 = CARTESIAN_POINT ( 'NONE',  ( 103.4750270504628844, -5.819803920172573086, 5.819803920172573086 ) ) ;
#107535 = CARTESIAN_POINT ( 'NONE',  ( 53.89169371712955581, 2.130196079827421762, 7.950000000000001066 ) ) ;
#107536 = DIRECTION ( 'NONE',  ( -0.7071067811865487940, 0.7071067811865463515, 0.000000000000000000 ) ) ;
#107537 = ORIENTED_EDGE ( 'NONE', *, *, #114850, .F. ) ;
#107538 = ORIENTED_EDGE ( 'NONE', *, *, #80977, .T. ) ;
#107539 = CARTESIAN_POINT ( 'NONE',  ( 51.16666666666666430, 6.884901960086285300, 3.975000000000003642 ) ) ;
#107540 = CARTESIAN_POINT ( 'NONE',  ( 34.92499999999998295, 15.66246187583885963, 4.000000000000000000 ) ) ;
#107541 = EDGE_CURVE ( 'NONE', #47692, #4072, #12065, .T. ) ;
#107542 = CARTESIAN_POINT ( 'NONE',  ( -11.99999999999991118, -15.41253812416059787, 4.000000000000000000 ) ) ;
#107543 = DIRECTION ( 'NONE',  ( 0.000000000000000000, 0.000000000000000000, 1.000000000000000000 ) ) ;
#107544 = VERTEX_POINT ( 'NONE', #78780 ) ;
#107545 = AXIS2_PLACEMENT_3D ( 'NONE', #118110, #27546, #139928 ) ;
#107546 = LINE ( 'NONE', #19818, #109422 ) ;
#107547 = CARTESIAN_POINT ( 'NONE',  ( 48.41709685856476852, 3.054999999999998828, 5.291415217122922066 ) ) ;
#107548 = EDGE_LOOP ( 'NONE', ( #16192, #42642, #43992, #116261 ) ) ;
#107549 = DIRECTION ( 'NONE',  ( -0.7071067811865486830, -0.7071067811865464625, 0.000000000000000000 ) ) ;
#107550 = EDGE_LOOP ( 'NONE', ( #25709, #120637, #121848, #27390 ) ) ;
#107551 = ORIENTED_EDGE ( 'NONE', *, *, #50056, .F. ) ;
#107552 = PLANE ( 'NONE',  #90966 ) ;
#107553 =( LENGTH_UNIT ( ) NAMED_UNIT ( * ) SI_UNIT ( .MILLI., .METRE. ) );
#107554 = LINE ( 'NONE', #96645, #9553 ) ;
#107555 = FILL_AREA_STYLE ('',( #64068 ) ) ;
#107556 = ORIENTED_EDGE ( 'NONE', *, *, #3092, .T. ) ;
#107557 = EDGE_CURVE ( 'NONE', #7557, #30943, #45457, .T. ) ;
#107558 = CARTESIAN_POINT ( 'NONE',  ( 24.39999999999999858, -1.600000000000012301, -20.40202195861969514 ) ) ;
#107561 = ADVANCED_FACE ( 'NONE', ( #55602 ), #11321, .F. ) ;
#107560 = VERTEX_POINT ( 'NONE', #131727 ) ;
#107559 = DIRECTION ( 'NONE',  ( 1.000000000000000000, 0.000000000000000000, 0.000000000000000000 ) ) ;
#107562 = CARTESIAN_POINT ( 'NONE',  ( 14.43749999999999822, -4.461849672132299105, 4.461849672132299993 ) ) ;
#107563 = CARTESIAN_POINT ( 'NONE',  ( 36.48921356237310221, -27.52281430457080802, 5.000000000000000000 ) ) ;
#107564 = VECTOR ( 'NONE', #122787, 1000.000000000000000 ) ;
#107565 = PLANE ( 'NONE',  #90081 ) ;
#107566 = EDGE_LOOP ( 'NONE', ( #112126, #22795, #103786, #117647 ) ) ;
#107567 = STYLED_ITEM ( 'NONE', ( #31953 ), #104071 ) ;
#107568 = VERTEX_POINT ( 'NONE', #32417 ) ;
#107569 = DIRECTION ( 'NONE',  ( 0.7071067811865487940, 0.7071067811865463515, -0.000000000000000000 ) ) ;
#107570 = CARTESIAN_POINT ( 'NONE',  ( 66.84959685856479439, 6.109999999999996767, 1.637169565754163836 ) ) ;
#107571 = DIRECTION ( 'NONE',  ( 0.7071067811865487940, 0.7071067811865463515, 0.000000000000000000 ) ) ;
#107572 = CARTESIAN_POINT ( 'NONE',  ( -21.48921356237309155, -27.52281430457070499, 5.000000000000000000 ) ) ;
#107573 = SURFACE_SIDE_STYLE ('',( #71400 ) ) ;
#107574 = ORIENTED_EDGE ( 'NONE', *, *, #95965, .F. ) ;
#107575 = ORIENTED_EDGE ( 'NONE', *, *, #75762, .F. ) ;
#107576 = DIRECTION ( 'NONE',  ( 0.7071067811865487940, -0.7071067811865463515, 0.000000000000000000 ) ) ;
#107577 = CARTESIAN_POINT ( 'NONE',  ( 3.087196949643289834, 3.821174125832445049E-16, 0.000000000000000000 ) ) ;
#107578 = ORIENTED_EDGE ( 'NONE', *, *, #16310, .F. ) ;
#107580 = EDGE_CURVE ( 'NONE', #67772, #55981, #76651, .T. ) ;
#107579 =( BOUNDED_CURVE ( )  B_SPLINE_CURVE ( 3, ( #87701, #32629, #99258, #77568 ),
 .UNSPECIFIED., .F., .F. ) 
 B_SPLINE_CURVE_WITH_KNOTS ( ( 4, 4 ),
 ( 5.005968288816728951, 5.074607125596368284 ),
 .UNSPECIFIED. ) 
 CURVE ( )  GEOMETRIC_REPRESENTATION_ITEM ( )  RATIONAL_B_SPLINE_CURVE ( ( 1.000000000000000000, 0.9996074310407762065, 0.9996074310407762065, 1.000000000000000000 ) ) 
 REPRESENTATION_ITEM ( '' )  );
#107581 = ORIENTED_EDGE ( 'NONE', *, *, #50531, .T. ) ;
#107582 = EDGE_CURVE ( 'NONE', #44190, #99753, #99794, .T. ) ;
#107583 = VECTOR ( 'NONE', #125149, 1000.000000000000000 ) ;
#107584 = CARTESIAN_POINT ( 'NONE',  ( -19.05499999999999261, 3.130000000000007887, -22.35000000000000142 ) ) ;
#107585 = ORIENTED_EDGE ( 'NONE', *, *, #102615, .T. ) ;
#107586 = DIRECTION ( 'NONE',  ( 0.3543493200069162685, -0.000000000000000000, -0.9351131265310288487 ) ) ;
#107587 = CARTESIAN_POINT ( 'NONE',  ( 0.02842916987967500017, 0.5999999999999986455, 3.398229573760036093 ) ) ;
#107588 =( BOUNDED_CURVE ( )  B_SPLINE_CURVE ( 3, ( #23461, #68441, #112620, #2393 ),
 .UNSPECIFIED., .F., .T. ) 
 B_SPLINE_CURVE_WITH_KNOTS ( ( 4, 4 ),
 ( 1.208578181583223055, 1.359146454359418055 ),
 .UNSPECIFIED. ) 
 CURVE ( )  GEOMETRIC_REPRESENTATION_ITEM ( )  RATIONAL_B_SPLINE_CURVE ( ( 1.000000000000000000, 0.9981116584018954185, 0.9981116584018954185, 1.000000000000000000 ) ) 
 REPRESENTATION_ITEM ( '' )  );
#107589 = LINE ( 'NONE', #130809, #30399 ) ;
#107590 = FACE_BOUND ( 'NONE', #111823, .T. ) ;
#107591 = EDGE_CURVE ( 'NONE', #85633, #90206, #138698, .T. ) ;
#107592 = DIRECTION ( 'NONE',  ( -0.3543493200069162685, -0.000000000000000000, -0.9351131265310288487 ) ) ;
#107593 = PLANE ( 'NONE',  #49010 ) ;
#107594 = CARTESIAN_POINT ( 'NONE',  ( 23.99999999999983302, -19.22509904557634286, 1.855685503482233933 ) ) ;
#107596 = VERTEX_POINT ( 'NONE', #139429 ) ;
#107595 = DIRECTION ( 'NONE',  ( 0.6830127018922181881, 0.6830127018922202975, -0.2588190451025214056 ) ) ;
#107597 = SURFACE_SIDE_STYLE ('',( #51819 ) ) ;
#107598 = AXIS2_PLACEMENT_3D ( 'NONE', #64584, #53727, #96456 ) ;
#107599 = ORIENTED_EDGE ( 'NONE', *, *, #93346, .F. ) ;
#107600 = VECTOR ( 'NONE', #123846, 1000.000000000000000 ) ;
#107602 = ORIENTED_EDGE ( 'NONE', *, *, #134166, .T. ) ;
#107601 = AXIS2_PLACEMENT_3D ( 'NONE', #95506, #19384, #52024 ) ;
#107603 = CARTESIAN_POINT ( 'NONE',  ( 84.64126352523145158, 4.472830434245835818, 4.472830434245840259 ) ) ;
#107604 = ORIENTED_EDGE ( 'NONE', *, *, #75166, .T. ) ;
#107605 = FACE_OUTER_BOUND ( 'NONE', #98381, .T. ) ;
#107606 = CIRCLE ( 'NONE', #26590, 2.500000000000000888 ) ;
#107607 = DIRECTION ( 'NONE',  ( 0.7071067811865487940, 0.7071067811865463515, 0.000000000000000000 ) ) ;
#107608 = DIRECTION ( 'NONE',  ( -0.7071067811865486830, -0.7071067811865464625, 0.000000000000000000 ) ) ;
#107609 = DIRECTION ( 'NONE',  ( -0.000000000000000000, -0.3543493200069152138, 0.9351131265310292928 ) ) ;
#107610 = LINE ( 'NONE', #53987, #34522 ) ;
#107611 = PLANE ( 'NONE',  #128781 ) ;
#107612 = CARTESIAN_POINT ( 'NONE',  ( -14.99999999999990230, 7.007997736742436423, -8.085015511992146742 ) ) ;
#107613 = DIRECTION ( 'NONE',  ( -0.7071067811865486830, -0.7071067811865464625, 0.000000000000000000 ) ) ;
#107614 = CARTESIAN_POINT ( 'NONE',  ( -24.18398860626899705, 28.73617430169804265, 5.000000000000000000 ) ) ;
#107615 = DIRECTION ( 'NONE',  ( -0.7071067811865486830, -0.7071067811865464625, 0.000000000000000000 ) ) ;
#107616 = ORIENTED_EDGE ( 'NONE', *, *, #14849, .T. ) ;
#107617 = DIRECTION ( 'NONE',  ( -0.7071067811865487940, 0.7071067811865463515, -0.000000000000000000 ) ) ;
#107618 = ORIENTED_EDGE ( 'NONE', *, *, #129201, .F. ) ;
#107619 = LINE ( 'NONE', #8279, #42614 ) ;
#107620 = CARTESIAN_POINT ( 'NONE',  ( 1.734723475976807094E-15, -0.03360074219774071558, 5.000000000000000000 ) ) ;
#107621 = ORIENTED_EDGE ( 'NONE', *, *, #43631, .F. ) ;
#107622 = ORIENTED_EDGE ( 'NONE', *, *, #60211, .F. ) ;
#107623 = ORIENTED_EDGE ( 'NONE', *, *, #4994, .T. ) ;
#107624 = CARTESIAN_POINT ( 'NONE',  ( 39.22959685856476142, -6.110000000000000320, -1.637169565754161393 ) ) ;
#107625 = VERTEX_POINT ( 'NONE', #59195 ) ;
#107626 = CARTESIAN_POINT ( 'NONE',  ( 45.62500000000000000, -7.950000000000000178, -4.867971026610729436E-16 ) ) ;
#107627 = EDGE_CURVE ( 'NONE', #89442, #76045, #94445, .T. ) ;
#107628 = CARTESIAN_POINT ( 'NONE',  ( 22.06663961620377634, 1.633150327867695095, 6.094999999999988205 ) ) ;
#107629 = CARTESIAN_POINT ( 'NONE',  ( -4.332298631122367460, 13.32507652626317096, -24.69132185691248438 ) ) ;
#107630 = ADVANCED_FACE ( 'NONE', ( #50964 ), #39384, .T. ) ;
#107631 = ORIENTED_EDGE ( 'NONE', *, *, #12363, .F. ) ;
#107632 = B_SPLINE_CURVE_WITH_KNOTS ( 'NONE', 3,
 ( #73692, #139698, #17172, #128093, #28773, #71562, #95433, #4804, #61435, #6952, #5553, #40378, #51953, #117863, #38923, #127349, #84581, #38218, #115010, #105576, #81748, #106277, #93300, #128778 ),
 .UNSPECIFIED., .F., .F.,
 ( 4, 2, 2, 2, 2, 2, 2, 2, 2, 2, 2, 4 ),
 ( 0.01986637577891036885, 0.02043143082653421302, 0.02099648587415805720, 0.02212659596940574208, 0.02269165101702958626, 0.02325670606465343043, 0.02438681615990111531, 0.02495187120752495602, 0.02551692625514880020, 0.02664703635039648508, 0.02777714644564416996, 0.02890725654089185484 ),
 .UNSPECIFIED. ) ;
#107633 = CARTESIAN_POINT ( 'NONE',  ( 0.000000000000000000, 0.000000000000000000, 5.000000000000000000 ) ) ;
#107635 = ORIENTED_EDGE ( 'NONE', *, *, #2838, .F. ) ;
#107634 = EDGE_CURVE ( 'NONE', #126278, #63804, #25804, .T. ) ;
#107636 = LINE ( 'NONE', #30827, #69637 ) ;
#107637 = DIRECTION ( 'NONE',  ( 0.6830127018922180770, -0.6830127018922204085, -0.2588190451025213501 ) ) ;
#107639 = VERTEX_POINT ( 'NONE', #14212 ) ;
#107638 = CARTESIAN_POINT ( 'NONE',  ( -45.18398860626900415, 28.73617430169818832, 5.000000000000000000 ) ) ;
#107640 = EDGE_LOOP ( 'NONE', ( #79940, #103800, #21910, #6317, #58746 ) ) ;
#107641 = EDGE_CURVE ( 'NONE', #119366, #64166, #57756, .T. ) ;
#107642 = CARTESIAN_POINT ( 'NONE',  ( 10.49999999999992539, -11.56887692260769640, 4.000000000000000000 ) ) ;
#107643 = CARTESIAN_POINT ( 'NONE',  ( -9.183988606268997046, 28.73617430169793607, 5.000000000000000000 ) ) ;
#107644 = EDGE_LOOP ( 'NONE', ( #133312, #133662, #47800, #140767 ) ) ;
#107645 = FACE_OUTER_BOUND ( 'NONE', #42362, .T. ) ;
#107646 = ORIENTED_EDGE ( 'NONE', *, *, #113153, .F. ) ;
#107647 = ORIENTED_EDGE ( 'NONE', *, *, #74422, .F. ) ;
#107648 = VERTEX_POINT ( 'NONE', #106015 ) ;
#107649 = ADVANCED_FACE ( 'NONE', ( #84330 ), #47610, .F. ) ;
#107650 = CYLINDRICAL_SURFACE ( 'NONE', #7745, 2.500000000000000000 ) ;
#107651 = DIRECTION ( 'NONE',  ( 0.6830127018922181881, 0.6830127018922202975, -0.2588190451025214056 ) ) ;
#107652 = DIRECTION ( 'NONE',  ( -0.7071067811865487940, 0.7071067811865463515, -0.000000000000000000 ) ) ;
#107653 = EDGE_CURVE ( 'NONE', #130333, #91901, #40115, .T. ) ;
#107654 = LINE ( 'NONE', #8314, #37887 ) ;
#107655 = FACE_OUTER_BOUND ( 'NONE', #60872, .T. ) ;
#107656 = EDGE_CURVE ( 'NONE', #38538, #74972, #123725, .T. ) ;
#107658 = ORIENTED_EDGE ( 'NONE', *, *, #49747, .T. ) ;
#107657 = B_SPLINE_CURVE_WITH_KNOTS ( 'NONE', 3,
 ( #132189, #77800, #121283, #56075, #88685, #182 ),
 .UNSPECIFIED., .F., .F.,
 ( 4, 2, 4 ),
 ( 0.01602987264650632127, 0.01771478214218283678, 0.01939969163785935230 ),
 .UNSPECIFIED. ) ;
#107659 = CARTESIAN_POINT ( 'NONE',  ( 32.67183060077623225, -18.74070752338409562, 4.000000000000000000 ) ) ;
#107660 = ORIENTED_EDGE ( 'NONE', *, *, #105049, .F. ) ;
#107661 = DIRECTION ( 'NONE',  ( -0.3543493200069163240, 0.000000000000000000, 0.9351131265310288487 ) ) ;
#107662 = ADVANCED_FACE ( 'NONE', ( #91096 ), #91915, .T. ) ;
#107663 = VECTOR ( 'NONE', #42683, 1000.000000000000000 ) ;
#107664 = CARTESIAN_POINT ( 'NONE',  ( 30.74956980810188867, 3.967499999999998916, 6.871911579029510442 ) ) ;
#107665 = ORIENTED_EDGE ( 'NONE', *, *, #42233, .F. ) ;
#107666 = DIRECTION ( 'NONE',  ( -0.3543493200069162685, -0.000000000000000000, -0.9351131265310288487 ) ) ;
#107667 = DIRECTION ( 'NONE',  ( 1.000000000000000000, 0.000000000000000000, 0.000000000000000000 ) ) ;
#107668 = ORIENTED_EDGE ( 'NONE', *, *, #4673, .F. ) ;
#107669 = VECTOR ( 'NONE', #125950, 1000.000000000000000 ) ;
#107670 = EDGE_LOOP ( 'NONE', ( #50592, #90153, #13088, #60910 ) ) ;
#107671 = LINE ( 'NONE', #61376, #69568 ) ;
#107672 = LINE ( 'NONE', #95372, #23314 ) ;
#107673 = DIRECTION ( 'NONE',  ( 0.7071067811865486830, -0.7071067811865464625, -0.000000000000000000 ) ) ;
#107674 = LINE ( 'NONE', #75092, #14953 ) ;
#107675 = CARTESIAN_POINT ( 'NONE',  ( 22.00193056682082826, -22.22500000000000142, 4.500000000000000888 ) ) ;
#107676 = CARTESIAN_POINT ( 'NONE',  ( 61.59959685856478018, -6.109999999999998543, -1.637169565754160727 ) ) ;
#107677 = CARTESIAN_POINT ( 'NONE',  ( 39.18398860626899705, 28.73617430169814568, 5.000000000000000000 ) ) ;
#107678 = VECTOR ( 'NONE', #31218, 999.9999999999998863 ) ;
#107679 = CARTESIAN_POINT ( 'NONE',  ( -6.874395825605905230, -40.07226884389044841, 19.48967909493512352 ) ) ;
#107680 = DIRECTION ( 'NONE',  ( 0.7071067811865486830, -0.7071067811865464625, -0.000000000000000000 ) ) ;
#107681 = ORIENTED_EDGE ( 'NONE', *, *, #105314, .T. ) ;
#107682 = DIRECTION ( 'NONE',  ( 1.000000000000000000, 0.000000000000000000, 0.000000000000000000 ) ) ;
#107683 = ADVANCED_FACE ( 'NONE', ( #87767 ), #93744, .T. ) ;
#107684 = VERTEX_POINT ( 'NONE', #40704 ) ;
#107685 = FACE_OUTER_BOUND ( 'NONE', #57363, .T. ) ;
#107686 = SURFACE_STYLE_FILL_AREA ( #19961 ) ;
#107687 = ORIENTED_EDGE ( 'NONE', *, *, #96638, .T. ) ;
#107688 = DIRECTION ( 'NONE',  ( -0.6830127018922180770, -0.6830127018922204085, -0.2588190451025214056 ) ) ;
#107690 = ORIENTED_EDGE ( 'NONE', *, *, #42208, .F. ) ;
#107689 = FACE_OUTER_BOUND ( 'NONE', #40739, .T. ) ;
#107691 = CARTESIAN_POINT ( 'NONE',  ( 42.18398860626899705, 28.73617430169816700, 5.000000000000000000 ) ) ;
#107692 = PLANE ( 'NONE',  #37073 ) ;
#107693 = LINE ( 'NONE', #62802, #8308 ) ;
#107694 = ORIENTED_EDGE ( 'NONE', *, *, #24593, .T. ) ;
#107695 = ADVANCED_FACE ( 'NONE', ( #118956 ), #84906, .T. ) ;
#107696 = ORIENTED_EDGE ( 'NONE', *, *, #77766, .T. ) ;
#107697 =( NAMED_UNIT ( * ) SI_UNIT ( $, .STERADIAN. ) SOLID_ANGLE_UNIT ( ) );
#107698 = DIRECTION ( 'NONE',  ( -0.6830127018922180770, -0.6830127018922204085, -0.2588190451025213501 ) ) ;
#107699 = DIRECTION ( 'NONE',  ( 0.7071067811865486830, -0.7071067811865464625, -0.000000000000000000 ) ) ;
#107700 = AXIS2_PLACEMENT_3D ( 'NONE', #89891, #34824, #47178 ) ;
#107701 = CARTESIAN_POINT ( 'NONE',  ( 85.10002705046289861, 5.819803920172570422, 5.819803920172574863 ) ) ;
#107703 = VECTOR ( 'NONE', #19908, 1000.000000000000114 ) ;
#107702 = CARTESIAN_POINT ( 'NONE',  ( 7.637717201596474048, 4.584330080086930965E-16, 0.000000000000000000 ) ) ;
#107704 = LINE ( 'NONE', #8362, #20561 ) ;
#107705 = ORIENTED_EDGE ( 'NONE', *, *, #77196, .T. ) ;
#107706 = AXIS2_PLACEMENT_3D ( 'NONE', #76380, #65534, #130043 ) ;
#107707 = LINE ( 'NONE', #8364, #95502 ) ;
#107708 = EDGE_CURVE ( 'NONE', #46912, #71167, #42145, .T. ) ;
#107709 = CARTESIAN_POINT ( 'NONE',  ( 30.48921356237309510, -27.52281430457076894, 5.000000000000000000 ) ) ;
#107710 = CARTESIAN_POINT ( 'NONE',  ( 29.02083333333333215, -6.094999999999989981, -1.633150327867689100 ) ) ;
#107711 = ORIENTED_EDGE ( 'NONE', *, *, #115973, .F. ) ;
#107712 = CARTESIAN_POINT ( 'NONE',  ( 0.000000000000000000, 0.000000000000000000, 5.000000000000000000 ) ) ;
#107713 = ORIENTED_EDGE ( 'NONE', *, *, #33416, .T. ) ;
#107714 = EDGE_CURVE ( 'NONE', #6561, #109345, #49799, .T. ) ;
#107715 = CARTESIAN_POINT ( 'NONE',  ( 75.10459685856474721, 1.637169565754164946, -6.109999999999999432 ) ) ;
#107716 = CARTESIAN_POINT ( 'NONE',  ( -14.29289321881335795, 8.259292476615634371, 5.000000000000000000 ) ) ;
#107717 = CARTESIAN_POINT ( 'NONE',  ( 8.999999999999937828, -0.2811185226894198363, -5.995736974527534180 ) ) ;
#107718 = EDGE_LOOP ( 'NONE', ( #120283, #95322, #84716 ) ) ;
#107719 = CARTESIAN_POINT ( 'NONE',  ( 27.48921356237309155, -27.52281430457074762, 5.000000000000000000 ) ) ;
#107720 = DIRECTION ( 'NONE',  ( -0.7071067811865487940, 0.7071067811865463515, 0.000000000000000000 ) ) ;
#107721 = LINE ( 'NONE', #130221, #46390 ) ;
#107722 = EDGE_CURVE ( 'NONE', #67449, #111297, #19646, .T. ) ;
#107723 = DIRECTION ( 'NONE',  ( 1.000000000000000000, 0.000000000000000000, 0.000000000000000000 ) ) ;
#107725 = VERTEX_POINT ( 'NONE', #130575 ) ;
#107724 = DIRECTION ( 'NONE',  ( 0.7071067811865486830, -0.7071067811865464625, -0.000000000000000000 ) ) ;
#107726 = FACE_OUTER_BOUND ( 'NONE', #60236, .T. ) ;
#107727 = DIRECTION ( 'NONE',  ( -0.3543493200069162685, -0.000000000000000000, -0.9351131265310288487 ) ) ;
#107728 = DIRECTION ( 'NONE',  ( 1.000000000000000000, 0.000000000000000000, 0.000000000000000000 ) ) ;
#107729 = DIRECTION ( 'NONE',  ( 1.000000000000000000, -0.000000000000000000, 0.000000000000000000 ) ) ;
#107730 = ORIENTED_EDGE ( 'NONE', *, *, #39651, .T. ) ;
#107731 = ORIENTED_EDGE ( 'NONE', *, *, #56125, .T. ) ;
#107732 = CARTESIAN_POINT ( 'NONE',  ( 73.93793019189809002, -6.110000000000001208, 1.637169565754158951 ) ) ;
#107733 = ORIENTED_EDGE ( 'NONE', *, *, #38683, .F. ) ;
#107734 = CARTESIAN_POINT ( 'NONE',  ( 18.53421140649331633, 9.121673282332597665, 4.000000000000000000 ) ) ;
#107735 = DIRECTION ( 'NONE',  ( 0.000000000000000000, -1.000000000000000000, 0.000000000000000000 ) ) ;
#107736 = CARTESIAN_POINT ( 'NONE',  ( 8.673617379884035472E-16, 16.55218569542899587, 5.000000000000000000 ) ) ;
#107737 = CARTESIAN_POINT ( 'NONE',  ( 2.924914550060624840, 2.500000000000000888, 0.000000000000000000 ) ) ;
#107738 = ORIENTED_EDGE ( 'NONE', *, *, #111158, .T. ) ;
#107739 = LINE ( 'NONE', #71574, #37581 ) ;
#107740 = CARTESIAN_POINT ( 'NONE',  ( 21.29974487139158512, -27.71228299555221142, 4.000000000000000000 ) ) ;
#107741 = ORIENTED_EDGE ( 'NONE', *, *, #16007, .F. ) ;
#107742 = EDGE_CURVE ( 'NONE', #76469, #63599, #99328, .T. ) ;
#107743 = EDGE_CURVE ( 'NONE', #33206, #47238, #102099, .T. ) ;
#107744 = DIRECTION ( 'NONE',  ( -0.7071067811865486830, 0.7071067811865464625, 0.000000000000000000 ) ) ;
#107745 = CARTESIAN_POINT ( 'NONE',  ( 33.18336038379622721, -2.130196079827426203, 7.949999999999996625 ) ) ;
#107746 = FACE_OUTER_BOUND ( 'NONE', #75271, .T. ) ;
#107747 = EDGE_LOOP ( 'NONE', ( #143482, #95897, #112962, #28182 ) ) ;
#107748 = EDGE_LOOP ( 'NONE', ( #101610, #29615, #5757, #86727 ) ) ;
#107749 = EDGE_CURVE ( 'NONE', #123709, #111380, #67475, .T. ) ;
#107750 = FACE_BOUND ( 'NONE', #102601, .T. ) ;
#107751 = EDGE_CURVE ( 'NONE', #2559, #66501, #13035, .T. ) ;
#107752 = FACE_OUTER_BOUND ( 'NONE', #55410, .T. ) ;
#107753 = CYLINDRICAL_SURFACE ( 'NONE', #21148, 0.5000000000000004441 ) ;
#107754 = CARTESIAN_POINT ( 'NONE',  ( -21.62762920772360786, 8.558752285115851066, 4.000000000000000000 ) ) ;
#107755 = PRESENTATION_STYLE_ASSIGNMENT (( #17200 ) ) ;
#107756 = CARTESIAN_POINT ( 'NONE',  ( 0.5685132242927012358, 4.584330080086930965E-16, 0.000000000000000000 ) ) ;
#107757 = PRESENTATION_STYLE_ASSIGNMENT (( #19344 ) ) ;
#107759 = ORIENTED_EDGE ( 'NONE', *, *, #126904, .T. ) ;
#107758 = VECTOR ( 'NONE', #123645, 1000.000000000000000 ) ;
#107760 = EDGE_LOOP ( 'NONE', ( #85643, #29390, #142723, #56700 ) ) ;
#107761 = ORIENTED_EDGE ( 'NONE', *, *, #48089, .T. ) ;
#107762 = COLOUR_RGB ( '', 0.08235294, 0.09019608, 0.10196078) ;
#107763 = VERTEX_POINT ( 'NONE', #101487 ) ;
#107764 = EDGE_CURVE ( 'NONE', #43048, #46174, #123277, .T. ) ;
#107765 = LINE ( 'NONE', #52682, #110350 ) ;
#107766 = DIRECTION ( 'NONE',  ( 1.000000000000000000, 0.000000000000000000, 0.000000000000000000 ) ) ;
#107767 = ORIENTED_EDGE ( 'NONE', *, *, #34508, .T. ) ;
#107768 = VECTOR ( 'NONE', #10672, 1000.000000000000000 ) ;
#107769 = DIRECTION ( 'NONE',  ( -1.000000000000000000, -1.224606353822377258E-16, -0.000000000000000000 ) ) ;
#107770 = CARTESIAN_POINT ( 'NONE',  ( 32.29387692260782217, 22.22500000000000142, 4.000000000000000000 ) ) ;
#107771 = CARTESIAN_POINT ( 'NONE',  ( -48.18398860626899705, 28.73617430169820608, 5.000000000000000000 ) ) ;
#107772 = LINE ( 'NONE', #72361, #6736 ) ;
#107773 = CARTESIAN_POINT ( 'NONE',  ( 1.320799999999990870, 1.617513596018363294E-16, 3.775643966265890494 ) ) ;
#107774 = ORIENTED_EDGE ( 'NONE', *, *, #108077, .T. ) ;
#107775 = LINE ( 'NONE', #41831, #26451 ) ;
#107776 = CARTESIAN_POINT ( 'NONE',  ( -2.510786437626908008, -27.52281430457053446, 5.000000000000000000 ) ) ;
#107777 = ORIENTED_EDGE ( 'NONE', *, *, #44690, .T. ) ;
#107778 = DIRECTION ( 'NONE',  ( -0.6830127018922180770, -0.6830127018922204085, -0.2588190451025213501 ) ) ;
#107779 = ORIENTED_EDGE ( 'NONE', *, *, #117251, .T. ) ;
#107780 = ORIENTED_EDGE ( 'NONE', *, *, #73165, .F. ) ;
#107781 = ORIENTED_EDGE ( 'NONE', *, *, #112277, .F. ) ;
#107782 = CARTESIAN_POINT ( 'NONE',  ( 60.37543019189810423, -5.291415217122920289, -3.055000000000001492 ) ) ;
#107783 = VERTEX_POINT ( 'NONE', #80481 ) ;
#107784 = ORIENTED_EDGE ( 'NONE', *, *, #4962, .F. ) ;
#107785 = VECTOR ( 'NONE', #64977, 1000.000000000000227 ) ;
#107786 = DIRECTION ( 'NONE',  ( 0.7071067811865487940, -0.7071067811865463515, 0.000000000000000000 ) ) ;
#107788 = EDGE_CURVE ( 'NONE', #55935, #124530, #124675, .T. ) ;
#107787 = VECTOR ( 'NONE', #21448, 1000.000000000000000 ) ;
#107789 = PLANE ( 'NONE',  #130714 ) ;
#107790 = CARTESIAN_POINT ( 'NONE',  ( 98.00043019189810423, -3.055000000000002380, 5.291415217122920289 ) ) ;
#107791 = CARTESIAN_POINT ( 'NONE',  ( -18.77004279457780811, 21.73644205237998506, 5.000000000000000888 ) ) ;
#107792 = AXIS2_PLACEMENT_3D ( 'NONE', #16721, #83426, #60999 ) ;
#107793 = ADVANCED_FACE ( 'NONE', ( #89895 ), #113072, .F. ) ;
#107794 = CARTESIAN_POINT ( 'NONE',  ( -60.18398860626900415, 28.73617430169829490, 5.000000000000000000 ) ) ;
#107795 = CARTESIAN_POINT ( 'NONE',  ( -0.3281693992235250046, -21.74070752338406365, 4.000000000000000000 ) ) ;
#107796 = AXIS2_PLACEMENT_3D ( 'NONE', #17122, #61390, #83844 ) ;
#107797 = CARTESIAN_POINT ( 'NONE',  ( 152.4000000000000057, -14.29000000000013593, 12.69999999999954632 ) ) ;
#107798 = ADVANCED_FACE ( 'NONE', ( #102233 ), #112381, .F. ) ;
#107799 = ADVANCED_FACE ( 'NONE', ( #132735 ), #73076, .T. ) ;
#107800 = DIRECTION ( 'NONE',  ( 0.7071067811865487940, 0.7071067811865463515, -0.000000000000000000 ) ) ;
#107801 = CARTESIAN_POINT ( 'NONE',  ( -34.42500000000001137, 2.977185695429387824, 5.000000000000000000 ) ) ;
#107802 = ORIENTED_EDGE ( 'NONE', *, *, #57619, .F. ) ;
#107803 = FACE_OUTER_BOUND ( 'NONE', #33262, .T. ) ;
#107804 = ORIENTED_EDGE ( 'NONE', *, *, #31398, .F. ) ;
#107805 = VERTEX_POINT ( 'NONE', #33427 ) ;
#107806 = EDGE_LOOP ( 'NONE', ( #32898, #12418, #79897, #18872 ) ) ;
#107807 = EDGE_LOOP ( 'NONE', ( #125254, #66975, #1512, #83150 ) ) ;
#107808 = DIRECTION ( 'NONE',  ( 0.000000000000000000, 0.9647414015272155474, -0.2631995976047525887 ) ) ;
#107809 = PLANE ( 'NONE',  #98830 ) ;
#107810 = ADVANCED_FACE ( 'NONE', ( #100784 ), #57312, .T. ) ;
#107811 = CARTESIAN_POINT ( 'NONE',  ( 1.369266385878517678, 0.000000000000000000, 0.000000000000000000 ) ) ;
#107812 = EDGE_CURVE ( 'NONE', #49576, #46218, #7256, .T. ) ;
#107813 = ORIENTED_EDGE ( 'NONE', *, *, #84383, .T. ) ;
#107814 = ORIENTED_EDGE ( 'NONE', *, *, #58973, .T. ) ;
#107815 = EDGE_CURVE ( 'NONE', #110351, #34779, #23190, .T. ) ;
#107816 = CARTESIAN_POINT ( 'NONE',  ( 5.374569808101886892, 6.871911579029510442, -3.967499999999998916 ) ) ;
#107817 = FILL_AREA_STYLE_COLOUR ( '', #129499 ) ;
#107818 = DIRECTION ( 'NONE',  ( -0.3543493200069162685, -0.000000000000000000, -0.9351131265310288487 ) ) ;
#107819 = DIRECTION ( 'NONE',  ( 0.000000000000000000, -1.000000000000000000, 0.000000000000000000 ) ) ;
#107820 = ORIENTED_EDGE ( 'NONE', *, *, #109794, .T. ) ;
#107821 = ORIENTED_EDGE ( 'NONE', *, *, #122611, .T. ) ;
#107822 = ORIENTED_EDGE ( 'NONE', *, *, #142907, .F. ) ;
#107823 = LINE ( 'NONE', #83994, #111216 ) ;
#107824 = CARTESIAN_POINT ( 'NONE',  ( -2.816011393730999401, 28.73617430169785436, 5.000000000000000000 ) ) ;
#107825 = EDGE_CURVE ( 'NONE', #129495, #22625, #12334, .T. ) ;
#107826 = PLANE ( 'NONE',  #114415 ) ;
#107827 = FACE_OUTER_BOUND ( 'NONE', #21558, .T. ) ;
#107828 = LINE ( 'NONE', #20828, #78165 ) ;
#107829 = DIRECTION ( 'NONE',  ( -1.000000000000000000, -0.000000000000000000, -0.000000000000000000 ) ) ;
#107830 = CARTESIAN_POINT ( 'NONE',  ( 32.81293019189809002, -1.637169565754159617, -6.110000000000001208 ) ) ;
#107831 = CARTESIAN_POINT ( 'NONE',  ( -45.48921356237309510, -27.52281430457087197, 5.000000000000000000 ) ) ;
#107832 = CARTESIAN_POINT ( 'NONE',  ( -18.18398860626898994, 28.73617430169800002, 5.000000000000000000 ) ) ;
#107833 = ORIENTED_EDGE ( 'NONE', *, *, #41024, .T. ) ;
#107834 = CARTESIAN_POINT ( 'NONE',  ( 34.92499999999998295, -6.183345613589489531, 4.500000000000000888 ) ) ;
#107835 = EDGE_CURVE ( 'NONE', #2581, #142459, #131737, .T. ) ;
#107836 = DIRECTION ( 'NONE',  ( 0.3543493200069162685, -0.000000000000000000, -0.9351131265310288487 ) ) ;
#107837 = EDGE_LOOP ( 'NONE', ( #74079, #24521, #101634, #33785 ) ) ;
#107838 = CARTESIAN_POINT ( 'NONE',  ( -21.70710678118638270, -18.74070752338409562, 5.000000000000000000 ) ) ;
#107840 = VERTEX_POINT ( 'NONE', #47867 ) ;
#107839 = CARTESIAN_POINT ( 'NONE',  ( 52.69985579144460530, -48.99436351328190398, -39.52330221398148069 ) ) ;
#107841 = CARTESIAN_POINT ( 'NONE',  ( 0.4000000000000001887, 0.000000000000000000, 1.249999999999969802 ) ) ;
#107842 = EDGE_CURVE ( 'NONE', #95326, #87449, #48546, .T. ) ;
#107843 = ORIENTED_EDGE ( 'NONE', *, *, #31680, .F. ) ;
#107845 = ADVANCED_FACE ( 'NONE', ( #136982 ), #58765, .F. ) ;
#107844 = CARTESIAN_POINT ( 'NONE',  ( 14.99999999999989519, -16.06887692260765377, 4.000000000000000000 ) ) ;
#107846 = VERTEX_POINT ( 'NONE', #4249 ) ;
#107847 = VERTEX_POINT ( 'NONE', #94874 ) ;
#107848 = EDGE_CURVE ( 'NONE', #58070, #108960, #139135, .T. ) ;
#107849 = VECTOR ( 'NONE', #126814, 999.9999999999998863 ) ;
#107850 = CARTESIAN_POINT ( 'NONE',  ( 124.6208603837962272, -6.884901960086286188, 3.974999999999997424 ) ) ;
#107851 = LINE ( 'NONE', #120143, #104037 ) ;
#107852 = CARTESIAN_POINT ( 'NONE',  ( -24.29974487139158867, -27.71228299555223273, 4.000000000000000000 ) ) ;
#107853 = CIRCLE ( 'NONE', #17535, 2.500000000000000888 ) ;
#107854 = DIRECTION ( 'NONE',  ( -0.3543493200069162685, -0.000000000000000000, -0.9351131265310288487 ) ) ;
#107855 = DIRECTION ( 'NONE',  ( 0.7071067811865486830, -0.7071067811865464625, -0.000000000000000000 ) ) ;
#107856 = DIRECTION ( 'NONE',  ( 0.6830127018922181881, 0.6830127018922202975, -0.2588190451025214056 ) ) ;
#107857 = CARTESIAN_POINT ( 'NONE',  ( 8.895833333333333925, 1.633150327867687324, -6.094999999999991758 ) ) ;
#107858 = CARTESIAN_POINT ( 'NONE',  ( 20.54123647476855652, 0.000000000000000000, 7.934999999999990727 ) ) ;
#107859 = DIRECTION ( 'NONE',  ( 0.7071067811865487940, -0.7071067811865463515, 0.000000000000000000 ) ) ;
#107860 = DIRECTION ( 'NONE',  ( -0.000000000000000000, -0.000000000000000000, 1.000000000000000000 ) ) ;
#107861 = ORIENTED_EDGE ( 'NONE', *, *, #20911, .F. ) ;
#107862 = ORIENTED_EDGE ( 'NONE', *, *, #32376, .F. ) ;
#107863 = DIRECTION ( 'NONE',  ( -0.000000000000000000, 0.3543493200069153248, 0.9351131265310292928 ) ) ;
#107864 = VERTEX_POINT ( 'NONE', #71033 ) ;
#107865 = VECTOR ( 'NONE', #106798, 1000.000000000000000 ) ;
#107866 = PLANE ( 'NONE',  #138289 ) ;
#107867 = LINE ( 'NONE', #64395, #138971 ) ;
#107868 = CARTESIAN_POINT ( 'NONE',  ( 128.5894344200537773, -52.00875322212549179, -39.86617647058817226 ) ) ;
#107869 = ORIENTED_EDGE ( 'NONE', *, *, #34369, .F. ) ;
#107870 = LINE ( 'NONE', #98452, #81266 ) ;
#107871 = CARTESIAN_POINT ( 'NONE',  ( 29.99451991528749417, 28.92564299267958816, 4.000000000000000000 ) ) ;
#107872 = LINE ( 'NONE', #52097, #58250 ) ;
#107873 = CARTESIAN_POINT ( 'NONE',  ( 0.01254890717039356708, -50.57777258831014677, 35.91905586107260007 ) ) ;
#107875 = VERTEX_POINT ( 'NONE', #71743 ) ;
#107874 = PLANE ( 'NONE',  #21983 ) ;
#107876 = CARTESIAN_POINT ( 'NONE',  ( 40.37499999999999289, 7.950000000000000178, 1.460391307983218535E-15 ) ) ;
#107877 = SURFACE_STYLE_FILL_AREA ( #52102 ) ;
#107878 = CYLINDRICAL_SURFACE ( 'NONE', #123407, 0.5000000000000004441 ) ;
#107879 = DIRECTION ( 'NONE',  ( -1.000000000000000000, -1.224606353822377258E-16, -0.000000000000000000 ) ) ;
#107880 = AXIS2_PLACEMENT_3D ( 'NONE', #110402, #35040, #45910 ) ;
#107881 = CARTESIAN_POINT ( 'NONE',  ( 58.16711163708901466, -46.44928942427405616, 35.85226645763361120 ) ) ;
#107882 = EDGE_LOOP ( 'NONE', ( #69140, #109396, #36923, #59125 ) ) ;
#107883 = ORIENTED_EDGE ( 'NONE', *, *, #28598, .F. ) ;
#107884 = ORIENTED_EDGE ( 'NONE', *, *, #5937, .F. ) ;
#107885 = VECTOR ( 'NONE', #46651, 999.9999999999998863 ) ;
#107886 = CARTESIAN_POINT ( 'NONE',  ( 102.8129301918981042, -1.637169565754159617, -6.110000000000001208 ) ) ;
#107887 = ORIENTED_EDGE ( 'NONE', *, *, #29306, .T. ) ;
#107888 = AXIS2_PLACEMENT_3D ( 'NONE', #39094, #105056, #16610 ) ;
#107889 = CARTESIAN_POINT ( 'NONE',  ( 128.1966263608613588, -51.41954113333839160, 38.53170190052058075 ) ) ;
#107890 = AXIS2_PLACEMENT_3D ( 'NONE', #107341, #67442, #76897 ) ;
#107891 = CARTESIAN_POINT ( 'NONE',  ( 84.66252705046289861, 7.949999999999998401, 1.460391307983218338E-15 ) ) ;
#107892 = ORIENTED_EDGE ( 'NONE', *, *, #87166, .F. ) ;
#107893 = CARTESIAN_POINT ( 'NONE',  ( 22.85159235450332105, 9.902892378096218942E-16, 0.000000000000000000 ) ) ;
#107894 = FACE_BOUND ( 'NONE', #44061, .T. ) ;
#107895 = CARTESIAN_POINT ( 'NONE',  ( 97.18293019189810877, -1.637169565754158951, -6.109999999999998543 ) ) ;
#107896 = ORIENTED_EDGE ( 'NONE', *, *, #54310, .T. ) ;
#107897 = DIRECTION ( 'NONE',  ( -1.000000000000000000, -1.224606353822377258E-16, -0.000000000000000000 ) ) ;
#107898 = CARTESIAN_POINT ( 'NONE',  ( 5.999999999999955591, -21.84840872380824095, 2.849755605029621996 ) ) ;
#107899 = CARTESIAN_POINT ( 'NONE',  ( 19.05000000000000071, 3.174999999999997158, 5.000000000000000000 ) ) ;
#107900 = PLANE ( 'NONE',  #9113 ) ;
#107901 = ORIENTED_EDGE ( 'NONE', *, *, #4508, .F. ) ;
#107902 = VERTEX_POINT ( 'NONE', #49289 ) ;
#107903 = EDGE_CURVE ( 'NONE', #47888, #65959, #86923, .T. ) ;
#107904 = VERTEX_POINT ( 'NONE', #37688 ) ;
#107905 = CARTESIAN_POINT ( 'NONE',  ( 27.60486233187505078, 21.75929247661550647, 21.32995629748180377 ) ) ;
#107906 = ADVANCED_FACE ( 'NONE', ( #115903 ), #84059, .F. ) ;
#107907 = PLANE ( 'NONE',  #98664 ) ;
#107908 = CARTESIAN_POINT ( 'NONE',  ( 20.33790314143522338, -6.871911579029513106, -3.967499999999993587 ) ) ;
#107909 = FACE_OUTER_BOUND ( 'NONE', #9684, .T. ) ;
#107910 = DIRECTION ( 'NONE',  ( -0.7071067811865486830, -0.7071067811865464625, 0.000000000000000000 ) ) ;
#107911 = FILL_AREA_STYLE ('',( #127563 ) ) ;
#107912 = ORIENTED_EDGE ( 'NONE', *, *, #137910, .T. ) ;
#107914 = VERTEX_POINT ( 'NONE', #125401 ) ;
#107913 = ADVANCED_FACE ( 'NONE', ( #92741 ), #5718, .T. ) ;
#107915 = PLANE ( 'NONE',  #1598 ) ;
#107916 = ORIENTED_EDGE ( 'NONE', *, *, #5579, .T. ) ;
#107917 = ORIENTED_EDGE ( 'NONE', *, *, #56944, .F. ) ;
#107918 = VECTOR ( 'NONE', #48354, 1000.000000000000227 ) ;
#107919 = EDGE_CURVE ( 'NONE', #81042, #137586, #81928, .T. ) ;
#107920 = DIRECTION ( 'NONE',  ( -0.000000000000000000, 0.000000000000000000, 1.000000000000000000 ) ) ;
#107921 = CARTESIAN_POINT ( 'NONE',  ( 59.99451991528749772, 28.92564299267980132, 4.000000000000000000 ) ) ;
#107922 = ORIENTED_EDGE ( 'NONE', *, *, #12758, .T. ) ;
#107923 = CARTESIAN_POINT ( 'NONE',  ( 56.27083333333332860, -7.949999999999998401, -2.130196079827426203 ) ) ;
#107924 = CARTESIAN_POINT ( 'NONE',  ( -17.52663903635773934, -5.240707523384225297, 16.25846745537491600 ) ) ;
#107925 = VECTOR ( 'NONE', #3882, 999.9999999999998863 ) ;
#107926 = CARTESIAN_POINT ( 'NONE',  ( 24.91272823266826109, 2.053671025133813277, 5.000000000000000000 ) ) ;
#107927 = EDGE_CURVE ( 'NONE', #139716, #138830, #83321, .T. ) ;
#107928 = PLANE ( 'NONE',  #81448 ) ;
#107929 = EDGE_LOOP ( 'NONE', ( #101379, #119452, #59250, #16799 ) ) ;
#107930 = SURFACE_SIDE_STYLE ('',( #8598 ) ) ;
#107931 = EDGE_LOOP ( 'NONE', ( #75895, #26409, #91499, #23664 ) ) ;
#107932 = CARTESIAN_POINT ( 'NONE',  ( 25.39999999999999147, 4.671400280653048576, -6.417465358227912198 ) ) ;
#107933 = DIRECTION ( 'NONE',  ( 0.7071067811865487940, -0.7071067811865463515, 0.000000000000000000 ) ) ;
#107934 = ORIENTED_EDGE ( 'NONE', *, *, #3947, .T. ) ;
#107935 = CARTESIAN_POINT ( 'NONE',  ( -45.18398860626900415, 28.73617430169818832, 5.000000000000000000 ) ) ;
#107936 = EDGE_LOOP ( 'NONE', ( #16871, #88646, #80041, #37609 ) ) ;
#107937 = CARTESIAN_POINT ( 'NONE',  ( 29.99999999999979039, -13.97847968911257865, -0.1324546996126097498 ) ) ;
#107938 = VERTEX_POINT ( 'NONE', #61588 ) ;
#107939 = ORIENTED_EDGE ( 'NONE', *, *, #93875, .F. ) ;
#107940 = ORIENTED_EDGE ( 'NONE', *, *, #13577, .F. ) ;
#107941 = VECTOR ( 'NONE', #47580, 1000.000000000000000 ) ;
#107942 = CARTESIAN_POINT ( 'NONE',  ( 30.97459685856477662, 1.637169565754164280, -6.109999999999996767 ) ) ;
#107943 = CARTESIAN_POINT ( 'NONE',  ( 174.7500000000000000, 7.919999999999947526, 19.12499999999998224 ) ) ;
#107944 = CONICAL_SURFACE ( 'NONE', #64015, 2.500000000000000444, 0.9599310885968830309 ) ;
#107945 = CARTESIAN_POINT ( 'NONE',  ( 125.1254301918981184, 5.291415217122919401, 3.055000000000002824 ) ) ;
#107946 = CARTESIAN_POINT ( 'NONE',  ( 4.600000000000001421, 9.521314400968980422E-16, 0.000000000000000000 ) ) ;
#107947 = EDGE_CURVE ( 'NONE', #65885, #62041, #17331, .T. ) ;
#107948 = DIRECTION ( 'NONE',  ( 0.7071067811865487940, 0.7071067811865463515, 0.000000000000000000 ) ) ;
#107949 = CARTESIAN_POINT ( 'NONE',  ( 42.48921356237308800, -27.52281430457085065, 5.000000000000000000 ) ) ;
#107950 = EDGE_CURVE ( 'NONE', #30447, #23039, #92033, .T. ) ;
#107951 = ADVANCED_FACE ( 'NONE', ( #81191 ), #26087, .T. ) ;
#107952 = DIRECTION ( 'NONE',  ( -0.000000000000000000, 0.3543493200069153248, 0.9351131265310292928 ) ) ;
#107953 = CARTESIAN_POINT ( 'NONE',  ( 44.99451991528749772, 28.92564299267969474, 4.000000000000000000 ) ) ;
#107954 = DIRECTION ( 'NONE',  ( 0.6830127018922180770, -0.6830127018922204085, -0.2588190451025213501 ) ) ;
#107955 = ORIENTED_EDGE ( 'NONE', *, *, #17735, .F. ) ;
#107956 = ORIENTED_EDGE ( 'NONE', *, *, #105538, .T. ) ;
#107957 = ORIENTED_EDGE ( 'NONE', *, *, #68612, .T. ) ;
#107958 = ORIENTED_EDGE ( 'NONE', *, *, #113959, .T. ) ;
#107959 = CARTESIAN_POINT ( 'NONE',  ( -0.1731940554707888380, 1.320799999999991092, 4.000000000000000000 ) ) ;
#107960 = ORIENTED_EDGE ( 'NONE', *, *, #89308, .F. ) ;
#107961 = EDGE_CURVE ( 'NONE', #28405, #139749, #6402, .T. ) ;
#107962 = ORIENTED_EDGE ( 'NONE', *, *, #63822, .F. ) ;
#107963 = FACE_OUTER_BOUND ( 'NONE', #43999, .T. ) ;
#107964 = FACE_OUTER_BOUND ( 'NONE', #136441, .T. ) ;
#107965 = ADVANCED_FACE ( 'NONE', ( #26783 ), #59453, .F. ) ;
#107966 = EDGE_CURVE ( 'NONE', #65370, #101800, #114494, .T. ) ;
#107967 = LINE ( 'NONE', #130495, #32355 ) ;
#107968 = EDGE_LOOP ( 'NONE', ( #82525, #102875, #143077, #97028, #59134 ) ) ;
#107969 = DIRECTION ( 'NONE',  ( 0.6830127018922180770, -0.6830127018922204085, -0.2588190451025213501 ) ) ;
#107970 = ORIENTED_EDGE ( 'NONE', *, *, #53483, .T. ) ;
#107971 = VECTOR ( 'NONE', #127368, 999.9999999999998863 ) ;
#107973 = DIRECTION ( 'NONE',  ( -0.7071067811865486830, -0.7071067811865464625, -0.000000000000000000 ) ) ;
#107972 = VECTOR ( 'NONE', #205, 1000.000000000000000 ) ;
#107974 = DIRECTION ( 'NONE',  ( 0.7071067811865487940, 0.7071067811865463515, -0.000000000000000000 ) ) ;
#107975 = VECTOR ( 'NONE', #114278, 1000.000000000000000 ) ;
#107976 = EDGE_CURVE ( 'NONE', #32821, #13806, #106719, .T. ) ;
#107977 = CARTESIAN_POINT ( 'NONE',  ( 5.317069808101885897, -2.126176841940956130, 7.934999999999991616 ) ) ;
#107978 = ORIENTED_EDGE ( 'NONE', *, *, #71081, .F. ) ;
#107980 = VECTOR ( 'NONE', #105531, 1000.000000000000000 ) ;
#107979 = CARTESIAN_POINT ( 'NONE',  ( 96.45376352523145158, -6.109999999999999432, -3.741295971395163529E-16 ) ) ;
#107981 = EDGE_CURVE ( 'NONE', #134825, #45274, #126794, .T. ) ;
#107982 = CARTESIAN_POINT ( 'NONE',  ( 29.99999999999979039, -8.151047557385043163, -8.977947279169871564 ) ) ;
#107983 = DIRECTION ( 'NONE',  ( -0.7071067811865486830, -0.7071067811865464625, 0.000000000000000000 ) ) ;
#107984 = DIRECTION ( 'NONE',  ( -0.6830127018922181881, 0.6830127018922202975, -0.2588190451025214056 ) ) ;
#107985 = ORIENTED_EDGE ( 'NONE', *, *, #64110, .T. ) ;
#107986 = ORIENTED_EDGE ( 'NONE', *, *, #97188, .T. ) ;
#107987 = LINE ( 'NONE', #76115, #63558 ) ;
#107988 = ORIENTED_EDGE ( 'NONE', *, *, #93098, .F. ) ;
#107989 = CARTESIAN_POINT ( 'NONE',  ( -13.49999999999990052, -13.91253812416061386, 4.000000000000000000 ) ) ;
#107990 = CARTESIAN_POINT ( 'NONE',  ( -34.92500000000001137, -1.545334305399999275, 14.00746825007385610 ) ) ;
#107991 = AXIS2_PLACEMENT_3D ( 'NONE', #67251, #66541, #33232 ) ;
#107993 = EDGE_CURVE ( 'NONE', #13678, #35612, #40535, .T. ) ;
#107992 = CARTESIAN_POINT ( 'NONE',  ( 30.18398860626900060, 28.73617430169808173, 5.000000000000000000 ) ) ;
#107994 = DIRECTION ( 'NONE',  ( -0.7071067811865486830, 0.7071067811865464625, 0.000000000000000000 ) ) ;
#107995 = CARTESIAN_POINT ( 'NONE',  ( 184.1499999999998067, -50.22575108203221816, -35.38524182945423746 ) ) ;
#107996 = ORIENTED_EDGE ( 'NONE', *, *, #132909, .T. ) ;
#107997 = DIRECTION ( 'NONE',  ( 0.7071067811865487940, 0.7071067811865463515, 0.000000000000000000 ) ) ;
#107998 = CARTESIAN_POINT ( 'NONE',  ( 19.04500000000000881, 3.130000000000007887, 0.000000000000000000 ) ) ;
#107999 = CARTESIAN_POINT ( 'NONE',  ( -4.828169399223496860, 21.75929247661549581, 4.000000000000000000 ) ) ;
#108000 = VERTEX_POINT ( 'NONE', #143219 ) ;
#108001 = FACE_OUTER_BOUND ( 'NONE', #100806, .T. ) ;
#108002 = CARTESIAN_POINT ( 'NONE',  ( -2.816011393730999401, 28.73617430169785436, 5.000000000000000000 ) ) ;
#108003 = VERTEX_POINT ( 'NONE', #22827 ) ;
#108005 = ORIENTED_EDGE ( 'NONE', *, *, #23196, .F. ) ;
#108004 = CARTESIAN_POINT ( 'NONE',  ( -75.48921356237309510, -27.52281430457107803, 5.000000000000000000 ) ) ;
#108006 = ORIENTED_EDGE ( 'NONE', *, *, #130799, .T. ) ;
#108007 = CARTESIAN_POINT ( 'NONE',  ( 0.2569208697893812232, 0.4000000000000001332, -2.015694669338588429 ) ) ;
#108009 = EDGE_CURVE ( 'NONE', #123934, #138063, #10538, .T. ) ;
#108008 = DIRECTION ( 'NONE',  ( -0.000000000000000000, 0.3543493200069152138, -0.9351131265310292928 ) ) ;
#108010 = ORIENTED_EDGE ( 'NONE', *, *, #93606, .F. ) ;
#108011 = FACE_OUTER_BOUND ( 'NONE', #96347, .T. ) ;
#108012 = ADVANCED_FACE ( 'NONE', ( #109874 ), #132383, .F. ) ;
#108013 = DIRECTION ( 'NONE',  ( 1.000000000000000000, 0.000000000000000000, 0.000000000000000000 ) ) ;
#108014 = EDGE_CURVE ( 'NONE', #39257, #141363, #55514, .T. ) ;
#108015 = AXIS2_PLACEMENT_3D ( 'NONE', #20981, #108676, #42774 ) ;
#108016 = CARTESIAN_POINT ( 'NONE',  ( 26.86500426248361606, 3.759292476615681888, 15.36553568819720006 ) ) ;
#108017 = DIRECTION ( 'NONE',  ( -0.3543493200069162685, -0.000000000000000000, -0.9351131265310288487 ) ) ;
#108018 = CARTESIAN_POINT ( 'NONE',  ( 0.1600000000000025846, -3.262421210207534283, -7.241152424009429822 ) ) ;
#108019 = LINE ( 'NONE', #53696, #134668 ) ;
#108020 = CARTESIAN_POINT ( 'NONE',  ( 47.66666666666666430, 6.884901960086285300, 3.975000000000003642 ) ) ;
#108021 = FACE_OUTER_BOUND ( 'NONE', #138386, .T. ) ;
#108022 = CARTESIAN_POINT ( 'NONE',  ( -20.99999999999984368, 14.96639925780210767, 5.000000000000000000 ) ) ;
#108024 = VECTOR ( 'NONE', #128440, 1000.000000000000227 ) ;
#108023 = DIRECTION ( 'NONE',  ( -0.000000000000000000, -1.000000000000000000, -0.000000000000000000 ) ) ;
#108025 = DIRECTION ( 'NONE',  ( -0.7071067811865486830, -0.7071067811865464625, 0.000000000000000000 ) ) ;
#108026 = ADVANCED_FACE ( 'NONE', ( #43211 ), #33077, .T. ) ;
#108027 = DIRECTION ( 'NONE',  ( 0.7071067811865487940, 0.7071067811865463515, 0.000000000000000000 ) ) ;
#108028 = ORIENTED_EDGE ( 'NONE', *, *, #83176, .T. ) ;
#108029 = ORIENTED_EDGE ( 'NONE', *, *, #68268, .F. ) ;
#108030 = VERTEX_POINT ( 'NONE', #45373 ) ;
#108031 = CARTESIAN_POINT ( 'NONE',  ( 107.4583333333333428, 3.974999999999997424, 6.884901960086288852 ) ) ;
#108032 = ORIENTED_EDGE ( 'NONE', *, *, #23391, .F. ) ;
#108033 = EDGE_LOOP ( 'NONE', ( #101354, #9973, #86748, #53062 ) ) ;
#108034 = EDGE_LOOP ( 'NONE', ( #72949, #48942, #50993, #71444 ) ) ;
#108035 = VECTOR ( 'NONE', #63348, 1000.000000000000227 ) ;
#108036 = DIRECTION ( 'NONE',  ( 0.000000000000000000, -1.000000000000000000, 0.000000000000000000 ) ) ;
#108037 = CARTESIAN_POINT ( 'NONE',  ( 34.92190055902133849, 21.78725130426366974, 4.173570450635243567 ) ) ;
#108038 = EDGE_LOOP ( 'NONE', ( #10986, #81810, #48031, #105489 ) ) ;
#108039 = DIRECTION ( 'NONE',  ( 0.7071067811865487940, 0.7071067811865463515, -0.000000000000000000 ) ) ;
#108040 = PLANE ( 'NONE',  #71856 ) ;
#108042 = AXIS2_PLACEMENT_3D ( 'NONE', #66614, #64457, #8594 ) ;
#108041 = DIRECTION ( 'NONE',  ( -0.000000000000000000, 0.000000000000000000, 1.000000000000000000 ) ) ;
#108043 = DIRECTION ( 'NONE',  ( -0.7071067811865486830, -0.7071067811865464625, -0.000000000000000000 ) ) ;
#108044 = CARTESIAN_POINT ( 'NONE',  ( 102.6670968585647756, -3.055000000000000160, -5.291415217122921177 ) ) ;
#108045 = ORIENTED_EDGE ( 'NONE', *, *, #30090, .T. ) ;
#108046 = CARTESIAN_POINT ( 'NONE',  ( 15.20840764549667767, 9.139736423841732040E-16, 0.000000000000000000 ) ) ;
#108047 = CARTESIAN_POINT ( 'NONE',  ( -34.92500000000001137, 22.22500000000000142, 4.000000000000000000 ) ) ;
#108048 = CARTESIAN_POINT ( 'NONE',  ( 0.000000000000000000, 0.000000000000000000, 5.000000000000000000 ) ) ;
#108049 = DIRECTION ( 'NONE',  ( 0.000000000000000000, -1.000000000000000000, 0.000000000000000000 ) ) ;
#108050 = CARTESIAN_POINT ( 'NONE',  ( 32.67183060077624646, -6.740707523384209310, 4.000000000000000000 ) ) ;
#108051 = CARTESIAN_POINT ( 'NONE',  ( -23.99451991528749062, 28.92564299267954908, 4.000000000000000000 ) ) ;
#108052 = CARTESIAN_POINT ( 'NONE',  ( 28.95419371712955225, 6.884901960086283523, 3.975000000000002753 ) ) ;
#108053 = AXIS2_PLACEMENT_3D ( 'NONE', #8105, #142933, #130656 ) ;
#108054 = CARTESIAN_POINT ( 'NONE',  ( -9.524999999999998579, -4.870000000000014317, -40.00000000000000000 ) ) ;
#108055 = VERTEX_POINT ( 'NONE', #128257 ) ;
#108056 = EDGE_LOOP ( 'NONE', ( #262, #112828, #111401, #37266 ) ) ;
#108057 = CARTESIAN_POINT ( 'NONE',  ( 27.24999999999999645, -9.735942053221458872E-16, 7.950000000000000178 ) ) ;
#108058 = ORIENTED_EDGE ( 'NONE', *, *, #142024, .F. ) ;
#108059 = CARTESIAN_POINT ( 'NONE',  ( 22.49999999999984013, 5.696342897626518464, -7.587980461218345241 ) ) ;
#108060 = EDGE_CURVE ( 'NONE', #141725, #61971, #66388, .T. ) ;
#108061 = CARTESIAN_POINT ( 'NONE',  ( -23.99451991528749062, 28.92564299267954908, 4.000000000000000000 ) ) ;
#108062 = DIRECTION ( 'NONE',  ( 1.000000000000000000, 0.000000000000000000, 0.000000000000000000 ) ) ;
#108063 = PLANE ( 'NONE',  #42295 ) ;
#108064 = CARTESIAN_POINT ( 'NONE',  ( -32.39513766812459750, 21.75929247661549226, 21.32995629748193878 ) ) ;
#108065 = CARTESIAN_POINT ( 'NONE',  ( 125.7662635252314658, 4.472830434245839371, -4.472830434245838482 ) ) ;
#108066 = ORIENTED_EDGE ( 'NONE', *, *, #75121, .F. ) ;
#108067 = DIRECTION ( 'NONE',  ( -1.000000000000000000, -1.224606353822377258E-16, -0.000000000000000000 ) ) ;
#108068 = ORIENTED_EDGE ( 'NONE', *, *, #115211, .F. ) ;
#108069 = PLANE ( 'NONE',  #29998 ) ;
#108070 = CARTESIAN_POINT ( 'NONE',  ( -22.49999999999984723, 16.77039438581777375, 0.4657186855308243500 ) ) ;
#108071 = LINE ( 'NONE', #117531, #41771 ) ;
#108072 = EDGE_CURVE ( 'NONE', #97559, #25402, #62289, .T. ) ;
#108073 = DIRECTION ( 'NONE',  ( -0.000000000000000000, -0.3543493200069152693, 0.9351131265310292928 ) ) ;
#108074 = EDGE_LOOP ( 'NONE', ( #80673, #113639, #79878, #104799 ) ) ;
#108075 = AXIS2_PLACEMENT_3D ( 'NONE', #20551, #132219, #131486 ) ;
#108076 = CARTESIAN_POINT ( 'NONE',  ( 44.91709685856476142, 3.054999999999998828, 5.291415217122922066 ) ) ;
#108077 = EDGE_CURVE ( 'NONE', #90471, #7602, #99704, .T. ) ;
#108078 = EDGE_LOOP ( 'NONE', ( #26022, #113245, #136861, #5557 ) ) ;
#108079 = PLANE ( 'NONE',  #100332 ) ;
#108080 = CARTESIAN_POINT ( 'NONE',  ( -34.49999999999976552, 3.054329344830908344, 4.994342998332172101 ) ) ;
#108081 = DIRECTION ( 'NONE',  ( -0.7071067811865486830, -0.7071067811865464625, 0.000000000000000000 ) ) ;
#108082 = DIRECTION ( 'NONE',  ( -0.7071067811865486830, 0.7071067811865464625, 0.000000000000000000 ) ) ;
#108083 = VECTOR ( 'NONE', #10405, 1000.000000000000000 ) ;
#108085 = EDGE_CURVE ( 'NONE', #53550, #94406, #117335, .T. ) ;
#108084 = AXIS2_PLACEMENT_3D ( 'NONE', #2169, #49324, #47213 ) ;
#108086 = EDGE_CURVE ( 'NONE', #135769, #81079, #111287, .T. ) ;
#108087 = AXIS2_PLACEMENT_3D ( 'NONE', #133941, #105566, #28761 ) ;
#108088 = CARTESIAN_POINT ( 'NONE',  ( 38.99543019189812298, 5.291415217122916737, 3.055000000000001936 ) ) ;
#108089 = ORIENTED_EDGE ( 'NONE', *, *, #115502, .T. ) ;
#108090 = EDGE_CURVE ( 'NONE', #35748, #63769, #65711, .T. ) ;
#108091 = VECTOR ( 'NONE', #43381, 1000.000000000000000 ) ;
#108092 = CARTESIAN_POINT ( 'NONE',  ( 45.48921356237309510, -27.52281430457087197, 5.000000000000000000 ) ) ;
#108093 = ORIENTED_EDGE ( 'NONE', *, *, #116529, .T. ) ;
#108094 = VERTEX_POINT ( 'NONE', #121456 ) ;
#108095 = VECTOR ( 'NONE', #114683, 1000.000000000000000 ) ;
#108096 = ORIENTED_EDGE ( 'NONE', *, *, #64689, .T. ) ;
#108097 = EDGE_CURVE ( 'NONE', #106517, #103136, #43919, .T. ) ;
#108098 = FACE_OUTER_BOUND ( 'NONE', #72751, .T. ) ;
#108099 = EDGE_LOOP ( 'NONE', ( #111054, #60080, #32420, #122268 ) ) ;
#108100 = CARTESIAN_POINT ( 'NONE',  ( -23.99999999999982236, 14.58746187583909837, 4.000000000000000000 ) ) ;
#108101 = CARTESIAN_POINT ( 'NONE',  ( -25.49999999999981881, -10.91253812416064761, 4.000000000000000000 ) ) ;
#108102 = ADVANCED_FACE ( 'NONE', ( #44669 ), #7866, .T. ) ;
#108103 = PLANE ( 'NONE',  #97433 ) ;
#108104 = FACE_BOUND ( 'NONE', #81096, .T. ) ;
#108105 = ORIENTED_EDGE ( 'NONE', *, *, #30345, .F. ) ;
#108106 = CARTESIAN_POINT ( 'NONE',  ( 153.4000000000000057, -16.48000000000005016, 33.92499999999998295 ) ) ;
#108107 = FACE_OUTER_BOUND ( 'NONE', #28211, .T. ) ;
#108108 = DIRECTION ( 'NONE',  ( 0.000000000000000000, 0.000000000000000000, -1.000000000000000000 ) ) ;
#108109 = ORIENTED_EDGE ( 'NONE', *, *, #56944, .T. ) ;
#108110 = FACE_OUTER_BOUND ( 'NONE', #41533, .T. ) ;
#108111 = ORIENTED_EDGE ( 'NONE', *, *, #69548, .F. ) ;
#108112 = VECTOR ( 'NONE', #126527, 1000.000000000000000 ) ;
#108114 = VERTEX_POINT ( 'NONE', #29620 ) ;
#108113 = EDGE_CURVE ( 'NONE', #18835, #65082, #84735, .T. ) ;
#108115 = PLANE ( 'NONE',  #67995 ) ;
#108116 = EDGE_LOOP ( 'NONE', ( #133936, #112276, #69201, #73993 ) ) ;
#108117 = CARTESIAN_POINT ( 'NONE',  ( 54.59959685856476597, -6.109999999999997655, -1.637169565754160283 ) ) ;
#108118 = AXIS2_PLACEMENT_3D ( 'NONE', #108504, #8473, #96916 ) ;
#108119 = ORIENTED_EDGE ( 'NONE', *, *, #60039, .F. ) ;
#108120 = CARTESIAN_POINT ( 'NONE',  ( -34.42500000000001137, 0.000000000000000000, 0.000000000000000000 ) ) ;
#108121 = EDGE_CURVE ( 'NONE', #20507, #103353, #73864, .T. ) ;
#108122 = ORIENTED_EDGE ( 'NONE', *, *, #48089, .F. ) ;
#108123 =( NAMED_UNIT ( * ) PLANE_ANGLE_UNIT ( ) SI_UNIT ( $, .RADIAN. ) );
#108124 = CARTESIAN_POINT ( 'NONE',  ( 10.06000000000000050, 9.521314400968980422E-16, 0.000000000000000000 ) ) ;
#108125 = CIRCLE ( 'NONE', #135900, 6.350000000000001421 ) ;
#108126 = ADVANCED_FACE ( 'NONE', ( #96285 ), #140529, .F. ) ;
#108127 = CARTESIAN_POINT ( 'NONE',  ( -69.18398860626899705, 28.73617430169835529, 5.000000000000000000 ) ) ;
#108128 = CARTESIAN_POINT ( 'NONE',  ( 2.207106781186530586, -11.24070752338416845, 5.000000000000000000 ) ) ;
#108129 = CARTESIAN_POINT ( 'NONE',  ( 25.51290636584444016, -22.22500000000000142, -17.90218200959884953 ) ) ;
#108130 = EDGE_CURVE ( 'NONE', #5968, #97631, #3005, .T. ) ;
#108131 = DIRECTION ( 'NONE',  ( 0.7071067811865486830, -0.7071067811865464625, -0.000000000000000000 ) ) ;
#108132 = LINE ( 'NONE', #10957, #13901 ) ;
#108133 = VERTEX_POINT ( 'NONE', #92379 ) ;
#108134 = VECTOR ( 'NONE', #123797, 1000.000000000000000 ) ;
#108135 = ORIENTED_EDGE ( 'NONE', *, *, #139176, .F. ) ;
#108136 = LINE ( 'NONE', #52356, #77490 ) ;
#108137 = DIRECTION ( 'NONE',  ( -0.000000000000000000, 0.000000000000000000, 1.000000000000000000 ) ) ;
#108138 = ORIENTED_EDGE ( 'NONE', *, *, #110063, .T. ) ;
#108139 = EDGE_CURVE ( 'NONE', #109145, #78583, #103267, .T. ) ;
#108140 = EDGE_LOOP ( 'NONE', ( #44694, #70430, #79863, #28985 ) ) ;
#108141 = ORIENTED_EDGE ( 'NONE', *, *, #111628, .T. ) ;
#108142 = CARTESIAN_POINT ( 'NONE',  ( -33.04687264925814816, -22.22500000000000142, 4.288307338716745853 ) ) ;
#108143 = CYLINDRICAL_SURFACE ( 'NONE', #3892, 0.5000000000000004441 ) ;
#108144 = DIRECTION ( 'NONE',  ( 0.7071067811865487940, 0.7071067811865463515, 0.000000000000000000 ) ) ;
#108145 = ORIENTED_EDGE ( 'NONE', *, *, #21804, .T. ) ;
#108146 = CARTESIAN_POINT ( 'NONE',  ( -23.99999999999982592, 4.384688058510544550, -7.090945410444739139 ) ) ;
#108147 = CARTESIAN_POINT ( 'NONE',  ( 14.79623647476855375, 7.934999999999990727, -1.457635852685135314E-15 ) ) ;
#108148 = ORIENTED_EDGE ( 'NONE', *, *, #75523, .F. ) ;
#108149 = CARTESIAN_POINT ( 'NONE',  ( 121.5370968585647802, -3.054999999999999272, -5.291415217122919401 ) ) ;
#108150 = VECTOR ( 'NONE', #18003, 1000.000000000000000 ) ;
#108151 = ADVANCED_FACE ( 'NONE', ( #91005 ), #89546, .T. ) ;
#108152 = LINE ( 'NONE', #109611, #69739 ) ;
#108153 = DIRECTION ( 'NONE',  ( 0.7071067811865486830, -0.7071067811865464625, -0.000000000000000000 ) ) ;
#108155 = EDGE_LOOP ( 'NONE', ( #133460, #86042, #77562, #50818 ) ) ;
#108154 = FACE_OUTER_BOUND ( 'NONE', #21052, .T. ) ;
#108156 = CARTESIAN_POINT ( 'NONE',  ( 67.01669371712957002, 7.950000000000000178, -2.130196079827421318 ) ) ;
#108157 = ORIENTED_EDGE ( 'NONE', *, *, #10527, .F. ) ;
#108158 = CARTESIAN_POINT ( 'NONE',  ( 76.49586038379621300, -3.974999999999998312, -6.884901960086286188 ) ) ;
#108159 = EDGE_CURVE ( 'NONE', #28445, #52993, #12685, .T. ) ;
#108160 = LINE ( 'NONE', #40810, #51599 ) ;
#108161 = DIRECTION ( 'NONE',  ( 0.3543493200069162685, -0.000000000000000000, -0.9351131265310288487 ) ) ;
#108162 = ORIENTED_EDGE ( 'NONE', *, *, #87561, .T. ) ;
#108163 = AXIS2_PLACEMENT_3D ( 'NONE', #99677, #353, #111261 ) ;
#108164 = DIRECTION ( 'NONE',  ( 0.7071067811865487940, 0.7071067811865463515, 0.000000000000000000 ) ) ;
#108165 = LINE ( 'NONE', #65448, #39783 ) ;
#108166 = VERTEX_POINT ( 'NONE', #56956 ) ;
#108167 = CARTESIAN_POINT ( 'NONE',  ( -48.48921356237309510, -27.52281430457089328, 5.000000000000000000 ) ) ;
#108168 = DIRECTION ( 'NONE',  ( 0.000000000000000000, -1.000000000000000000, 0.000000000000000000 ) ) ;
#108169 = ORIENTED_EDGE ( 'NONE', *, *, #20302, .T. ) ;
#108170 = CARTESIAN_POINT ( 'NONE',  ( 4.375000000000000000, -6.094999999999989981, 3.732111120401553285E-16 ) ) ;
#108171 = AXIS2_PLACEMENT_3D ( 'NONE', #136654, #1130, #45408 ) ;
#108172 = DIRECTION ( 'NONE',  ( -0.7071067811865487940, 0.7071067811865463515, 0.000000000000000000 ) ) ;
#108173 = VERTEX_POINT ( 'NONE', #101852 ) ;
#108174 = ORIENTED_EDGE ( 'NONE', *, *, #57935, .T. ) ;
#108175 = DIRECTION ( 'NONE',  ( 0.6830127018922181881, 0.6830127018922202975, -0.2588190451025214056 ) ) ;
#108176 = DIRECTION ( 'NONE',  ( 1.000000000000000000, 1.224606353822377258E-16, 0.000000000000000000 ) ) ;
#108177 = VECTOR ( 'NONE', #142055, 1000.000000000000000 ) ;
#108178 = VECTOR ( 'NONE', #129343, 999.9999999999998863 ) ;
#108179 = CARTESIAN_POINT ( 'NONE',  ( 13.68706980810188334, -2.126176841940956130, 7.934999999999991616 ) ) ;
#108180 = LINE ( 'NONE', #21207, #129233 ) ;
#108181 = ADVANCED_FACE ( 'NONE', ( #133776 ), #57669, .F. ) ;
#108182 = VECTOR ( 'NONE', #1448, 1000.000000000000000 ) ;
#108183 = CARTESIAN_POINT ( 'NONE',  ( -72.29974487139158157, -27.71228299555256669, 4.000000000000000000 ) ) ;
#108184 = CARTESIAN_POINT ( 'NONE',  ( 18.18398860626898994, 28.73617430169800002, 5.000000000000000000 ) ) ;
#108185 = ORIENTED_EDGE ( 'NONE', *, *, #79973, .F. ) ;
#108186 = PLANE ( 'NONE',  #97453 ) ;
#108187 = LINE ( 'NONE', #64724, #116109 ) ;
#108188 = LINE ( 'NONE', #84370, #23868 ) ;
#108189 = VECTOR ( 'NONE', #127359, 1000.000000000000227 ) ;
#108190 = CARTESIAN_POINT ( 'NONE',  ( 126.6275873549815003, -6.299348860240304937, -2.637261474849121878 ) ) ;
#108191 = CARTESIAN_POINT ( 'NONE',  ( 37.97459685856477307, 1.637169565754164280, -6.109999999999997655 ) ) ;
#108192 = CARTESIAN_POINT ( 'NONE',  ( -20.20710678118639692, -20.24070752338406720, 5.000000000000000000 ) ) ;
#108193 = VERTEX_POINT ( 'NONE', #78681 ) ;
#108194 = CARTESIAN_POINT ( 'NONE',  ( -17.99451991528748351, 28.92564299267950645, 4.000000000000000000 ) ) ;
#108195 = ORIENTED_EDGE ( 'NONE', *, *, #100449, .T. ) ;
#108196 = ORIENTED_EDGE ( 'NONE', *, *, #20731, .F. ) ;
#108197 = CARTESIAN_POINT ( 'NONE',  ( 30.18398860626900060, 28.73617430169808173, 5.000000000000000000 ) ) ;
#108198 = PLANE ( 'NONE',  #55563 ) ;
#108199 = ORIENTED_EDGE ( 'NONE', *, *, #29855, .F. ) ;
#108200 =( NAMED_UNIT ( * ) SI_UNIT ( $, .STERADIAN. ) SOLID_ANGLE_UNIT ( ) );
#108201 = DIRECTION ( 'NONE',  ( -0.7071067811865487940, 0.7071067811865463515, 0.000000000000000000 ) ) ;
#108202 = DIRECTION ( 'NONE',  ( -0.7071067811865486830, -0.7071067811865464625, 0.000000000000000000 ) ) ;
#108203 = CARTESIAN_POINT ( 'NONE',  ( -20.67183060077632817, -18.74070752338409207, 4.000000000000000000 ) ) ;
#108204 = FACE_OUTER_BOUND ( 'NONE', #97322, .T. ) ;
#108205 = VERTEX_POINT ( 'NONE', #3915 ) ;
#108206 = FACE_OUTER_BOUND ( 'NONE', #63524, .T. ) ;
#108207 = LINE ( 'NONE', #8869, #9768 ) ;
#108208 = VECTOR ( 'NONE', #105483, 1000.000000000000114 ) ;
#108209 = CARTESIAN_POINT ( 'NONE',  ( -31.82816939922330945, 15.75929247661555443, 4.000000000000000000 ) ) ;
#108210 = CARTESIAN_POINT ( 'NONE',  ( 13.60343192894634967, -14.24070752338413293, 19.24067776001729158 ) ) ;
#108211 = PLANE ( 'NONE',  #137718 ) ;
#108212 = CARTESIAN_POINT ( 'NONE',  ( -45.48921356237309510, -27.52281430457087197, 5.000000000000000000 ) ) ;
#108213 = CARTESIAN_POINT ( 'NONE',  ( 22.22840764549667725, 9.139736423841732040E-16, 0.000000000000000000 ) ) ;
#108214 = CARTESIAN_POINT ( 'NONE',  ( 53.01669371712955581, 7.950000000000001066, -2.130196079827421318 ) ) ;
#108215 = VECTOR ( 'NONE', #102877, 1000.000000000000000 ) ;
#108216 = LINE ( 'NONE', #131449, #69334 ) ;
#108217 = ORIENTED_EDGE ( 'NONE', *, *, #67327, .F. ) ;
#108218 = ORIENTED_EDGE ( 'NONE', *, *, #6447, .F. ) ;
#108219 = CARTESIAN_POINT ( 'NONE',  ( 52.04166666666666430, -3.975000000000002753, 6.884901960086286188 ) ) ;
#108220 = CARTESIAN_POINT ( 'NONE',  ( -21.18398860626899349, 28.73617430169802134, 5.000000000000000000 ) ) ;
#108221 = DIRECTION ( 'NONE',  ( 0.7071067811865487940, 0.7071067811865463515, -0.000000000000000000 ) ) ;
#108222 = DIRECTION ( 'NONE',  ( -0.000000000000000000, 0.3543493200069153248, 0.9351131265310292928 ) ) ;
#108223 = VERTEX_POINT ( 'NONE', #91687 ) ;
#108224 = CARTESIAN_POINT ( 'NONE',  ( 1.828169399223519953, -20.24070752338407431, 4.000000000000000000 ) ) ;
#108225 = CARTESIAN_POINT ( 'NONE',  ( 49.14626352523143282, -4.472830434245840259, 4.472830434245839371 ) ) ;
#108226 = VERTEX_POINT ( 'NONE', #23577 ) ;
#108227 = EDGE_CURVE ( 'NONE', #80973, #126820, #70690, .T. ) ;
#108228 = LINE ( 'NONE', #84407, #45566 ) ;
#108229 = ORIENTED_EDGE ( 'NONE', *, *, #30605, .T. ) ;
#108230 = ORIENTED_EDGE ( 'NONE', *, *, #10782, .F. ) ;
#108231 = LINE ( 'NONE', #89382, #135258 ) ;
#108232 = CARTESIAN_POINT ( 'NONE',  ( 80.57919371712955581, 3.975000000000002753, -6.884901960086283523 ) ) ;
#108233 = CARTESIAN_POINT ( 'NONE',  ( 12.70612307739187052, 22.22500000000000142, 4.000000000000000000 ) ) ;
#108234 = DIRECTION ( 'NONE',  ( -0.7071067811865487940, 0.7071067811865463515, 0.000000000000000000 ) ) ;
#108235 = ORIENTED_EDGE ( 'NONE', *, *, #2751, .F. ) ;
#108236 = CARTESIAN_POINT ( 'NONE',  ( 12.48921356237309155, -27.52281430457064104, 5.000000000000000000 ) ) ;
#108237 = EDGE_CURVE ( 'NONE', #76949, #137069, #25716, .T. ) ;
#108238 = EDGE_CURVE ( 'NONE', #20015, #24720, #69989, .T. ) ;
#108240 = ORIENTED_EDGE ( 'NONE', *, *, #6277, .T. ) ;
#108239 = CARTESIAN_POINT ( 'NONE',  ( 20.99065804761471199, 4.584330080086930965E-16, 0.000000000000000000 ) ) ;
#108241 = CARTESIAN_POINT ( 'NONE',  ( 84.87543019189810423, -5.291415217122920289, -3.055000000000001492 ) ) ;
#108242 = CARTESIAN_POINT ( 'NONE',  ( -15.56584921360887108, 8.021612662230191759, 4.000000000000000000 ) ) ;
#108243 = DIRECTION ( 'NONE',  ( 0.000000000000000000, 0.000000000000000000, 1.000000000000000000 ) ) ;
#108244 = DIRECTION ( 'NONE',  ( -0.7071067811865486830, -0.7071067811865464625, -0.000000000000000000 ) ) ;
#108245 = EDGE_CURVE ( 'NONE', #102633, #52625, #14836, .T. ) ;
#108246 = ADVANCED_FACE ( 'NONE', ( #46078 ), #75341, .T. ) ;
#108247 = EDGE_LOOP ( 'NONE', ( #34478, #52737, #57382, #104555, #30981 ) ) ;
#108248 = VECTOR ( 'NONE', #73577, 999.9999999999998863 ) ;
#108249 = CARTESIAN_POINT ( 'NONE',  ( 64.22459685856478018, -1.637169565754160949, 6.109999999999997655 ) ) ;
#108250 = CARTESIAN_POINT ( 'NONE',  ( -4.499999999999962697, 16.46639925780210234, 5.000000000000000000 ) ) ;
#108251 = EDGE_CURVE ( 'NONE', #35225, #142584, #81564, .T. ) ;
#108252 = FACE_OUTER_BOUND ( 'NONE', #133072, .T. ) ;
#108253 = ORIENTED_EDGE ( 'NONE', *, *, #42871, .F. ) ;
#108254 = ORIENTED_EDGE ( 'NONE', *, *, #105264, .T. ) ;
#108255 = EDGE_CURVE ( 'NONE', #66262, #66281, #35201, .T. ) ;
#108256 = CARTESIAN_POINT ( 'NONE',  ( 11.58838509405160089, 22.22500000000000497, 4.777194822843814137 ) ) ;
#108257 =( NAMED_UNIT ( * ) PLANE_ANGLE_UNIT ( ) SI_UNIT ( $, .RADIAN. ) );
#108258 = ORIENTED_EDGE ( 'NONE', *, *, #125170, .F. ) ;
#108259 = EDGE_CURVE ( 'NONE', #132937, #75865, #123640, .T. ) ;
#108260 = ORIENTED_EDGE ( 'NONE', *, *, #24807, .T. ) ;
#108261 = CARTESIAN_POINT ( 'NONE',  ( -21.32816939922338051, 17.25929247661554911, 4.000000000000000000 ) ) ;
#108262 = VERTEX_POINT ( 'NONE', #2509 ) ;
#108263 = DIRECTION ( 'NONE',  ( 0.000000000000000000, 0.000000000000000000, 1.000000000000000000 ) ) ;
#108264 = DIRECTION ( 'NONE',  ( -0.6830127018922180770, -0.6830127018922204085, -0.2588190451025213501 ) ) ;
#108265 = VECTOR ( 'NONE', #17763, 1000.000000000000000 ) ;
#108266 = EDGE_CURVE ( 'NONE', #91948, #67296, #24295, .T. ) ;
#108267 = DIRECTION ( 'NONE',  ( 0.7071067811865487940, 0.7071067811865463515, 0.000000000000000000 ) ) ;
#108268 = VECTOR ( 'NONE', #64104, 1000.000000000000000 ) ;
#108269 = FACE_BOUND ( 'NONE', #50197, .T. ) ;
#108270 = DIRECTION ( 'NONE',  ( 0.7071067811865487940, -0.7071067811865463515, 0.000000000000000000 ) ) ;
#108271 = DIRECTION ( 'NONE',  ( 0.000000000000000000, -1.000000000000000000, 0.000000000000000000 ) ) ;
#108272 = DIRECTION ( 'NONE',  ( -0.7071067811865486830, -0.7071067811865463515, 0.000000000000000000 ) ) ;
#108274 = ORIENTED_EDGE ( 'NONE', *, *, #96800, .T. ) ;
#108273 = DIRECTION ( 'NONE',  ( -0.7071067811865486830, 0.7071067811865464625, 0.000000000000000000 ) ) ;
#108275 = EDGE_CURVE ( 'NONE', #34581, #78703, #80137, .T. ) ;
#108276 = CONICAL_SURFACE ( 'NONE', #78323, 2.500000000000000888, 0.9599310885968822538 ) ;
#108277 = AXIS2_PLACEMENT_3D ( 'NONE', #36999, #124730, #37744 ) ;
#108278 = LINE ( 'NONE', #19171, #11557 ) ;
#108279 = ORIENTED_EDGE ( 'NONE', *, *, #121359, .T. ) ;
#108280 = ORIENTED_EDGE ( 'NONE', *, *, #16284, .F. ) ;
#108281 = CARTESIAN_POINT ( 'NONE',  ( 88.43293019189809456, 1.637169565754156508, 6.110000000000000320 ) ) ;
#108282 = ORIENTED_EDGE ( 'NONE', *, *, #89087, .T. ) ;
#108283 = LINE ( 'NONE', #130090, #36022 ) ;
#108284 = CARTESIAN_POINT ( 'NONE',  ( -39.29974487139159578, -27.71228299555233576, 4.000000000000000000 ) ) ;
#108285 = EDGE_CURVE ( 'NONE', #20535, #105827, #58407, .T. ) ;
#108286 = ORIENTED_EDGE ( 'NONE', *, *, #12785, .T. ) ;
#108287 = LINE ( 'NONE', #6825, #2776 ) ;
#108288 = CARTESIAN_POINT ( 'NONE',  ( 8.878526836628477525, -20.24070752338407431, 7.412974875817769593 ) ) ;
#108289 = EDGE_CURVE ( 'NONE', #117114, #2861, #84411, .T. ) ;
#108290 = LINE ( 'NONE', #75023, #110851 ) ;
#108291 = CARTESIAN_POINT ( 'NONE',  ( -21.29974487139158512, -27.71228299555221142, 4.000000000000000000 ) ) ;
#108292 = LINE ( 'NONE', #140950, #31922 ) ;
#108293 = PLANE ( 'NONE',  #121378 ) ;
#108294 = EDGE_CURVE ( 'NONE', #135854, #80606, #60527, .T. ) ;
#108295 = DIRECTION ( 'NONE',  ( 0.7071067811865487940, 0.7071067811865463515, -0.000000000000000000 ) ) ;
#108296 = LINE ( 'NONE', #8967, #13787 ) ;
#108297 = ORIENTED_EDGE ( 'NONE', *, *, #32853, .T. ) ;
#108298 = DIRECTION ( 'NONE',  ( -0.000000000000000000, -0.3543493200069152693, 0.9351131265310292928 ) ) ;
#108299 = VERTEX_POINT ( 'NONE', #106835 ) ;
#108300 = DIRECTION ( 'NONE',  ( 0.000000000000000000, 1.000000000000000000, 0.000000000000000000 ) ) ;
#108301 = EDGE_CURVE ( 'NONE', #1370, #61259, #106098, .T. ) ;
#108302 = DIRECTION ( 'NONE',  ( 0.7071067811865487940, -0.7071067811865463515, 0.000000000000000000 ) ) ;
#108303 = EDGE_CURVE ( 'NONE', #85621, #58156, #29281, .T. ) ;
#108304 = VERTEX_POINT ( 'NONE', #39474 ) ;
#108305 = VERTEX_POINT ( 'NONE', #139520 ) ;
#108306 = CARTESIAN_POINT ( 'NONE',  ( 14.51078643762690490, -27.52281430457045275, 5.000000000000000000 ) ) ;
#108307 = ORIENTED_EDGE ( 'NONE', *, *, #50976, .T. ) ;
#108308 = CARTESIAN_POINT ( 'NONE',  ( 31.35459685856476497, -1.637169565754161615, 6.110000000000000320 ) ) ;
#108309 = ORIENTED_EDGE ( 'NONE', *, *, #75552, .T. ) ;
#108310 = DIRECTION ( 'NONE',  ( 0.6830127018922181881, 0.6830127018922202975, -0.2588190451025214056 ) ) ;
#108311 = CARTESIAN_POINT ( 'NONE',  ( 23.37913961620377279, -5.278424836066145431, -3.047499999999993658 ) ) ;
#108312 = CARTESIAN_POINT ( 'NONE',  ( -5.349701230251782569, 11.76033174582461527, -25.84502411307383696 ) ) ;
#108313 = EDGE_LOOP ( 'NONE', ( #68027, #142443, #57919, #110895 ) ) ;
#108314 = ADVANCED_FACE ( 'NONE', ( #83709 ), #117685, .F. ) ;
#108315 = CARTESIAN_POINT ( 'NONE',  ( -60.48921356237309510, -27.52281430457097500, 5.000000000000000000 ) ) ;
#108316 = VERTEX_POINT ( 'NONE', #117005 ) ;
#108317 = CARTESIAN_POINT ( 'NONE',  ( 152.4000000000000057, 7.919999999999947526, -21.52770000000001005 ) ) ;
#108318 = LINE ( 'NONE', #88042, #128522 ) ;
#108320 = ORIENTED_EDGE ( 'NONE', *, *, #23589, .T. ) ;
#108319 = CARTESIAN_POINT ( 'NONE',  ( 1.499999999999994449, 0.4497235411627456547, -5.599840258123537140 ) ) ;
#108321 = ORIENTED_EDGE ( 'NONE', *, *, #122099, .F. ) ;
#108322 = CARTESIAN_POINT ( 'NONE',  ( -23.89661266223020419, -0.3091507863911187037, 4.000000000000000000 ) ) ;
#108323 = VECTOR ( 'NONE', #141014, 1000.000000000000000 ) ;
#108324 = CARTESIAN_POINT ( 'NONE',  ( 23.29289321881329755, -15.74070752338412049, 5.000000000000000000 ) ) ;
#108325 = EDGE_LOOP ( 'NONE', ( #41117, #11373, #31531, #7883, #86176 ) ) ;
#108326 = DIRECTION ( 'NONE',  ( -0.7071067811865486830, -0.7071067811865464625, 0.000000000000000000 ) ) ;
#108327 = ORIENTED_EDGE ( 'NONE', *, *, #75130, .T. ) ;
#108328 = PRODUCT_DEFINITION_SHAPE ( 'NONE', 'NONE',  #12014 ) ;
#108329 = VERTEX_POINT ( 'NONE', #38045 ) ;
#108330 = EDGE_CURVE ( 'NONE', #24720, #111950, #74229, .T. ) ;
#108331 = ORIENTED_EDGE ( 'NONE', *, *, #102129, .F. ) ;
#108332 = CARTESIAN_POINT ( 'NONE',  ( -20.51078643762690490, -27.52281430457041012, 5.000000000000000000 ) ) ;
#108333 = CARTESIAN_POINT ( 'NONE',  ( 39.48921356237310221, -27.52281430457082934, 5.000000000000000000 ) ) ;
#108334 = LINE ( 'NONE', #126043, #42182 ) ;
#108335 = DIRECTION ( 'NONE',  ( 0.7071067811865487940, 0.7071067811865463515, 0.000000000000000000 ) ) ;
#108336 = EDGE_CURVE ( 'NONE', #109228, #140721, #82966, .T. ) ;
#108337 = CARTESIAN_POINT ( 'NONE',  ( -3.792893218813421008, -5.240707523384228850, 5.000000000000000000 ) ) ;
#108338 = VERTEX_POINT ( 'NONE', #17673 ) ;
#108340 = EDGE_CURVE ( 'NONE', #94913, #59092, #18375, .T. ) ;
#108339 = FACE_OUTER_BOUND ( 'NONE', #17524, .T. ) ;
#108341 = ORIENTED_EDGE ( 'NONE', *, *, #81689, .T. ) ;
#108342 = DIRECTION ( 'NONE',  ( -0.7071067811865486830, -0.7071067811865464625, -0.000000000000000000 ) ) ;
#108343 = LINE ( 'NONE', #9018, #55170 ) ;
#108344 = ORIENTED_EDGE ( 'NONE', *, *, #34201, .T. ) ;
#108345 = DIRECTION ( 'NONE',  ( 0.7071067811865487940, 0.7071067811865463515, -0.000000000000000000 ) ) ;
#108346 = DIRECTION ( 'NONE',  ( 0.7071067811865486830, -0.7071067811865464625, -0.000000000000000000 ) ) ;
#108347 = EDGE_LOOP ( 'NONE', ( #43568, #118727, #101434, #124052 ) ) ;
#108348 = ORIENTED_EDGE ( 'NONE', *, *, #114506, .T. ) ;
#108349 =( NAMED_UNIT ( * ) PLANE_ANGLE_UNIT ( ) SI_UNIT ( $, .RADIAN. ) );
#108350 = CARTESIAN_POINT ( 'NONE',  ( -1.828169399223515512, -20.24070752338407431, 4.000000000000000000 ) ) ;
#108351 = DIRECTION ( 'NONE',  ( 1.000000000000000000, 0.000000000000000000, 0.000000000000000000 ) ) ;
#108352 = CARTESIAN_POINT ( 'NONE',  ( 7.014532492589830248, 3.821174125832445049E-16, 0.000000000000000000 ) ) ;
#108353 = DIRECTION ( 'NONE',  ( 0.7071067811865487940, -0.7071067811865463515, 0.000000000000000000 ) ) ;
#108354 = CARTESIAN_POINT ( 'NONE',  ( 65.53709685856478018, -3.054999999999999272, -5.291415217122919401 ) ) ;
#108355 = EDGE_CURVE ( 'NONE', #3249, #49064, #61263, .T. ) ;
#108356 = FACE_OUTER_BOUND ( 'NONE', #8062, .T. ) ;
#108357 = CARTESIAN_POINT ( 'NONE',  ( 0.000000000000000000, 0.000000000000000000, 5.000000000000000000 ) ) ;
#108358 = ADVANCED_FACE ( 'NONE', ( #49652 ), #115541, .F. ) ;
#108359 = CARTESIAN_POINT ( 'NONE',  ( -57.18398860626899705, 28.73617430169827358, 5.000000000000000000 ) ) ;
#108360 = CARTESIAN_POINT ( 'NONE',  ( 34.49999999999976552, 19.39370406404970026, 1.459788787078122319 ) ) ;
#108361 = ORIENTED_EDGE ( 'NONE', *, *, #78418, .F. ) ;
#108362 = CARTESIAN_POINT ( 'NONE',  ( 17.99999999999986855, -5.527737879153178824, -7.983877177622413335 ) ) ;
#108363 = VERTEX_POINT ( 'NONE', #93830 ) ;
#108364 = LINE ( 'NONE', #87385, #131147 ) ;
#108365 = DIRECTION ( 'NONE',  ( 0.7071067811865487940, 0.7071067811865463515, -0.000000000000000000 ) ) ;
#108366 = ORIENTED_EDGE ( 'NONE', *, *, #43197, .F. ) ;
#108367 = DIRECTION ( 'NONE',  ( -0.000000000000000000, -0.3543493200069152693, 0.9351131265310292928 ) ) ;
#108369 = VERTEX_POINT ( 'NONE', #138057 ) ;
#108368 = CARTESIAN_POINT ( 'NONE',  ( 3.183988606268992161, 28.73617430169789699, 5.000000000000000000 ) ) ;
#108370 = AXIS2_PLACEMENT_3D ( 'NONE', #3950, #81596, #123678 ) ;
#108371 = DIRECTION ( 'NONE',  ( -0.6830127018922180770, -0.6830127018922204085, -0.2588190451025213501 ) ) ;
#108372 = EDGE_CURVE ( 'NONE', #16482, #31359, #68525, .T. ) ;
#108373 = DIRECTION ( 'NONE',  ( -0.000000000000000000, -0.3543493200069152693, 0.9351131265310292928 ) ) ;
#108374 = CARTESIAN_POINT ( 'NONE',  ( -9.792893218813384593, -17.24070752338409918, 5.000000000000000000 ) ) ;
#108375 = ORIENTED_EDGE ( 'NONE', *, *, #20728, .T. ) ;
#108376 = ORIENTED_EDGE ( 'NONE', *, *, #107903, .T. ) ;
#108377 = DIRECTION ( 'NONE',  ( -0.7071067811865487940, 0.7071067811865463515, 0.000000000000000000 ) ) ;
#108378 = LINE ( 'NONE', #109130, #65278 ) ;
#108379 = AXIS2_PLACEMENT_3D ( 'NONE', #109587, #33493, #19717 ) ;
#108380 = VECTOR ( 'NONE', #23828, 1000.000000000000000 ) ;
#108381 = LINE ( 'NONE', #7668, #56914 ) ;
#108382 = CARTESIAN_POINT ( 'NONE',  ( 80.14169371712957002, -2.130196079827424871, -7.949999999999999289 ) ) ;
#108383 = PLANE ( 'NONE',  #104140 ) ;
#108384 = CARTESIAN_POINT ( 'NONE',  ( 13.92145407031093818, 4.584330080086930965E-16, 0.000000000000000000 ) ) ;
#108385 = VERTEX_POINT ( 'NONE', #77804 ) ;
#108386 = CARTESIAN_POINT ( 'NONE',  ( -29.67183060077625711, -0.7407075233842770334, 4.000000000000000000 ) ) ;
#108387 = PLANE ( 'NONE',  #29889 ) ;
#108388 = CARTESIAN_POINT ( 'NONE',  ( 13.71003237941630104, 5.842153316012715258, 5.000000000000000000 ) ) ;
#108389 = COLOUR_RGB ( '', 0.72549020, 0.75294118, 0.79215686) ;
#108390 = EDGE_LOOP ( 'NONE', ( #44859, #122421, #138497, #85675 ) ) ;
#108391 = LINE ( 'NONE', #9076, #74578 ) ;
#108392 = VERTEX_POINT ( 'NONE', #11068 ) ;
#108393 = AXIS2_PLACEMENT_3D ( 'NONE', #28901, #73137, #62253 ) ;
#108394 = CARTESIAN_POINT ( 'NONE',  ( 72.91709685856477563, 3.054999999999998828, 5.291415217122922066 ) ) ;
#108395 = DIRECTION ( 'NONE',  ( 0.7071067811865487940, -0.7071067811865463515, 0.000000000000000000 ) ) ;
#108396 = CARTESIAN_POINT ( 'NONE',  ( 0.000000000000000000, 21.72500000000000142, 4.500000000000000888 ) ) ;
#108398 = ORIENTED_EDGE ( 'NONE', *, *, #73880, .F. ) ;
#108397 = VECTOR ( 'NONE', #66368, 1000.000000000000000 ) ;
#108399 = CARTESIAN_POINT ( 'NONE',  ( -20.99999999999984368, -3.033600742197705369, 5.000000000000000000 ) ) ;
#108400 =( BOUNDED_CURVE ( )  B_SPLINE_CURVE ( 3, ( #118220, #18927, #84226, #64582 ),
 .UNSPECIFIED., .F., .T. ) 
 B_SPLINE_CURVE_WITH_KNOTS ( ( 4, 4 ),
 ( 5.043186909253408956, 5.074607125596347856 ),
 .UNSPECIFIED. ) 
 CURVE ( )  GEOMETRIC_REPRESENTATION_ITEM ( )  RATIONAL_B_SPLINE_CURVE ( ( 1.000000000000000000, 0.9999177325257868620, 0.9999177325257868620, 1.000000000000000000 ) ) 
 REPRESENTATION_ITEM ( '' )  );
#108401 =( GEOMETRIC_REPRESENTATION_CONTEXT ( 3 ) GLOBAL_UNCERTAINTY_ASSIGNED_CONTEXT ( ( #52074 ) ) GLOBAL_UNIT_ASSIGNED_CONTEXT ( ( #53104, #140827, #141576 ) ) REPRESENTATION_CONTEXT ( 'NONE', 'WORKASPACE' ) );
#108402 = DIRECTION ( 'NONE',  ( -0.6830127018922181881, 0.6830127018922202975, -0.2588190451025214056 ) ) ;
#108403 = VECTOR ( 'NONE', #121700, 1000.000000000000000 ) ;
#108404 = CARTESIAN_POINT ( 'NONE',  ( 0.000000000000000000, -0.3999999999999998002, -2.015694669338588429 ) ) ;
#108405 = DIRECTION ( 'NONE',  ( -0.7071067811865486830, -0.7071067811865464625, -0.000000000000000000 ) ) ;
#108406 = ADVANCED_FACE ( 'NONE', ( #132925 ), #22655, .F. ) ;
#108408 = ORIENTED_EDGE ( 'NONE', *, *, #103550, .F. ) ;
#108407 = DIRECTION ( 'NONE',  ( -0.7071067811865486830, -0.7071067811865464625, -0.000000000000000000 ) ) ;
#108409 = CARTESIAN_POINT ( 'NONE',  ( 24.18398860626899705, 28.73617430169804265, 5.000000000000000000 ) ) ;
#108410 = LINE ( 'NONE', #73691, #119372 ) ;
#108411 = DIRECTION ( 'NONE',  ( 0.7071067811865486830, -0.7071067811865464625, -0.000000000000000000 ) ) ;
#108412 = CARTESIAN_POINT ( 'NONE',  ( 15.79289321881333841, 12.75929247661558463, 5.000000000000000000 ) ) ;
#108413 = ORIENTED_EDGE ( 'NONE', *, *, #32929, .F. ) ;
#108415 = VERTEX_POINT ( 'NONE', #119833 ) ;
#108414 = EDGE_CURVE ( 'NONE', #59299, #61284, #32895, .T. ) ;
#108416 = EDGE_CURVE ( 'NONE', #109375, #53162, #77114, .T. ) ;
#108417 = CARTESIAN_POINT ( 'NONE',  ( 67.08376352523143282, -6.110000000000001208, -3.741295971395164515E-16 ) ) ;
#108418 = VERTEX_POINT ( 'NONE', #98812 ) ;
#108419 = EDGE_CURVE ( 'NONE', #2143, #122205, #141635, .T. ) ;
#108420 = DIRECTION ( 'NONE',  ( -0.000000000000000000, -0.3543493200069152693, 0.9351131265310292928 ) ) ;
#108421 = CARTESIAN_POINT ( 'NONE',  ( -18.70701326429291456, -21.74070752338405654, 4.999753212805221558 ) ) ;
#108422 = ADVANCED_FACE ( 'NONE', ( #30741 ), #96291, .T. ) ;
#108423 = DIRECTION ( 'NONE',  ( 0.000000000000000000, 1.000000000000000000, 0.000000000000000000 ) ) ;
#108424 = ORIENTED_EDGE ( 'NONE', *, *, #70383, .F. ) ;
#108425 = AXIS2_PLACEMENT_3D ( 'NONE', #55770, #132636, #143459 ) ;
#108426 = EDGE_CURVE ( 'NONE', #24049, #119425, #64786, .T. ) ;
#108427 = DIRECTION ( 'NONE',  ( 0.000000000000000000, 0.000000000000000000, 1.000000000000000000 ) ) ;
#108428 = CARTESIAN_POINT ( 'NONE',  ( 21.70701326429288613, -21.74070752338406365, 4.999753212805217117 ) ) ;
#108429 = EDGE_CURVE ( 'NONE', #98838, #34604, #17808, .T. ) ;
#108430 = EDGE_LOOP ( 'NONE', ( #138200, #31934, #57243, #98017 ) ) ;
#108431 = EDGE_CURVE ( 'NONE', #35909, #40105, #52454, .T. ) ;
#108432 = CARTESIAN_POINT ( 'NONE',  ( 16.49999999999988987, 13.56627193232216477, -10.57019076586064976 ) ) ;
#108433 = CARTESIAN_POINT ( 'NONE',  ( 0.000000000000000000, 0.000000000000000000, 5.000000000000000000 ) ) ;
#108434 = CARTESIAN_POINT ( 'NONE',  ( -39.48921356237310221, -27.52281430457082934, 5.000000000000000000 ) ) ;
#108435 = EDGE_LOOP ( 'NONE', ( #131719, #29181, #102985, #53993 ) ) ;
#108436 = EDGE_LOOP ( 'NONE', ( #15, #110160, #29118, #111027 ) ) ;
#108437 = EDGE_CURVE ( 'NONE', #37549, #49848, #96644, .T. ) ;
#108438 = EDGE_CURVE ( 'NONE', #115267, #28809, #85802, .T. ) ;
#108439 = CARTESIAN_POINT ( 'NONE',  ( 11.70025512860841133, -27.71228299555198049, 4.000000000000000000 ) ) ;
#108440 = CARTESIAN_POINT ( 'NONE',  ( 13.49999999999991118, 12.43112307739206024, 4.000000000000000000 ) ) ;
#108441 = CARTESIAN_POINT ( 'NONE',  ( 128.3052689125804875, -5.499261314031185677, -3.175000000000000711 ) ) ;
#108442 = CARTESIAN_POINT ( 'NONE',  ( 18.63999999999999702, 9.521314400968980422E-16, 0.000000000000000000 ) ) ;
#108443 = FACE_OUTER_BOUND ( 'NONE', #41449, .T. ) ;
#108444 = EDGE_CURVE ( 'NONE', #45259, #20400, #130773, .T. ) ;
#108445 = DIRECTION ( 'NONE',  ( -1.000000000000000000, -1.224606353822377258E-16, -0.000000000000000000 ) ) ;
#108446 = FILL_AREA_STYLE_COLOUR ( '', #60948 ) ;
#108447 = ORIENTED_EDGE ( 'NONE', *, *, #140266, .T. ) ;
#108448 = VERTEX_POINT ( 'NONE', #88690 ) ;
#108449 = CARTESIAN_POINT ( 'NONE',  ( 109.7245968585647660, -1.637169565754160949, 6.109999999999997655 ) ) ;
#108450 = ORIENTED_EDGE ( 'NONE', *, *, #106279, .T. ) ;
#108451 = ORIENTED_EDGE ( 'NONE', *, *, #121376, .T. ) ;
#108452 = CARTESIAN_POINT ( 'NONE',  ( 32.99999999999977263, -11.35517001088068945, -1.126524801160033507 ) ) ;
#108453 = CARTESIAN_POINT ( 'NONE',  ( 15.79333936457837062, 21.75929247661549937, 4.998822639870715179 ) ) ;
#108454 = CARTESIAN_POINT ( 'NONE',  ( 13.31312592467349454, 1.515602562757560223, 4.636692559446319528 ) ) ;
#108455 = VERTEX_POINT ( 'NONE', #53931 ) ;
#108456 = PLANE ( 'NONE',  #66814 ) ;
#108457 = LINE ( 'NONE', #140416, #79673 ) ;
#108458 = VECTOR ( 'NONE', #28344, 1000.000000000000000 ) ;
#108459 = DIRECTION ( 'NONE',  ( -0.6830127018922180770, -0.6830127018922204085, -0.2588190451025213501 ) ) ;
#108460 = EDGE_CURVE ( 'NONE', #14564, #48060, #33604, .T. ) ;
#108461 = CARTESIAN_POINT ( 'NONE',  ( 4.898587196589412829E-16, 60.00000000000000000, 4.000000000000000000 ) ) ;
#108462 = AXIS2_PLACEMENT_3D ( 'NONE', #104929, #70224, #15053 ) ;
#108463 = AXIS2_PLACEMENT_3D ( 'NONE', #75245, #109269, #142622 ) ;
#108464 = FACE_OUTER_BOUND ( 'NONE', #45289, .T. ) ;
#108465 = AXIS2_PLACEMENT_3D ( 'NONE', #5036, #27526, #137025 ) ;
#108466 = ORIENTED_EDGE ( 'NONE', *, *, #72526, .T. ) ;
#108467 = FACE_OUTER_BOUND ( 'NONE', #112886, .T. ) ;
#108468 = DIRECTION ( 'NONE',  ( -1.000000000000000000, -1.224606353822377258E-16, -0.000000000000000000 ) ) ;
#108469 = VECTOR ( 'NONE', #114546, 999.9999999999998863 ) ;
#108470 = EDGE_LOOP ( 'NONE', ( #121947, #59970, #18808, #93793 ) ) ;
#108471 = DIRECTION ( 'NONE',  ( -0.3543493200069162685, -0.000000000000000000, -0.9351131265310288487 ) ) ;
#108472 = VERTEX_POINT ( 'NONE', #98124 ) ;
#108473 = ORIENTED_EDGE ( 'NONE', *, *, #73214, .F. ) ;
#108474 = VERTEX_POINT ( 'NONE', #43040 ) ;
#108475 = CARTESIAN_POINT ( 'NONE',  ( 60.95876352523143993, 0.000000000000000000, -6.110000000000001208 ) ) ;
#108476 = AXIS2_PLACEMENT_3D ( 'NONE', #77695, #45097, #76999 ) ;
#108477 = ORIENTED_EDGE ( 'NONE', *, *, #30210, .T. ) ;
#108478 = ORIENTED_EDGE ( 'NONE', *, *, #128501, .T. ) ;
#108479 = VECTOR ( 'NONE', #38979, 1000.000000000000000 ) ;
#108480 = EDGE_CURVE ( 'NONE', #90561, #42516, #32677, .T. ) ;
#108481 = CARTESIAN_POINT ( 'NONE',  ( 15.18398860626900237, 28.73617430169797871, 5.000000000000000000 ) ) ;
#108482 = CARTESIAN_POINT ( 'NONE',  ( -1.850027050462894174, -4.461849672132299105, 4.461849672132299993 ) ) ;
#108483 = CARTESIAN_POINT ( 'NONE',  ( 96.83376352523144703, 6.110000000000001208, 1.122388791418549305E-15 ) ) ;
#108484 = EDGE_CURVE ( 'NONE', #136079, #93121, #21272, .T. ) ;
#108485 = CARTESIAN_POINT ( 'NONE',  ( 25.39999999999999858, 0.000000000000000000, 0.000000000000000000 ) ) ;
#108486 = ORIENTED_EDGE ( 'NONE', *, *, #141566, .T. ) ;
#108487 = DIRECTION ( 'NONE',  ( -0.6830127018922180770, -0.6830127018922204085, -0.2588190451025213501 ) ) ;
#108488 = COLOUR_RGB ( '', 0.72549020, 0.75294118, 0.79215686) ;
#108489 = FACE_OUTER_BOUND ( 'NONE', #124912, .T. ) ;
#108490 = CARTESIAN_POINT ( 'NONE',  ( 2.000000000000000000, -2.375000000000000000, 1.069999999999998508 ) ) ;
#108491 = CARTESIAN_POINT ( 'NONE',  ( 78.24586038379621300, 3.974999999999996980, 6.884901960086287964 ) ) ;
#108492 = ORIENTED_EDGE ( 'NONE', *, *, #22995, .T. ) ;
#108493 = LINE ( 'NONE', #9176, #124764 ) ;
#108494 = EDGE_CURVE ( 'NONE', #32917, #67920, #89383, .T. ) ;
#108495 = ORIENTED_EDGE ( 'NONE', *, *, #45865, .T. ) ;
#108496 = ORIENTED_EDGE ( 'NONE', *, *, #10758, .F. ) ;
#108497 = ORIENTED_EDGE ( 'NONE', *, *, #129858, .T. ) ;
#108498 = CARTESIAN_POINT ( 'NONE',  ( 126.3495968585647802, 6.109999999999996767, 1.637169565754163836 ) ) ;
#108499 = VECTOR ( 'NONE', #141399, 1000.000000000000000 ) ;
#108500 = ORIENTED_EDGE ( 'NONE', *, *, #55169, .T. ) ;
#108501 = VECTOR ( 'NONE', #36764, 1000.000000000000000 ) ;
#108502 = VECTOR ( 'NONE', #53496, 999.9999999999998863 ) ;
#108503 = DIRECTION ( 'NONE',  ( 1.000000000000000000, 0.000000000000000000, 0.000000000000000000 ) ) ;
#108504 = CARTESIAN_POINT ( 'NONE',  ( 51.18398860626899705, 28.73617430169823095, 5.000000000000000000 ) ) ;
#108505 = VECTOR ( 'NONE', #91805, 1000.000000000000000 ) ;
#108506 = ADVANCED_FACE ( 'NONE', ( #56802 ), #45901, .F. ) ;
#108507 = CARTESIAN_POINT ( 'NONE',  ( 10.83999999999999986, -2.055000000000000160, 0.000000000000000000 ) ) ;
#108508 = EDGE_LOOP ( 'NONE', ( #59064, #24764, #49787, #14261, #139018 ) ) ;
#108509 = CARTESIAN_POINT ( 'NONE',  ( -6.489213562373093325, -27.52281430457059841, 5.000000000000000000 ) ) ;
#108510 = ORIENTED_EDGE ( 'NONE', *, *, #134560, .T. ) ;
#108511 = CIRCLE ( 'NONE', #138691, 2.500000000000000888 ) ;
#108512 = AXIS2_PLACEMENT_3D ( 'NONE', #54355, #10087, #76073 ) ;
#108513 = CARTESIAN_POINT ( 'NONE',  ( 0.2704031414352193186, -7.934999999999989839, 2.126176841940957907 ) ) ;
#108514 = SPHERICAL_SURFACE ( 'NONE', #78714, 3.000000000000000000 ) ;
#108515 = DIRECTION ( 'NONE',  ( 0.6830127018922181881, 0.6830127018922202975, -0.2588190451025214056 ) ) ;
#108516 = CARTESIAN_POINT ( 'NONE',  ( 0.000000000000000000, -13.97847968911260530, -0.1324546996126791387 ) ) ;
#108517 = VERTEX_POINT ( 'NONE', #24836 ) ;
#108518 = EDGE_LOOP ( 'NONE', ( #97844, #31835, #100803, #60904 ) ) ;
#108519 = VERTEX_POINT ( 'NONE', #113260 ) ;
#108520 = CARTESIAN_POINT ( 'NONE',  ( -51.18398860626899705, 28.73617430169823095, 5.000000000000000000 ) ) ;
#108521 = FACE_OUTER_BOUND ( 'NONE', #41576, .T. ) ;
#108522 = CIRCLE ( 'NONE', #83123, 2.500000000000000888 ) ;
#108523 = LINE ( 'NONE', #74536, #137617 ) ;
#108525 = EDGE_CURVE ( 'NONE', #43020, #15065, #48044, .T. ) ;
#108524 = CARTESIAN_POINT ( 'NONE',  ( 57.18398860626899705, 28.73617430169827358, 5.000000000000000000 ) ) ;
#108526 = CARTESIAN_POINT ( 'NONE',  ( 34.49999999999975842, 8.900465351122182511, -2.516491619111592914 ) ) ;
#108527 = LINE ( 'NONE', #131763, #138684 ) ;
#108528 = EDGE_CURVE ( 'NONE', #101812, #13435, #37145, .T. ) ;
#108529 = CARTESIAN_POINT ( 'NONE',  ( 29.75043019189810423, 3.055000000000002824, -5.291415217122919401 ) ) ;
#108530 = FILL_AREA_STYLE_COLOUR ( '', #34842 ) ;
#108531 =( NAMED_UNIT ( * ) SI_UNIT ( $, .STERADIAN. ) SOLID_ANGLE_UNIT ( ) );
#108532 = ORIENTED_EDGE ( 'NONE', *, *, #38155, .T. ) ;
#108533 = CARTESIAN_POINT ( 'NONE',  ( -15.18398860626900237, 28.73617430169797871, 5.000000000000000000 ) ) ;
#108534 = ORIENTED_EDGE ( 'NONE', *, *, #55691, .T. ) ;
#108535 = FACE_OUTER_BOUND ( 'NONE', #41216, .T. ) ;
#108536 = VERTEX_POINT ( 'NONE', #111103 ) ;
#108537 = CARTESIAN_POINT ( 'NONE',  ( 22.99806943317885199, -22.22500000000000142, 4.500000000000000888 ) ) ;
#108539 = EDGE_LOOP ( 'NONE', ( #15391, #3422, #62122 ) ) ;
#108538 = CARTESIAN_POINT ( 'NONE',  ( 41.24999999999999289, -9.735942053221458872E-16, 7.950000000000000178 ) ) ;
#108540 = ADVANCED_FACE ( 'NONE', ( #78514 ), #56081, .F. ) ;
#108541 = DIRECTION ( 'NONE',  ( 0.7071067811865486830, -0.7071067811865464625, -0.000000000000000000 ) ) ;
#108542 = ORIENTED_EDGE ( 'NONE', *, *, #103549, .F. ) ;
#108543 = DIRECTION ( 'NONE',  ( -1.000000000000000000, -1.224606353822377258E-16, -0.000000000000000000 ) ) ;
#108544 = ORIENTED_EDGE ( 'NONE', *, *, #96479, .F. ) ;
#108545 = CARTESIAN_POINT ( 'NONE',  ( 34.92499999999998295, 3.662461875838979974, 4.000000000000000000 ) ) ;
#108546 = UNCERTAINTY_MEASURE_WITH_UNIT (LENGTH_MEASURE( 1.000000000000000082E-05 ), #60894, 'distance_accuracy_value', 'NONE');
#108547 = EDGE_LOOP ( 'NONE', ( #92337, #142035, #34154, #33705, #91409 ) ) ;
#108548 = LINE ( 'NONE', #53507, #100765 ) ;
#108549 = CARTESIAN_POINT ( 'NONE',  ( 116.8916937171295558, 2.130196079827421762, 7.950000000000001066 ) ) ;
#108550 = LINE ( 'NONE', #96958, #67036 ) ;
#108551 = CARTESIAN_POINT ( 'NONE',  ( -13.49999999999990052, 5.696342897626497148, -7.587980461218431394 ) ) ;
#108552 = CARTESIAN_POINT ( 'NONE',  ( 20.99999999999986500, -10.44781430457071458, 5.000000000000000000 ) ) ;
#108553 = CARTESIAN_POINT ( 'NONE',  ( 20.99999999999987210, 20.58746187583903264, 4.000000000000000000 ) ) ;
#108554 = LINE ( 'NONE', #9234, #2135 ) ;
#108555 = CARTESIAN_POINT ( 'NONE',  ( 0.4375000000000001665, -4.461849672132299105, 4.461849672132299993 ) ) ;
#108556 = CARTESIAN_POINT ( 'NONE',  ( 14.56206980810188512, -7.934999999999990727, -2.126176841940955242 ) ) ;
#108557 = CARTESIAN_POINT ( 'NONE',  ( 0.000000000000000000, 0.000000000000000000, 0.000000000000000000 ) ) ;
#108558 = DIRECTION ( 'NONE',  ( 0.6830127018922180770, -0.6830127018922204085, -0.2588190451025213501 ) ) ;
#108559 = ORIENTED_EDGE ( 'NONE', *, *, #137198, .T. ) ;
#108560 = EDGE_CURVE ( 'NONE', #40356, #5851, #58239, .T. ) ;
#108561 = EDGE_LOOP ( 'NONE', ( #33443, #3077, #74784, #30594, #96675, #2069, #23490, #95710 ) ) ;
#108562 = DIRECTION ( 'NONE',  ( 0.6830127018922180770, -0.6830127018922204085, -0.2588190451025213501 ) ) ;
#108563 = ORIENTED_EDGE ( 'NONE', *, *, #115619, .T. ) ;
#108564 = PLANE ( 'NONE',  #50334 ) ;
#108565 = DIRECTION ( 'NONE',  ( -0.000000000000000000, -0.3543493200069152693, 0.9351131265310292928 ) ) ;
#108566 = AXIS2_PLACEMENT_3D ( 'NONE', #121824, #131300, #66765 ) ;
#108567 = CARTESIAN_POINT ( 'NONE',  ( 128.6786164994711612, -49.14501756083436135, -40.36361034346619903 ) ) ;
#108568 = EDGE_LOOP ( 'NONE', ( #21709, #5835, #16245, #60806 ) ) ;
#108569 = AXIS2_PLACEMENT_3D ( 'NONE', #32209, #139574, #40257 ) ;
#108570 = VECTOR ( 'NONE', #24247, 1000.000000000000114 ) ;
#108571 = MECHANICAL_DESIGN_GEOMETRIC_PRESENTATION_REPRESENTATION (  '', ( #113259 ), #78513 ) ;
#108572 = LINE ( 'NONE', #131089, #116888 ) ;
#108573 = DIRECTION ( 'NONE',  ( 0.000000000000000000, 0.000000000000000000, 1.000000000000000000 ) ) ;
#108574 = AXIS2_PLACEMENT_3D ( 'NONE', #15213, #48589, #94221 ) ;
#108575 = CARTESIAN_POINT ( 'NONE',  ( 93.45833333333334281, 3.974999999999997424, 6.884901960086288852 ) ) ;
#108576 = SURFACE_STYLE_USAGE ( .BOTH. , #139854 ) ;
#108578 = ORIENTED_EDGE ( 'NONE', *, *, #55144, .T. ) ;
#108577 = DIRECTION ( 'NONE',  ( -0.6830127018922181881, 0.6830127018922202975, -0.2588190451025214056 ) ) ;
#108579 = CARTESIAN_POINT ( 'NONE',  ( 39.49999999999999289, 0.000000000000000000, -7.950000000000000178 ) ) ;
#108580 = DIRECTION ( 'NONE',  ( 0.7071067811865486830, -0.7071067811865464625, -0.000000000000000000 ) ) ;
#108581 = PLANE ( 'NONE',  #47933 ) ;
#108582 = AXIS2_PLACEMENT_3D ( 'NONE', #41520, #121926, #54576 ) ;
#108583 =( BOUNDED_CURVE ( )  B_SPLINE_CURVE ( 3, ( #18025, #61609, #19492, #139876 ),
 .UNSPECIFIED., .F., .T. ) 
 B_SPLINE_CURVE_WITH_KNOTS ( ( 4, 4 ),
 ( 5.043186909253412509, 5.074607125596351409 ),
 .UNSPECIFIED. ) 
 CURVE ( )  GEOMETRIC_REPRESENTATION_ITEM ( )  RATIONAL_B_SPLINE_CURVE ( ( 1.000000000000000000, 0.9999177325257868620, 0.9999177325257868620, 1.000000000000000000 ) ) 
 REPRESENTATION_ITEM ( '' )  );
#108584 = DIRECTION ( 'NONE',  ( -0.000000000000000000, 0.3543493200069153248, 0.9351131265310292928 ) ) ;
#108585 = ORIENTED_EDGE ( 'NONE', *, *, #68544, .T. ) ;
#108586 = ORIENTED_EDGE ( 'NONE', *, *, #97689, .T. ) ;
#108587 = VERTEX_POINT ( 'NONE', #124868 ) ;
#108588 = EDGE_CURVE ( 'NONE', #98608, #6354, #47370, .T. ) ;
#108589 = CARTESIAN_POINT ( 'NONE',  ( 92.89626352523143282, 4.472830434245840259, -4.472830434245839371 ) ) ;
#108590 = ORIENTED_EDGE ( 'NONE', *, *, #123370, .T. ) ;
#108591 = EDGE_CURVE ( 'NONE', #17366, #74602, #23396, .T. ) ;
#108592 = CARTESIAN_POINT ( 'NONE',  ( 128.6577301979972390, -49.12413125935271552, 39.93743342457242562 ) ) ;
#108593 = EDGE_CURVE ( 'NONE', #110860, #140411, #45205, .T. ) ;
#108594 = VECTOR ( 'NONE', #51737, 1000.000000000000000 ) ;
#108595 = VECTOR ( 'NONE', #66910, 1000.000000000000000 ) ;
#108596 = PLANE ( 'NONE',  #142987 ) ;
#108597 = VERTEX_POINT ( 'NONE', #68383 ) ;
#108598 = EDGE_CURVE ( 'NONE', #43430, #42382, #102431, .T. ) ;
#108599 = CARTESIAN_POINT ( 'NONE',  ( 9.489213562373095101, -27.52281430457062328, 5.000000000000000000 ) ) ;
#108600 = LINE ( 'NONE', #33274, #132236 ) ;
#108601 = VECTOR ( 'NONE', #168, 1000.000000000000000 ) ;
#108602 = CARTESIAN_POINT ( 'NONE',  ( 93.68293019189812298, -1.637169565754158951, -6.109999999999998543 ) ) ;
#108603 = ORIENTED_EDGE ( 'NONE', *, *, #80924, .T. ) ;
#108604 = CARTESIAN_POINT ( 'NONE',  ( 9.183988606268997046, 28.73617430169793607, 5.000000000000000000 ) ) ;
#108605 = DIRECTION ( 'NONE',  ( 0.3543493200069162685, -0.000000000000000000, -0.9351131265310288487 ) ) ;
#108606 = CARTESIAN_POINT ( 'NONE',  ( 27.68840764549667455, -3.851859888774471706E-31, 2.500000000000001332 ) ) ;
#108607 = VECTOR ( 'NONE', #133097, 1000.000000000000000 ) ;
#108608 = FACE_OUTER_BOUND ( 'NONE', #98633, .T. ) ;
#108609 = VECTOR ( 'NONE', #72975, 1000.000000000000000 ) ;
#108610 = AXIS2_PLACEMENT_3D ( 'NONE', #28365, #116062, #118920 ) ;
#108611 = ORIENTED_EDGE ( 'NONE', *, *, #23716, .F. ) ;
#108612 = EDGE_LOOP ( 'NONE', ( #138149, #67621, #12713, #132945 ) ) ;
#108613 = EDGE_CURVE ( 'NONE', #65412, #52532, #133615, .T. ) ;
#108614 = EDGE_LOOP ( 'NONE', ( #20698, #29039, #102631, #132906 ) ) ;
#108615 = CARTESIAN_POINT ( 'NONE',  ( 6.183988606268994381, 28.73617430169791476, 5.000000000000000000 ) ) ;
#108616 = EDGE_CURVE ( 'NONE', #97401, #96891, #77149, .T. ) ;
#108617 = DIRECTION ( 'NONE',  ( -0.7071067811865486830, 0.7071067811865464625, 0.000000000000000000 ) ) ;
#108618 = CARTESIAN_POINT ( 'NONE',  ( 15.81706980810188767, -2.126176841940956130, 7.934999999999990727 ) ) ;
#108619 = CONICAL_SURFACE ( 'NONE', #22932, 2.055000000000000604, 0.9599310885968764806 ) ;
#108620 = AXIS2_PLACEMENT_3D ( 'NONE', #93933, #138170, #62054 ) ;
#108621 = DIRECTION ( 'NONE',  ( -0.000000000000000000, 0.3543493200069153248, 0.9351131265310292928 ) ) ;
#108622 = EDGE_CURVE ( 'NONE', #28852, #45152, #90082, .T. ) ;
#108623 = LINE ( 'NONE', #10743, #138 ) ;
#108624 =( NAMED_UNIT ( * ) PLANE_ANGLE_UNIT ( ) SI_UNIT ( $, .RADIAN. ) );
#108625 = ORIENTED_EDGE ( 'NONE', *, *, #101118, .F. ) ;
#108626 = ORIENTED_EDGE ( 'NONE', *, *, #58246, .F. ) ;
#108627 = DIRECTION ( 'NONE',  ( -0.7071067811865486830, -0.7071067811865464625, 0.000000000000000000 ) ) ;
#108628 = VERTEX_POINT ( 'NONE', #35761 ) ;
#108629 = ORIENTED_EDGE ( 'NONE', *, *, #81230, .F. ) ;
#108630 = EDGE_CURVE ( 'NONE', #80972, #92701, #35030, .T. ) ;
#108631 = VECTOR ( 'NONE', #107491, 1000.000000000000227 ) ;
#108632 = DIRECTION ( 'NONE',  ( 1.000000000000000000, 0.000000000000000000, 0.000000000000000000 ) ) ;
#108633 = CARTESIAN_POINT ( 'NONE',  ( 30.32816939922331656, -15.74070752338412760, 4.000000000000000000 ) ) ;
#108634 = ORIENTED_EDGE ( 'NONE', *, *, #38078, .T. ) ;
#108635 = CARTESIAN_POINT ( 'NONE',  ( -19.63753812416085154, 22.22500000000000142, 4.000000000000000000 ) ) ;
#108636 = CARTESIAN_POINT ( 'NONE',  ( -0.3281693992235254487, -9.740707523384187994, 4.000000000000000000 ) ) ;
#108637 = EDGE_CURVE ( 'NONE', #21299, #118847, #80669, .T. ) ;
#108638 = CARTESIAN_POINT ( 'NONE',  ( 9.208651418775088970, 4.584330080086930965E-16, 0.000000000000000000 ) ) ;
#108639 = DIRECTION ( 'NONE',  ( 0.3543493200069162685, -0.000000000000000000, -0.9351131265310288487 ) ) ;
#108640 = ORIENTED_EDGE ( 'NONE', *, *, #65192, .T. ) ;
#108641 =( NAMED_UNIT ( * ) PLANE_ANGLE_UNIT ( ) SI_UNIT ( $, .RADIAN. ) );
#108642 = VERTEX_POINT ( 'NONE', #79979 ) ;
#108643 = CARTESIAN_POINT ( 'NONE',  ( 17.06332250466817158, -2.500000000000000444, 3.061616997868384127E-16 ) ) ;
#108644 = LINE ( 'NONE', #9324, #108177 ) ;
#108645 = ORIENTED_EDGE ( 'NONE', *, *, #11872, .F. ) ;
#108646 = DIRECTION ( 'NONE',  ( 0.000000000000000000, 0.000000000000000000, -1.000000000000000000 ) ) ;
#108647 = ORIENTED_EDGE ( 'NONE', *, *, #134458, .F. ) ;
#108648 = LINE ( 'NONE', #109400, #62090 ) ;
#108649 = VERTEX_POINT ( 'NONE', #69816 ) ;
#108650 = EDGE_LOOP ( 'NONE', ( #43941, #98154, #11400, #9290 ) ) ;
#108651 = ORIENTED_EDGE ( 'NONE', *, *, #62664, .F. ) ;
#108652 = EDGE_CURVE ( 'NONE', #22073, #87140, #58963, .T. ) ;
#108653 = CARTESIAN_POINT ( 'NONE',  ( 27.47459685856478018, 1.637169565754164280, -6.109999999999996767 ) ) ;
#108654 = DIRECTION ( 'NONE',  ( -0.7071067811865486830, 0.7071067811865464625, 0.000000000000000000 ) ) ;
#108655 = FACE_OUTER_BOUND ( 'NONE', #105179, .T. ) ;
#108656 = DIRECTION ( 'NONE',  ( -0.7071067811865486830, -0.7071067811865464625, 0.000000000000000000 ) ) ;
#108657 = DIRECTION ( 'NONE',  ( -0.7071067811865487940, 0.7071067811865463515, -0.000000000000000000 ) ) ;
#108658 = DIRECTION ( 'NONE',  ( -0.000000000000000000, 0.3543493200069153248, 0.9351131265310292928 ) ) ;
#108659 = LINE ( 'NONE', #97062, #117721 ) ;
#108660 = CARTESIAN_POINT ( 'NONE',  ( 39.29974487139159578, -27.71228299555233576, 4.000000000000000000 ) ) ;
#108661 = CARTESIAN_POINT ( 'NONE',  ( 13.49159235450332162, 9.902892378096218942E-16, 0.000000000000000000 ) ) ;
#108662 = EDGE_CURVE ( 'NONE', #133807, #114819, #139350, .T. ) ;
#108663 = ORIENTED_EDGE ( 'NONE', *, *, #23700, .T. ) ;
#108664 = VERTEX_POINT ( 'NONE', #70541 ) ;
#108665 = AXIS2_PLACEMENT_3D ( 'NONE', #65565, #33635, #56110 ) ;
#108666 = EDGE_LOOP ( 'NONE', ( #138156, #97490, #87299, #52065 ) ) ;
#108667 = EDGE_LOOP ( 'NONE', ( #43340, #31235, #34706, #6990 ) ) ;
#108668 = LINE ( 'NONE', #95687, #88911 ) ;
#108669 = AXIS2_PLACEMENT_3D ( 'NONE', #40603, #84806, #16683 ) ;
#108670 = VECTOR ( 'NONE', #132129, 1000.000000000000000 ) ;
#108671 = VERTEX_POINT ( 'NONE', #137902 ) ;
#108672 = CIRCLE ( 'NONE', #136539, 2.500000000000000888 ) ;
#108674 = VERTEX_POINT ( 'NONE', #83528 ) ;
#108673 = VECTOR ( 'NONE', #49156, 1000.000000000000000 ) ;
#108675 = DIRECTION ( 'NONE',  ( -0.7071067811865487940, 0.7071067811865463515, 0.000000000000000000 ) ) ;
#108676 = DIRECTION ( 'NONE',  ( 0.6830127018922181881, 0.6830127018922202975, -0.2588190451025214056 ) ) ;
#108677 = ADVANCED_FACE ( 'NONE', ( #106657 ), #72686, .F. ) ;
#108678 = CARTESIAN_POINT ( 'NONE',  ( 0.000000000000000000, 0.000000000000000000, 0.000000000000000000 ) ) ;
#108679 = ORIENTED_EDGE ( 'NONE', *, *, #6811, .F. ) ;
#108680 = LINE ( 'NONE', #8643, #20908 ) ;
#108682 = VERTEX_POINT ( 'NONE', #105940 ) ;
#108681 = AXIS2_PLACEMENT_3D ( 'NONE', #139097, #15137, #126758 ) ;
#108683 = DIRECTION ( 'NONE',  ( -0.000000000000000000, 0.3543493200069153248, 0.9351131265310292928 ) ) ;
#108684 = DIRECTION ( 'NONE',  ( -0.000000000000000000, 0.000000000000000000, 1.000000000000000000 ) ) ;
#108686 = AXIS2_PLACEMENT_3D ( 'NONE', #38675, #72783, #105343 ) ;
#108685 = CARTESIAN_POINT ( 'NONE',  ( 7.212903141435218934, 3.967499999999992699, -6.871911579029513994 ) ) ;
#108687 = EDGE_LOOP ( 'NONE', ( #12114, #64559, #682, #6670 ) ) ;
#108688 = CARTESIAN_POINT ( 'NONE',  ( 91.93293019189812298, 1.637169565754156730, 6.110000000000001208 ) ) ;
#108689 = CARTESIAN_POINT ( 'NONE',  ( 13.82816939922343380, -14.24070752338414003, 4.000000000000000000 ) ) ;
#108690 = DIRECTION ( 'NONE',  ( -0.000000000000000000, 0.000000000000000000, 1.000000000000000000 ) ) ;
#108691 = CARTESIAN_POINT ( 'NONE',  ( 33.79289321881322650, 0.7592924766157104211, 5.000000000000000000 ) ) ;
#108692 = VERTEX_POINT ( 'NONE', #17519 ) ;
#108693 = ORIENTED_EDGE ( 'NONE', *, *, #112928, .F. ) ;
#108694 = DIRECTION ( 'NONE',  ( -1.000000000000000000, -1.224606353822377258E-16, -0.000000000000000000 ) ) ;
#108695 = ORIENTED_EDGE ( 'NONE', *, *, #138282, .F. ) ;
#108696 = VECTOR ( 'NONE', #113221, 1000.000000000000114 ) ;
#108697 = FACE_OUTER_BOUND ( 'NONE', #74330, .T. ) ;
#108699 = DIRECTION ( 'NONE',  ( 0.000000000000000000, -1.000000000000000000, 0.000000000000000000 ) ) ;
#108698 = VECTOR ( 'NONE', #97229, 1000.000000000000000 ) ;
#108700 = CARTESIAN_POINT ( 'NONE',  ( -6.299744871391586898, -27.71228299555210484, 4.000000000000000000 ) ) ;
#108701 = LINE ( 'NONE', #118157, #130596 ) ;
#108702 = ORIENTED_EDGE ( 'NONE', *, *, #1559, .T. ) ;
#108703 = LINE ( 'NONE', #140644, #53015 ) ;
#108704 = VECTOR ( 'NONE', #95783, 1000.000000000000000 ) ;
#108705 = EDGE_CURVE ( 'NONE', #74278, #96665, #5904, .T. ) ;
#108706 = CARTESIAN_POINT ( 'NONE',  ( 8.994519915287490619, 28.92564299267944250, 4.000000000000000000 ) ) ;
#108707 = CARTESIAN_POINT ( 'NONE',  ( 13.49999999999990763, 3.653845994658403651, -4.504631822206401459 ) ) ;
#108708 = ORIENTED_EDGE ( 'NONE', *, *, #35649, .F. ) ;
#108709 = CARTESIAN_POINT ( 'NONE',  ( -24.79289321881328334, 15.75929247661555799, 5.000000000000000000 ) ) ;
#108710 = AXIS2_PLACEMENT_3D ( 'NONE', #63394, #30750, #52464 ) ;
#108712 = STYLED_ITEM ( 'NONE', ( #120502 ), #58892 ) ;
#108711 = DIRECTION ( 'NONE',  ( 0.7071067811865487940, 0.7071067811865463515, -0.000000000000000000 ) ) ;
#108713 = VERTEX_POINT ( 'NONE', #61776 ) ;
#108714 = VECTOR ( 'NONE', #72448, 1000.000000000000000 ) ;
#108715 = EDGE_CURVE ( 'NONE', #47367, #4770, #37885, .T. ) ;
#108717 = VERTEX_POINT ( 'NONE', #61099 ) ;
#108716 = DIRECTION ( 'NONE',  ( -0.7071067811865486830, -0.7071067811865464625, 0.000000000000000000 ) ) ;
#108718 = ORIENTED_EDGE ( 'NONE', *, *, #119137, .F. ) ;
#108719 = VECTOR ( 'NONE', #70969, 1000.000000000000000 ) ;
#108720 = ADVANCED_FACE ( 'NONE', ( #105254 ), #59641, .F. ) ;
#108721 = DIRECTION ( 'NONE',  ( -1.000000000000000000, -0.000000000000000000, -0.000000000000000000 ) ) ;
#108722 = VECTOR ( 'NONE', #91677, 1000.000000000000227 ) ;
#108723 = CARTESIAN_POINT ( 'NONE',  ( 0.000000000000000000, 0.000000000000000000, 5.000000000000000000 ) ) ;
#108724 = ORIENTED_EDGE ( 'NONE', *, *, #71272, .F. ) ;
#108725 = CARTESIAN_POINT ( 'NONE',  ( -20.99999999999985079, 13.55218569542903140, 5.000000000000000000 ) ) ;
#108726 = UNCERTAINTY_MEASURE_WITH_UNIT (LENGTH_MEASURE( 1.000000000000000082E-05 ), #90147, 'distance_accuracy_value', 'NONE');
#108727 = DIRECTION ( 'NONE',  ( -0.7071067811865486830, -0.7071067811865464625, -0.000000000000000000 ) ) ;
#108728 = LINE ( 'NONE', #142135, #85554 ) ;
#108729 = CARTESIAN_POINT ( 'NONE',  ( 0.1600000000000028066, -2.637033663574361420, -7.491577539992840151 ) ) ;
#108730 = LINE ( 'NONE', #85570, #111554 ) ;
#108731 = DIRECTION ( 'NONE',  ( -0.000000000000000000, -0.000000000000000000, 1.000000000000000000 ) ) ;
#108732 = CARTESIAN_POINT ( 'NONE',  ( 22.42820000000000036, 3.174999999999997158, 1.444000000000000394 ) ) ;
#108734 = VECTOR ( 'NONE', #56581, 1000.000000000000000 ) ;
#108733 = CARTESIAN_POINT ( 'NONE',  ( 0.1839886062690032631, 28.73617430169787568, 5.000000000000000000 ) ) ;
#108735 = DIRECTION ( 'NONE',  ( 0.6830127018922181881, 0.6830127018922202975, -0.2588190451025214056 ) ) ;
#108736 = PLANE ( 'NONE',  #83002 ) ;
#108737 = CARTESIAN_POINT ( 'NONE',  ( 20.97999999999999687, 9.521314400968980422E-16, 0.000000000000000000 ) ) ;
#108738 = FACE_OUTER_BOUND ( 'NONE', #97445, .T. ) ;
#108739 = ORIENTED_EDGE ( 'NONE', *, *, #6994, .F. ) ;
#108740 = EDGE_CURVE ( 'NONE', #105598, #56006, #114686, .T. ) ;
#108741 = VERTEX_POINT ( 'NONE', #127741 ) ;
#108742 = EDGE_LOOP ( 'NONE', ( #19598, #22910, #134459, #69877 ) ) ;
#108743 = CARTESIAN_POINT ( 'NONE',  ( 102.5000000000000142, 0.000000000000000000, -7.950000000000000178 ) ) ;
#108744 = VERTEX_POINT ( 'NONE', #117530 ) ;
#108745 = VERTEX_POINT ( 'NONE', #39304 ) ;
#108746 = ORIENTED_EDGE ( 'NONE', *, *, #73760, .F. ) ;
#108747 = CARTESIAN_POINT ( 'NONE',  ( -0.5166543864104510275, 22.22500000000000142, 4.500000000000000888 ) ) ;
#108748 = CARTESIAN_POINT ( 'NONE',  ( 13.13598696172163116, 4.584330080086930965E-16, 0.000000000000000000 ) ) ;
#108749 = VECTOR ( 'NONE', #16137, 1000.000000000000227 ) ;
#108750 = VERTEX_POINT ( 'NONE', #15355 ) ;
#108751 = CARTESIAN_POINT ( 'NONE',  ( 34.92499999999998295, -22.22500000000000142, 4.500000000000000888 ) ) ;
#108752 =( LENGTH_UNIT ( ) NAMED_UNIT ( * ) SI_UNIT ( .MILLI., .METRE. ) );
#108753 = CARTESIAN_POINT ( 'NONE',  ( 89.03752705046288440, -9.735942053221456900E-16, 7.949999999999998401 ) ) ;
#108754 = LINE ( 'NONE', #74767, #55834 ) ;
#108755 = VERTEX_POINT ( 'NONE', #103797 ) ;
#108756 = CARTESIAN_POINT ( 'NONE',  ( 4.609452035336649267, 11.99542526557792321, -27.26742746539979834 ) ) ;
#108757 = CARTESIAN_POINT ( 'NONE',  ( 20.29289321881331887, 14.25929247661557397, 5.000000000000000000 ) ) ;
#108758 = CARTESIAN_POINT ( 'NONE',  ( -34.92500000000001137, 16.70193056682083821, 4.500000000000000888 ) ) ;
#108759 = FACE_OUTER_BOUND ( 'NONE', #110043, .T. ) ;
#108760 = CARTESIAN_POINT ( 'NONE',  ( 0.4427966827908959013, -0.5999999999999994227, -4.147834322102035287 ) ) ;
#108761 = CARTESIAN_POINT ( 'NONE',  ( 31.57919371712955581, 3.975000000000002753, -6.884901960086283523 ) ) ;
#108762 = CARTESIAN_POINT ( 'NONE',  ( -14.81601139373099585, 28.73617430169776910, 5.000000000000000000 ) ) ;
#108763 = ORIENTED_EDGE ( 'NONE', *, *, #30756, .F. ) ;
#108764 = EDGE_LOOP ( 'NONE', ( #31994, #139307, #56941, #79223 ) ) ;
#108765 = EDGE_CURVE ( 'NONE', #60766, #42962, #29123, .T. ) ;
#108766 = CARTESIAN_POINT ( 'NONE',  ( 28.85416666666666075, -2.130196079827425315, -7.950000000000001066 ) ) ;
#108767 = ORIENTED_EDGE ( 'NONE', *, *, #47495, .T. ) ;
#108768 = PLANE ( 'NONE',  #92596 ) ;
#108769 = EDGE_CURVE ( 'NONE', #51451, #35489, #92952, .T. ) ;
#108770 = DIRECTION ( 'NONE',  ( -0.000000000000000000, 1.000000000000000000, -0.000000000000000000 ) ) ;
#108771 = CYLINDRICAL_SURFACE ( 'NONE', #85037, 0.5000000000000001110 ) ;
#108773 = EDGE_CURVE ( 'NONE', #66690, #95326, #50883, .T. ) ;
#108772 = DIRECTION ( 'NONE',  ( 0.7071067811865487940, 0.7071067811865463515, 0.000000000000000000 ) ) ;
#108774 = EDGE_CURVE ( 'NONE', #74659, #105294, #126295, .T. ) ;
#108775 = CARTESIAN_POINT ( 'NONE',  ( -20.99999999999985789, 13.93112307739204070, 4.000000000000000000 ) ) ;
#108776 = FACE_OUTER_BOUND ( 'NONE', #88798, .T. ) ;
#108777 = AXIS2_PLACEMENT_3D ( 'NONE', #54902, #11335, #99811 ) ;
#108778 = CARTESIAN_POINT ( 'NONE',  ( 120.0787635252314516, -7.482591942790325086E-16, 6.109999999999998543 ) ) ;
#108779 = ORIENTED_EDGE ( 'NONE', *, *, #130976, .T. ) ;
#108780 = VERTEX_POINT ( 'NONE', #26976 ) ;
#108781 = PLANE ( 'NONE',  #64682 ) ;
#108782 = VECTOR ( 'NONE', #126879, 1000.000000000000227 ) ;
#108783 = VECTOR ( 'NONE', #9397, 1000.000000000000114 ) ;
#108784 = STYLED_ITEM ( 'NONE', ( #39208 ), #63723 ) ;
#108785 = DIRECTION ( 'NONE',  ( -0.000000000000000000, -0.3543493200069152693, 0.9351131265310292928 ) ) ;
#108786 = PRESENTATION_STYLE_ASSIGNMENT (( #118980 ) ) ;
#108787 = AXIS2_PLACEMENT_3D ( 'NONE', #94423, #84311, #7404 ) ;
#108788 = LINE ( 'NONE', #130606, #127464 ) ;
#108789 = EDGE_LOOP ( 'NONE', ( #20368, #42709, #97248, #47453 ) ) ;
#108791 = EDGE_CURVE ( 'NONE', #136929, #27557, #47527, .T. ) ;
#108790 = CARTESIAN_POINT ( 'NONE',  ( 46.81293019189811133, -1.637169565754159617, -6.110000000000001208 ) ) ;
#108792 = ORIENTED_EDGE ( 'NONE', *, *, #25078, .F. ) ;
#108793 = CARTESIAN_POINT ( 'NONE',  ( 19.05000000000000071, 3.174999999999997158, 5.000000000000000000 ) ) ;
#108794 = ADVANCED_FACE ( 'NONE', ( #5201 ), #18206, .F. ) ;
#108795 = DIRECTION ( 'NONE',  ( 0.7071067811865487940, -0.7071067811865463515, 0.000000000000000000 ) ) ;
#108796 = DIRECTION ( 'NONE',  ( 0.000000000000000000, -1.000000000000000000, 0.000000000000000000 ) ) ;
#108797 = DIRECTION ( 'NONE',  ( 0.7071067811865486830, -0.7071067811865464625, -0.000000000000000000 ) ) ;
#108798 = CIRCLE ( 'NONE', #92561, 2.500000000000000444 ) ;
#108799 = EDGE_CURVE ( 'NONE', #40076, #105497, #86379, .T. ) ;
#108800 = CARTESIAN_POINT ( 'NONE',  ( 35.20376352523143737, 6.109999999999998543, 1.122388791418548911E-15 ) ) ;
#108801 = ORIENTED_EDGE ( 'NONE', *, *, #90459, .T. ) ;
#108802 = PLANE ( 'NONE',  #71094 ) ;
#108803 = ORIENTED_EDGE ( 'NONE', *, *, #44240, .F. ) ;
#108804 = ORIENTED_EDGE ( 'NONE', *, *, #136303, .F. ) ;
#108805 = VECTOR ( 'NONE', #62237, 1000.000000000000000 ) ;
#108806 = EDGE_CURVE ( 'NONE', #22653, #62049, #97955, .T. ) ;
#108807 = ORIENTED_EDGE ( 'NONE', *, *, #126915, .F. ) ;
#108808 = SHAPE_REPRESENTATION ( '1.7 Special Key', ( #127880 ), #114089 ) ;
#108809 = CIRCLE ( 'NONE', #25534, 4.582731094065999322 ) ;
#108810 = DIRECTION ( 'NONE',  ( -0.7071067811865486830, -0.7071067811865464625, -0.000000000000000000 ) ) ;
#108811 = CARTESIAN_POINT ( 'NONE',  ( -26.99999999999980815, -9.412538124160660047, 4.000000000000000000 ) ) ;
#108812 = ORIENTED_EDGE ( 'NONE', *, *, #19186, .F. ) ;
#108813 = CARTESIAN_POINT ( 'NONE',  ( 27.51665438641025219, 22.22500000000000142, 4.500000000000000888 ) ) ;
#108814 = AXIS2_PLACEMENT_3D ( 'NONE', #19971, #64936, #110536 ) ;
#108815 = EDGE_CURVE ( 'NONE', #88886, #52530, #52995, .T. ) ;
#108816 = FACE_OUTER_BOUND ( 'NONE', #112699, .T. ) ;
#108817 = AXIS2_PLACEMENT_3D ( 'NONE', #77615, #75461, #142158 ) ;
#108818 = DIRECTION ( 'NONE',  ( -0.6830127018922180770, -0.6830127018922204085, -0.2588190451025213501 ) ) ;
#108819 = FACE_BOUND ( 'NONE', #137568, .T. ) ;
#108820 = ORIENTED_EDGE ( 'NONE', *, *, #60358, .F. ) ;
#108821 = CARTESIAN_POINT ( 'NONE',  ( 1.500000000000001332, 19.46639925780206326, 5.000000000000000000 ) ) ;
#108822 = CIRCLE ( 'NONE', #44, 2.500000000000000888 ) ;
#108823 = DIRECTION ( 'NONE',  ( 0.000000000000000000, -1.000000000000000000, 0.000000000000000000 ) ) ;
#108824 = ORIENTED_EDGE ( 'NONE', *, *, #58835, .T. ) ;
#108825 = EDGE_CURVE ( 'NONE', #7326, #6269, #3768, .T. ) ;
#108826 = FACE_OUTER_BOUND ( 'NONE', #140489, .T. ) ;
#108827 = ORIENTED_EDGE ( 'NONE', *, *, #54979, .T. ) ;
#108828 = EDGE_CURVE ( 'NONE', #106357, #7107, #97193, .T. ) ;
#108829 = VERTEX_POINT ( 'NONE', #118249 ) ;
#108830 = PLANE ( 'NONE',  #88873 ) ;
#108831 = ORIENTED_EDGE ( 'NONE', *, *, #74311, .T. ) ;
#108832 = EDGE_CURVE ( 'NONE', #50033, #2047, #20359, .T. ) ;
#108833 = CARTESIAN_POINT ( 'NONE',  ( 53.14126352523145158, 4.472830434245835818, 4.472830434245840259 ) ) ;
#108834 = EDGE_LOOP ( 'NONE', ( #117825, #8985, #66135, #91481 ) ) ;
#108835 = PRESENTATION_LAYER_ASSIGNMENT (  '', '', ( #27840 ) ) ;
#108836 = LINE ( 'NONE', #120414, #44081 ) ;
#108837 = ORIENTED_EDGE ( 'NONE', *, *, #78263, .F. ) ;
#108838 =( LENGTH_UNIT ( ) NAMED_UNIT ( * ) SI_UNIT ( .MILLI., .METRE. ) );
#108839 = ORIENTED_EDGE ( 'NONE', *, *, #95489, .T. ) ;
#108840 = CARTESIAN_POINT ( 'NONE',  ( -16.49999999999988276, 9.052185695429079360, 5.000000000000000000 ) ) ;
#108842 = CARTESIAN_POINT ( 'NONE',  ( 10.56687199751251249, -21.74070752338406365, 6.915939825044048028 ) ) ;
#108841 = VECTOR ( 'NONE', #107357, 1000.000000000000000 ) ;
#108843 = FACE_OUTER_BOUND ( 'NONE', #48792, .T. ) ;
#108844 =( NAMED_UNIT ( * ) SI_UNIT ( $, .STERADIAN. ) SOLID_ANGLE_UNIT ( ) );
#108845 = FILL_AREA_STYLE_COLOUR ( '', #46052 ) ;
#108846 = CARTESIAN_POINT ( 'NONE',  ( 7.140000000000044089, -1.036479131253094653E-14, -39.50000000000000000 ) ) ;
#108847 = CARTESIAN_POINT ( 'NONE',  ( 18.48921356237309510, -27.52281430457068367, 5.000000000000000000 ) ) ;
#108848 = ORIENTED_EDGE ( 'NONE', *, *, #9560, .F. ) ;
#108849 = ORIENTED_EDGE ( 'NONE', *, *, #88071, .F. ) ;
#108850 = AXIS2_PLACEMENT_3D ( 'NONE', #34038, #122438, #23103 ) ;
#108851 = ORIENTED_EDGE ( 'NONE', *, *, #2686, .F. ) ;
#108852 = CARTESIAN_POINT ( 'NONE',  ( 19.44163961620376924, -6.094999999999989093, 1.633150327867691542 ) ) ;
#108853 = DIRECTION ( 'NONE',  ( -0.6830127018922181881, 0.6830127018922202975, -0.2588190451025214056 ) ) ;
#108854 = VERTEX_POINT ( 'NONE', #42881 ) ;
#108855 = ORIENTED_EDGE ( 'NONE', *, *, #128156, .F. ) ;
#108856 = PLANE ( 'NONE',  #104490 ) ;
#108857 = CARTESIAN_POINT ( 'NONE',  ( 36.18398860626899705, 28.73617430169812437, 5.000000000000000000 ) ) ;
#108858 = DIRECTION ( 'NONE',  ( -0.7071067811865486830, -0.7071067811865464625, -0.000000000000000000 ) ) ;
#108859 = VERTEX_POINT ( 'NONE', #98652 ) ;
#108860 = LINE ( 'NONE', #74876, #122750 ) ;
#108861 = CARTESIAN_POINT ( 'NONE',  ( 24.39999999999999858, -7.600000000000055600, -33.92499999999998295 ) ) ;
#108862 = CARTESIAN_POINT ( 'NONE',  ( 14.35873647476855197, 5.808823158059031044, -5.808823158059038150 ) ) ;
#108863 = DIRECTION ( 'NONE',  ( 0.7071067811865486830, -0.7071067811865464625, -0.000000000000000000 ) ) ;
#108864 = ORIENTED_EDGE ( 'NONE', *, *, #72203, .F. ) ;
#108865 = CARTESIAN_POINT ( 'NONE',  ( 123.5787635252314516, -7.482591942790327058E-16, 6.109999999999999432 ) ) ;
#108867 = EDGE_CURVE ( 'NONE', #101520, #72881, #88519, .T. ) ;
#108866 = LINE ( 'NONE', #111015, #95147 ) ;
#108868 = DIRECTION ( 'NONE',  ( 0.7071067811865486830, -0.7071067811865464625, -0.000000000000000000 ) ) ;
#108870 = ORIENTED_EDGE ( 'NONE', *, *, #10702, .T. ) ;
#108869 = PLANE ( 'NONE',  #135153 ) ;
#108871 = DIRECTION ( 'NONE',  ( 0.7071067811865487940, -0.7071067811865463515, 0.000000000000000000 ) ) ;
#108872 = ORIENTED_EDGE ( 'NONE', *, *, #116922, .T. ) ;
#108873 = DIRECTION ( 'NONE',  ( -0.7071067811865486830, -0.7071067811865464625, -0.000000000000000000 ) ) ;
#108874 = VECTOR ( 'NONE', #43878, 1000.000000000000000 ) ;
#108875 = PLANE ( 'NONE',  #12233 ) ;
#108876 = CARTESIAN_POINT ( 'NONE',  ( 19.73159235450332005, 9.902892378096218942E-16, 0.000000000000000000 ) ) ;
#108877 = ORIENTED_EDGE ( 'NONE', *, *, #16436, .T. ) ;
#108878 = CIRCLE ( 'NONE', #4744, 2.500000000000000888 ) ;
#108879 = CONICAL_SURFACE ( 'NONE', #106601, 2.055000000000000604, 0.9599310885968764806 ) ;
#108880 = DIRECTION ( 'NONE',  ( -0.7071067811865486830, 0.7071067811865464625, 0.000000000000000000 ) ) ;
#108881 = LINE ( 'NONE', #21191, #58340 ) ;
#108882 = ORIENTED_EDGE ( 'NONE', *, *, #96901, .T. ) ;
#108883 = VECTOR ( 'NONE', #10803, 1000.000000000000000 ) ;
#108884 = AXIS2_PLACEMENT_3D ( 'NONE', #60679, #6911, #106240 ) ;
#108885 = CIRCLE ( 'NONE', #67338, 2.500000000000000444 ) ;
#108886 = CARTESIAN_POINT ( 'NONE',  ( -78.48921356237309510, -27.52281430457109934, 5.000000000000000000 ) ) ;
#108887 = CONICAL_SURFACE ( 'NONE', #85729, 2.055000000000000604, 0.9599310885968764806 ) ;
#108888 = CARTESIAN_POINT ( 'NONE',  ( -25.49999999999982236, -9.462702396501025959, -9.474982329943454573 ) ) ;
#108890 = ORIENTED_EDGE ( 'NONE', *, *, #66140, .T. ) ;
#108889 = AXIS2_PLACEMENT_3D ( 'NONE', #54886, #1172, #78064 ) ;
#108891 = CARTESIAN_POINT ( 'NONE',  ( -9.489213562373095101, -27.52281430457062328, 5.000000000000000000 ) ) ;
#108892 = DIRECTION ( 'NONE',  ( 0.6830127018922181881, 0.6830127018922202975, -0.2588190451025214056 ) ) ;
#108893 = EDGE_CURVE ( 'NONE', #57800, #128877, #76944, .T. ) ;
#108894 = VERTEX_POINT ( 'NONE', #65356 ) ;
#108896 = VERTEX_POINT ( 'NONE', #9476 ) ;
#108895 = EDGE_CURVE ( 'NONE', #69740, #107875, #63223, .T. ) ;
#108897 = DIRECTION ( 'NONE',  ( 1.000000000000000000, -1.248002500702738701E-15, 0.000000000000000000 ) ) ;
#108898 = VECTOR ( 'NONE', #86344, 1000.000000000000000 ) ;
#108899 = CARTESIAN_POINT ( 'NONE',  ( 36.29974487139159578, -27.71228299555231445, 4.000000000000000000 ) ) ;
#108900 = ADVANCED_FACE ( 'NONE', ( #53753 ), #8057, .T. ) ;
#108901 = DIRECTION ( 'NONE',  ( -1.000000000000000000, -1.224606353822377258E-16, -0.000000000000000000 ) ) ;
#108902 = CARTESIAN_POINT ( 'NONE',  ( -8.999999999999932498, -15.03360074219758324, 5.000000000000000000 ) ) ;
#108903 = PLANE ( 'NONE',  #132439 ) ;
#108904 = EDGE_LOOP ( 'NONE', ( #120708, #32695, #36391, #111791 ) ) ;
#108905 = EDGE_CURVE ( 'NONE', #94854, #3140, #126523, .T. ) ;
#108906 = DIRECTION ( 'NONE',  ( -0.6830127018922180770, -0.6830127018922204085, -0.2588190451025213501 ) ) ;
#108907 = CARTESIAN_POINT ( 'NONE',  ( -12.00548008471251293, 28.92564299267929684, 4.000000000000000000 ) ) ;
#108908 = CARTESIAN_POINT ( 'NONE',  ( -2.700255128608413990, -27.71228299555204089, 4.000000000000000000 ) ) ;
#108909 = VECTOR ( 'NONE', #25115, 999.9999999999998863 ) ;
#108910 = DIRECTION ( 'NONE',  ( -0.3543493200069162685, -0.000000000000000000, -0.9351131265310288487 ) ) ;
#108911 = CARTESIAN_POINT ( 'NONE',  ( 33.74543019189811588, -5.291415217122919401, -3.055000000000000604 ) ) ;
#108912 = DIRECTION ( 'NONE',  ( 0.000000000000000000, 0.7453559924999308972, -0.6666666666666655194 ) ) ;
#108913 = EDGE_CURVE ( 'NONE', #78506, #125898, #54472, .T. ) ;
#108914 = VECTOR ( 'NONE', #79664, 1000.000000000000000 ) ;
#108915 = ORIENTED_EDGE ( 'NONE', *, *, #98719, .F. ) ;
#108916 = ORIENTED_EDGE ( 'NONE', *, *, #10173, .F. ) ;
#108917 = DIRECTION ( 'NONE',  ( -0.7071067811865486830, -0.7071067811865464625, -0.000000000000000000 ) ) ;
#108918 = VECTOR ( 'NONE', #27737, 1000.000000000000000 ) ;
#108919 = ORIENTED_EDGE ( 'NONE', *, *, #122635, .F. ) ;
#108920 = AXIS2_PLACEMENT_3D ( 'NONE', #21237, #143019, #100237 ) ;
#108921 = ORIENTED_EDGE ( 'NONE', *, *, #111727, .T. ) ;
#108922 = CARTESIAN_POINT ( 'NONE',  ( 9.799968779831573329, 8.259292476615627265, 16.85664084051838785 ) ) ;
#108923 = LINE ( 'NONE', #9612, #124887 ) ;
#108924 = ADVANCED_FACE ( 'NONE', ( #55168 ), #120368, .F. ) ;
#108925 = VECTOR ( 'NONE', #18325, 1000.000000000000000 ) ;
#108926 = ORIENTED_EDGE ( 'NONE', *, *, #57435, .F. ) ;
#108927 = DIRECTION ( 'NONE',  ( 0.7071067811865486830, -0.7071067811865464625, -0.000000000000000000 ) ) ;
#108928 = CYLINDRICAL_SURFACE ( 'NONE', #16220, 7.950000000000000178 ) ;
#108929 = CARTESIAN_POINT ( 'NONE',  ( 28.49999999999981171, 13.56627193232217898, -10.57019076586062134 ) ) ;
#108930 = DIRECTION ( 'NONE',  ( 0.000000000000000000, 0.000000000000000000, 1.000000000000000000 ) ) ;
#108931 = VECTOR ( 'NONE', #44618, 1000.000000000000000 ) ;
#108932 = ORIENTED_EDGE ( 'NONE', *, *, #67699, .T. ) ;
#108933 = CARTESIAN_POINT ( 'NONE',  ( -18.29974487139159223, -27.71228299555219010, 4.000000000000000000 ) ) ;
#108934 = DIRECTION ( 'NONE',  ( -0.000000000000000000, -5.075120898959323014E-15, -1.000000000000000000 ) ) ;
#108935 = EDGE_CURVE ( 'NONE', #49877, #111950, #41418, .T. ) ;
#108936 = CARTESIAN_POINT ( 'NONE',  ( 79.60416666666667140, 2.130196079827498146, 7.949999999999958433 ) ) ;
#108937 = CARTESIAN_POINT ( 'NONE',  ( 14.99451991528749595, 28.92564299267948513, 4.000000000000000000 ) ) ;
#108938 = CARTESIAN_POINT ( 'NONE',  ( 19.49999999999986500, -12.66682484999664560, -0.6294897503863490229 ) ) ;
#108939 = DIRECTION ( 'NONE',  ( 0.7071067811865487940, 0.7071067811865463515, 0.000000000000000000 ) ) ;
#108940 = CARTESIAN_POINT ( 'NONE',  ( -78.18398860626899705, 28.73617430169841924, 5.000000000000000000 ) ) ;
#108941 = CARTESIAN_POINT ( 'NONE',  ( 58.55836038379621300, -7.949999999999997513, -2.130196079827425759 ) ) ;
#108942 = DIRECTION ( 'NONE',  ( 0.7071067811865487940, 0.7071067811865463515, 0.000000000000000000 ) ) ;
#108943 = PRESENTATION_LAYER_ASSIGNMENT (  '', '', ( #34898 ) ) ;
#108944 = EDGE_LOOP ( 'NONE', ( #39899, #5376, #142038, #17427 ) ) ;
#108945 = ORIENTED_EDGE ( 'NONE', *, *, #128941, .F. ) ;
#108946 = CARTESIAN_POINT ( 'NONE',  ( 57.43750000000000711, 5.819803920172573974, -5.819803920172572198 ) ) ;
#108947 = LINE ( 'NONE', #2132, #88715 ) ;
#108948 = DIRECTION ( 'NONE',  ( -0.000000000000000000, -0.000000000000000000, 1.000000000000000000 ) ) ;
#108949 = EDGE_CURVE ( 'NONE', #38542, #79128, #74804, .T. ) ;
#108950 = VECTOR ( 'NONE', #92731, 999.9999999999998863 ) ;
#108951 = DIRECTION ( 'NONE',  ( -0.7071067811865487940, 0.7071067811865463515, -0.000000000000000000 ) ) ;
#108952 = ORIENTED_EDGE ( 'NONE', *, *, #52305, .F. ) ;
#108953 = CARTESIAN_POINT ( 'NONE',  ( -0.5879028318752435034, -1.185901033534117133, 3.957378740546157569 ) ) ;
#108955 = EDGE_CURVE ( 'NONE', #142079, #16751, #62310, .T. ) ;
#108954 = CARTESIAN_POINT ( 'NONE',  ( 28.56687199751240414, -21.74070752338405654, 6.915939825044008060 ) ) ;
#108956 = ADVANCED_FACE ( 'NONE', ( #102954 ), #89223, .F. ) ;
#108957 = CARTESIAN_POINT ( 'NONE',  ( 49.72959685856476852, -6.110000000000000320, -1.637169565754161393 ) ) ;
#108958 = ORIENTED_EDGE ( 'NONE', *, *, #69363, .F. ) ;
#108959 = DIRECTION ( 'NONE',  ( 0.000000000000000000, 0.000000000000000000, 1.000000000000000000 ) ) ;
#108960 = VERTEX_POINT ( 'NONE', #113092 ) ;
#108961 = ORIENTED_EDGE ( 'NONE', *, *, #71755, .T. ) ;
#108962 = VECTOR ( 'NONE', #60072, 1000.000000000000000 ) ;
#108963 = CARTESIAN_POINT ( 'NONE',  ( 54.48921356237310221, -27.52281430457093236, 5.000000000000000000 ) ) ;
#108964 = EDGE_CURVE ( 'NONE', #47828, #106324, #45740, .T. ) ;
#108965 = CARTESIAN_POINT ( 'NONE',  ( 80.72502705046288440, 5.819803920172573974, -5.819803920172573086 ) ) ;
#108966 = DIRECTION ( 'NONE',  ( 0.000000000000000000, 0.000000000000000000, -1.000000000000000000 ) ) ;
#108967 = CARTESIAN_POINT ( 'NONE',  ( -11.99451991528749417, 28.92564299267946382, 4.000000000000000000 ) ) ;
#108968 = VERTEX_POINT ( 'NONE', #22490 ) ;
#108969 = ADVANCED_FACE ( 'NONE', ( #79818 ), #66756, .F. ) ;
#108970 = DIRECTION ( 'NONE',  ( -0.000000000000000000, 0.3543493200069153248, 0.9351131265310292928 ) ) ;
#108972 = ORIENTED_EDGE ( 'NONE', *, *, #135412, .T. ) ;
#108971 = CYLINDRICAL_SURFACE ( 'NONE', #93899, 0.5000000000000004441 ) ;
#108973 = CARTESIAN_POINT ( 'NONE',  ( 80.50043019189810423, -3.055000000000002380, 5.291415217122920289 ) ) ;
#108974 = CARTESIAN_POINT ( 'NONE',  ( 20.14818355038132580, 17.25929247661554200, 8.802941693769250620 ) ) ;
#108975 = CARTESIAN_POINT ( 'NONE',  ( 26.99999999999980815, 20.70535890316563155, 1.956823837851852987 ) ) ;
#108976 = FACE_OUTER_BOUND ( 'NONE', #123873, .T. ) ;
#108977 = AXIS2_PLACEMENT_3D ( 'NONE', #125001, #25681, #136577 ) ;
#108978 = VECTOR ( 'NONE', #142110, 999.9999999999998863 ) ;
#108979 = ORIENTED_EDGE ( 'NONE', *, *, #112227, .T. ) ;
#108980 = EDGE_CURVE ( 'NONE', #129678, #7365, #134156, .T. ) ;
#108981 = DIRECTION ( 'NONE',  ( 1.000000000000000000, 0.000000000000000000, 0.000000000000000000 ) ) ;
#108982 = CARTESIAN_POINT ( 'NONE',  ( 67.28709685856478018, 3.054999999999997495, 5.291415217122919401 ) ) ;
#108983 = PLANE ( 'NONE',  #136735 ) ;
#108984 = LINE ( 'NONE', #74988, #15365 ) ;
#108985 =( NAMED_UNIT ( * ) PLANE_ANGLE_UNIT ( ) SI_UNIT ( $, .RADIAN. ) );
#108986 = VERTEX_POINT ( 'NONE', #47200 ) ;
#108987 = ORIENTED_EDGE ( 'NONE', *, *, #141166, .T. ) ;
#108988 = PLANE ( 'NONE',  #97790 ) ;
#108991 = EDGE_CURVE ( 'NONE', #80231, #47388, #7655, .T. ) ;
#108990 = VECTOR ( 'NONE', #138551, 1000.000000000000000 ) ;
#108989 =( LENGTH_UNIT ( ) NAMED_UNIT ( * ) SI_UNIT ( .MILLI., .METRE. ) );
#108992 = ORIENTED_EDGE ( 'NONE', *, *, #15796, .T. ) ;
#108993 = AXIS2_PLACEMENT_3D ( 'NONE', #78755, #56329, #43985 ) ;
#108995 = ORIENTED_EDGE ( 'NONE', *, *, #28023, .F. ) ;
#108994 = VECTOR ( 'NONE', #126652, 1000.000000000000000 ) ;
#108996 = CARTESIAN_POINT ( 'NONE',  ( 3.516654386410431599, 22.22500000000000142, 4.500000000000000888 ) ) ;
#108997 = EDGE_LOOP ( 'NONE', ( #99497, #121525, #10971, #38727 ) ) ;
#108998 = DIRECTION ( 'NONE',  ( -0.7071067811865487940, 0.7071067811865463515, -0.000000000000000000 ) ) ;
#108999 = CARTESIAN_POINT ( 'NONE',  ( -9.489213562373095101, -27.52281430457062328, 5.000000000000000000 ) ) ;
#109000 = AXIS2_PLACEMENT_3D ( 'NONE', #110315, #132843, #11711 ) ;
#109001 = CIRCLE ( 'NONE', #136849, 2.552699999999997971 ) ;
#109002 = CONICAL_SURFACE ( 'NONE', #46577, 2.552699999999928693, 1.029744258676634772 ) ;
#109003 = STYLED_ITEM ( 'NONE', ( #20620 ), #115617 ) ;
#109004 = LINE ( 'NONE', #9698, #14033 ) ;
#109005 = FACE_BOUND ( 'NONE', #98199, .T. ) ;
#109006 = CARTESIAN_POINT ( 'NONE',  ( -36.87485380690743852, -14.24070752338414003, 9.401115078912742007 ) ) ;
#109007 = DIRECTION ( 'NONE',  ( -0.6830127018922181881, 0.6830127018922202975, -0.2588190451025214056 ) ) ;
#109008 = EDGE_CURVE ( 'NONE', #118949, #59656, #123297, .T. ) ;
#109010 = CARTESIAN_POINT ( 'NONE',  ( -20.99451991528748707, 28.92564299267952777, 4.000000000000000000 ) ) ;
#109009 = AXIS2_PLACEMENT_3D ( 'NONE', #131643, #18549, #87425 ) ;
#109012 = ORIENTED_EDGE ( 'NONE', *, *, #133203, .F. ) ;
#109011 = DIRECTION ( 'NONE',  ( 1.000000000000000000, 0.000000000000000000, 0.000000000000000000 ) ) ;
#109013 = FACE_OUTER_BOUND ( 'NONE', #74511, .T. ) ;
#109014 = CONTEXT_DEPENDENT_SHAPE_REPRESENTATION ( #17933, #41201 ) ;
#109015 = ORIENTED_EDGE ( 'NONE', *, *, #137147, .T. ) ;
#109016 = EDGE_CURVE ( 'NONE', #143327, #10069, #55898, .T. ) ;
#109017 = ORIENTED_EDGE ( 'NONE', *, *, #100629, .F. ) ;
#109018 = CARTESIAN_POINT ( 'NONE',  ( 82.45376352523145158, -6.109999999999998543, -3.741295971395162543E-16 ) ) ;
#109019 = EDGE_LOOP ( 'NONE', ( #46961, #79458, #132752, #18310 ) ) ;
#109020 = LINE ( 'NONE', #129352, #87016 ) ;
#109021 = AXIS2_PLACEMENT_3D ( 'NONE', #19687, #107414, #40749 ) ;
#109022 = LINE ( 'NONE', #66976, #28119 ) ;
#109023 = VECTOR ( 'NONE', #61388, 999.9999999999998863 ) ;
#109024 = ORIENTED_EDGE ( 'NONE', *, *, #140874, .F. ) ;
#109025 = CARTESIAN_POINT ( 'NONE',  ( 20.65000000000000213, 1.163414459189985485E-15, -9.500000000000000000 ) ) ;
#109026 = COLOUR_RGB ( '', 0.09019608, 0.27058824, 0.51372549) ;
#109027 = LINE ( 'NONE', #140947, #79635 ) ;
#109028 = FACE_OUTER_BOUND ( 'NONE', #130161, .T. ) ;
#109029 = VECTOR ( 'NONE', #22660, 1000.000000000000000 ) ;
#109030 = CARTESIAN_POINT ( 'NONE',  ( -34.92500000000001137, -10.29806943317888290, 4.500000000000000888 ) ) ;
#109031 = LINE ( 'NONE', #30045, #66698 ) ;
#109032 = VECTOR ( 'NONE', #15071, 1000.000000000000000 ) ;
#109033 = CARTESIAN_POINT ( 'NONE',  ( 19.41972383043609440, 3.061616997868383634E-16, -2.500000000000000444 ) ) ;
#109034 = CARTESIAN_POINT ( 'NONE',  ( 17.90156419391752962, 11.25929247661561305, 10.79108189686411023 ) ) ;
#109035 = ORIENTED_EDGE ( 'NONE', *, *, #59136, .T. ) ;
#109036 = LINE ( 'NONE', #143111, #114013 ) ;
#109037 = ORIENTED_EDGE ( 'NONE', *, *, #107376, .F. ) ;
#109038 = CIRCLE ( 'NONE', #141458, 34.92999999999999261 ) ;
#109039 = CARTESIAN_POINT ( 'NONE',  ( 20.67183060077632817, 17.25929247661554200, 4.000000000000000000 ) ) ;
#109040 = CARTESIAN_POINT ( 'NONE',  ( 2.999999999999999112, -43.14999999999997726, 34.92499999999998295 ) ) ;
#109041 = ORIENTED_EDGE ( 'NONE', *, *, #96118, .F. ) ;
#109042 = EDGE_LOOP ( 'NONE', ( #4326, #98751, #62505 ) ) ;
#109043 = VECTOR ( 'NONE', #121930, 1000.000000000000000 ) ;
#109044 = ORIENTED_EDGE ( 'NONE', *, *, #9348, .T. ) ;
#109045 = CARTESIAN_POINT ( 'NONE',  ( 38.20876352523143282, -7.482591942790329030E-16, 6.110000000000001208 ) ) ;
#109046 = ORIENTED_EDGE ( 'NONE', *, *, #98632, .T. ) ;
#109047 = LINE ( 'NONE', #98200, #85685 ) ;
#109048 = CARTESIAN_POINT ( 'NONE',  ( 20.99999999999985434, -7.447814304570756327, 5.000000000000000000 ) ) ;
#109049 = CIRCLE ( 'NONE', #273, 2.500000000000000444 ) ;
#109050 = CARTESIAN_POINT ( 'NONE',  ( 22.50413961620377634, -3.047499999999994547, 5.278424836066145431 ) ) ;
#109051 = CARTESIAN_POINT ( 'NONE',  ( -4.885316295235775819, 11.90249068597260873, -25.74872977259890305 ) ) ;
#109052 = ORIENTED_EDGE ( 'NONE', *, *, #101946, .F. ) ;
#109053 = CARTESIAN_POINT ( 'NONE',  ( -33.18398860626899705, 28.73617430169810305, 5.000000000000000000 ) ) ;
#109054 = ORIENTED_EDGE ( 'NONE', *, *, #28998, .F. ) ;
#109055 = DIRECTION ( 'NONE',  ( -0.3543493200069162685, -0.000000000000000000, -0.9351131265310288487 ) ) ;
#109056 = VECTOR ( 'NONE', #45541, 1000.000000000000000 ) ;
#109057 = DIRECTION ( 'NONE',  ( -0.7071067811865487940, 0.7071067811865463515, 0.000000000000000000 ) ) ;
#109059 = ORIENTED_EDGE ( 'NONE', *, *, #41405, .T. ) ;
#109058 = DIRECTION ( 'NONE',  ( -0.000000000000000000, -0.3543493200069152693, 0.9351131265310292928 ) ) ;
#109060 = AXIS2_PLACEMENT_3D ( 'NONE', #123029, #57081, #9964 ) ;
#109061 = ORIENTED_EDGE ( 'NONE', *, *, #28340, .F. ) ;
#109062 = CARTESIAN_POINT ( 'NONE',  ( -1.499999999999987566, 7.466399257802191158, 5.000000000000000000 ) ) ;
#109063 = DIRECTION ( 'NONE',  ( -0.7071067811865486830, 0.7071067811865464625, 0.000000000000000000 ) ) ;
#109064 = CARTESIAN_POINT ( 'NONE',  ( 31.49999999999977973, 0.4311230773921780335, 4.000000000000000000 ) ) ;
#109065 = ORIENTED_EDGE ( 'NONE', *, *, #14587, .F. ) ;
#109066 = DIRECTION ( 'NONE',  ( 0.6830127018922180770, -0.6830127018922204085, -0.2588190451025213501 ) ) ;
#109067 = ORIENTED_EDGE ( 'NONE', *, *, #92785, .F. ) ;
#109068 = ORIENTED_EDGE ( 'NONE', *, *, #134251, .T. ) ;
#109069 = ORIENTED_EDGE ( 'NONE', *, *, #135330, .T. ) ;
#109070 = VECTOR ( 'NONE', #86794, 1000.000000000000000 ) ;
#109071 = FACE_OUTER_BOUND ( 'NONE', #64252, .T. ) ;
#109072 = CARTESIAN_POINT ( 'NONE',  ( -7.140000000000001457, -39.92999999999999261, -39.50000000000000000 ) ) ;
#109073 = AXIS2_PLACEMENT_3D ( 'NONE', #88446, #133376, #143513 ) ;
#109074 = DIRECTION ( 'NONE',  ( 1.000000000000000000, 0.000000000000000000, 0.000000000000000000 ) ) ;
#109075 = CARTESIAN_POINT ( 'NONE',  ( 15.20840764549667767, 9.139736423841732040E-16, 0.000000000000000000 ) ) ;
#109076 = DIRECTION ( 'NONE',  ( -0.6830127018922180770, -0.6830127018922204085, -0.2588190451025213501 ) ) ;
#109077 = ADVANCED_FACE ( 'NONE', ( #45044 ), #133445, .T. ) ;
#109078 = CARTESIAN_POINT ( 'NONE',  ( -12.75860074219786711, 21.72500000000000142, 5.000000000000000000 ) ) ;
#109079 = CARTESIAN_POINT ( 'NONE',  ( 27.48921356237309155, -27.52281430457074762, 5.000000000000000000 ) ) ;
#109080 = EDGE_CURVE ( 'NONE', #2427, #126541, #46471, .T. ) ;
#109082 = ORIENTED_EDGE ( 'NONE', *, *, #91339, .T. ) ;
#109081 = EDGE_CURVE ( 'NONE', #97758, #141006, #35591, .T. ) ;
#109083 = DIRECTION ( 'NONE',  ( 0.7071067811865487940, 0.7071067811865463515, 0.000000000000000000 ) ) ;
#109084 = VERTEX_POINT ( 'NONE', #23213 ) ;
#109085 = CIRCLE ( 'NONE', #106691, 2.500000000000000444 ) ;
#109086 = CARTESIAN_POINT ( 'NONE',  ( 8.811592354503320124, 9.902892378096218942E-16, 0.000000000000000000 ) ) ;
#109087 = ADVANCED_FACE ( 'NONE', ( #24660 ), #80498, .F. ) ;
#109088 = ADVANCED_FACE ( 'NONE', ( #12353 ), #94189, .T. ) ;
#109089 = CARTESIAN_POINT ( 'NONE',  ( 7.939999999999994174, -39.93000000000000682, -10.00000000000000178 ) ) ;
#109090 = VERTEX_POINT ( 'NONE', #127552 ) ;
#109091 = DIRECTION ( 'NONE',  ( -1.000000000000000000, -1.224606353822377258E-16, -0.000000000000000000 ) ) ;
#109092 = DIRECTION ( 'NONE',  ( 1.000000000000000000, 0.000000000000000000, 0.000000000000000000 ) ) ;
#109093 = ORIENTED_EDGE ( 'NONE', *, *, #106018, .T. ) ;
#109094 = VERTEX_POINT ( 'NONE', #94896 ) ;
#109095 = EDGE_CURVE ( 'NONE', #41713, #134257, #4268, .T. ) ;
#109096 = LINE ( 'NONE', #43158, #53387 ) ;
#109097 = DIRECTION ( 'NONE',  ( 0.7071067811865486830, -0.7071067811865464625, -0.000000000000000000 ) ) ;
#109098 = FACE_OUTER_BOUND ( 'NONE', #83794, .T. ) ;
#109099 = PRESENTATION_STYLE_ASSIGNMENT (( #3016 ) ) ;
#109100 = VECTOR ( 'NONE', #20275, 999.9999999999998863 ) ;
#109101 = LINE ( 'NONE', #33023, #43584 ) ;
#109102 = CARTESIAN_POINT ( 'NONE',  ( 70.20376352523143737, 6.109999999999999432, 1.122388791418549108E-15 ) ) ;
#109103 = CARTESIAN_POINT ( 'NONE',  ( 22.42820000000000036, 3.174999999999997158, 1.444000000000000394 ) ) ;
#109104 = VECTOR ( 'NONE', #16128, 1000.000000000000227 ) ;
#109105 = ADVANCED_FACE ( 'NONE', ( #137733 ), #139163, .T. ) ;
#109106 = VECTOR ( 'NONE', #44529, 1000.000000000000000 ) ;
#109107 = CARTESIAN_POINT ( 'NONE',  ( -14.20710678118643244, -14.24070752338413648, 5.000000000000000000 ) ) ;
#109108 = CARTESIAN_POINT ( 'NONE',  ( 1.637538124160967001, 22.22500000000000142, 4.000000000000000000 ) ) ;
#109109 = CARTESIAN_POINT ( 'NONE',  ( 33.29974487139158867, -27.71228299555229313, 4.000000000000000000 ) ) ;
#109110 = VERTEX_POINT ( 'NONE', #136276 ) ;
#109111 = CARTESIAN_POINT ( 'NONE',  ( -10.49999999999992184, 21.43112307739196609, 4.000000000000000000 ) ) ;
#109112 = EDGE_LOOP ( 'NONE', ( #66952, #100736, #45439, #27160, #87390, #29683 ) ) ;
#109113 = VECTOR ( 'NONE', #31200, 1000.000000000000227 ) ;
#109114 = CIRCLE ( 'NONE', #141630, 7.950000000000000178 ) ;
#109115 = VECTOR ( 'NONE', #63687, 1000.000000000000227 ) ;
#109116 = DIRECTION ( 'NONE',  ( -0.6830127018922180770, -0.6830127018922204085, -0.2588190451025213501 ) ) ;
#109118 = PLANE ( 'NONE',  #119382 ) ;
#109117 = AXIS2_PLACEMENT_3D ( 'NONE', #1969, #69445, #125234 ) ;
#109119 = ORIENTED_EDGE ( 'NONE', *, *, #97777, .F. ) ;
#109120 = VECTOR ( 'NONE', #106739, 1000.000000000000227 ) ;
#109121 = DIRECTION ( 'NONE',  ( 0.3543493200069162685, -0.000000000000000000, -0.9351131265310288487 ) ) ;
#109123 = ORIENTED_EDGE ( 'NONE', *, *, #141152, .F. ) ;
#109122 = DIRECTION ( 'NONE',  ( -0.6830127018922181881, 0.6830127018922202975, -0.2588190451025214056 ) ) ;
#109124 = CARTESIAN_POINT ( 'NONE',  ( -18.48921356237309510, -27.52281430457068367, 5.000000000000000000 ) ) ;
#109125 = LINE ( 'NONE', #54080, #141275 ) ;
#109126 = DIRECTION ( 'NONE',  ( -0.6830127018922180770, -0.6830127018922204085, -0.2588190451025213501 ) ) ;
#109127 = EDGE_LOOP ( 'NONE', ( #80938, #128487, #6485, #26600, #4993 ) ) ;
#109128 = VERTEX_POINT ( 'NONE', #92766 ) ;
#109129 = CARTESIAN_POINT ( 'NONE',  ( -48.48921356237309510, -27.52281430457089328, 5.000000000000000000 ) ) ;
#109130 = CARTESIAN_POINT ( 'NONE',  ( 34.42499999999998295, 22.22500000000000142, 5.000000000000000000 ) ) ;
#109131 = AXIS2_PLACEMENT_3D ( 'NONE', #117686, #8215, #64067 ) ;
#109132 = EDGE_CURVE ( 'NONE', #43296, #16866, #5739, .T. ) ;
#109133 = LINE ( 'NONE', #19278, #100554 ) ;
#109134 = CARTESIAN_POINT ( 'NONE',  ( -0.7175773864256695944, -21.73023691814493219, 5.000000000000000888 ) ) ;
#109135 = CARTESIAN_POINT ( 'NONE',  ( 85.24586038379622721, 3.974999999999996980, 6.884901960086287964 ) ) ;
#109136 = CARTESIAN_POINT ( 'NONE',  ( -20.33153258840131272, -18.74070752338409207, 20.73178291233836390 ) ) ;
#109137 = CARTESIAN_POINT ( 'NONE',  ( 23.67183060077630330, -9.740707523384186217, 4.000000000000000000 ) ) ;
#109138 = VERTEX_POINT ( 'NONE', #60916 ) ;
#109139 = CARTESIAN_POINT ( 'NONE',  ( 82.52083333333331439, 7.949999999999999289, 2.130196079827431532 ) ) ;
#109140 = VECTOR ( 'NONE', #43090, 1000.000000000000000 ) ;
#109141 = CARTESIAN_POINT ( 'NONE',  ( -54.48921356237310221, -27.52281430457093236, 5.000000000000000000 ) ) ;
#109142 = DIRECTION ( 'NONE',  ( 0.000000000000000000, -1.000000000000000000, 0.000000000000000000 ) ) ;
#109143 = CARTESIAN_POINT ( 'NONE',  ( 28.29166666666667140, -3.047499999999994547, 5.278424836066145431 ) ) ;
#109144 = EDGE_CURVE ( 'NONE', #27298, #134862, #136375, .T. ) ;
#109145 = VERTEX_POINT ( 'NONE', #36963 ) ;
#109146 = AXIS2_PLACEMENT_3D ( 'NONE', #68250, #80526, #59493 ) ;
#109147 = CARTESIAN_POINT ( 'NONE',  ( -0.4892135623730947680, -27.52281430457055578, 5.000000000000000000 ) ) ;
#109148 = EDGE_CURVE ( 'NONE', #58827, #50577, #81217, .T. ) ;
#109149 = ORIENTED_EDGE ( 'NONE', *, *, #89457, .F. ) ;
#109150 = CIRCLE ( 'NONE', #106754, 2.500000000000000888 ) ;
#109151 = CARTESIAN_POINT ( 'NONE',  ( 71.89626352523144703, 4.472830434245840259, -4.472830434245839371 ) ) ;
#109152 = EDGE_CURVE ( 'NONE', #55852, #45578, #83341, .T. ) ;
#109153 = VECTOR ( 'NONE', #143291, 1000.000000000000000 ) ;
#109154 = DIRECTION ( 'NONE',  ( -0.7071067811865486830, -0.7071067811865464625, 0.000000000000000000 ) ) ;
#109155 = CARTESIAN_POINT ( 'NONE',  ( -4.828169399223493308, 15.75929247661555799, 4.000000000000000000 ) ) ;
#109156 = VERTEX_POINT ( 'NONE', #126134 ) ;
#109157 = AXIS2_PLACEMENT_3D ( 'NONE', #129628, #30329, #94845 ) ;
#109158 = LINE ( 'NONE', #9841, #60476 ) ;
#109159 = ADVANCED_FACE ( 'NONE', ( #17353 ), #125423, .F. ) ;
#109160 = LINE ( 'NONE', #43212, #88240 ) ;
#109161 = CARTESIAN_POINT ( 'NONE',  ( 25.49999999999982592, -17.91344420646039737, 1.358650452708521916 ) ) ;
#109162 = CARTESIAN_POINT ( 'NONE',  ( 31.49999999999978684, 21.43112307739196964, 4.000000000000000000 ) ) ;
#109164 = ORIENTED_EDGE ( 'NONE', *, *, #103747, .F. ) ;
#109163 = CARTESIAN_POINT ( 'NONE',  ( 34.49999999999975842, -8.945670655168960650, 4.994342998332163219 ) ) ;
#109165 = FILL_AREA_STYLE ('',( #98990 ) ) ;
#109166 = DIRECTION ( 'NONE',  ( -0.000000000000000000, 0.000000000000000000, 1.000000000000000000 ) ) ;
#109167 = LINE ( 'NONE', #77296, #820 ) ;
#109168 = ADVANCED_FACE ( 'NONE', ( #93497 ), #105764, .F. ) ;
#109169 = DIRECTION ( 'NONE',  ( -0.6830127018922181881, 0.6830127018922202975, -0.2588190451025214056 ) ) ;
#109170 = ORIENTED_EDGE ( 'NONE', *, *, #115532, .F. ) ;
#109171 = ORIENTED_EDGE ( 'NONE', *, *, #60269, .F. ) ;
#109172 = CARTESIAN_POINT ( 'NONE',  ( 61.10459685856476852, 1.637169565754164946, -6.109999999999999432 ) ) ;
#109173 = EDGE_LOOP ( 'NONE', ( #99562, #68918, #75476, #4689 ) ) ;
#109174 = ADVANCED_FACE ( 'NONE', ( #70366 ), #126816, .F. ) ;
#109175 = DIRECTION ( 'NONE',  ( 0.7071067811865486830, -0.7071067811865464625, -0.000000000000000000 ) ) ;
#109176 = CARTESIAN_POINT ( 'NONE',  ( 1.828169399223519731, -8.240707523384200428, 4.000000000000000000 ) ) ;
#109177 = VECTOR ( 'NONE', #89217, 1000.000000000000000 ) ;
#109178 = CARTESIAN_POINT ( 'NONE',  ( 20.66652290003515446, 8.920938975803856863, 4.000000000000000000 ) ) ;
#109179 = SURFACE_SIDE_STYLE ('',( #76585 ) ) ;
#109180 = ORIENTED_EDGE ( 'NONE', *, *, #7771, .F. ) ;
#109181 = AXIS2_PLACEMENT_3D ( 'NONE', #118184, #30508, #97899 ) ;
#109182 = DIRECTION ( 'NONE',  ( -0.3543493200069162685, -0.000000000000000000, -0.9351131265310288487 ) ) ;
#109183 = ORIENTED_EDGE ( 'NONE', *, *, #72407, .F. ) ;
#109184 = EDGE_CURVE ( 'NONE', #135984, #123357, #87280, .T. ) ;
#109185 = DIRECTION ( 'NONE',  ( -0.6830127018922180770, -0.6830127018922204085, -0.2588190451025213501 ) ) ;
#109186 = DIRECTION ( 'NONE',  ( 1.000000000000000000, 0.000000000000000000, 0.000000000000000000 ) ) ;
#109187 = DIRECTION ( 'NONE',  ( 0.7071067811865487940, 0.7071067811865463515, -0.000000000000000000 ) ) ;
#109188 = CIRCLE ( 'NONE', #18832, 2.055000000000001048 ) ;
#109189 = ORIENTED_EDGE ( 'NONE', *, *, #33840, .F. ) ;
#109190 = ORIENTED_EDGE ( 'NONE', *, *, #128815, .T. ) ;
#109191 = FACE_BOUND ( 'NONE', #71056, .T. ) ;
#109192 = CARTESIAN_POINT ( 'NONE',  ( -22.17183060077631396, -17.24070752338410273, 4.000000000000000000 ) ) ;
#109193 = EDGE_CURVE ( 'NONE', #54275, #1086, #48566, .T. ) ;
#109194 = CARTESIAN_POINT ( 'NONE',  ( -21.48921356237309155, -27.52281430457070499, 5.000000000000000000 ) ) ;
#109195 = CARTESIAN_POINT ( 'NONE',  ( 61.66666666666666430, 6.884901960086285300, 3.975000000000003642 ) ) ;
#109196 = CIRCLE ( 'NONE', #23512, 6.350000000000008527 ) ;
#109197 = FILL_AREA_STYLE ('',( #30952 ) ) ;
#109198 = LINE ( 'NONE', #42554, #139210 ) ;
#109199 = CARTESIAN_POINT ( 'NONE',  ( 0.000000000000000000, 0.000000000000000000, 0.000000000000000000 ) ) ;
#109200 = ORIENTED_EDGE ( 'NONE', *, *, #37267, .T. ) ;
#109201 = EDGE_CURVE ( 'NONE', #138495, #43532, #59231, .T. ) ;
#109202 = EDGE_LOOP ( 'NONE', ( #114707, #64016, #124450, #9153 ) ) ;
#109203 = CARTESIAN_POINT ( 'NONE',  ( 111.6204301918981088, 3.055000000000001936, -5.291415217122916737 ) ) ;
#109204 = ORIENTED_EDGE ( 'NONE', *, *, #67317, .T. ) ;
#109205 = ORIENTED_EDGE ( 'NONE', *, *, #96074, .T. ) ;
#109206 = CARTESIAN_POINT ( 'NONE',  ( 180.8090197240729537, -49.02095135882289156, 39.67421197282972400 ) ) ;
#109207 = AXIS2_PLACEMENT_3D ( 'NONE', #73630, #30857, #119944 ) ;
#109208 = VECTOR ( 'NONE', #110296, 1000.000000000000227 ) ;
#109209 = CARTESIAN_POINT ( 'NONE',  ( -15.48921356237309510, -27.52281430457066236, 5.000000000000000000 ) ) ;
#109210 = VECTOR ( 'NONE', #20427, 999.9999999999998863 ) ;
#109211 = COLOUR_RGB ( '', 0.08235294, 0.09019608, 0.10196078) ;
#109213 = EDGE_CURVE ( 'NONE', #17061, #49517, #25109, .T. ) ;
#109212 = DIRECTION ( 'NONE',  ( -0.7071067811865486830, 0.7071067811865464625, 0.000000000000000000 ) ) ;
#109214 = ORIENTED_EDGE ( 'NONE', *, *, #96680, .T. ) ;
#109215 = PLANE ( 'NONE',  #80697 ) ;
#109216 = CARTESIAN_POINT ( 'NONE',  ( 21.48921356237309155, -27.52281430457070499, 5.000000000000000000 ) ) ;
#109218 = CARTESIAN_POINT ( 'NONE',  ( 27.43680103220812327, -12.74070752338415602, 9.898150129686310805 ) ) ;
#109217 = CARTESIAN_POINT ( 'NONE',  ( -21.18398860626899349, 28.73617430169802134, 5.000000000000000000 ) ) ;
#109219 = CARTESIAN_POINT ( 'NONE',  ( -15.18398860626900237, 28.73617430169797871, 5.000000000000000000 ) ) ;
#109220 = VECTOR ( 'NONE', #63548, 1000.000000000000000 ) ;
#109221 = VECTOR ( 'NONE', #64937, 1000.000000000000227 ) ;
#109222 = CIRCLE ( 'NONE', #42093, 2.500000000000000444 ) ;
#109223 = CARTESIAN_POINT ( 'NONE',  ( 1.320799999999991092, 0.08682076437340231767, 3.775643966265890494 ) ) ;
#109224 = ORIENTED_EDGE ( 'NONE', *, *, #39123, .T. ) ;
#109225 = DIRECTION ( 'NONE',  ( -0.7071067811865487940, 0.7071067811865463515, -0.000000000000000000 ) ) ;
#109226 = CARTESIAN_POINT ( 'NONE',  ( 22.07159235450331991, 9.902892378096218942E-16, 0.000000000000000000 ) ) ;
#109227 = VERTEX_POINT ( 'NONE', #47643 ) ;
#109228 = VERTEX_POINT ( 'NONE', #124439 ) ;
#109229 = EDGE_CURVE ( 'NONE', #80743, #87397, #68658, .T. ) ;
#109230 = ORIENTED_EDGE ( 'NONE', *, *, #93264, .T. ) ;
#109231 = VECTOR ( 'NONE', #7347, 1000.000000000000227 ) ;
#109232 = CARTESIAN_POINT ( 'NONE',  ( 66.06293019189810423, 1.637169565754157174, 6.110000000000002984 ) ) ;
#109233 = ORIENTED_EDGE ( 'NONE', *, *, #32972, .T. ) ;
#109234 = DIRECTION ( 'NONE',  ( -0.6830127018922180770, -0.6830127018922204085, -0.2588190451025213501 ) ) ;
#109235 = DIRECTION ( 'NONE',  ( 0.000000000000000000, -1.000000000000000000, 0.000000000000000000 ) ) ;
#109236 = CARTESIAN_POINT ( 'NONE',  ( 96.25043019189810423, 3.055000000000002824, -5.291415217122919401 ) ) ;
#109237 = CARTESIAN_POINT ( 'NONE',  ( 9.096670641874002428, -2.240707523384257716, 15.26439735382754570 ) ) ;
#109239 = CARTESIAN_POINT ( 'NONE',  ( 39.18398860626899705, 28.73617430169814568, 5.000000000000000000 ) ) ;
#109238 = DIRECTION ( 'NONE',  ( 0.7071067811865486830, -0.7071067811865464625, -0.000000000000000000 ) ) ;
#109240 = VERTEX_POINT ( 'NONE', #101257 ) ;
#109241 = CARTESIAN_POINT ( 'NONE',  ( 5.207106781186512379, 0.7592924766157120864, 5.000000000000000000 ) ) ;
#109242 = LINE ( 'NONE', #9926, #86495 ) ;
#109243 = LINE ( 'NONE', #130312, #118520 ) ;
#109244 = CIRCLE ( 'NONE', #123140, 3.000000000000001332 ) ;
#109245 = LINE ( 'NONE', #10627, #140122 ) ;
#109246 = ORIENTED_EDGE ( 'NONE', *, *, #73001, .F. ) ;
#109247 = VECTOR ( 'NONE', #80162, 1000.000000000000114 ) ;
#109248 = CARTESIAN_POINT ( 'NONE',  ( 3.489213562373097322, -27.52281430457057709, 5.000000000000000000 ) ) ;
#109249 = ORIENTED_EDGE ( 'NONE', *, *, #137253, .F. ) ;
#109250 = VECTOR ( 'NONE', #99990, 1000.000000000000000 ) ;
#109251 = ORIENTED_EDGE ( 'NONE', *, *, #110960, .T. ) ;
#109252 = VERTEX_POINT ( 'NONE', #91803 ) ;
#109253 = CARTESIAN_POINT ( 'NONE',  ( 121.9745968585647802, 1.637169565754164280, -6.109999999999996767 ) ) ;
#109254 = ORIENTED_EDGE ( 'NONE', *, *, #18606, .T. ) ;
#109255 = VECTOR ( 'NONE', #112883, 1000.000000000000000 ) ;
#109256 = CARTESIAN_POINT ( 'NONE',  ( 28.49999999999980460, -19.53360074219753884, 5.000000000000000000 ) ) ;
#109257 = DIRECTION ( 'NONE',  ( -0.7071067811865487940, -0.7071067811865463515, -0.000000000000000000 ) ) ;
#109258 = ADVANCED_FACE ( 'NONE', ( #91128 ), #123754, .T. ) ;
#109259 = EDGE_LOOP ( 'NONE', ( #74236, #106810, #114064, #137040 ) ) ;
#109260 = CARTESIAN_POINT ( 'NONE',  ( 17.67183060077634593, -6.740707523384211086, 4.000000000000000000 ) ) ;
#109261 = ORIENTED_EDGE ( 'NONE', *, *, #83682, .T. ) ;
#109262 = VECTOR ( 'NONE', #54683, 1000.000000000000000 ) ;
#109263 = EDGE_CURVE ( 'NONE', #3502, #94791, #46208, .T. ) ;
#109264 = EDGE_CURVE ( 'NONE', #55786, #97574, #136026, .T. ) ;
#109265 = EDGE_CURVE ( 'NONE', #139877, #73811, #41412, .T. ) ;
#109266 = CARTESIAN_POINT ( 'NONE',  ( 16.16623647476855652, 7.934999999999990727, -1.457635852685135314E-15 ) ) ;
#109267 = LINE ( 'NONE', #121560, #60198 ) ;
#109268 = EDGE_CURVE ( 'NONE', #46985, #132831, #67970, .T. ) ;
#109269 = DIRECTION ( 'NONE',  ( 0.6830127018922180770, -0.6830127018922204085, -0.2588190451025213501 ) ) ;
#109270 = DIRECTION ( 'NONE',  ( -0.000000000000000000, 0.3543493200069153248, 0.9351131265310292928 ) ) ;
#109271 = ORIENTED_EDGE ( 'NONE', *, *, #141882, .T. ) ;
#109272 = VERTEX_POINT ( 'NONE', #14950 ) ;
#109273 = EDGE_CURVE ( 'NONE', #73811, #139877, #5193, .T. ) ;
#109274 = CIRCLE ( 'NONE', #39876, 2.500000000000000888 ) ;
#109275 = ORIENTED_EDGE ( 'NONE', *, *, #133245, .F. ) ;
#109276 = CARTESIAN_POINT ( 'NONE',  ( 30.18398860626900060, 28.73617430169808173, 5.000000000000000000 ) ) ;
#109277 = VECTOR ( 'NONE', #118750, 1000.000000000000227 ) ;
#109278 = ADVANCED_FACE ( 'NONE', ( #79784 ), #123262, .F. ) ;
#109279 = CARTESIAN_POINT ( 'NONE',  ( 5.380000000000000782, 2.055000000000001492, 0.000000000000000000 ) ) ;
#109280 = LINE ( 'NONE', #12096, #25091 ) ;
#109281 = PLANE ( 'NONE',  #54988 ) ;
#109282 = EDGE_CURVE ( 'NONE', #63170, #120276, #36239, .T. ) ;
#109283 = DIRECTION ( 'NONE',  ( -0.7071067811865486830, 0.7071067811865464625, 0.000000000000000000 ) ) ;
#109284 = CARTESIAN_POINT ( 'NONE',  ( 34.56293019189810423, 1.637169565754157174, 6.110000000000002984 ) ) ;
#109285 = DIRECTION ( 'NONE',  ( -0.7071067811865486830, -0.7071067811865464625, -0.000000000000000000 ) ) ;
#109286 = ORIENTED_EDGE ( 'NONE', *, *, #94469, .T. ) ;
#109287 = DIRECTION ( 'NONE',  ( 0.6830127018922180770, -0.6830127018922204085, -0.2588190451025213501 ) ) ;
#109288 = ORIENTED_EDGE ( 'NONE', *, *, #72917, .F. ) ;
#109289 = LINE ( 'NONE', #63676, #33762 ) ;
#109290 = VERTEX_POINT ( 'NONE', #92022 ) ;
#109291 =( BOUNDED_CURVE ( )  B_SPLINE_CURVE ( 2, ( #21648, #43401, #97771, #10732, #41981, #86191, #99166, #130421, #142018, #31108, #120196, #20907, #143413 ),
 .UNSPECIFIED., .F., .T. ) 
 B_SPLINE_CURVE_WITH_KNOTS ( ( 3, 2, 2, 2, 2, 2, 3 ),
 ( 0.09999999999999995004, 0.1027777777777777179, 0.1055555555555555136, 0.1083333333333332954, 0.1111111111111110633, 0.1138888888888888590, 0.1166666666666666408 ),
 .UNSPECIFIED. ) 
 CURVE ( )  GEOMETRIC_REPRESENTATION_ITEM ( )  RATIONAL_B_SPLINE_CURVE ( ( 1.000000000000000666, 0.9659258262890676461, 1.000000000000000000, 0.9659258262890683122, 1.000000000000000000, 0.9659258262890683122, 1.000000000000000000, 0.9659258262890683122, 1.000000000000000000, 0.9659258262890683122, 1.000000000000000000, 0.9659258262890686453, 0.9999999999999996669 ) ) 
 REPRESENTATION_ITEM ( '' )  );
#109292 = ADVANCED_FACE ( 'NONE', ( #37676 ), #58751, .T. ) ;
#109293 = DIRECTION ( 'NONE',  ( -0.7071067811865487940, 0.7071067811865463515, -0.000000000000000000 ) ) ;
#109295 = ORIENTED_EDGE ( 'NONE', *, *, #9778, .F. ) ;
#109294 = DIRECTION ( 'NONE',  ( -0.7071067811865486830, -0.7071067811865464625, 0.000000000000000000 ) ) ;
#109296 = LINE ( 'NONE', #7825, #81608 ) ;
#109297 = EDGE_LOOP ( 'NONE', ( #76668, #46639, #120904, #103989 ) ) ;
#109298 = CARTESIAN_POINT ( 'NONE',  ( 2.700255128608413990, -27.71228299555204089, 4.000000000000000000 ) ) ;
#109300 = VERTEX_POINT ( 'NONE', #67459 ) ;
#109299 = VECTOR ( 'NONE', #529, 1000.000000000000000 ) ;
#109301 = DIRECTION ( 'NONE',  ( 0.7071067811865487940, -0.7071067811865463515, 0.000000000000000000 ) ) ;
#109302 = ORIENTED_EDGE ( 'NONE', *, *, #38960, .F. ) ;
#109303 = ADVANCED_FACE ( 'NONE', ( #59439 ), #111652, .F. ) ;
#109304 = LINE ( 'NONE', #95565, #133173 ) ;
#109305 = CARTESIAN_POINT ( 'NONE',  ( 111.3500270504628986, -5.819803920172572198, -5.819803920172572198 ) ) ;
#109306 = LINE ( 'NONE', #53509, #60112 ) ;
#109307 = LINE ( 'NONE', #44066, #53169 ) ;
#109308 = CARTESIAN_POINT ( 'NONE',  ( -13.49999999999990763, 16.08746187583908238, 4.000000000000000000 ) ) ;
#109309 = DIRECTION ( 'NONE',  ( -0.7071067811865486830, -0.7071067811865464625, 0.000000000000000000 ) ) ;
#109310 = CARTESIAN_POINT ( 'NONE',  ( 18.63999999999999702, 2.055000000000001492, 0.000000000000000000 ) ) ;
#109311 = CARTESIAN_POINT ( 'NONE',  ( 2.187499999999999556, 4.461849672132297329, -4.461849672132302658 ) ) ;
#109312 = CARTESIAN_POINT ( 'NONE',  ( 19.66623647476855297, 7.934999999999990727, -1.457635852685135314E-15 ) ) ;
#109313 = AXIS2_PLACEMENT_3D ( 'NONE', #84366, #40153, #96589 ) ;
#109314 = AXIS2_PLACEMENT_3D ( 'NONE', #41312, #22398, #33354 ) ;
#109316 = FACE_OUTER_BOUND ( 'NONE', #82310, .T. ) ;
#109315 = VECTOR ( 'NONE', #28251, 1000.000000000000000 ) ;
#109317 = CARTESIAN_POINT ( 'NONE',  ( 32.99999999999976552, 12.83542986846999945, -1.025386466790447093 ) ) ;
#109318 = ORIENTED_EDGE ( 'NONE', *, *, #56835, .F. ) ;
#109319 = VERTEX_POINT ( 'NONE', #89876 ) ;
#109320 = AXIS2_PLACEMENT_3D ( 'NONE', #131555, #19216, #75059 ) ;
#109321 = AXIS2_PLACEMENT_3D ( 'NONE', #30420, #97806, #76065 ) ;
#109322 = CARTESIAN_POINT ( 'NONE',  ( -47.99451991528749062, 28.92564299267971251, 4.000000000000000000 ) ) ;
#109323 = VERTEX_POINT ( 'NONE', #34812 ) ;
#109324 = ADVANCED_FACE ( 'NONE', ( #79058 ), #23934, .T. ) ;
#109325 = CARTESIAN_POINT ( 'NONE',  ( -25.49999999999981526, 16.46639925780209879, 5.000000000000000000 ) ) ;
#109326 = DIRECTION ( 'NONE',  ( -0.000000000000000000, 0.3543493200069153248, 0.9351131265310292928 ) ) ;
#109327 = AXIS2_PLACEMENT_3D ( 'NONE', #134491, #114831, #70682 ) ;
#109328 = VECTOR ( 'NONE', #103936, 1000.000000000000227 ) ;
#109329 = CARTESIAN_POINT ( 'NONE',  ( 34.45011844616453800, 21.00230414159372216, 5.000000000000001776 ) ) ;
#109330 = ORIENTED_EDGE ( 'NONE', *, *, #33086, .F. ) ;
#109331 = DIRECTION ( 'NONE',  ( -1.000000000000000000, -1.224606353822377258E-16, -0.000000000000000000 ) ) ;
#109332 = DIRECTION ( 'NONE',  ( 0.000000000000000000, 1.000000000000000000, 0.000000000000000000 ) ) ;
#109333 = ADVANCED_FACE ( 'NONE', ( #2120 ), #104306, .F. ) ;
#109334 = LINE ( 'NONE', #10015, #120590 ) ;
#109335 = DIRECTION ( 'NONE',  ( 0.000000000000000000, 0.000000000000000000, 1.000000000000000000 ) ) ;
#109336 = CARTESIAN_POINT ( 'NONE',  ( 0.000000000000000000, -49.85820393249939286, 34.92500000000001847 ) ) ;
#109338 = VERTEX_POINT ( 'NONE', #71726 ) ;
#109337 = CARTESIAN_POINT ( 'NONE',  ( 9.994118527364397764, 4.584330080086930965E-16, 0.000000000000000000 ) ) ;
#109339 = DIRECTION ( 'NONE',  ( 0.7071067811865487940, 0.7071067811865463515, -0.000000000000000000 ) ) ;
#109340 = DIRECTION ( 'NONE',  ( -0.000000000000000000, 0.000000000000000000, 1.000000000000000000 ) ) ;
#109341 =( NAMED_UNIT ( * ) PLANE_ANGLE_UNIT ( ) SI_UNIT ( $, .RADIAN. ) );
#109342 = LINE ( 'NONE', #63720, #128917 ) ;
#109343 = EDGE_CURVE ( 'NONE', #123719, #110682, #105042, .T. ) ;
#109344 = DIRECTION ( 'NONE',  ( 0.3543493200069162685, -0.000000000000000000, -0.9351131265310288487 ) ) ;
#109345 = VERTEX_POINT ( 'NONE', #40521 ) ;
#109346 = VERTEX_POINT ( 'NONE', #63004 ) ;
#109347 = ORIENTED_EDGE ( 'NONE', *, *, #101502, .T. ) ;
#109348 = CARTESIAN_POINT ( 'NONE',  ( 91.87543019189811844, -5.291415217122920289, -3.055000000000001492 ) ) ;
#109349 = VERTEX_POINT ( 'NONE', #96271 ) ;
#109350 = EDGE_CURVE ( 'NONE', #82894, #43938, #138391, .T. ) ;
#109351 = CARTESIAN_POINT ( 'NONE',  ( 21.51665438641029482, 22.22500000000000142, 4.500000000000000888 ) ) ;
#109352 = DIRECTION ( 'NONE',  ( 0.6830127018922180770, 0.6830127018922202975, -0.2588190451025213501 ) ) ;
#109353 = ORIENTED_EDGE ( 'NONE', *, *, #82956, .T. ) ;
#109354 = CARTESIAN_POINT ( 'NONE',  ( 183.9346320274810012, -51.67626207039724306, 38.40320453011148771 ) ) ;
#109355 = DIRECTION ( 'NONE',  ( 0.7071067811865487940, 0.7071067811865463515, -0.000000000000000000 ) ) ;
#109356 = AXIS2_PLACEMENT_3D ( 'NONE', #17731, #62009, #65598 ) ;
#109357 = CARTESIAN_POINT ( 'NONE',  ( 81.87043019189812298, -3.055000000000001492, 5.291415217122917625 ) ) ;
#109358 = ORIENTED_EDGE ( 'NONE', *, *, #138454, .T. ) ;
#109359 = AXIS2_PLACEMENT_3D ( 'NONE', #9937, #57058, #43302 ) ;
#109360 = DIRECTION ( 'NONE',  ( -0.6830127018922180770, -0.6830127018922204085, -0.2588190451025213501 ) ) ;
#109361 = ORIENTED_EDGE ( 'NONE', *, *, #64232, .F. ) ;
#109362 = EDGE_LOOP ( 'NONE', ( #21438, #101445, #82790, #116280 ) ) ;
#109363 = ADVANCED_FACE ( 'NONE', ( #71019 ), #29608, .F. ) ;
#109364 = ORIENTED_EDGE ( 'NONE', *, *, #27124, .T. ) ;
#109365 = CARTESIAN_POINT ( 'NONE',  ( -27.48921356237309155, -27.52281430457074762, 5.000000000000000000 ) ) ;
#109366 = EDGE_CURVE ( 'NONE', #133408, #39160, #7116, .T. ) ;
#109367 = DIRECTION ( 'NONE',  ( 0.6830127018922180770, -0.6830127018922204085, -0.2588190451025213501 ) ) ;
#109368 = CARTESIAN_POINT ( 'NONE',  ( 18.29623647476855197, 7.934999999999990727, -1.457635852685135314E-15 ) ) ;
#109369 = CARTESIAN_POINT ( 'NONE',  ( -8.999999999999928946, 19.55218569542897100, 5.000000000000000000 ) ) ;
#109370 = CARTESIAN_POINT ( 'NONE',  ( 166.8575281714868765, 26.96999999999993847, 32.10205088422555519 ) ) ;
#109371 = LINE ( 'NONE', #593, #39530 ) ;
#109372 =( NAMED_UNIT ( * ) PLANE_ANGLE_UNIT ( ) SI_UNIT ( $, .RADIAN. ) );
#109373 = EDGE_CURVE ( 'NONE', #56845, #7390, #93463, .T. ) ;
#109374 = VERTEX_POINT ( 'NONE', #115889 ) ;
#109375 = VERTEX_POINT ( 'NONE', #84723 ) ;
#109376 = FACE_OUTER_BOUND ( 'NONE', #79317, .T. ) ;
#109377 = ORIENTED_EDGE ( 'NONE', *, *, #128585, .F. ) ;
#109378 = ORIENTED_EDGE ( 'NONE', *, *, #140564, .T. ) ;
#109379 = VECTOR ( 'NONE', #50528, 1000.000000000000000 ) ;
#109380 = CIRCLE ( 'NONE', #102477, 6.000000000000001776 ) ;
#109381 = ADVANCED_FACE ( 'NONE', ( #50661 ), #105728, .F. ) ;
#109382 = EDGE_CURVE ( 'NONE', #141003, #134564, #126780, .T. ) ;
#109384 = ADVANCED_FACE ( 'NONE', ( #39827 ), #95590, .F. ) ;
#109383 = CARTESIAN_POINT ( 'NONE',  ( -8.994519915287490619, 28.92564299267944250, 4.000000000000000000 ) ) ;
#109385 = ORIENTED_EDGE ( 'NONE', *, *, #86243, .F. ) ;
#109386 = CARTESIAN_POINT ( 'NONE',  ( 24.32816939922336630, 14.25929247661557397, 4.000000000000000000 ) ) ;
#109387 = CARTESIAN_POINT ( 'NONE',  ( 25.82816939922335209, -5.240707523384228850, 4.000000000000000000 ) ) ;
#109388 = CARTESIAN_POINT ( 'NONE',  ( -39.48921356237310221, -27.52281430457082934, 5.000000000000000000 ) ) ;
#109389 = PLANE ( 'NONE',  #134087 ) ;
#109390 = AXIS2_PLACEMENT_3D ( 'NONE', #104344, #122729, #121298 ) ;
#109391 = CARTESIAN_POINT ( 'NONE',  ( -80.99451991528748351, 28.92564299267994699, 4.000000000000000000 ) ) ;
#109392 = ORIENTED_EDGE ( 'NONE', *, *, #57956, .T. ) ;
#109393 = CARTESIAN_POINT ( 'NONE',  ( 28.49999999999981881, -17.94781430457063820, 5.000000000000000000 ) ) ;
#109394 = EDGE_LOOP ( 'NONE', ( #56903, #78678, #24872, #82641 ) ) ;
#109395 = CARTESIAN_POINT ( 'NONE',  ( -30.79289321881324781, 9.759292476615621936, 5.000000000000000000 ) ) ;
#109396 = ORIENTED_EDGE ( 'NONE', *, *, #124735, .T. ) ;
#109397 = CARTESIAN_POINT ( 'NONE',  ( 116.3083603837962130, 7.949999999999996625, 2.130196079827431088 ) ) ;
#109398 = ADVANCED_FACE ( 'NONE', ( #15841 ), #51397, .T. ) ;
#109399 = VERTEX_POINT ( 'NONE', #72469 ) ;
#109400 = CARTESIAN_POINT ( 'NONE',  ( 0.6048623318752055500, 21.75929247661549226, 21.32995629748186417 ) ) ;
#109401 = ORIENTED_EDGE ( 'NONE', *, *, #7862, .F. ) ;
#109402 = ORIENTED_EDGE ( 'NONE', *, *, #64450, .T. ) ;
#109403 = VECTOR ( 'NONE', #26085, 1000.000000000000000 ) ;
#109404 = ORIENTED_EDGE ( 'NONE', *, *, #116627, .T. ) ;
#109405 = CARTESIAN_POINT ( 'NONE',  ( 10.78501580275803562, -3.740707523384244837, 15.76143240460126371 ) ) ;
#109406 = FACE_OUTER_BOUND ( 'NONE', #49059, .T. ) ;
#109407 = CARTESIAN_POINT ( 'NONE',  ( -7.171830600776415210, -17.24070752338409918, 4.000000000000000000 ) ) ;
#109408 = CARTESIAN_POINT ( 'NONE',  ( 124.9795968585647756, 6.109999999999999432, 1.637169565754164280 ) ) ;
#109409 = LINE ( 'NONE', #120991, #40413 ) ;
#109410 = DIRECTION ( 'NONE',  ( 0.6830127018922180770, -0.6830127018922204085, -0.2588190451025213501 ) ) ;
#109411 = DIRECTION ( 'NONE',  ( -0.000000000000000000, -0.3543493200069152693, 0.9351131265310292928 ) ) ;
#109412 = VECTOR ( 'NONE', #66154, 1000.000000000000114 ) ;
#109413 = VECTOR ( 'NONE', #47727, 1000.000000000000227 ) ;
#109414 = CARTESIAN_POINT ( 'NONE',  ( -9.712309939660212166, -21.73547319004781642, 4.999917730833664642 ) ) ;
#109415 = AXIS2_PLACEMENT_3D ( 'NONE', #55991, #22577, #67583 ) ;
#109416 = AXIS2_PLACEMENT_3D ( 'NONE', #67730, #123532, #111167 ) ;
#109417 = DIRECTION ( 'NONE',  ( -0.6830127018922180770, -0.6830127018922204085, -0.2588190451025213501 ) ) ;
#109418 = CARTESIAN_POINT ( 'NONE',  ( -25.82816939922334853, 9.759292476615621936, 4.000000000000000000 ) ) ;
#109419 = CARTESIAN_POINT ( 'NONE',  ( -26.20710678118635784, 0.7592924766157156391, 5.000000000000000000 ) ) ;
#109420 = VERTEX_POINT ( 'NONE', #60139 ) ;
#109421 = EDGE_LOOP ( 'NONE', ( #129175, #101251, #111845, #65063 ) ) ;
#109422 = VECTOR ( 'NONE', #131460, 1000.000000000000227 ) ;
#109423 = ORIENTED_EDGE ( 'NONE', *, *, #125688, .F. ) ;
#109424 = VECTOR ( 'NONE', #15675, 1000.000000000000227 ) ;
#109425 = CARTESIAN_POINT ( 'NONE',  ( 2.999999999999975131, -13.39766691384883224, -10.96608748226466545 ) ) ;
#109426 = ORIENTED_EDGE ( 'NONE', *, *, #77385, .T. ) ;
#109427 = ORIENTED_EDGE ( 'NONE', *, *, #55881, .F. ) ;
#109428 = CARTESIAN_POINT ( 'NONE',  ( -54.18398860626899705, 28.73617430169825226, 5.000000000000000000 ) ) ;
#109429 = LINE ( 'NONE', #12249, #133516 ) ;
#109430 = DIRECTION ( 'NONE',  ( 0.7071067811865487940, 0.7071067811865463515, -0.000000000000000000 ) ) ;
#109431 = VERTEX_POINT ( 'NONE', #106427 ) ;
#109432 = CARTESIAN_POINT ( 'NONE',  ( -12.69999999999998153, 0.000000000000000000, 2.500000000000000444 ) ) ;
#109433 = ORIENTED_EDGE ( 'NONE', *, *, #20715, .T. ) ;
#109434 = FACE_OUTER_BOUND ( 'NONE', #74926, .T. ) ;
#109435 = EDGE_CURVE ( 'NONE', #91210, #38530, #3801, .T. ) ;
#109436 = VECTOR ( 'NONE', #114110, 1000.000000000000000 ) ;
#109437 = CARTESIAN_POINT ( 'NONE',  ( 23.10873647476855552, -5.808823158059033709, 5.808823158059035485 ) ) ;
#109438 = EDGE_LOOP ( 'NONE', ( #65446, #1517, #8987, #75551 ) ) ;
#109439 = CARTESIAN_POINT ( 'NONE',  ( 91.20376352523145158, 6.109999999999999432, 1.122388791418549108E-15 ) ) ;
#109440 = EDGE_CURVE ( 'NONE', #107596, #75676, #82585, .T. ) ;
#109441 = DIRECTION ( 'NONE',  ( 0.7071067811865486830, -0.7071067811865464625, -0.000000000000000000 ) ) ;
#109442 = EDGE_CURVE ( 'NONE', #93231, #19799, #30340, .T. ) ;
#109443 = PLANE ( 'NONE',  #25817 ) ;
#109444 = CARTESIAN_POINT ( 'NONE',  ( -27.71230993966009493, -21.73547319004781642, 4.999917730833664642 ) ) ;
#109445 = EDGE_LOOP ( 'NONE', ( #43331, #98244, #6288, #85709 ) ) ;
#109446 = VERTEX_POINT ( 'NONE', #76732 ) ;
#109447 = EDGE_CURVE ( 'NONE', #26808, #141246, #7643, .T. ) ;
#109448 = ORIENTED_EDGE ( 'NONE', *, *, #65, .F. ) ;
#109449 = PLANE ( 'NONE',  #92654 ) ;
#109450 = LINE ( 'NONE', #133365, #67314 ) ;
#109451 = LINE ( 'NONE', #98570, #49694 ) ;
#109452 = ADVANCED_FACE ( 'NONE', ( #88308 ), #9251, .F. ) ;
#109453 = PLANE ( 'NONE',  #79708 ) ;
#109454 = ORIENTED_EDGE ( 'NONE', *, *, #39977, .F. ) ;
#109455 = VECTOR ( 'NONE', #100696, 1000.000000000000000 ) ;
#109456 = LINE ( 'NONE', #32632, #34623 ) ;
#109457 = VECTOR ( 'NONE', #22753, 1000.000000000000000 ) ;
#109458 = EDGE_CURVE ( 'NONE', #36583, #93715, #54274, .T. ) ;
#109459 = DIRECTION ( 'NONE',  ( -0.7071067811865487940, 0.7071067811865463515, 0.000000000000000000 ) ) ;
#109460 = DIRECTION ( 'NONE',  ( 0.000000000000000000, 0.000000000000000000, 1.000000000000000000 ) ) ;
#109461 = VERTEX_POINT ( 'NONE', #10693 ) ;
#109462 = CARTESIAN_POINT ( 'NONE',  ( -14.81601139373099585, 28.73617430169776910, 5.000000000000000000 ) ) ;
#109463 = AXIS2_PLACEMENT_3D ( 'NONE', #1265, #33938, #78154 ) ;
#109464 = VECTOR ( 'NONE', #18559, 999.9999999999998863 ) ;
#109465 = DIRECTION ( 'NONE',  ( -0.7071067811865486830, 0.7071067811865464625, 0.000000000000000000 ) ) ;
#109466 = EDGE_LOOP ( 'NONE', ( #91314, #96569, #10771, #138019 ) ) ;
#109467 = ADVANCED_FACE ( 'NONE', ( #129639 ), #48309, .T. ) ;
#109469 = ORIENTED_EDGE ( 'NONE', *, *, #76868, .F. ) ;
#109468 = CARTESIAN_POINT ( 'NONE',  ( -69.48921356237309510, -27.52281430457103895, 5.000000000000000000 ) ) ;
#109470 = EDGE_LOOP ( 'NONE', ( #91078, #39922, #97761, #93036 ) ) ;
#109471 = EDGE_CURVE ( 'NONE', #92475, #12567, #89031, .T. ) ;
#109472 = LINE ( 'NONE', #9400, #47043 ) ;
#109473 = DIRECTION ( 'NONE',  ( 0.7071067811865487940, 0.7071067811865463515, 0.000000000000000000 ) ) ;
#109474 = ORIENTED_EDGE ( 'NONE', *, *, #60355, .F. ) ;
#109475 = DIRECTION ( 'NONE',  ( 0.7071067811865487940, 0.7071067811865463515, -0.000000000000000000 ) ) ;
#109477 = EDGE_CURVE ( 'NONE', #102386, #111653, #100610, .T. ) ;
#109476 =( BOUNDED_CURVE ( )  B_SPLINE_CURVE ( 3, ( #88851, #46807, #24974, #67085 ),
 .UNSPECIFIED., .F., .T. ) 
 B_SPLINE_CURVE_WITH_KNOTS ( ( 4, 4 ),
 ( 1.208578181583235045, 1.359146454359427825 ),
 .UNSPECIFIED. ) 
 CURVE ( )  GEOMETRIC_REPRESENTATION_ITEM ( )  RATIONAL_B_SPLINE_CURVE ( ( 1.000000000000000000, 0.9981116584018955296, 0.9981116584018955296, 1.000000000000000000 ) ) 
 REPRESENTATION_ITEM ( '' )  );
#109478 = VECTOR ( 'NONE', #140657, 1000.000000000000000 ) ;
#109479 = LINE ( 'NONE', #118179, #112360 ) ;
#109480 = FACE_OUTER_BOUND ( 'NONE', #17391, .T. ) ;
#109481 = CARTESIAN_POINT ( 'NONE',  ( -9.005480084712511157, 28.92564299267931816, 4.000000000000000000 ) ) ;
#109482 = CARTESIAN_POINT ( 'NONE',  ( 0.1600000000000006972, -7.413834132789976827, 2.908321245901498209 ) ) ;
#109483 = FACE_OUTER_BOUND ( 'NONE', #20131, .T. ) ;
#109484 = FACE_OUTER_BOUND ( 'NONE', #43388, .T. ) ;
#109485 = DIRECTION ( 'NONE',  ( -0.7071067811865486830, 0.7071067811865464625, 0.000000000000000000 ) ) ;
#109486 = CARTESIAN_POINT ( 'NONE',  ( -2.999999999999975131, -19.06887692260761469, 4.000000000000000000 ) ) ;
#109487 = CARTESIAN_POINT ( 'NONE',  ( -48.18398860626899705, 28.73617430169820608, 5.000000000000000000 ) ) ;
#109488 = VECTOR ( 'NONE', #134133, 1000.000000000000000 ) ;
#109489 = LINE ( 'NONE', #54427, #20566 ) ;
#109490 = DIRECTION ( 'NONE',  ( 0.000000000000000000, -1.000000000000000000, 0.000000000000000000 ) ) ;
#109491 = LINE ( 'NONE', #75448, #45452 ) ;
#109492 = ORIENTED_EDGE ( 'NONE', *, *, #67754, .T. ) ;
#109493 = EDGE_LOOP ( 'NONE', ( #11637, #47614, #87526, #53862 ) ) ;
#109494 = ORIENTED_EDGE ( 'NONE', *, *, #12283, .T. ) ;
#109495 = CARTESIAN_POINT ( 'NONE',  ( 101.1874999999999858, -5.819803920172573086, 5.819803920172572198 ) ) ;
#109496 = EDGE_LOOP ( 'NONE', ( #7221, #58979, #10857, #124107 ) ) ;
#109497 = VERTEX_POINT ( 'NONE', #135396 ) ;
#109498 = ORIENTED_EDGE ( 'NONE', *, *, #30459, .T. ) ;
#109499 = ADVANCED_FACE ( 'NONE', ( #58582 ), #125207, .F. ) ;
#109500 = DIRECTION ( 'NONE',  ( 1.000000000000000000, 0.000000000000000000, 0.000000000000000000 ) ) ;
#109501 = CARTESIAN_POINT ( 'NONE',  ( 89.37500000000000000, 7.950000000000000178, 1.460391307983218535E-15 ) ) ;
#109502 = AXIS2_PLACEMENT_3D ( 'NONE', #108434, #141088, #87457 ) ;
#109503 = ORIENTED_EDGE ( 'NONE', *, *, #1429, .T. ) ;
#109504 = LINE ( 'NONE', #142849, #4575 ) ;
#109505 = FACE_OUTER_BOUND ( 'NONE', #116346, .T. ) ;
#109506 = PLANE ( 'NONE',  #97302 ) ;
#109507 = DIRECTION ( 'NONE',  ( 0.000000000000000000, -1.000000000000000000, 0.000000000000000000 ) ) ;
#109508 = ORIENTED_EDGE ( 'NONE', *, *, #137605, .F. ) ;
#109509 = CARTESIAN_POINT ( 'NONE',  ( 14.45613577907006331, 4.931321518839284046, -31.93570391306389666 ) ) ;
#109511 =( GEOMETRIC_REPRESENTATION_CONTEXT ( 3 ) GLOBAL_UNCERTAINTY_ASSIGNED_CONTEXT ( ( #34434 ) ) GLOBAL_UNIT_ASSIGNED_CONTEXT ( ( #86886, #109341, #142686 ) ) REPRESENTATION_CONTEXT ( 'NONE', 'WORKASPACE' ) );
#109510 = CARTESIAN_POINT ( 'NONE',  ( -8.510786437626906675, -27.52281430457049183, 5.000000000000000000 ) ) ;
#109512 = LINE ( 'NONE', #9448, #130818 ) ;
#109513 = FACE_OUTER_BOUND ( 'NONE', #125187, .T. ) ;
#109514 = LINE ( 'NONE', #32691, #38487 ) ;
#109515 = CARTESIAN_POINT ( 'NONE',  ( 28.07919371712955225, 3.975000000000002753, -6.884901960086283523 ) ) ;
#109516 = EDGE_CURVE ( 'NONE', #48278, #22430, #122318, .T. ) ;
#109517 = LINE ( 'NONE', #22476, #120945 ) ;
#109518 = ORIENTED_EDGE ( 'NONE', *, *, #23688, .T. ) ;
#109519 = ORIENTED_EDGE ( 'NONE', *, *, #52687, .F. ) ;
#109520 = CARTESIAN_POINT ( 'NONE',  ( 118.1254301918981184, 5.291415217122919401, 3.055000000000002824 ) ) ;
#109521 = VERTEX_POINT ( 'NONE', #114320 ) ;
#109522 = DIRECTION ( 'NONE',  ( -1.000000000000000000, -0.000000000000000000, -0.000000000000000000 ) ) ;
#109523 = EDGE_CURVE ( 'NONE', #90471, #19069, #22992, .T. ) ;
#109524 = CARTESIAN_POINT ( 'NONE',  ( -60.48921356237309510, -27.52281430457097500, 5.000000000000000000 ) ) ;
#109525 = VECTOR ( 'NONE', #60843, 1000.000000000000000 ) ;
#109526 = DIRECTION ( 'NONE',  ( 0.6830127018922181881, 0.6830127018922202975, -0.2588190451025214056 ) ) ;
#109527 = CARTESIAN_POINT ( 'NONE',  ( 156.1500000000000057, -49.14999999999999147, 49.92499999999997584 ) ) ;
#109528 = DIRECTION ( 'NONE',  ( 0.6830127018922181881, 0.6830127018922202975, -0.2588190451025214056 ) ) ;
#109530 = AXIS2_PLACEMENT_3D ( 'NONE', #6484, #138493, #84138 ) ;
#109529 =( LENGTH_UNIT ( ) NAMED_UNIT ( * ) SI_UNIT ( .MILLI., .METRE. ) );
#109531 = CARTESIAN_POINT ( 'NONE',  ( 127.9537635252314658, -6.109999999999998543, -3.741295971395162543E-16 ) ) ;
#109532 = ORIENTED_EDGE ( 'NONE', *, *, #105117, .F. ) ;
#109533 = EDGE_CURVE ( 'NONE', #16928, #76456, #13557, .T. ) ;
#109534 = VERTEX_POINT ( 'NONE', #3396 ) ;
#109535 = AXIS2_PLACEMENT_3D ( 'NONE', #16067, #94373, #28432 ) ;
#109536 = CARTESIAN_POINT ( 'NONE',  ( -28.49999999999979750, -12.66682484999668468, -0.6294897503864617105 ) ) ;
#109537 = CARTESIAN_POINT ( 'NONE',  ( 26.50183651486027969, -17.24070752338409918, 8.407044977365165650 ) ) ;
#109538 = VERTEX_POINT ( 'NONE', #23756 ) ;
#109539 = CARTESIAN_POINT ( 'NONE',  ( 42.29209685856477563, -5.291415217122921177, 3.054999999999999272 ) ) ;
#109540 = ADVANCED_FACE ( 'NONE', ( #14996 ), #25161, .T. ) ;
#109541 = ORIENTED_EDGE ( 'NONE', *, *, #83391, .T. ) ;
#109542 = DIRECTION ( 'NONE',  ( -0.000000000000000000, 0.000000000000000000, 1.000000000000000000 ) ) ;
#109543 = CARTESIAN_POINT ( 'NONE',  ( -22.21498419724176188, -3.740707523384238176, 15.76143240460118733 ) ) ;
#109544 = VECTOR ( 'NONE', #17625, 1000.000000000000000 ) ;
#109545 = CARTESIAN_POINT ( 'NONE',  ( 38.12043019189811588, 3.055000000000001936, -5.291415217122916737 ) ) ;
#109546 = ORIENTED_EDGE ( 'NONE', *, *, #50281, .F. ) ;
#109547 = CARTESIAN_POINT ( 'NONE',  ( -22.49999999999984013, -12.08601207473290451, -10.46905243149088705 ) ) ;
#109548 = ORIENTED_EDGE ( 'NONE', *, *, #76213, .F. ) ;
#109549 = EDGE_LOOP ( 'NONE', ( #79340, #124612, #94456, #140370 ) ) ;
#109550 = ORIENTED_EDGE ( 'NONE', *, *, #75617, .T. ) ;
#109551 = VECTOR ( 'NONE', #38831, 999.9999999999998863 ) ;
#109552 = CARTESIAN_POINT ( 'NONE',  ( -24.18398860626899705, 28.73617430169804265, 5.000000000000000000 ) ) ;
#109553 = PRODUCT_DEFINITION_SHAPE ( 'NONE', 'NONE',  #143556 ) ;
#109554 = DIRECTION ( 'NONE',  ( 0.7071067811865487940, 0.7071067811865463515, 0.000000000000000000 ) ) ;
#109555 = ADVANCED_FACE ( 'NONE', ( #133249 ), #12148, .F. ) ;
#109556 = VERTEX_POINT ( 'NONE', #36756 ) ;
#109557 = VECTOR ( 'NONE', #76302, 1000.000000000000000 ) ;
#109558 = CARTESIAN_POINT ( 'NONE',  ( 3.710381658649933634, 4.584330080086930965E-16, 0.000000000000000000 ) ) ;
#109559 = CARTESIAN_POINT ( 'NONE',  ( 25.39999999999999858, 1.399999999999986366, 20.40202195861970580 ) ) ;
#109560 = CARTESIAN_POINT ( 'NONE',  ( -8.671830600776406328, -3.740707523384244837, 4.000000000000000000 ) ) ;
#109561 = VECTOR ( 'NONE', #64175, 1000.000000000000000 ) ;
#109562 = EDGE_CURVE ( 'NONE', #102959, #110646, #56430, .T. ) ;
#109563 = FACE_BOUND ( 'NONE', #137107, .T. ) ;
#109564 = ORIENTED_EDGE ( 'NONE', *, *, #131094, .T. ) ;
#109565 = FACE_OUTER_BOUND ( 'NONE', #69117, .T. ) ;
#109566 = CARTESIAN_POINT ( 'NONE',  ( 3.000000000000000888, -47.87246431468552998, 37.20487561447691149 ) ) ;
#109567 = ADVANCED_FACE ( 'NONE', ( #45538 ), #89714, .T. ) ;
#109568 = VERTEX_POINT ( 'NONE', #4071 ) ;
#109569 = CARTESIAN_POINT ( 'NONE',  ( 25.39999999999999503, 3.246059068589359775, 5.158694168414005077 ) ) ;
#109570 = VERTEX_POINT ( 'NONE', #119824 ) ;
#109571 = ORIENTED_EDGE ( 'NONE', *, *, #45421, .F. ) ;
#109572 = EDGE_LOOP ( 'NONE', ( #41373, #53033, #89051, #18982, #15255 ) ) ;
#109573 = AXIS2_PLACEMENT_3D ( 'NONE', #136667, #104762, #103312 ) ;
#109574 = CARTESIAN_POINT ( 'NONE',  ( 44.24543019189810877, -5.291415217122918513, -3.055000000000000160 ) ) ;
#109576 = VERTEX_POINT ( 'NONE', #73009 ) ;
#109575 = VECTOR ( 'NONE', #11912, 1000.000000000000000 ) ;
#109577 = DIRECTION ( 'NONE',  ( 0.7071067811865487940, 0.7071067811865463515, 0.000000000000000000 ) ) ;
#109578 = PRESENTATION_STYLE_ASSIGNMENT (( #22538 ) ) ;
#109579 = CARTESIAN_POINT ( 'NONE',  ( 25.49999999999982236, 10.94296225409029510, -9.576120664313199526 ) ) ;
#109580 = ORIENTED_EDGE ( 'NONE', *, *, #91262, .F. ) ;
#109581 = FACE_OUTER_BOUND ( 'NONE', #109938, .T. ) ;
#109582 = DIRECTION ( 'NONE',  ( -0.000000000000000000, -0.3543493200069152693, 0.9351131265310292928 ) ) ;
#109583 = AXIS2_PLACEMENT_3D ( 'NONE', #115715, #70169, #125215 ) ;
#109584 = ADVANCED_FACE ( 'NONE', ( #81737 ), #137518, .F. ) ;
#109585 = LINE ( 'NONE', #10261, #10776 ) ;
#109586 = DIRECTION ( 'NONE',  ( -1.000000000000000000, 0.000000000000000000, 0.000000000000000000 ) ) ;
#109587 = CARTESIAN_POINT ( 'NONE',  ( 6.471592354503322042, 9.902892378096218942E-16, 0.000000000000000000 ) ) ;
#109588 = LINE ( 'NONE', #140105, #139677 ) ;
#109589 = CARTESIAN_POINT ( 'NONE',  ( 28.49999999999980460, 21.05218569542895324, 5.000000000000000000 ) ) ;
#109590 = ORIENTED_EDGE ( 'NONE', *, *, #23529, .T. ) ;
#109592 = ORIENTED_EDGE ( 'NONE', *, *, #94668, .F. ) ;
#109591 = VECTOR ( 'NONE', #78786, 1000.000000000000000 ) ;
#109593 = EDGE_LOOP ( 'NONE', ( #90613, #63843, #130969, #1677 ) ) ;
#109594 = DIRECTION ( 'NONE',  ( -0.7071067811865486830, 0.7071067811865464625, 0.000000000000000000 ) ) ;
#109595 = CARTESIAN_POINT ( 'NONE',  ( 35.99451991528749772, 28.92564299267963079, 4.000000000000000000 ) ) ;
#109596 = ORIENTED_EDGE ( 'NONE', *, *, #19759, .F. ) ;
#109597 = ORIENTED_EDGE ( 'NONE', *, *, #29745, .T. ) ;
#109598 = DIRECTION ( 'NONE',  ( -0.000000000000000000, 1.000000000000000000, -0.000000000000000000 ) ) ;
#109599 = PLANE ( 'NONE',  #38719 ) ;
#109600 = LINE ( 'NONE', #79163, #20838 ) ;
#109601 = VERTEX_POINT ( 'NONE', #59963 ) ;
#109602 = DIRECTION ( 'NONE',  ( -1.000000000000000000, -1.224606353822377258E-16, -0.000000000000000000 ) ) ;
#109603 = CARTESIAN_POINT ( 'NONE',  ( 2.139447441471317379, 4.584330080086930965E-16, 0.000000000000000000 ) ) ;
#109604 = CARTESIAN_POINT ( 'NONE',  ( 21.50456980810188412, 6.871911579029510442, -3.967499999999998916 ) ) ;
#109605 = EDGE_CURVE ( 'NONE', #74842, #59437, #6228, .T. ) ;
#109606 = VECTOR ( 'NONE', #96198, 1000.000000000000000 ) ;
#109607 = DIRECTION ( 'NONE',  ( -0.6830127018922180770, -0.6830127018922204085, -0.2588190451025213501 ) ) ;
#109608 = ORIENTED_EDGE ( 'NONE', *, *, #136078, .T. ) ;
#109609 = CARTESIAN_POINT ( 'NONE',  ( 123.8704301918981230, -3.055000000000001936, 5.291415217122918513 ) ) ;
#109610 = EDGE_CURVE ( 'NONE', #17066, #89804, #50504, .T. ) ;
#109611 = CARTESIAN_POINT ( 'NONE',  ( -34.92500000000001137, 22.22500000000000142, 4.500000000000000888 ) ) ;
#109612 = CARTESIAN_POINT ( 'NONE',  ( 4.495848767239241539, -2.500000000000000444, 3.061616997868384127E-16 ) ) ;
#109614 = ORIENTED_EDGE ( 'NONE', *, *, #89886, .F. ) ;
#109613 = DIRECTION ( 'NONE',  ( 0.7071067811865487940, 0.7071067811865463515, -0.000000000000000000 ) ) ;
#109615 = LINE ( 'NONE', #63306, #81003 ) ;
#109616 = ORIENTED_EDGE ( 'NONE', *, *, #101594, .F. ) ;
#109617 = LINE ( 'NONE', #130691, #89009 ) ;
#109618 = LINE ( 'NONE', #44406, #125687 ) ;
#109619 = ADVANCED_FACE ( 'NONE', ( #61425 ), #39653, .T. ) ;
#109620 = EDGE_CURVE ( 'NONE', #73002, #75311, #94690, .T. ) ;
#109621 = CARTESIAN_POINT ( 'NONE',  ( 9.682526172861077640, 4.202752102959690472E-16, 0.000000000000000000 ) ) ;
#109623 = VERTEX_POINT ( 'NONE', #49816 ) ;
#109622 = AXIS2_PLACEMENT_3D ( 'NONE', #37766, #103005, #3638 ) ;
#109624 = DIRECTION ( 'NONE',  ( -0.7071067811865486830, 0.7071067811865464625, 0.000000000000000000 ) ) ;
#109625 = DIRECTION ( 'NONE',  ( 0.7071067811865487940, 0.7071067811865463515, -0.000000000000000000 ) ) ;
#109626 = ORIENTED_EDGE ( 'NONE', *, *, #73623, .T. ) ;
#109627 = PRODUCT_DEFINITION_FORMATION_WITH_SPECIFIED_SOURCE ( 'ANY', '', #76820, .NOT_KNOWN. ) ;
#109628 = DIRECTION ( 'NONE',  ( -0.6830127018922181881, 0.6830127018922202975, -0.2588190451025214056 ) ) ;
#109629 = CARTESIAN_POINT ( 'NONE',  ( -42.18398860626899705, 28.73617430169816700, 5.000000000000000000 ) ) ;
#109630 = VERTEX_POINT ( 'NONE', #138223 ) ;
#109631 = EDGE_CURVE ( 'NONE', #41654, #140719, #92545, .T. ) ;
#109632 = LINE ( 'NONE', #141567, #108631 ) ;
#109634 = ORIENTED_EDGE ( 'NONE', *, *, #60366, .T. ) ;
#109633 = DIRECTION ( 'NONE',  ( 0.6830127018922180770, -0.6830127018922204085, -0.2588190451025213501 ) ) ;
#109635 = EDGE_CURVE ( 'NONE', #6599, #97151, #128083, .T. ) ;
#109636 =( REPRESENTATION_RELATIONSHIP ('NONE','NONE', #69070, #104156 ) REPRESENTATION_RELATIONSHIP_WITH_TRANSFORMATION ( #75706 )SHAPE_REPRESENTATION_RELATIONSHIP( ) );
#109637 = VERTEX_POINT ( 'NONE', #38909 ) ;
#109638 = PLANE ( 'NONE',  #17163 ) ;
#109639 = CARTESIAN_POINT ( 'NONE',  ( 14.70692117890024697, 4.584330080086930965E-16, 0.000000000000000000 ) ) ;
#109640 = AXIS2_PLACEMENT_3D ( 'NONE', #51296, #92618, #17219 ) ;
#109641 = VERTEX_POINT ( 'NONE', #138949 ) ;
#109642 = EDGE_CURVE ( 'NONE', #141613, #36536, #15676, .T. ) ;
#109643 = DIRECTION ( 'NONE',  ( 0.7071067811865487940, 0.7071067811865463515, -0.000000000000000000 ) ) ;
#109644 = AXIS2_PLACEMENT_3D ( 'NONE', #10161, #76891, #79037 ) ;
#109645 = LINE ( 'NONE', #108183, #62182 ) ;
#109646 = CARTESIAN_POINT ( 'NONE',  ( 31.49999999999978684, 7.087461875839177416, 4.000000000000000000 ) ) ;
#109647 = ORIENTED_EDGE ( 'NONE', *, *, #64823, .F. ) ;
#109648 = PLANE ( 'NONE',  #123041 ) ;
#109649 = CARTESIAN_POINT ( 'NONE',  ( -48.48921356237309510, -27.52281430457089328, 5.000000000000000000 ) ) ;
#109650 = CARTESIAN_POINT ( 'NONE',  ( 5.510786437626906675, -27.52281430457051314, 5.000000000000000000 ) ) ;
#109651 = EDGE_CURVE ( 'NONE', #25131, #33645, #106267, .T. ) ;
#109652 = CARTESIAN_POINT ( 'NONE',  ( 5.999999999999958256, -16.60178936734448030, 0.8616154019347637139 ) ) ;
#109653 = CARTESIAN_POINT ( 'NONE',  ( 36.66209685856478018, -5.291415217122919401, 3.054999999999998384 ) ) ;
#109654 = AXIS2_PLACEMENT_3D ( 'NONE', #114070, #14024, #3155 ) ;
#109655 = DIRECTION ( 'NONE',  ( 0.6830127018922180770, -0.6830127018922204085, -0.2588190451025213501 ) ) ;
#109656 = ORIENTED_EDGE ( 'NONE', *, *, #113914, .F. ) ;
#109657 = ORIENTED_EDGE ( 'NONE', *, *, #112766, .T. ) ;
#109658 = DIRECTION ( 'NONE',  ( -0.7071067811865487940, 0.7071067811865463515, -0.000000000000000000 ) ) ;
#109659 = STYLED_ITEM ( 'NONE', ( #27598 ), #87420 ) ;
#109660 = ORIENTED_EDGE ( 'NONE', *, *, #34511, .T. ) ;
#109661 = ORIENTED_EDGE ( 'NONE', *, *, #96015, .T. ) ;
#109662 = ADVANCED_FACE ( 'NONE', ( #6941 ), #82422, .F. ) ;
#109663 = CARTESIAN_POINT ( 'NONE',  ( -23.99999999999982236, -9.412538124160663600, 4.000000000000000000 ) ) ;
#109664 = LINE ( 'NONE', #98771, #27706 ) ;
#109665 = ORIENTED_EDGE ( 'NONE', *, *, #8540, .F. ) ;
#109667 = VECTOR ( 'NONE', #94217, 1000.000000000000000 ) ;
#109666 = CARTESIAN_POINT ( 'NONE',  ( -31.92499999999997584, -21.76999999999999247, -37.00000000000000000 ) ) ;
#109668 = CARTESIAN_POINT ( 'NONE',  ( -13.64175702458852335, 15.75929247661555799, 19.34181609438702765 ) ) ;
#109669 = CARTESIAN_POINT ( 'NONE',  ( -39.48921356237310221, -27.52281430457082934, 5.000000000000000000 ) ) ;
#109670 = CARTESIAN_POINT ( 'NONE',  ( 34.49999999999975131, -20.94567065516883630, 4.994342998332155226 ) ) ;
#109671 = ORIENTED_EDGE ( 'NONE', *, *, #4152, .T. ) ;
#109672 = ADVANCED_FACE ( 'NONE', ( #4792 ), #40367, .F. ) ;
#109673 = DIRECTION ( 'NONE',  ( 0.6830127018922180770, -0.6830127018922204085, -0.2588190451025213501 ) ) ;
#109674 = FACE_OUTER_BOUND ( 'NONE', #71058, .T. ) ;
#109675 = EDGE_CURVE ( 'NONE', #79378, #110593, #130763, .T. ) ;
#109676 = PLANE ( 'NONE',  #56622 ) ;
#109678 = CARTESIAN_POINT ( 'NONE',  ( 0.2519841907209453002, 4.694990751126481676, -6.337663282209763160 ) ) ;
#109677 = VECTOR ( 'NONE', #123757, 999.9999999999998863 ) ;
#109679 = CARTESIAN_POINT ( 'NONE',  ( 64.53752705046289861, -9.735942053221456900E-16, 7.949999999999998401 ) ) ;
#109680 = DIRECTION ( 'NONE',  ( 0.7071067811865487940, -0.7071067811865463515, 0.000000000000000000 ) ) ;
#109681 = DIRECTION ( 'NONE',  ( 0.000000000000000000, -1.000000000000000000, 0.000000000000000000 ) ) ;
#109682 = AXIS2_PLACEMENT_3D ( 'NONE', #63787, #139212, #39904 ) ;
#109683 = CARTESIAN_POINT ( 'NONE',  ( 54.18336038379622011, -2.130196079827426203, 7.949999999999997513 ) ) ;
#109684 = EDGE_CURVE ( 'NONE', #143089, #121198, #20136, .T. ) ;
#109685 = DIRECTION ( 'NONE',  ( -0.7071067811865487940, 0.7071067811865463515, 0.000000000000000000 ) ) ;
#109686 = AXIS2_PLACEMENT_3D ( 'NONE', #76090, #1350, #54371 ) ;
#109687 = CARTESIAN_POINT ( 'NONE',  ( 21.18398860626899349, 28.73617430169802134, 5.000000000000000000 ) ) ;
#109688 = ORIENTED_EDGE ( 'NONE', *, *, #124422, .F. ) ;
#109689 = VERTEX_POINT ( 'NONE', #48356 ) ;
#109690 = CARTESIAN_POINT ( 'NONE',  ( 44.45833333333332149, 3.974999999999997424, 6.884901960086288852 ) ) ;
#109691 = FACE_OUTER_BOUND ( 'NONE', #8756, .T. ) ;
#109692 = VECTOR ( 'NONE', #4043, 1000.000000000000000 ) ;
#109693 = VERTEX_POINT ( 'NONE', #37500 ) ;
#109694 = CARTESIAN_POINT ( 'NONE',  ( -17.99999999999987210, -11.35517001088073563, -1.126524801160152300 ) ) ;
#109695 =( BOUNDED_CURVE ( )  B_SPLINE_CURVE ( 2, ( #105513, #6177, #128715, #104074, #106216, #71489, #50453, #29391, #5481, #70792, #92495, #93228, #138898 ),
 .UNSPECIFIED., .F., .F. ) 
 B_SPLINE_CURVE_WITH_KNOTS ( ( 3, 2, 2, 2, 2, 2, 3 ),
 ( 0.2833333333333333259, 0.2861111111111110938, 0.2888888888888888618, 0.2916666666666666852, 0.2944444444444444531, 0.2972222222222222210, 0.2999999999999999889 ),
 .UNSPECIFIED. ) 
 CURVE ( )  GEOMETRIC_REPRESENTATION_ITEM ( )  RATIONAL_B_SPLINE_CURVE ( ( 1.000000000000000000, 0.9659258262890683122, 1.000000000000000000, 0.9659258262890683122, 1.000000000000000000, 0.9659258262890683122, 1.000000000000000000, 0.9659258262890683122, 1.000000000000000000, 0.9659258262890683122, 1.000000000000000000, 0.9659258262890683122, 1.000000000000000000 ) ) 
 REPRESENTATION_ITEM ( '' )  );
#109696 = CARTESIAN_POINT ( 'NONE',  ( 0.000000000000000000, 0.000000000000000000, 5.000000000000000000 ) ) ;
#109697 = CARTESIAN_POINT ( 'NONE',  ( 43.89626352523143282, 4.472830434245840259, -4.472830434245839371 ) ) ;
#109698 = ORIENTED_EDGE ( 'NONE', *, *, #96621, .T. ) ;
#109699 = CARTESIAN_POINT ( 'NONE',  ( 6.852250093007166143, -2.500000000000000000, 3.061616997868383634E-16 ) ) ;
#109700 = EDGE_LOOP ( 'NONE', ( #39106, #123428, #98148, #10807 ) ) ;
#109701 = ORIENTED_EDGE ( 'NONE', *, *, #39296, .T. ) ;
#109702 = AXIS2_PLACEMENT_3D ( 'NONE', #77208, #19923, #99620 ) ;
#109703 = LINE ( 'NONE', #132923, #104806 ) ;
#109704 = CARTESIAN_POINT ( 'NONE',  ( 18.38945826904184599, 9.109118024354394549, 4.348864708961791337 ) ) ;
#109705 = DIRECTION ( 'NONE',  ( 0.3543493200069162685, -0.000000000000000000, -0.9351131265310288487 ) ) ;
#109706 = FACE_OUTER_BOUND ( 'NONE', #52089, .T. ) ;
#109707 = ORIENTED_EDGE ( 'NONE', *, *, #133729, .F. ) ;
#109708 = CARTESIAN_POINT ( 'NONE',  ( 51.29974487139158867, -27.71228299555242103, 4.000000000000000000 ) ) ;
#109710 = ORIENTED_EDGE ( 'NONE', *, *, #71330, .T. ) ;
#109709 = DIRECTION ( 'NONE',  ( 0.000000000000000000, -1.000000000000000000, 0.000000000000000000 ) ) ;
#109711 = CARTESIAN_POINT ( 'NONE',  ( 81.08376352523144703, -6.110000000000001208, -3.741295971395164515E-16 ) ) ;
#109712 = PLANE ( 'NONE',  #108710 ) ;
#109713 = DIRECTION ( 'NONE',  ( 0.6830127018922180770, -0.6830127018922204085, -0.2588190451025213501 ) ) ;
#109714 = DIRECTION ( 'NONE',  ( -0.7071067811865487940, 0.7071067811865463515, -0.000000000000000000 ) ) ;
#109715 = CARTESIAN_POINT ( 'NONE',  ( -11.28242261357426379, -21.73023691814493930, 5.000000000000000888 ) ) ;
#109716 = CARTESIAN_POINT ( 'NONE',  ( 34.92499999999998295, 19.70193056682078137, 4.500000000000000888 ) ) ;
#109717 = ORIENTED_EDGE ( 'NONE', *, *, #116696, .T. ) ;
#109718 = CIRCLE ( 'NONE', #121303, 2.500000000000000444 ) ;
#109719 = LINE ( 'NONE', #132214, #110137 ) ;
#109720 = CARTESIAN_POINT ( 'NONE',  ( 66.55793019189812298, 6.110000000000000320, -1.637169565754156064 ) ) ;
#109721 = CARTESIAN_POINT ( 'NONE',  ( 17.70025512860841488, -27.71228299555193786, 4.000000000000000000 ) ) ;
#109722 = CARTESIAN_POINT ( 'NONE',  ( 39.18398860626899705, 28.73617430169814568, 5.000000000000000000 ) ) ;
#109723 = PRESENTATION_STYLE_ASSIGNMENT (( #140909 ) ) ;
#109724 = VERTEX_POINT ( 'NONE', #125930 ) ;
#109725 = ORIENTED_EDGE ( 'NONE', *, *, #140510, .T. ) ;
#109726 = DIRECTION ( 'NONE',  ( 0.6830127018922181881, 0.6830127018922202975, -0.2588190451025214056 ) ) ;
#109727 = CARTESIAN_POINT ( 'NONE',  ( -31.92499999999997584, -7.730000000000015525, 3.180000000000000160 ) ) ;
#109728 = ORIENTED_EDGE ( 'NONE', *, *, #96784, .F. ) ;
#109729 = VECTOR ( 'NONE', #2758, 1000.000000000000000 ) ;
#109730 = ORIENTED_EDGE ( 'NONE', *, *, #103956, .T. ) ;
#109731 = CARTESIAN_POINT ( 'NONE',  ( -27.47512612785028807, 14.25929247661557042, 9.797011795316574734 ) ) ;
#109732 = ORIENTED_EDGE ( 'NONE', *, *, #6308, .F. ) ;
#109733 = CARTESIAN_POINT ( 'NONE',  ( 0.7307956238753654521, -0.3999999999999997446, -2.467792535850613866 ) ) ;
#109734 = FACE_OUTER_BOUND ( 'NONE', #44054, .T. ) ;
#109735 = CARTESIAN_POINT ( 'NONE',  ( 13.49999999999990408, -10.04351517176476882, -1.623559851933791931 ) ) ;
#109736 = ADVANCED_FACE ( 'NONE', ( #26604 ), #70847, .F. ) ;
#109737 = FACE_BOUND ( 'NONE', #7543, .T. ) ;
#109738 = DIRECTION ( 'NONE',  ( -0.6830127018922180770, -0.6830127018922204085, -0.2588190451025213501 ) ) ;
#109739 = CARTESIAN_POINT ( 'NONE',  ( 41.49586038379622721, -3.974999999999998312, -6.884901960086286188 ) ) ;
#109740 = EDGE_CURVE ( 'NONE', #13955, #4377, #100255, .T. ) ;
#109741 = PLANE ( 'NONE',  #15553 ) ;
#109743 = ORIENTED_EDGE ( 'NONE', *, *, #9311, .T. ) ;
#109742 = FACE_OUTER_BOUND ( 'NONE', #42179, .T. ) ;
#109744 = VECTOR ( 'NONE', #29340, 1000.000000000000227 ) ;
#109745 = PLANE ( 'NONE',  #92602 ) ;
#109746 = EDGE_LOOP ( 'NONE', ( #109017, #114721, #29532, #21962, #55794, #32139 ) ) ;
#109747 = VECTOR ( 'NONE', #22268, 1000.000000000000000 ) ;
#109748 = ORIENTED_EDGE ( 'NONE', *, *, #78055, .F. ) ;
#109749 = CARTESIAN_POINT ( 'NONE',  ( 85.66209685856478018, -5.291415217122919401, 3.054999999999997939 ) ) ;
#109750 = ORIENTED_EDGE ( 'NONE', *, *, #66270, .T. ) ;
#109751 = CARTESIAN_POINT ( 'NONE',  ( 20.99999999999985434, 15.45873954670187089, -0.03131636524298948149 ) ) ;
#109752 = EDGE_CURVE ( 'NONE', #23963, #42862, #62233, .T. ) ;
#109753 = DIRECTION ( 'NONE',  ( 0.7071067811865487940, 0.7071067811865463515, 0.000000000000000000 ) ) ;
#109754 = ORIENTED_EDGE ( 'NONE', *, *, #93745, .F. ) ;
#109755 = PLANE ( 'NONE',  #127817 ) ;
#109756 = EDGE_CURVE ( 'NONE', #48818, #38475, #56793, .T. ) ;
#109757 = CARTESIAN_POINT ( 'NONE',  ( 21.15612307739225884, -22.22499999999999432, 4.000000000000000000 ) ) ;
#109758 = LINE ( 'NONE', #69681, #9003 ) ;
#109759 = LINE ( 'NONE', #140949, #38556 ) ;
#109760 = VECTOR ( 'NONE', #34058, 1000.000000000000000 ) ;
#109761 = CARTESIAN_POINT ( 'NONE',  ( -60.18398860626900415, 28.73617430169829490, 5.000000000000000000 ) ) ;
#109762 = DIRECTION ( 'NONE',  ( -0.3543493200069162685, -0.000000000000000000, -0.9351131265310288487 ) ) ;
#109763 = FACE_OUTER_BOUND ( 'NONE', #94212, .T. ) ;
#109764 = DIRECTION ( 'NONE',  ( 0.7071067811865487940, -0.7071067811865463515, 0.000000000000000000 ) ) ;
#109765 = EDGE_LOOP ( 'NONE', ( #116734, #46355, #120674, #71159 ) ) ;
#109766 = EDGE_CURVE ( 'NONE', #6851, #23129, #90069, .T. ) ;
#109767 = FACE_OUTER_BOUND ( 'NONE', #121842, .T. ) ;
#109768 = ORIENTED_EDGE ( 'NONE', *, *, #113374, .F. ) ;
#109769 = CARTESIAN_POINT ( 'NONE',  ( 123.1625270504628986, 7.949999999999998401, 1.460391307983218338E-15 ) ) ;
#109770 = SURFACE_SIDE_STYLE ('',( #78581 ) ) ;
#109771 = AXIS2_PLACEMENT_3D ( 'NONE', #79921, #13867, #21913 ) ;
#109772 = ORIENTED_EDGE ( 'NONE', *, *, #48164, .F. ) ;
#109773 = ORIENTED_EDGE ( 'NONE', *, *, #44593, .T. ) ;
#109774 = VECTOR ( 'NONE', #133523, 999.9999999999998863 ) ;
#109775 = CARTESIAN_POINT ( 'NONE',  ( 33.83376352523143282, 6.110000000000001208, 1.122388791418549305E-15 ) ) ;
#109776 = ORIENTED_EDGE ( 'NONE', *, *, #67832, .F. ) ;
#109777 = LINE ( 'NONE', #96720, #101426 ) ;
#109778 = MECHANICAL_DESIGN_GEOMETRIC_PRESENTATION_REPRESENTATION (  '', ( #135371 ), #139921 ) ;
#109779 = CARTESIAN_POINT ( 'NONE',  ( -27.48921356237309155, -27.52281430457074762, 5.000000000000000000 ) ) ;
#109780 = CIRCLE ( 'NONE', #58940, 1.499999999999999556 ) ;
#109781 = CARTESIAN_POINT ( 'NONE',  ( 26.00413961620377279, -3.047499999999994547, 5.278424836066145431 ) ) ;
#109782 = CARTESIAN_POINT ( 'NONE',  ( 2.139883101372844543, 13.64905519538773859, -24.44323996371117147 ) ) ;
#109783 = ORIENTED_EDGE ( 'NONE', *, *, #137302, .T. ) ;
#109784 = CARTESIAN_POINT ( 'NONE',  ( 15.98840764549667703, -2.500000000000000888, 0.000000000000000000 ) ) ;
#109785 = EDGE_CURVE ( 'NONE', #73824, #80946, #111849, .T. ) ;
#109786 = ORIENTED_EDGE ( 'NONE', *, *, #47240, .T. ) ;
#109787 = CARTESIAN_POINT ( 'NONE',  ( 36.29974487139159578, -27.71228299555231445, 4.000000000000000000 ) ) ;
#109788 = DIRECTION ( 'NONE',  ( 0.000000000000000000, -1.000000000000000000, 0.000000000000000000 ) ) ;
#109790 = EDGE_LOOP ( 'NONE', ( #80570, #100454, #19148, #89736 ) ) ;
#109789 = DIRECTION ( 'NONE',  ( 1.000000000000000000, 0.000000000000000000, 0.000000000000000000 ) ) ;
#109791 = ORIENTED_EDGE ( 'NONE', *, *, #136069, .F. ) ;
#109792 = DIRECTION ( 'NONE',  ( 0.6830127018922180770, -0.6830127018922204085, -0.2588190451025213501 ) ) ;
#109793 = CARTESIAN_POINT ( 'NONE',  ( 26.99999999999981526, 4.384688058510593400, -7.090945410444622787 ) ) ;
#109794 = EDGE_CURVE ( 'NONE', #96695, #83079, #15439, .T. ) ;
#109795 = EDGE_CURVE ( 'NONE', #126646, #64188, #98114, .T. ) ;
#109796 = LINE ( 'NONE', #86640, #88787 ) ;
#109797 = ORIENTED_EDGE ( 'NONE', *, *, #24362, .T. ) ;
#109798 = DIRECTION ( 'NONE',  ( 0.7071067811865486830, -0.7071067811865464625, -0.000000000000000000 ) ) ;
#109799 = EDGE_LOOP ( 'NONE', ( #68565, #24938, #139458, #37385 ) ) ;
#109800 = EDGE_LOOP ( 'NONE', ( #121315, #9328, #116235, #138966, #84176 ) ) ;
#109801 = DIRECTION ( 'NONE',  ( -1.000000000000000000, -1.224606353822377258E-16, -0.000000000000000000 ) ) ;
#109802 = CARTESIAN_POINT ( 'NONE',  ( 34.22674160717812697, -11.24070752338416490, 18.24660765846990529 ) ) ;
#109803 = VECTOR ( 'NONE', #100725, 999.9999999999998863 ) ;
#109804 = PLANE ( 'NONE',  #55462 ) ;
#109805 = ADVANCED_FACE ( 'NONE', ( #89373 ), #142343, .F. ) ;
#109806 = SPHERICAL_SURFACE ( 'NONE', #97875, 3.000000000000000000 ) ;
#109807 = DIRECTION ( 'NONE',  ( 0.7071067811865487940, 0.7071067811865463515, 0.000000000000000000 ) ) ;
#109808 = CARTESIAN_POINT ( 'NONE',  ( -10.49999999999992006, -1.912538124160735542, 4.000000000000000000 ) ) ;
#109809 = EDGE_CURVE ( 'NONE', #79885, #102792, #89589, .T. ) ;
#109810 = DIRECTION ( 'NONE',  ( -0.7071067811865486830, -0.7071067811865464625, -0.000000000000000000 ) ) ;
#109811 = ORIENTED_EDGE ( 'NONE', *, *, #30382, .T. ) ;
#109812 = ADVANCED_FACE ( 'NONE', ( #23387 ), #65518, .F. ) ;
#109813 = CARTESIAN_POINT ( 'NONE',  ( 96.76669371712955581, -7.949999999999998401, 2.130196079827423983 ) ) ;
#109814 = ORIENTED_EDGE ( 'NONE', *, *, #36611, .T. ) ;
#109815 = CARTESIAN_POINT ( 'NONE',  ( -27.48921356237309155, -27.52281430457074762, 5.000000000000000000 ) ) ;
#109816 = CARTESIAN_POINT ( 'NONE',  ( -25.39999999999996305, 3.061616997868383141E-16, -2.500000000000000000 ) ) ;
#109817 = CARTESIAN_POINT ( 'NONE',  ( 34.92499999999998295, 16.70193056682081334, 4.500000000000000888 ) ) ;
#109818 = EDGE_LOOP ( 'NONE', ( #141440, #73627, #17382, #75378 ) ) ;
#109819 = CARTESIAN_POINT ( 'NONE',  ( 7.499999999999954703, -8.947814304570741228, 5.000000000000000000 ) ) ;
#109820 = CARTESIAN_POINT ( 'NONE',  ( 54.48921356237310221, -27.52281430457093236, 5.000000000000000000 ) ) ;
#109821 = ADVANCED_FACE ( 'NONE', ( #121279 ), #77795, .F. ) ;
#109822 = DIRECTION ( 'NONE',  ( -1.000000000000000000, -1.224606353822377258E-16, -0.000000000000000000 ) ) ;
#109823 = ORIENTED_EDGE ( 'NONE', *, *, #59351, .F. ) ;
#109824 = EDGE_LOOP ( 'NONE', ( #30077, #3578, #71453, #16281 ) ) ;
#109825 = PLANE ( 'NONE',  #2448 ) ;
#109826 = CARTESIAN_POINT ( 'NONE',  ( 39.48921356237310221, -27.52281430457082934, 5.000000000000000000 ) ) ;
#109827 = LINE ( 'NONE', #45325, #5214 ) ;
#109828 = EDGE_CURVE ( 'NONE', #122500, #77801, #100952, .T. ) ;
#109829 = DIRECTION ( 'NONE',  ( 0.6830127018922181881, 0.6830127018922202975, -0.2588190451025214056 ) ) ;
#109830 = CARTESIAN_POINT ( 'NONE',  ( 63.34959685856478018, 6.109999999999997655, 1.637169565754163836 ) ) ;
#109831 = VECTOR ( 'NONE', #62887, 1000.000000000000114 ) ;
#109832 = DIRECTION ( 'NONE',  ( 0.7071067811865487940, 0.7071067811865463515, -0.000000000000000000 ) ) ;
#109833 = CARTESIAN_POINT ( 'NONE',  ( -19.49999999999986500, 18.05218569542898521, 5.000000000000000000 ) ) ;
#109834 = CARTESIAN_POINT ( 'NONE',  ( 83.54166666666667140, -3.975000000000002753, 6.884901960086286188 ) ) ;
#109835 = ORIENTED_EDGE ( 'NONE', *, *, #64823, .T. ) ;
#109836 = CARTESIAN_POINT ( 'NONE',  ( 153.6500000000000057, 0.000000000000000000, 0.000000000000000000 ) ) ;
#109837 = ORIENTED_EDGE ( 'NONE', *, *, #59328, .T. ) ;
#109838 = FACE_OUTER_BOUND ( 'NONE', #121429, .T. ) ;
#109839 = LINE ( 'NONE', #41016, #17472 ) ;
#109840 = DIRECTION ( 'NONE',  ( 1.000000000000000000, 0.000000000000000000, 0.000000000000000000 ) ) ;
#109841 = LINE ( 'NONE', #110529, #95140 ) ;
#109842 = DIRECTION ( 'NONE',  ( -0.7071067811865487940, -0.7071067811865463515, -0.000000000000000000 ) ) ;
#109843 = CARTESIAN_POINT ( 'NONE',  ( -31.49999999999978684, 11.52377502935400955, -1.522421517564011006 ) ) ;
#109844 = CARTESIAN_POINT ( 'NONE',  ( 69.48921356237309510, -27.52281430457103895, 5.000000000000000000 ) ) ;
#109845 = VERTEX_POINT ( 'NONE', #21963 ) ;
#109846 = EDGE_LOOP ( 'NONE', ( #133336, #84620, #22510, #50472 ) ) ;
#109847 = CARTESIAN_POINT ( 'NONE',  ( -57.18398860626899705, 28.73617430169827358, 5.000000000000000000 ) ) ;
#109848 = PLANE ( 'NONE',  #18986 ) ;
#109849 = UNCERTAINTY_MEASURE_WITH_UNIT (LENGTH_MEASURE( 1.000000000000000082E-05 ), #121620, 'distance_accuracy_value', 'NONE');
#109850 = VECTOR ( 'NONE', #14004, 1000.000000000000000 ) ;
#109851 = CARTESIAN_POINT ( 'NONE',  ( 56.90810577924028024, -46.18886352141520035, 34.92499999999998295 ) ) ;
#109853 = ADVANCED_FACE ( 'NONE', ( #98803 ), #66209, .F. ) ;
#109852 = DIRECTION ( 'NONE',  ( -0.7071067811865486830, -0.7071067811865464625, 0.000000000000000000 ) ) ;
#109854 = CARTESIAN_POINT ( 'NONE',  ( 83.20419371712955581, -6.884901960086285300, -3.975000000000000089 ) ) ;
#109856 = EDGE_CURVE ( 'NONE', #74581, #23590, #87941, .T. ) ;
#109855 = CARTESIAN_POINT ( 'NONE',  ( -31.49999999999977973, 10.94296225409023826, -9.576120664313327424 ) ) ;
#109857 = AXIS2_PLACEMENT_3D ( 'NONE', #4242, #93470, #137705 ) ;
#109858 = ORIENTED_EDGE ( 'NONE', *, *, #38594, .T. ) ;
#109859 = CARTESIAN_POINT ( 'NONE',  ( 84.27083333333332860, -7.949999999999999289, -2.130196079827426203 ) ) ;
#109860 = DIRECTION ( 'NONE',  ( 1.734723475976806848E-16, -1.000000000000000000, 0.000000000000000000 ) ) ;
#109861 = AXIS2_PLACEMENT_3D ( 'NONE', #23555, #11212, #88111 ) ;
#109862 = CARTESIAN_POINT ( 'NONE',  ( -25.80981832425536027, -18.74070752338408852, 7.910009926591568430 ) ) ;
#109863 = DIRECTION ( 'NONE',  ( 0.7071067811865487940, 0.7071067811865463515, 0.000000000000000000 ) ) ;
#109864 = ORIENTED_EDGE ( 'NONE', *, *, #116490, .T. ) ;
#109865 = EDGE_CURVE ( 'NONE', #128485, #60505, #92940, .T. ) ;
#109866 = FACE_OUTER_BOUND ( 'NONE', #57539, .T. ) ;
#109867 = VERTEX_POINT ( 'NONE', #135058 ) ;
#109868 = CONICAL_SURFACE ( 'NONE', #12679, 2.055000000000001048, 0.9599310885968758145 ) ;
#109869 = VECTOR ( 'NONE', #35760, 1000.000000000000000 ) ;
#109870 = CARTESIAN_POINT ( 'NONE',  ( 77.43793019189810423, -6.110000000000001208, 1.637169565754158951 ) ) ;
#109871 = LINE ( 'NONE', #43207, #73209 ) ;
#109872 = ORIENTED_EDGE ( 'NONE', *, *, #108774, .F. ) ;
#109873 = DIRECTION ( 'NONE',  ( 0.7071067811865487940, -0.7071067811865463515, 0.000000000000000000 ) ) ;
#109874 = FACE_OUTER_BOUND ( 'NONE', #122613, .T. ) ;
#109875 = LINE ( 'NONE', #118604, #34965 ) ;
#109876 = DIRECTION ( 'NONE',  ( -0.000000000000000000, 0.3543493200069153248, 0.9351131265310292928 ) ) ;
#109877 = CARTESIAN_POINT ( 'NONE',  ( 15.05159235450332034, -3.851859888774471706E-31, 2.500000000000001332 ) ) ;
#109879 = ORIENTED_EDGE ( 'NONE', *, *, #39331, .F. ) ;
#109878 = DIRECTION ( 'NONE',  ( 1.000000000000000000, 0.000000000000000000, 0.000000000000000000 ) ) ;
#109880 = PLANE ( 'NONE',  #60025 ) ;
#109881 = LINE ( 'NONE', #124326, #52235 ) ;
#109882 = FACE_OUTER_BOUND ( 'NONE', #101910, .T. ) ;
#109883 =( BOUNDED_CURVE ( )  B_SPLINE_CURVE ( 3, ( #1748, #113396, #14080, #2476 ),
 .UNSPECIFIED., .F., .F. ) 
 B_SPLINE_CURVE_WITH_KNOTS ( ( 4, 4 ),
 ( 5.005968288816728062, 5.074607125596347856 ),
 .UNSPECIFIED. ) 
 CURVE ( )  GEOMETRIC_REPRESENTATION_ITEM ( )  RATIONAL_B_SPLINE_CURVE ( ( 1.000000000000000000, 0.9996074310407763175, 0.9996074310407763175, 1.000000000000000000 ) ) 
 REPRESENTATION_ITEM ( '' )  );
#109884 = DIRECTION ( 'NONE',  ( -1.000000000000000000, 0.000000000000000000, 0.000000000000000000 ) ) ;
#109885 = VECTOR ( 'NONE', #42445, 1000.000000000000000 ) ;
#109886 = ORIENTED_EDGE ( 'NONE', *, *, #14812, .T. ) ;
#109887 = ORIENTED_EDGE ( 'NONE', *, *, #89796, .F. ) ;
#109888 = CARTESIAN_POINT ( 'NONE',  ( 63.14626352523143282, -4.472830434245840259, 4.472830434245839371 ) ) ;
#109889 = VECTOR ( 'NONE', #46305, 999.9999999999998863 ) ;
#109890 = VECTOR ( 'NONE', #4184, 1000.000000000000000 ) ;
#109891 = ORIENTED_EDGE ( 'NONE', *, *, #129751, .F. ) ;
#109892 = PRESENTATION_LAYER_ASSIGNMENT (  '', '', ( #28868 ) ) ;
#109893 = CARTESIAN_POINT ( 'NONE',  ( -34.92500000000001137, -22.22500000000000142, 4.000000000000000000 ) ) ;
#109894 = DIRECTION ( 'NONE',  ( -0.000000000000000000, -0.3543493200069152693, 0.9351131265310292928 ) ) ;
#109895 = EDGE_CURVE ( 'NONE', #26574, #141092, #92208, .T. ) ;
#109896 = DIRECTION ( 'NONE',  ( -0.000000000000000000, 0.000000000000000000, 1.000000000000000000 ) ) ;
#109897 = VERTEX_POINT ( 'NONE', #25531 ) ;
#109898 = ORIENTED_EDGE ( 'NONE', *, *, #56857, .F. ) ;
#109899 = CARTESIAN_POINT ( 'NONE',  ( 0.000000000000000000, 0.000000000000000000, 5.000000000000000000 ) ) ;
#109900 = DIRECTION ( 'NONE',  ( 0.000000000000000000, 0.000000000000000000, 1.000000000000000000 ) ) ;
#109901 = ORIENTED_EDGE ( 'NONE', *, *, #64445, .T. ) ;
#109902 = DIRECTION ( 'NONE',  ( 0.7071067811865486830, -0.7071067811865464625, -0.000000000000000000 ) ) ;
#109903 = DIRECTION ( 'NONE',  ( 0.6830127018922180770, -0.6830127018922204085, -0.2588190451025213501 ) ) ;
#109904 = CARTESIAN_POINT ( 'NONE',  ( -8.010880286539427075, -22.02621442084248216, 4.990779571109221990 ) ) ;
#109905 = EDGE_LOOP ( 'NONE', ( #14207, #6874, #31506, #92288 ) ) ;
#109906 = EDGE_CURVE ( 'NONE', #129514, #49064, #3748, .T. ) ;
#109907 = EDGE_CURVE ( 'NONE', #49712, #97236, #57486, .T. ) ;
#109908 = FACE_BOUND ( 'NONE', #83879, .T. ) ;
#109909 = FACE_OUTER_BOUND ( 'NONE', #7476, .T. ) ;
#109910 = FACE_OUTER_BOUND ( 'NONE', #39373, .T. ) ;
#109911 = LINE ( 'NONE', #22868, #69109 ) ;
#109912 =( NAMED_UNIT ( * ) SI_UNIT ( $, .STERADIAN. ) SOLID_ANGLE_UNIT ( ) );
#109913 = ADVANCED_FACE ( 'NONE', ( #112553 ), #113981, .F. ) ;
#109914 = EDGE_CURVE ( 'NONE', #112461, #128588, #68723, .T. ) ;
#109915 = FACE_OUTER_BOUND ( 'NONE', #132409, .T. ) ;
#109916 = VERTEX_POINT ( 'NONE', #35752 ) ;
#109917 = ORIENTED_EDGE ( 'NONE', *, *, #4857, .T. ) ;
#109918 = CARTESIAN_POINT ( 'NONE',  ( 116.2870968585647802, 3.054999999999997495, 5.291415217122919401 ) ) ;
#109919 = ORIENTED_EDGE ( 'NONE', *, *, #34944, .F. ) ;
#109920 = EDGE_CURVE ( 'NONE', #75431, #131861, #48036, .T. ) ;
#109921 = ORIENTED_EDGE ( 'NONE', *, *, #105147, .F. ) ;
#109922 = CARTESIAN_POINT ( 'NONE',  ( 183.5369301914312530, -49.19053253528764458, 40.77637019028212251 ) ) ;
#109923 = VECTOR ( 'NONE', #116722, 999.9999999999998863 ) ;
#109924 = ADVANCED_FACE ( 'NONE', ( #59633 ), #136434, .F. ) ;
#109925 = FACE_OUTER_BOUND ( 'NONE', #39408, .T. ) ;
#109926 = EDGE_LOOP ( 'NONE', ( #11837, #57804, #19334, #56084, #85995 ) ) ;
#109927 = DIRECTION ( 'NONE',  ( 0.3543493200069162685, -0.000000000000000000, -0.9351131265310288487 ) ) ;
#109928 = DIRECTION ( 'NONE',  ( 0.6830127018922181881, 0.6830127018922202975, -0.2588190451025214056 ) ) ;
#109930 = CARTESIAN_POINT ( 'NONE',  ( 57.53752705046289151, -9.735942053221456900E-16, 7.949999999999998401 ) ) ;
#109929 = DIRECTION ( 'NONE',  ( -0.6830127018922181881, 0.6830127018922202975, -0.2588190451025214056 ) ) ;
#109931 = ADVANCED_FACE ( 'NONE', ( #124854 ), #126287, .F. ) ;
#109932 = CARTESIAN_POINT ( 'NONE',  ( -8.994519915287490619, 28.92564299267944250, 4.000000000000000000 ) ) ;
#109933 = ADVANCED_FACE ( 'NONE', ( #103109 ), #114677, .T. ) ;
#109934 = LINE ( 'NONE', #20052, #60665 ) ;
#109935 = ORIENTED_EDGE ( 'NONE', *, *, #12077, .T. ) ;
#109936 = DIRECTION ( 'NONE',  ( -0.3543493200069162685, -0.000000000000000000, -0.9351131265310288487 ) ) ;
#109937 = DIRECTION ( 'NONE',  ( -0.7071067811865486830, -0.7071067811865464625, 0.000000000000000000 ) ) ;
#109938 = EDGE_LOOP ( 'NONE', ( #9690, #11547, #140621 ) ) ;
#109939 = EDGE_LOOP ( 'NONE', ( #89227, #71260, #128604, #93910 ) ) ;
#109940 = VERTEX_POINT ( 'NONE', #103788 ) ;
#109941 = CARTESIAN_POINT ( 'NONE',  ( 63.87543019189810423, -5.291415217122920289, -3.055000000000001492 ) ) ;
#109942 = EDGE_CURVE ( 'NONE', #8318, #141462, #90826, .T. ) ;
#109943 = ORIENTED_EDGE ( 'NONE', *, *, #105935, .F. ) ;
#109944 = DIRECTION ( 'NONE',  ( 0.7071067811865487940, 0.7071067811865463515, 0.000000000000000000 ) ) ;
#109945 = AXIS2_PLACEMENT_3D ( 'NONE', #93296, #27305, #47000 ) ;
#109946 = CARTESIAN_POINT ( 'NONE',  ( 1.066639616203771901, 1.633150327867695095, 6.094999999999988205 ) ) ;
#109947 = CARTESIAN_POINT ( 'NONE',  ( 100.3337635252314328, 6.110000000000001208, 1.122388791418549305E-15 ) ) ;
#109948 = DIRECTION ( 'NONE',  ( 0.7071067811865486830, -0.7071067811865464625, -0.000000000000000000 ) ) ;
#109949 = VECTOR ( 'NONE', #88310, 999.9999999999998863 ) ;
#109950 = EDGE_CURVE ( 'NONE', #16237, #39945, #38791, .T. ) ;
#109951 = EDGE_LOOP ( 'NONE', ( #118762, #129934, #84855, #120232 ) ) ;
#109952 = CARTESIAN_POINT ( 'NONE',  ( -2.816011393730999401, 28.73617430169785436, 5.000000000000000000 ) ) ;
#109953 = CARTESIAN_POINT ( 'NONE',  ( 33.18398860626899705, 28.73617430169810305, 5.000000000000000000 ) ) ;
#109954 = CARTESIAN_POINT ( 'NONE',  ( 19.49999999999986855, 21.43112307739196609, 4.000000000000000000 ) ) ;
#109956 = EDGE_CURVE ( 'NONE', #133790, #79052, #69069, .T. ) ;
#109955 = CARTESIAN_POINT ( 'NONE',  ( -11.51078643762690490, -27.52281430457047406, 5.000000000000000000 ) ) ;
#109957 = ORIENTED_EDGE ( 'NONE', *, *, #69236, .F. ) ;
#109958 =( NAMED_UNIT ( * ) SI_UNIT ( $, .STERADIAN. ) SOLID_ANGLE_UNIT ( ) );
#109959 = AXIS2_PLACEMENT_3D ( 'NONE', #114625, #59577, #8679 ) ;
#109960 = ORIENTED_EDGE ( 'NONE', *, *, #130779, .F. ) ;
#109961 = ADVANCED_FACE ( 'NONE', ( #125594 ), #70532, .T. ) ;
#109962 = VERTEX_POINT ( 'NONE', #48737 ) ;
#109963 = ORIENTED_EDGE ( 'NONE', *, *, #26078, .T. ) ;
#109964 = CARTESIAN_POINT ( 'NONE',  ( 123.1412635252314374, 4.472830434245835818, 4.472830434245840259 ) ) ;
#109965 = ORIENTED_EDGE ( 'NONE', *, *, #140217, .F. ) ;
#109966 = ADVANCED_FACE ( 'NONE', ( #60341 ), #104525, .T. ) ;
#109967 = DIRECTION ( 'NONE',  ( 0.6830127018922181881, 0.6830127018922202975, -0.2588190451025214056 ) ) ;
#109968 = DIRECTION ( 'NONE',  ( -0.7071067811865486830, -0.7071067811865464625, 0.000000000000000000 ) ) ;
#109969 = ORIENTED_EDGE ( 'NONE', *, *, #131364, .T. ) ;
#109970 = CARTESIAN_POINT ( 'NONE',  ( -8.994519915287490619, 28.92564299267944250, 4.000000000000000000 ) ) ;
#109971 = VERTEX_POINT ( 'NONE', #102421 ) ;
#109972 = CIRCLE ( 'NONE', #66043, 2.055000000000001048 ) ;
#109973 = CARTESIAN_POINT ( 'NONE',  ( 13.68706980810188334, -2.126176841940956130, 7.934999999999991616 ) ) ;
#109974 = CARTESIAN_POINT ( 'NONE',  ( 14.99999999999989164, -11.35517001088070721, -1.126524801160074363 ) ) ;
#109975 = CIRCLE ( 'NONE', #107601, 2.500000000000000888 ) ;
#109976 = FACE_OUTER_BOUND ( 'NONE', #86781, .T. ) ;
#109977 = AXIS2_PLACEMENT_3D ( 'NONE', #117947, #128856, #16511 ) ;
#109978 = ADVANCED_FACE ( 'NONE', ( #80659 ), #61766, .F. ) ;
#109979 = CARTESIAN_POINT ( 'NONE',  ( 24.41159235450331977, 2.500000000000001776, 0.000000000000000000 ) ) ;
#109980 = VERTEX_POINT ( 'NONE', #16809 ) ;
#109981 = ORIENTED_EDGE ( 'NONE', *, *, #124157, .T. ) ;
#109982 = ORIENTED_EDGE ( 'NONE', *, *, #61555, .T. ) ;
#109983 = SURFACE_STYLE_USAGE ( .BOTH. , #33875 ) ;
#109984 = DIRECTION ( 'NONE',  ( -0.000000000000000000, 0.000000000000000000, 1.000000000000000000 ) ) ;
#109985 = UNCERTAINTY_MEASURE_WITH_UNIT (LENGTH_MEASURE( 1.000000000000000082E-05 ), #65078, 'distance_accuracy_value', 'NONE');
#109986 = FACE_OUTER_BOUND ( 'NONE', #108056, .T. ) ;
#109987 = ADVANCED_FACE ( 'NONE', ( #74048 ), #96470, .T. ) ;
#109988 = DIRECTION ( 'NONE',  ( 0.7071067811865486830, -0.7071067811865464625, -0.000000000000000000 ) ) ;
#109989 = DIRECTION ( 'NONE',  ( -0.000000000000000000, -0.000000000000000000, 1.000000000000000000 ) ) ;
#109990 = CARTESIAN_POINT ( 'NONE',  ( 31.06293019189809712, 1.637169565754157174, 6.110000000000002984 ) ) ;
#109991 = CARTESIAN_POINT ( 'NONE',  ( 51.29974487139158867, -27.71228299555242103, 4.000000000000000000 ) ) ;
#109992 = DIRECTION ( 'NONE',  ( -0.3543493200069162685, -0.000000000000000000, -0.9351131265310288487 ) ) ;
#109993 = ORIENTED_EDGE ( 'NONE', *, *, #110587, .T. ) ;
#109994 = CARTESIAN_POINT ( 'NONE',  ( -42.18398860626899705, 28.73617430169816700, 5.000000000000000000 ) ) ;
#109995 = ORIENTED_EDGE ( 'NONE', *, *, #50229, .T. ) ;
#109996 = CARTESIAN_POINT ( 'NONE',  ( 12.32816939922344268, 20.25929247661551713, 4.000000000000000000 ) ) ;
#109997 = ORIENTED_EDGE ( 'NONE', *, *, #43720, .T. ) ;
#109998 = DIRECTION ( 'NONE',  ( 0.7071067811865486830, -0.7071067811865464625, -0.000000000000000000 ) ) ;
#110000 = ORIENTED_EDGE ( 'NONE', *, *, #8101, .F. ) ;
#109999 = FACE_OUTER_BOUND ( 'NONE', #48016, .T. ) ;
#110001 = CARTESIAN_POINT ( 'NONE',  ( 26.99999999999982236, 14.87792677143811737, -11.06722581663433935 ) ) ;
#110002 = EDGE_CURVE ( 'NONE', #100802, #132053, #118966, .T. ) ;
#110003 = ORIENTED_EDGE ( 'NONE', *, *, #27243, .T. ) ;
#110004 = ORIENTED_EDGE ( 'NONE', *, *, #104091, .T. ) ;
#110005 = CARTESIAN_POINT ( 'NONE',  ( -5.999999999999952927, -19.06887692260761469, 4.000000000000000000 ) ) ;
#110006 = ORIENTED_EDGE ( 'NONE', *, *, #61419, .T. ) ;
#110007 = CARTESIAN_POINT ( 'NONE',  ( -42.48921356237308800, -27.52281430457085065, 5.000000000000000000 ) ) ;
#110008 = EDGE_CURVE ( 'NONE', #142445, #62352, #141446, .T. ) ;
#110009 = CARTESIAN_POINT ( 'NONE',  ( 114.7041937171295558, -6.884901960086285300, -3.975000000000000089 ) ) ;
#110010 = CARTESIAN_POINT ( 'NONE',  ( -5.186508646023577640, -15.74070752338412049, 8.904080028138954717 ) ) ;
#110011 = FACE_OUTER_BOUND ( 'NONE', #57762, .T. ) ;
#110012 = FILL_AREA_STYLE ('',( #79600 ) ) ;
#110013 = FACE_OUTER_BOUND ( 'NONE', #83596, .T. ) ;
#110014 = LINE ( 'NONE', #97719, #52968 ) ;
#110015 = CARTESIAN_POINT ( 'NONE',  ( 17.64583333333333215, -1.633150327867689988, 6.094999999999989981 ) ) ;
#110016 = CARTESIAN_POINT ( 'NONE',  ( 16.02040314143522082, 7.934999999999988951, -2.126176841940961904 ) ) ;
#110017 = DIRECTION ( 'NONE',  ( -0.7071067811865486830, 0.7071067811865464625, 0.000000000000000000 ) ) ;
#110018 = DIRECTION ( 'NONE',  ( -0.7071067811865486830, -0.7071067811865464625, 0.000000000000000000 ) ) ;
#110019 = ORIENTED_EDGE ( 'NONE', *, *, #17458, .T. ) ;
#110020 = ORIENTED_EDGE ( 'NONE', *, *, #115643, .T. ) ;
#110021 = EDGE_CURVE ( 'NONE', #1441, #127035, #27671, .T. ) ;
#110022 = CARTESIAN_POINT ( 'NONE',  ( 1.998069433179001653, -22.22500000000000142, 4.500000000000000888 ) ) ;
#110023 = ORIENTED_EDGE ( 'NONE', *, *, #131079, .T. ) ;
#110024 = CARTESIAN_POINT ( 'NONE',  ( 14.67183060077636902, -6.740707523384207533, 4.000000000000000000 ) ) ;
#110025 = PLANE ( 'NONE',  #132650 ) ;
#110026 = CARTESIAN_POINT ( 'NONE',  ( 78.18398860626899705, 28.73617430169841924, 5.000000000000000000 ) ) ;
#110027 = EDGE_LOOP ( 'NONE', ( #50812, #126634, #59523, #73552 ) ) ;
#110028 = LINE ( 'NONE', #54276, #137813 ) ;
#110029 = CARTESIAN_POINT ( 'NONE',  ( -7.499999999999951150, -20.56887692260760048, 4.000000000000000000 ) ) ;
#110030 = FACE_OUTER_BOUND ( 'NONE', #93734, .T. ) ;
#110031 = ADVANCED_FACE ( 'NONE', ( #29113 ), #142892, .T. ) ;
#110032 = DIRECTION ( 'NONE',  ( 2.781805975412905274E-17, -0.3543493200069152138, 0.9351131265310292928 ) ) ;
#110033 = CARTESIAN_POINT ( 'NONE',  ( 0.000000000000000000, 0.000000000000000000, 5.000000000000000000 ) ) ;
#110035 = ORIENTED_EDGE ( 'NONE', *, *, #128045, .T. ) ;
#110034 = CARTESIAN_POINT ( 'NONE',  ( -12.20000000000000284, -28.33999999999998565, 13.17925390838734323 ) ) ;
#110036 = DIRECTION ( 'NONE',  ( 0.7071067811865486830, -0.7071067811865464625, -0.000000000000000000 ) ) ;
#110037 = FACE_OUTER_BOUND ( 'NONE', #104223, .T. ) ;
#110038 = CARTESIAN_POINT ( 'NONE',  ( -25.39999999999996305, 3.061616997868383141E-16, -2.500000000000000000 ) ) ;
#110039 = DIRECTION ( 'NONE',  ( 0.7071067811865487940, -0.7071067811865463515, 0.000000000000000000 ) ) ;
#110040 = PLANE ( 'NONE',  #114019 ) ;
#110041 = ORIENTED_EDGE ( 'NONE', *, *, #3443, .F. ) ;
#110042 = VECTOR ( 'NONE', #73687, 1000.000000000000000 ) ;
#110043 = EDGE_LOOP ( 'NONE', ( #141960, #2376, #67656, #6205 ) ) ;
#110044 = ORIENTED_EDGE ( 'NONE', *, *, #107788, .F. ) ;
#110045 = CARTESIAN_POINT ( 'NONE',  ( 90.56293019189811844, 1.637169565754157174, 6.110000000000002984 ) ) ;
#110046 = ORIENTED_EDGE ( 'NONE', *, *, #41029, .F. ) ;
#110047 = VECTOR ( 'NONE', #41068, 1000.000000000000000 ) ;
#110048 = CARTESIAN_POINT ( 'NONE',  ( 125.0591050317584632, -46.71325913968133392, 35.40428284070863896 ) ) ;
#110049 = CARTESIAN_POINT ( 'NONE',  ( 84.07919371712955581, 3.975000000000002753, -6.884901960086283523 ) ) ;
#110050 = EDGE_LOOP ( 'NONE', ( #9852, #100167, #106484, #50745 ) ) ;
#110051 = DIRECTION ( 'NONE',  ( -0.000000000000000000, 0.000000000000000000, 1.000000000000000000 ) ) ;
#110052 = CARTESIAN_POINT ( 'NONE',  ( 84.78709685856478018, 3.054999999999997495, 5.291415217122919401 ) ) ;
#110053 =( GEOMETRIC_REPRESENTATION_CONTEXT ( 3 ) GLOBAL_UNCERTAINTY_ASSIGNED_CONTEXT ( ( #69219 ) ) GLOBAL_UNIT_ASSIGNED_CONTEXT ( ( #31054, #20854, #31751 ) ) REPRESENTATION_CONTEXT ( 'NONE', 'WORKASPACE' ) );
#110054 = ORIENTED_EDGE ( 'NONE', *, *, #33932, .T. ) ;
#110055 = LINE ( 'NONE', #132583, #37350 ) ;
#110056 = EDGE_CURVE ( 'NONE', #36671, #94039, #39289, .T. ) ;
#110057 = DIRECTION ( 'NONE',  ( -0.7071067811865487940, 0.7071067811865463515, 0.000000000000000000 ) ) ;
#110058 = ORIENTED_EDGE ( 'NONE', *, *, #135777, .F. ) ;
#110059 = VERTEX_POINT ( 'NONE', #85613 ) ;
#110060 = ORIENTED_EDGE ( 'NONE', *, *, #55104, .F. ) ;
#110061 = CARTESIAN_POINT ( 'NONE',  ( -18.00548008471250583, 28.92564299267925776, 4.000000000000000000 ) ) ;
#110062 = EDGE_CURVE ( 'NONE', #81231, #69434, #136368, .T. ) ;
#110063 = EDGE_CURVE ( 'NONE', #115305, #49295, #61085, .T. ) ;
#110064 = CYLINDRICAL_SURFACE ( 'NONE', #105584, 2.500000000000000000 ) ;
#110065 = CARTESIAN_POINT ( 'NONE',  ( 14.50456980810188767, 6.871911579029510442, -3.967499999999998916 ) ) ;
#110066 = CARTESIAN_POINT ( 'NONE',  ( 0.000000000000000000, 0.000000000000000000, 5.000000000000000000 ) ) ;
#110067 = DIRECTION ( 'NONE',  ( 0.7071067811865487940, -0.7071067811865463515, -0.000000000000000000 ) ) ;
#110068 = AXIS2_PLACEMENT_3D ( 'NONE', #52969, #110908, #113796 ) ;
#110069 = DIRECTION ( 'NONE',  ( -0.6830127018922180770, -0.6830127018922204085, -0.2588190451025213501 ) ) ;
#110070 = ADVANCED_FACE ( 'NONE', ( #40714 ), #127730, .F. ) ;
#110071 = EDGE_CURVE ( 'NONE', #92828, #82762, #73467, .T. ) ;
#110072 = VECTOR ( 'NONE', #139860, 1000.000000000000000 ) ;
#110073 = ADVANCED_FACE ( 'NONE', ( #129852 ), #5894, .F. ) ;
#110074 = ORIENTED_EDGE ( 'NONE', *, *, #52644, .F. ) ;
#110076 = VERTEX_POINT ( 'NONE', #72673 ) ;
#110075 = VECTOR ( 'NONE', #83962, 1000.000000000000000 ) ;
#110078 = EDGE_CURVE ( 'NONE', #41370, #128174, #105930, .T. ) ;
#110077 = CARTESIAN_POINT ( 'NONE',  ( 63.29974487139158867, -27.71228299555250274, 4.000000000000000000 ) ) ;
#110079 = VERTEX_POINT ( 'NONE', #74790 ) ;
#110080 = ORIENTED_EDGE ( 'NONE', *, *, #31495, .T. ) ;
#110082 = EDGE_CURVE ( 'NONE', #61139, #58008, #139338, .T. ) ;
#110081 = VECTOR ( 'NONE', #10661, 1000.000000000000000 ) ;
#110083 = ADVANCED_FACE ( 'NONE', ( #63898 ), #128441, .T. ) ;
#110084 = CARTESIAN_POINT ( 'NONE',  ( 4.171830600776440079, 15.75929247661555976, 4.000000000000000000 ) ) ;
#110085 = EDGE_LOOP ( 'NONE', ( #35594, #49386, #109364 ) ) ;
#110086 = CARTESIAN_POINT ( 'NONE',  ( 56.12499999999999289, -7.950000000000000178, -4.867971026610729436E-16 ) ) ;
#110087 = CARTESIAN_POINT ( 'NONE',  ( 25.39999999999999858, -5.520864266206504263E-14, 0.000000000000000000 ) ) ;
#110088 = CARTESIAN_POINT ( 'NONE',  ( -21.18398860626899349, 28.73617430169802134, 5.000000000000000000 ) ) ;
#110089 = DIRECTION ( 'NONE',  ( 0.7071067811865487940, 0.7071067811865463515, 0.000000000000000000 ) ) ;
#110090 = EDGE_LOOP ( 'NONE', ( #113975, #60414, #100542, #136915, #117681 ) ) ;
#110091 = EDGE_CURVE ( 'NONE', #14957, #58958, #94240, .T. ) ;
#110092 = CARTESIAN_POINT ( 'NONE',  ( 15.48921356237309510, -27.52281430457066236, 5.000000000000000000 ) ) ;
#110093 = ORIENTED_EDGE ( 'NONE', *, *, #78775, .F. ) ;
#110094 = LINE ( 'NONE', #76806, #38786 ) ;
#110095 = ORIENTED_EDGE ( 'NONE', *, *, #133318, .F. ) ;
#110096 = DIRECTION ( 'NONE',  ( -0.7071067811865487940, 0.7071067811865463515, -0.000000000000000000 ) ) ;
#110097 = ORIENTED_EDGE ( 'NONE', *, *, #129731, .T. ) ;
#110098 = LINE ( 'NONE', #9329, #11109 ) ;
#110099 = ORIENTED_EDGE ( 'NONE', *, *, #84415, .T. ) ;
#110100 = ORIENTED_EDGE ( 'NONE', *, *, #7291, .F. ) ;
#110101 = EDGE_CURVE ( 'NONE', #137228, #140889, #96587, .T. ) ;
#110102 = ORIENTED_EDGE ( 'NONE', *, *, #100629, .T. ) ;
#110103 = CARTESIAN_POINT ( 'NONE',  ( 27.48921356237309155, -27.52281430457074762, 5.000000000000000000 ) ) ;
#110104 = CARTESIAN_POINT ( 'NONE',  ( -25.49999999999982236, 22.01701374228153085, 2.453858888625688905 ) ) ;
#110105 = PLANE ( 'NONE',  #135271 ) ;
#110106 = CARTESIAN_POINT ( 'NONE',  ( 124.6879301918981042, 6.110000000000002984, -1.637169565754156730 ) ) ;
#110107 = CARTESIAN_POINT ( 'NONE',  ( 60.48921356237309510, -27.52281430457097500, 5.000000000000000000 ) ) ;
#110108 = DIRECTION ( 'NONE',  ( 0.7071067811865486830, -0.7071067811865464625, -0.000000000000000000 ) ) ;
#110109 = FACE_OUTER_BOUND ( 'NONE', #43498, .T. ) ;
#110110 = DIRECTION ( 'NONE',  ( -0.7071067811865486830, -0.7071067811865464625, 0.000000000000000000 ) ) ;
#110112 = ADVANCED_FACE ( 'NONE', ( #44296 ), #110920, .F. ) ;
#110111 = FACE_OUTER_BOUND ( 'NONE', #115049, .T. ) ;
#110113 = DIRECTION ( 'NONE',  ( 0.6830127018922181881, 0.6830127018922202975, -0.2588190451025214056 ) ) ;
#110114 = PLANE ( 'NONE',  #33301 ) ;
#110115 = ORIENTED_EDGE ( 'NONE', *, *, #57360, .F. ) ;
#110116 = EDGE_CURVE ( 'NONE', #68584, #142173, #88509, .T. ) ;
#110117 = ORIENTED_EDGE ( 'NONE', *, *, #75617, .F. ) ;
#110118 = ORIENTED_EDGE ( 'NONE', *, *, #2202, .T. ) ;
#110119 = CARTESIAN_POINT ( 'NONE',  ( 0.000000000000000000, 60.00000000000000000, 0.000000000000000000 ) ) ;
#110120 = EDGE_LOOP ( 'NONE', ( #118136, #79639, #106189, #98106 ) ) ;
#110122 = EDGE_CURVE ( 'NONE', #115190, #97236, #119654, .T. ) ;
#110121 =( BOUNDED_CURVE ( )  B_SPLINE_CURVE ( 2, ( #69606, #1430, #79790, #57306, #24634, #34821, #34110, #68888, #25343, #23181, #58025, #102225, #79066, #80474, #124667, #131734, #8468, #108498, #120093, #54897, #52719, #99064, #142613, #10633, #77381, #96910, #78077, #141917, #110649, #11329, #143308, #55609, #41869, #54207, #33172, #53446, #121549, #131023, #122252, #109964, #133177, #33861, #22924, #99803, #44012, #88230, #43299, #109253, #98393, #32424, #22224, #20808, #476, #9934, #132485, #87511, #86088, #66486, #9180, #130318, #76659, #120835, #44769, #64332, #88960, #21539, #141156, #97662, #67189, #65064, #65804, #31007, #42607, #75230, #75921, #119392, #20085, #86806, #31701, #65755, #99027, #128298, #9885, #54850, #119344, #64282, #109918, #130984, #17373, #43261, #61630, #120785, #105782, #139185, #83359, #43963, #86760, #39143, #97602, #75879, #72527, #10581, #84099, #138453, #28976, #127571, #16656, #143261, #88183, #6446, #141864, #50727, #120040, #115949, #27522, #71781, #9126, #87470, #109203, #75188, #20039, #50025, #54159, #94214, #60938, #105096, #28266, #39878, #65016, #94916, #131685, #108449, #53398, #5759, #42558, #21497, #98346, #31658, #116688, #20760, #142569, #32372, #76614, #12733, #33124, #57003, #121497, #25037, #67896, #89591, #11286, #133822, #3284, #132435, #23622, #124371, #99752, #69290, #419, #133132, #45415, #113473, #1818, #102634, #111333, #34505, #112773, #14167, #78730, #112079, #58455, #90300, #122204, #2560, #22873, #80180, #67142, #100490, #44721, #47571, #46121, #135277, #134553, #79493, #68586, #1135, #12019, #78028, #56306, #24338, #33809, #122947, #35961, #101899, #55560, #101178, #66437, #77338, #57711, #22175, #35250, #46868, #13432, #123685, #91056, #110606, #88913, #116345, #48967, #25761, #114198, #104005, #38092, #91732, #70034, #81603, #93873, #82309, #137398, #126490, #27907, #26487, #105447, #71426, #135955, #48232, #59840, #138103, #36634, #104752, #127958, #17717, #27183, #125076, #15558, #4665, #106146, #94575, #59157, #83014, #114880, #115581, #17040, #136660, #61309, #70735, #61994, #49696, #72897, #6821, #6108, #93167, #138829, #16282, #38793, #60579, #14883, #50387, #92426, #103306, #5416, #127208, #39524, #3958, #83754, #72175, #80881, #37368, #28646, #117049, #125812, #119190, #106883, #65579, #118477, #75015, #85851, #108281, #131515, #64113, #21321, #76429, #42381, #63435, #29325, #95299, #32199, #19175, #52508, #20584, #120598, #73567, #31487, #51824, #8260, #140250, #109749, #7562, #53976, #8953, #141680, #117736, #51107, #107603, #18420, #96694, #96010, #40246, #87294, #139563, #40936, #19873, #74283, #97424, #84460, #128652, #62701, #30787, #109018, #130823, #140941, #85140, #129350, #75710, #30035, #41632, #130088, #53215, #86594, #119879, #64834, #9709, #98172, #142403, #43088, #238, #43789, #57541, #88738, #24178, #133657, #88002, #44539, #77845, #101007, #132970, #56849, #968, #12568, #79318, #54678, #80025, #33649, #112610, #13268, #1661, #101730, #132251, #56127, #35077, #55390, #23448, #123520, #98858, #32942, #45948, #135114, #24877, #2380, #111907, #90133, #45253, #111151, #100315, #34337, #121332, #11841, #110440, #143095, #46701, #124199, #77162, #122032, #22016, #66265, #68431, #90883, #22702, #99564, #35801, #11114, #78566, #66974, #89424, #134378, #122762, #67718, #69126, #10420, #37188, #70579, #71993, #15396, #38623, #82853, #103155, #3118, #16870, #48080, #127037, #93000, #113304, #69859, #81441, #16110, #13982, #126335, #5948, #39353, #59678, #47409, #83572, #3794, #116176, #61144, #60398, #105293, #91575, #103837, #137945, #14723, #27735, #92262, #127786, #71265, #94411, #28472, #58285, #114031, #125642, #5247, #4488, #114724, #48793, #137227, #50221, #26322, #138660, #37926, #104584, #82157, #135793, #102471, #59000, #36478, #27019, #80717, #115417, #124913, #25583, #49531, #136491, #93716, #19707, #40771, #107433, #140762, #128492, #87118, #140091, #96525, #8096, #129905, #9519, #85670, #42919, #51649, #29862, #53040, #97994, #19002, #53797, #84974, #74105, #42205, #142235, #50933, #97237, #73402, #118296, #18249, #131334, #29163, #75536, #30616, #63948, #8780, #129176, #95844, #141502, #62530, #86421, #72732, #74844, #63266, #130648, #105979, #106695, #52338, #108117, #41455, #119021, #31317, #119706, #20404, #116885, #17557, #7389, #64652, #108833, #61821, #6649, #95123, #117566, #139395, #40082, #84296, #100844, #76249, #10250, #78389, #13099, #46520, #34896, #133487, #67533, #22535, #132799, #121856, #55939, #1498, #123338, #111729, #100142, #43603, #110268, #87825, #134200, #132065, #90703, #76990, #66795, #45784, #32755, #79133, #33482, #32018, #121156, #122581, #55, #110974, #24006, #142921, #68264, #21852, #66097, #88565, #112440, #57369, #101544, #2198, #120410, #23257, #44352, #54511, #21137, #65397, #99384, #77684, #89948, #109574, #98692, #10943, #11655, #55208, #792, #89259, #45086, #34172, #12395, #56679, #13801, #115975, #47927, #102298, #136317, #91412, #124032, #27542, #105123, #124736, #25403, #68960, #35627, #60215, #38451, #69677, #36312, #82674, #79858, #15229, #135625, #58096, #71096, #2945, #24704, #47241, #37006, #58829, #92091, #113130, #113854, #137043, #125462, #115238, #80540, #81257, #14550, #50047, #102991, #137773, #92812, #81987, #15925, #3627, #26145, #70415, #114560, #26844, #59508, #103665, #5781, #4306, #48609, #37750, #126173, #104396, #134938, #5058, #49356, #93541, #126856, #71810, #16678, #60964, #28290, #118851, #51474, #72552, #116716, #106518, #95667, #17394, #52859, #139922, #19539, #63785, #84122, #127600, #141316, #28999, #107942, #73928, #94241, #50751, #62358, #140596, #138479, #107254, #130468, #20233, #8614, #39164, #64478, #128324, #97054, #42030, #41284, #86245, #61651, #40599, #31155, #139209, #75367, #73232, #108653, #52168, #119535, #9334, #83385, #94941, #129721, #18071 ),
 .UNSPECIFIED., .F., .T. ) 
 B_SPLINE_CURVE_WITH_KNOTS ( ( 3, 2, 2, 2, 2, 2, 2, 2, 2, 2, 2, 2, 2, 2, 2, 2, 2, 2, 2, 2, 2, 2, 2, 2, 2, 2, 2, 2, 2, 2, 2, 2, 2, 2, 2, 2, 2, 2, 2, 2, 2, 2, 2, 2, 2, 2, 2, 2, 2, 2, 2, 2, 2, 2, 2, 2, 2, 2, 2, 2, 2, 2, 2, 2, 2, 2, 2, 2, 2, 2, 2, 2, 2, 2, 2, 2, 2, 2, 2, 2, 2, 2, 2, 2, 2, 2, 2, 2, 2, 2, 2, 2, 2, 2, 2, 2, 2, 2, 2, 2, 2, 2, 2, 2, 2, 2, 2, 2, 2, 2, 2, 2, 2, 2, 2, 2, 2, 2, 2, 2, 2, 2, 2, 2, 2, 2, 2, 2, 2, 2, 2, 2, 2, 2, 2, 2, 2, 2, 2, 2, 2, 2, 2, 2, 2, 2, 2, 2, 2, 2, 2, 2, 2, 2, 2, 2, 2, 2, 2, 2, 2, 2, 2, 2, 2, 2, 2, 2, 2, 2, 2, 2, 2, 2, 2, 2, 2, 2, 2, 2, 2, 2, 2, 2, 2, 2, 2, 2, 2, 2, 2, 2, 2, 2, 2, 2, 2, 2, 2, 2, 2, 2, 2, 2, 2, 2, 2, 2, 2, 2, 2, 2, 2, 2, 2, 2, 2, 2, 2, 2, 2, 2, 2, 2, 2, 2, 2, 2, 2, 2, 2, 2, 2, 2, 2, 2, 2, 2, 2, 2, 2, 2, 2, 2, 2, 2, 2, 2, 2, 2, 2, 2, 2, 2, 2, 2, 2, 2, 2, 2, 2, 2, 2, 2, 2, 2, 2, 2, 2, 2, 2, 2, 2, 2, 2, 2, 2, 2, 2, 2, 2, 2, 2, 2, 2, 2, 2, 2, 2, 2, 2, 2, 2, 2, 2, 2, 2, 2, 2, 2, 2, 2, 2, 2, 2, 2, 2, 2, 2, 2, 2, 2, 2, 2, 2, 2, 2, 2, 2, 2, 2, 2, 2, 2, 2, 2, 2, 2, 2, 2, 2, 2, 2, 2, 2, 2, 2, 2, 2, 2, 2, 2, 2, 2, 2, 2, 2, 2, 2, 2, 2, 3 ),
 ( 0.000000000000000000, 0.002777777777777777884, 0.005555555555555555768, 0.008333333333333333218, 0.01111111111111111154, 0.01388888888888888812, 0.01666666666666666644, 0.01944444444444444475, 0.02222222222222222307, 0.02500000000000000139, 0.02777777777777777624, 0.03055555555555555455, 0.03333333333333333287, 0.03611111111111110772, 0.03888888888888888951, 0.04166666666666666435, 0.04444444444444444614, 0.04722222222222222099, 0.05000000000000000278, 0.05277777777777777762, 0.05555555555555555247, 0.05833333333333333426, 0.06111111111111110911, 0.06388888888888888395, 0.06666666666666666574, 0.06944444444444444753, 0.07222222222222221544, 0.07499999999999999722, 0.07777777777777777901, 0.08055555555555556080, 0.08333333333333332871, 0.08611111111111111049, 0.08888888888888889228, 0.09166666666666666019, 0.09444444444444444198, 0.09722222222222222376, 0.1000000000000000056, 0.1027777777777777735, 0.1055555555555555552, 0.1083333333333333370, 0.1111111111111111049, 0.1138888888888888867, 0.1166666666666666685, 0.1194444444444444503, 0.1222222222222222182, 0.1250000000000000000, 0.1277777777777777679, 0.1305555555555555636, 0.1333333333333333315, 0.1361111111111110994, 0.1388888888888888951, 0.1416666666666666630, 0.1444444444444444309, 0.1472222222222222265, 0.1499999999999999944, 0.1527777777777777901, 0.1555555555555555580, 0.1583333333333333259, 0.1611111111111111216, 0.1638888888888888895, 0.1666666666666666574, 0.1694444444444444531, 0.1722222222222222210, 0.1750000000000000167, 0.1777777777777777846, 0.1805555555555555525, 0.1833333333333333204, 0.1861111111111111160, 0.1888888888888888840, 0.1916666666666666796, 0.1944444444444444475, 0.1972222222222222154, 0.2000000000000000111, 0.2027777777777777790, 0.2055555555555555469, 0.2083333333333333426, 0.2111111111111111105, 0.2138888888888888784, 0.2166666666666666741, 0.2194444444444444420, 0.2222222222222222099, 0.2249999999999999778, 0.2277777777777777735, 0.2305555555555555691, 0.2333333333333333370, 0.2361111111111111049, 0.2388888888888889006, 0.2416666666666666685, 0.2444444444444444364, 0.2472222222222222321, 0.2500000000000000000, 0.2527777777777777679, 0.2555555555555555358, 0.2583333333333333592, 0.2611111111111111271, 0.2638888888888888951, 0.2666666666666666630, 0.2694444444444444309, 0.2722222222222221988, 0.2750000000000000222, 0.2777777777777777901, 0.2805555555555555580, 0.2833333333333333259, 0.2861111111111110938, 0.2888888888888888618, 0.2916666666666666852, 0.2944444444444444531, 0.2972222222222222210, 0.2999999999999999889, 0.3027777777777777568, 0.3055555555555555802, 0.3083333333333333481, 0.3111111111111111160, 0.3138888888888888840, 0.3166666666666666519, 0.3194444444444444198, 0.3222222222222222432, 0.3250000000000000111, 0.3277777777777777790, 0.3305555555555555469, 0.3333333333333333148, 0.3361111111111111382, 0.3388888888888889062, 0.3416666666666666741, 0.3444444444444444420, 0.3472222222222222099, 0.3500000000000000333, 0.3527777777777778012, 0.3555555555555555691, 0.3583333333333333370, 0.3611111111111111049, 0.3638888888888888729, 0.3666666666666666408, 0.3694444444444444642, 0.3722222222222222321, 0.3750000000000000000, 0.3777777777777777679, 0.3805555555555555358, 0.3833333333333333592, 0.3861111111111111271, 0.3888888888888888951, 0.3916666666666666630, 0.3944444444444444309, 0.3972222222222221988, 0.4000000000000000222, 0.4027777777777777901, 0.4055555555555555580, 0.4083333333333333259, 0.4111111111111110938, 0.4138888888888888618, 0.4166666666666666852, 0.4194444444444444531, 0.4222222222222222210, 0.4249999999999999889, 0.4277777777777777568, 0.4305555555555555802, 0.4333333333333333481, 0.4361111111111111160, 0.4388888888888888840, 0.4416666666666666519, 0.4444444444444444198, 0.4472222222222222432, 0.4499999999999999556, 0.4527777777777777790, 0.4555555555555555469, 0.4583333333333333148, 0.4611111111111111382, 0.4638888888888889062, 0.4666666666666666741, 0.4694444444444444420, 0.4722222222222222099, 0.4749999999999999778, 0.4777777777777778012, 0.4805555555555555691, 0.4833333333333333370, 0.4861111111111111049, 0.4888888888888888729, 0.4916666666666666408, 0.4944444444444444642, 0.4972222222222222321, 0.5000000000000000000, 0.5027777777777777679, 0.5055555555555555358, 0.5083333333333333037, 0.5111111111111110716, 0.5138888888888888395, 0.5166666666666667185, 0.5194444444444444864, 0.5222222222222222543, 0.5250000000000000222, 0.5277777777777777901, 0.5305555555555555580, 0.5333333333333333259, 0.5361111111111110938, 0.5388888888888888618, 0.5416666666666666297, 0.5444444444444443976, 0.5472222222222222765, 0.5500000000000000444, 0.5527777777777778123, 0.5555555555555555802, 0.5583333333333333481, 0.5611111111111111160, 0.5638888888888888840, 0.5666666666666666519, 0.5694444444444444198, 0.5722222222222221877, 0.5749999999999999556, 0.5777777777777777235, 0.5805555555555556024, 0.5833333333333333703, 0.5861111111111112493, 0.5888888888888889062, 0.5916666666666666741, 0.5944444444444444420, 0.5972222222222222099, 0.5999999999999999778, 0.6027777777777777457, 0.6055555555555555136, 0.6083333333333332815, 0.6111111111111111605, 0.6138888888888889284, 0.6166666666666666963, 0.6194444444444444642, 0.6222222222222222321, 0.6250000000000000000, 0.6277777777777777679, 0.6305555555555555358, 0.6333333333333333037, 0.6361111111111110716, 0.6388888888888888395, 0.6416666666666667185, 0.6444444444444444864, 0.6472222222222222543, 0.6500000000000000222, 0.6527777777777777901, 0.6555555555555555580, 0.6583333333333333259, 0.6611111111111110938, 0.6638888888888888618, 0.6666666666666666297, 0.6694444444444443976, 0.6722222222222222765, 0.6750000000000000444, 0.6777777777777778123, 0.6805555555555555802, 0.6833333333333333481, 0.6861111111111111160, 0.6888888888888888840, 0.6916666666666666519, 0.6944444444444444198, 0.6972222222222221877, 0.7000000000000000666, 0.7027777777777777235, 0.7055555555555556024, 0.7083333333333333703, 0.7111111111111111382, 0.7138888888888889062, 0.7166666666666666741, 0.7194444444444444420, 0.7222222222222222099, 0.7249999999999999778, 0.7277777777777777457, 0.7305555555555555136, 0.7333333333333332815, 0.7361111111111111605, 0.7388888888888889284, 0.7416666666666666963, 0.7444444444444444642, 0.7472222222222222321, 0.7500000000000000000, 0.7527777777777777679, 0.7555555555555555358, 0.7583333333333333037, 0.7611111111111110716, 0.7638888888888888395, 0.7666666666666667185, 0.7694444444444444864, 0.7722222222222222543, 0.7750000000000000222, 0.7777777777777777901, 0.7805555555555555580, 0.7833333333333333259, 0.7861111111111110938, 0.7888888888888888618, 0.7916666666666666297, 0.7944444444444443976, 0.7972222222222222765, 0.8000000000000000444, 0.8027777777777778123, 0.8055555555555555802, 0.8083333333333333481, 0.8111111111111111160, 0.8138888888888888840, 0.8166666666666666519, 0.8194444444444444198, 0.8222222222222221877, 0.8249999999999999556, 0.8277777777777777235, 0.8305555555555556024, 0.8333333333333333703, 0.8361111111111111382, 0.8388888888888889062, 0.8416666666666666741, 0.8444444444444444420, 0.8472222222222222099, 0.8499999999999999778, 0.8527777777777777457, 0.8555555555555555136, 0.8583333333333332815, 0.8611111111111111605, 0.8638888888888889284, 0.8666666666666666963, 0.8694444444444444642, 0.8722222222222222321, 0.8750000000000000000, 0.8777777777777777679, 0.8805555555555555358, 0.8833333333333333037, 0.8861111111111110716, 0.8888888888888888395, 0.8916666666666667185, 0.8944444444444444864, 0.8972222222222222543, 0.8999999999999999112, 0.9027777777777777901, 0.9055555555555555580, 0.9083333333333333259, 0.9111111111111110938, 0.9138888888888888618, 0.9166666666666666297, 0.9194444444444443976, 0.9222222222222222765, 0.9250000000000000444, 0.9277777777777778123, 0.9305555555555555802, 0.9333333333333333481, 0.9361111111111111160, 0.9388888888888888840, 0.9416666666666666519, 0.9444444444444444198, 0.9472222222222221877, 0.9499999999999999556, 0.9527777777777777235, 0.9555555555555556024, 0.9583333333333333703, 0.9611111111111111382, 0.9638888888888889062, 0.9666666666666666741, 0.9694444444444444420, 0.9722222222222222099, 0.9749999999999999778 ),
 .UNSPECIFIED. ) 
 CURVE ( )  GEOMETRIC_REPRESENTATION_ITEM ( )  RATIONAL_B_SPLINE_CURVE ( ( 1.000000000000000000, 0.9659258262890683122, 1.000000000000000000, 0.9659258262890683122, 1.000000000000000000, 0.9659258262890683122, 1.000000000000000000, 0.9659258262890683122, 1.000000000000000000, 0.9659258262890683122, 1.000000000000000000, 0.9659258262890683122, 1.000000000000000000, 0.9659258262890683122, 1.000000000000000000, 0.9659258262890683122, 1.000000000000000000, 0.9659258262890683122, 1.000000000000000000, 0.9659258262890683122, 1.000000000000000000, 0.9659258262890683122, 1.000000000000000000, 0.9659258262890683122, 1.000000000000000000, 0.9659258262890683122, 1.000000000000000000, 0.9659258262890683122, 1.000000000000000000, 0.9659258262890683122, 1.000000000000000000, 0.9659258262890683122, 1.000000000000000000, 0.9659258262890683122, 1.000000000000000000, 0.9659258262890683122, 1.000000000000000000, 0.9659258262890683122, 1.000000000000000000, 0.9659258262890683122, 1.000000000000000000, 0.9659258262890683122, 1.000000000000000000, 0.9659258262890683122, 1.000000000000000000, 0.9659258262890683122, 1.000000000000000000, 0.9659258262890683122, 1.000000000000000000, 0.9659258262890683122, 1.000000000000000000, 0.9659258262890683122, 1.000000000000000000, 0.9659258262890683122, 1.000000000000000000, 0.9659258262890683122, 1.000000000000000000, 0.9659258262890683122, 1.000000000000000000, 0.9659258262890683122, 1.000000000000000000, 0.9659258262890683122, 1.000000000000000000, 0.9659258262890683122, 1.000000000000000000, 0.9659258262890683122, 1.000000000000000000, 0.9659258262890683122, 1.000000000000000000, 0.9659258262890683122, 1.000000000000000000, 0.9659258262890683122, 1.000000000000000000, 0.9659258262890683122, 1.000000000000000000, 0.9659258262890683122, 1.000000000000000000, 0.9659258262890683122, 1.000000000000000000, 0.9659258262890683122, 1.000000000000000000, 0.9659258262890683122, 1.000000000000000000, 0.9659258262890683122, 1.000000000000000000, 0.9659258262890683122, 1.000000000000000000, 0.9659258262890683122, 1.000000000000000000, 0.9659258262890683122, 1.000000000000000000, 0.9659258262890683122, 1.000000000000000000, 0.9659258262890683122, 1.000000000000000000, 0.9659258262890683122, 1.000000000000000000, 0.9659258262890683122, 1.000000000000000000, 0.9659258262890683122, 1.000000000000000000, 0.9659258262890683122, 1.000000000000000000, 0.9659258262890683122, 1.000000000000000000, 0.9659258262890683122, 1.000000000000000000, 0.9659258262890683122, 1.000000000000000000, 0.9659258262890683122, 1.000000000000000000, 0.9659258262890683122, 1.000000000000000000, 0.9659258262890683122, 1.000000000000000000, 0.9659258262890683122, 1.000000000000000000, 0.9659258262890683122, 1.000000000000000000, 0.9659258262890683122, 1.000000000000000000, 0.9659258262890683122, 1.000000000000000000, 0.9659258262890683122, 1.000000000000000000, 0.9659258262890683122, 1.000000000000000000, 0.9659258262890683122, 1.000000000000000000, 0.9659258262890683122, 1.000000000000000000, 0.9659258262890683122, 1.000000000000000000, 0.9659258262890683122, 1.000000000000000000, 0.9659258262890683122, 1.000000000000000000, 0.9659258262890683122, 1.000000000000000000, 0.9659258262890683122, 1.000000000000000000, 0.9659258262890683122, 1.000000000000000000, 0.9659258262890683122, 1.000000000000000000, 0.9659258262890683122, 1.000000000000000000, 0.9659258262890683122, 1.000000000000000000, 0.9659258262890683122, 1.000000000000000000, 0.9659258262890683122, 1.000000000000000000, 0.9659258262890683122, 1.000000000000000000, 0.9659258262890683122, 1.000000000000000000, 0.9659258262890683122, 1.000000000000000000, 0.9659258262890683122, 1.000000000000000000, 0.9659258262890683122, 1.000000000000000000, 0.9659258262890683122, 1.000000000000000000, 0.9659258262890683122, 1.000000000000000000, 0.9659258262890683122, 1.000000000000000000, 0.9659258262890683122, 1.000000000000000000, 0.9659258262890683122, 1.000000000000000000, 0.9659258262890683122, 1.000000000000000000, 0.9659258262890683122, 1.000000000000000000, 0.9659258262890683122, 1.000000000000000000, 0.9659258262890683122, 1.000000000000000000, 0.9659258262890683122, 1.000000000000000000, 0.9659258262890683122, 1.000000000000000000, 0.9659258262890683122, 1.000000000000000000, 0.9659258262890683122, 1.000000000000000000, 0.9659258262890683122, 1.000000000000000000, 0.9659258262890683122, 1.000000000000000000, 0.9659258262890683122, 1.000000000000000000, 0.9659258262890683122, 1.000000000000000000, 0.9659258262890683122, 1.000000000000000000, 0.9659258262890683122, 1.000000000000000000, 0.9659258262890683122, 1.000000000000000000, 0.9659258262890683122, 1.000000000000000000, 0.9659258262890683122, 1.000000000000000000, 0.9659258262890683122, 1.000000000000000000, 0.9659258262890683122, 1.000000000000000000, 0.9659258262890683122, 1.000000000000000000, 0.9659258262890683122, 1.000000000000000000, 0.9659258262890683122, 1.000000000000000000, 0.9659258262890683122, 1.000000000000000000, 0.9659258262890683122, 1.000000000000000000, 0.9659258262890683122, 1.000000000000000000, 0.9659258262890683122, 1.000000000000000000, 0.9659258262890683122, 1.000000000000000000, 0.9659258262890683122, 1.000000000000000000, 0.9659258262890683122, 1.000000000000000000, 0.9659258262890683122, 1.000000000000000000, 0.9659258262890683122, 1.000000000000000000, 0.9659258262890683122, 1.000000000000000000, 0.9659258262890683122, 1.000000000000000000, 0.9659258262890683122, 1.000000000000000000, 0.9659258262890683122, 1.000000000000000000, 0.9659258262890683122, 1.000000000000000000, 0.9659258262890683122, 1.000000000000000000, 0.9659258262890683122, 1.000000000000000000, 0.9659258262890683122, 1.000000000000000000, 0.9659258262890683122, 1.000000000000000000, 0.9659258262890683122, 1.000000000000000000, 0.9659258262890683122, 1.000000000000000000, 0.9659258262890683122, 1.000000000000000000, 0.9659258262890683122, 1.000000000000000000, 0.9659258262890683122, 1.000000000000000000, 0.9659258262890683122, 1.000000000000000000, 0.9659258262890683122, 1.000000000000000000, 0.9659258262890683122, 1.000000000000000000, 0.9659258262890683122, 1.000000000000000000, 0.9659258262890683122, 1.000000000000000000, 0.9659258262890683122, 1.000000000000000000, 0.9659258262890683122, 1.000000000000000000, 0.9659258262890683122, 1.000000000000000000, 0.9659258262890683122, 1.000000000000000000, 0.9659258262890683122, 1.000000000000000000, 0.9659258262890683122, 1.000000000000000000, 0.9659258262890683122, 1.000000000000000000, 0.9659258262890683122, 1.000000000000000000, 0.9659258262890683122, 1.000000000000000000, 0.9659258262890683122, 1.000000000000000000, 0.9659258262890683122, 1.000000000000000000, 0.9659258262890683122, 1.000000000000000000, 0.9659258262890683122, 1.000000000000000000, 0.9659258262890683122, 1.000000000000000000, 0.9659258262890683122, 1.000000000000000000, 0.9659258262890683122, 1.000000000000000000, 0.9659258262890683122, 1.000000000000000000, 0.9659258262890683122, 1.000000000000000000, 0.9659258262890683122, 1.000000000000000000, 0.9659258262890683122, 1.000000000000000000, 0.9659258262890683122, 1.000000000000000000, 0.9659258262890683122, 1.000000000000000000, 0.9659258262890683122, 1.000000000000000000, 0.9659258262890683122, 1.000000000000000000, 0.9659258262890683122, 1.000000000000000000, 0.9659258262890683122, 1.000000000000000000, 0.9659258262890683122, 1.000000000000000000, 0.9659258262890683122, 1.000000000000000000, 0.9659258262890683122, 1.000000000000000000, 0.9659258262890683122, 1.000000000000000000, 0.9659258262890683122, 1.000000000000000000, 0.9659258262890683122, 1.000000000000000000, 0.9659258262890683122, 1.000000000000000000, 0.9659258262890683122, 1.000000000000000000, 0.9659258262890683122, 1.000000000000000000, 0.9659258262890683122, 1.000000000000000000, 0.9659258262890683122, 1.000000000000000000, 0.9659258262890683122, 1.000000000000000000, 0.9659258262890683122, 1.000000000000000000, 0.9659258262890683122, 1.000000000000000000, 0.9659258262890683122, 1.000000000000000000, 0.9659258262890683122, 1.000000000000000000, 0.9659258262890683122, 1.000000000000000000, 0.9659258262890683122, 1.000000000000000000, 0.9659258262890683122, 1.000000000000000000, 0.9659258262890683122, 1.000000000000000000, 0.9659258262890683122, 1.000000000000000000, 0.9659258262890683122, 1.000000000000000000, 0.9659258262890683122, 1.000000000000000000, 0.9659258262890683122, 1.000000000000000000, 0.9659258262890683122, 1.000000000000000000, 0.9659258262890683122, 1.000000000000000000, 0.9659258262890683122, 1.000000000000000000, 0.9659258262890683122, 1.000000000000000000, 0.9659258262890683122, 1.000000000000000000, 0.9659258262890683122, 1.000000000000000000, 0.9659258262890683122, 1.000000000000000000, 0.9659258262890683122, 1.000000000000000000, 0.9659258262890683122, 1.000000000000000000, 0.9659258262890683122, 1.000000000000000000, 0.9659258262890683122, 1.000000000000000000, 0.9659258262890683122, 1.000000000000000000, 0.9659258262890683122, 1.000000000000000000, 0.9659258262890683122, 1.000000000000000000, 0.9659258262890683122, 1.000000000000000000, 0.9659258262890683122, 1.000000000000000000, 0.9659258262890683122, 1.000000000000000000, 0.9659258262890683122, 1.000000000000000000, 0.9659258262890683122, 1.000000000000000000, 0.9659258262890683122, 1.000000000000000000, 0.9659258262890683122, 1.000000000000000000, 0.9659258262890683122, 1.000000000000000000, 0.9659258262890683122, 1.000000000000000000, 0.9659258262890683122, 1.000000000000000000, 0.9659258262890683122, 1.000000000000000000, 0.9659258262890683122, 1.000000000000000000, 0.9659258262890683122, 1.000000000000000000, 0.9659258262890683122, 1.000000000000000000, 0.9659258262890683122, 1.000000000000000000, 0.9659258262890683122, 1.000000000000000000, 0.9659258262890683122, 1.000000000000000000, 0.9659258262890683122, 1.000000000000000000, 0.9659258262890683122, 1.000000000000000000, 0.9659258262890683122, 1.000000000000000000, 0.9659258262890683122, 1.000000000000000000, 0.9659258262890683122, 1.000000000000000000, 0.9659258262890683122, 1.000000000000000000, 0.9659258262890683122, 1.000000000000000000, 0.9659258262890683122, 1.000000000000000000, 0.9659258262890683122, 1.000000000000000000, 0.9659258262890683122, 1.000000000000000000, 0.9659258262890683122, 1.000000000000000000, 0.9659258262890683122, 1.000000000000000000, 0.9659258262890683122, 1.000000000000000000, 0.9659258262890683122, 1.000000000000000000, 0.9659258262890683122, 1.000000000000000000, 0.9659258262890683122, 1.000000000000000000, 0.9659258262890683122, 1.000000000000000000, 0.9659258262890683122, 1.000000000000000000, 0.9659258262890683122, 1.000000000000000000, 0.9659258262890683122, 1.000000000000000000, 0.9659258262890683122, 1.000000000000000000, 0.9659258262890683122, 1.000000000000000000, 0.9659258262890683122, 1.000000000000000000, 0.9659258262890683122, 1.000000000000000000, 0.9659258262890683122, 1.000000000000000000, 0.9659258262890683122, 1.000000000000000000, 0.9659258262890683122, 1.000000000000000000, 0.9659258262890683122, 1.000000000000000000, 0.9659258262890683122, 1.000000000000000000, 0.9659258262890683122, 1.000000000000000000, 0.9659258262890683122, 1.000000000000000000, 0.9659258262890683122, 1.000000000000000000, 0.9659258262890683122, 1.000000000000000000, 0.9659258262890683122, 1.000000000000000000, 0.9659258262890683122, 1.000000000000000000, 0.9659258262890683122, 1.000000000000000000, 0.9659258262890683122, 1.000000000000000000, 0.9659258262890683122, 1.000000000000000000, 0.9659258262890683122, 1.000000000000000000, 0.9659258262890683122, 1.000000000000000000, 0.9659258262890683122, 1.000000000000000000, 0.9659258262890683122, 1.000000000000000000, 0.9659258262890683122, 1.000000000000000000, 0.9659258262890683122, 1.000000000000000000, 0.9659258262890683122, 1.000000000000000000, 0.9659258262890683122, 1.000000000000000000, 0.9659258262890683122, 1.000000000000000000, 0.9659258262890683122, 1.000000000000000000, 0.9659258262890683122, 1.000000000000000000, 0.9659258262890683122, 1.000000000000000000, 0.9659258262890683122, 1.000000000000000000, 0.9659258262890683122, 1.000000000000000000, 0.9659258262890683122, 1.000000000000000000, 0.9659258262890683122, 1.000000000000000000, 0.9659258262890683122, 1.000000000000000000, 0.9659258262890683122, 1.000000000000000000, 0.9659258262890683122, 1.000000000000000000, 0.9659258262890683122, 1.000000000000000000, 0.9659258262890683122, 1.000000000000000000, 0.9659258262890683122, 1.000000000000000000, 0.9659258262890683122, 1.000000000000000000, 0.9659258262890683122, 1.000000000000000000, 0.9659258262890683122, 1.000000000000000000, 0.9659258262890683122, 1.000000000000000000, 0.9659258262890683122, 1.000000000000000000, 0.9659258262890683122, 1.000000000000000000, 0.9659258262890683122, 1.000000000000000000, 0.9659258262890683122, 1.000000000000000000, 0.9659258262890683122, 1.000000000000000000, 0.9659258262890683122, 1.000000000000000000, 0.9659258262890683122, 1.000000000000000000, 0.9659258262890683122, 1.000000000000000000, 0.9659258262890683122, 1.000000000000000000, 0.9659258262890683122, 1.000000000000000000, 0.9659258262890683122, 1.000000000000000000, 0.9659258262890683122, 1.000000000000000000, 0.9659258262890683122, 1.000000000000000000, 0.9659258262890683122, 1.000000000000000000, 0.9659258262890683122, 1.000000000000000000, 0.9659258262890683122, 1.000000000000000000, 0.9659258262890683122, 1.000000000000000000, 0.9659258262890683122, 1.000000000000000000, 0.9659258262890683122, 1.000000000000000000, 0.9659258262890683122, 1.000000000000000000, 0.9659258262890683122, 1.000000000000000000, 0.9659258262890683122, 1.000000000000000000, 0.9659258262890683122, 1.000000000000000000, 0.9659258262890683122, 1.000000000000000000, 0.9659258262890683122, 1.000000000000000000, 0.9659258262890683122, 1.000000000000000000, 0.9659258262890683122, 1.000000000000000000, 0.9659258262890683122, 1.000000000000000000, 0.9659258262890683122, 1.000000000000000000, 0.9659258262890683122, 1.000000000000000000, 0.9659258262890683122, 1.000000000000000000, 0.9659258262890683122, 1.000000000000000000, 0.9659258262890683122, 1.000000000000000000, 0.9659258262890683122, 1.000000000000000000, 0.9659258262890683122, 1.000000000000000000, 0.9659258262890683122, 1.000000000000000000, 0.9659258262890683122, 1.000000000000000000, 0.9659258262890683122, 1.000000000000000000, 0.9659258262890683122, 1.000000000000000000, 0.9659258262890683122, 1.000000000000000000, 0.9659258262890683122, 1.000000000000000000, 0.9659258262890683122, 1.000000000000000000, 0.9659258262890683122, 1.000000000000000000, 0.9659258262890683122, 1.000000000000000000, 0.9659258262890683122, 1.000000000000000000, 0.9659258262890683122, 1.000000000000000000, 0.9659258262890683122, 1.000000000000000000, 0.9659258262890683122, 1.000000000000000000, 0.9659258262890683122, 1.000000000000000000, 0.9659258262890683122, 1.000000000000000000, 0.9659258262890683122, 1.000000000000000000, 0.9659258262890683122, 1.000000000000000000, 0.9659258262890683122, 1.000000000000000000, 0.9659258262890683122, 1.000000000000000000, 0.9659258262890683122, 1.000000000000000000, 0.9659258262890683122, 1.000000000000000000, 0.9659258262890683122, 1.000000000000000000, 0.9659258262890683122, 1.000000000000000000, 0.9659258262890683122, 1.000000000000000000, 0.9659258262890683122, 1.000000000000000000, 0.9659258262890683122, 1.000000000000000000, 0.9659258262890683122, 1.000000000000000000, 0.9659258262890683122, 1.000000000000000000, 0.9659258262890683122, 1.000000000000000000, 0.9659258262890683122, 1.000000000000000000, 0.9659258262890683122, 1.000000000000000000, 0.9659258262890683122, 1.000000000000000000, 0.9659258262890683122, 1.000000000000000000, 0.9659258262890683122, 1.000000000000000000, 0.9659258262890683122, 1.000000000000000000 ) ) 
 REPRESENTATION_ITEM ( '' )  );
#110123 = EDGE_LOOP ( 'NONE', ( #42648, #100161, #138880, #27871 ) ) ;
#110124 = LINE ( 'NONE', #22388, #19015 ) ;
#110125 = CARTESIAN_POINT ( 'NONE',  ( 13.89997294953710494, 4.461849672132297329, -4.461849672132302658 ) ) ;
#110126 = CARTESIAN_POINT ( 'NONE',  ( 25.49999999999982236, 5.696342897626525570, -7.587980461218338135 ) ) ;
#110127 = CARTESIAN_POINT ( 'NONE',  ( -27.32816939922334143, -18.74070752338409562, 4.000000000000000000 ) ) ;
#110128 = VERTEX_POINT ( 'NONE', #75483 ) ;
#110129 = DIRECTION ( 'NONE',  ( -0.5735764363510499342, -0.8191520442889891340, 0.000000000000000000 ) ) ;
#110130 = VERTEX_POINT ( 'NONE', #20351 ) ;
#110131 = FACE_OUTER_BOUND ( 'NONE', #76122, .T. ) ;
#110132 = AXIS2_PLACEMENT_3D ( 'NONE', #59227, #127286, #27984 ) ;
#110133 = CARTESIAN_POINT ( 'NONE',  ( 16.83790314143521982, -6.871911579029513106, -3.967499999999993587 ) ) ;
#110134 = VERTEX_POINT ( 'NONE', #130589 ) ;
#110135 = CARTESIAN_POINT ( 'NONE',  ( 82.45376352523145158, -6.109999999999999432, -3.741295971395163529E-16 ) ) ;
#110136 = CARTESIAN_POINT ( 'NONE',  ( 5.979043268340604733, -9.486524475911640053, -0.5800208356449471081 ) ) ;
#110137 = VECTOR ( 'NONE', #77818, 1000.000000000000000 ) ;
#110139 = EDGE_CURVE ( 'NONE', #70259, #136354, #55159, .T. ) ;
#110138 = LINE ( 'NONE', #130508, #136970 ) ;
#110140 = FACE_OUTER_BOUND ( 'NONE', #5028, .T. ) ;
#110141 = ORIENTED_EDGE ( 'NONE', *, *, #110917, .T. ) ;
#110142 = VERTEX_POINT ( 'NONE', #33437 ) ;
#110143 = ORIENTED_EDGE ( 'NONE', *, *, #86758, .T. ) ;
#110144 = FACE_OUTER_BOUND ( 'NONE', #94461, .T. ) ;
#110145 = DIRECTION ( 'NONE',  ( 1.000000000000000000, 0.000000000000000000, 0.000000000000000000 ) ) ;
#110146 = PLANE ( 'NONE',  #134477 ) ;
#110147 = FACE_OUTER_BOUND ( 'NONE', #6650, .T. ) ;
#110148 = LINE ( 'NONE', #111598, #14863 ) ;
#110149 = ORIENTED_EDGE ( 'NONE', *, *, #36289, .T. ) ;
#110150 = CARTESIAN_POINT ( 'NONE',  ( -18.18398860626898994, 28.73617430169800002, 5.000000000000000000 ) ) ;
#110151 = EDGE_CURVE ( 'NONE', #70446, #32019, #98643, .T. ) ;
#110152 = AXIS2_PLACEMENT_3D ( 'NONE', #38713, #105378, #116270 ) ;
#110153 = CARTESIAN_POINT ( 'NONE',  ( 0.000000000000000000, -4.870000000000014317, -40.00000000000000000 ) ) ;
#110154 = CARTESIAN_POINT ( 'NONE',  ( 38.99451991528749062, 28.92564299267965211, 4.000000000000000000 ) ) ;
#110155 = VERTEX_POINT ( 'NONE', #142179 ) ;
#110156 = CARTESIAN_POINT ( 'NONE',  ( -34.57058949319514340, 22.20469455417149618, 4.123089426795147006 ) ) ;
#110157 = DIRECTION ( 'NONE',  ( 0.7071067811865487940, -0.7071067811865463515, 0.000000000000000000 ) ) ;
#110158 = ORIENTED_EDGE ( 'NONE', *, *, #129858, .F. ) ;
#110161 = ADVANCED_FACE ( 'NONE', ( #56630 ), #89216, .F. ) ;
#110160 = ORIENTED_EDGE ( 'NONE', *, *, #76, .F. ) ;
#110159 = DIRECTION ( 'NONE',  ( -0.6830127018922181881, 0.6830127018922202975, -0.2588190451025214056 ) ) ;
#110162 = ORIENTED_EDGE ( 'NONE', *, *, #93949, .T. ) ;
#110163 = EDGE_CURVE ( 'NONE', #63317, #91527, #21078, .T. ) ;
#110164 = CARTESIAN_POINT ( 'NONE',  ( 1.499999999999987566, 8.319652575858389909, -8.582050562765823898 ) ) ;
#110165 = LINE ( 'NONE', #99280, #97001 ) ;
#110166 = ORIENTED_EDGE ( 'NONE', *, *, #121642, .F. ) ;
#110167 = LINE ( 'NONE', #44243, #111385 ) ;
#110168 = UNCERTAINTY_MEASURE_WITH_UNIT (LENGTH_MEASURE( 1.000000000000000082E-05 ), #92059, 'distance_accuracy_value', 'NONE');
#110169 = PLANE ( 'NONE',  #80003 ) ;
#110170 = VECTOR ( 'NONE', #13938, 1000.000000000000000 ) ;
#110171 = FILL_AREA_STYLE ('',( #120311 ) ) ;
#110172 = VECTOR ( 'NONE', #76113, 1000.000000000000000 ) ;
#110173 = DIRECTION ( 'NONE',  ( -0.6830127018922180770, -0.6830127018922204085, -0.2588190451025213501 ) ) ;
#110175 = MECHANICAL_DESIGN_GEOMETRIC_PRESENTATION_REPRESENTATION (  '', ( #142600 ), #24508 ) ;
#110174 = LINE ( 'NONE', #2099, #37358 ) ;
#110176 = LINE ( 'NONE', #102192, #39877 ) ;
#110177 = FACE_OUTER_BOUND ( 'NONE', #33264, .T. ) ;
#110178 = DIRECTION ( 'NONE',  ( 0.6830127018922180770, -0.6830127018922204085, -0.2588190451025213501 ) ) ;
#110179 = CARTESIAN_POINT ( 'NONE',  ( 39.18398860626899705, 28.73617430169814568, 5.000000000000000000 ) ) ;
#110180 = FACE_OUTER_BOUND ( 'NONE', #79925, .T. ) ;
#110181 = LINE ( 'NONE', #10854, #87640 ) ;
#110182 = AXIS2_PLACEMENT_3D ( 'NONE', #60130, #79774, #123955 ) ;
#110183 = LINE ( 'NONE', #134112, #134539 ) ;
#110184 = CARTESIAN_POINT ( 'NONE',  ( -26.57672154193630476, 11.25929247661559529, 17.85071094206590203 ) ) ;
#110185 = ORIENTED_EDGE ( 'NONE', *, *, #92167, .F. ) ;
#110186 = EDGE_CURVE ( 'NONE', #45858, #111873, #98888, .T. ) ;
#110187 = EDGE_LOOP ( 'NONE', ( #82227, #1282, #29672, #42163, #69361, #56599 ) ) ;
#110188 = CARTESIAN_POINT ( 'NONE',  ( 98.41666666666667140, -6.884901960086287076, -3.975000000000000977 ) ) ;
#110189 = EDGE_CURVE ( 'NONE', #131796, #123357, #97942, .T. ) ;
#110190 = ORIENTED_EDGE ( 'NONE', *, *, #37133, .F. ) ;
#110191 = ORIENTED_EDGE ( 'NONE', *, *, #34636, .T. ) ;
#110192 = ORIENTED_EDGE ( 'NONE', *, *, #1169, .T. ) ;
#110193 = LINE ( 'NONE', #2866, #38738 ) ;
#110194 = CARTESIAN_POINT ( 'NONE',  ( 12.32816939922343913, -12.74070752338415957, 4.000000000000000000 ) ) ;
#110195 = ORIENTED_EDGE ( 'NONE', *, *, #73311, .T. ) ;
#110196 = CARTESIAN_POINT ( 'NONE',  ( 8.811592354503320124, 9.902892378096218942E-16, 0.000000000000000000 ) ) ;
#110197 = LINE ( 'NONE', #100773, #71969 ) ;
#110198 = DIRECTION ( 'NONE',  ( -0.7071067811865486830, -0.7071067811865464625, 0.000000000000000000 ) ) ;
#110199 = LINE ( 'NONE', #110902, #83679 ) ;
#110200 = ORIENTED_EDGE ( 'NONE', *, *, #53483, .F. ) ;
#110201 = ADVANCED_FACE ( 'NONE', ( #53743 ), #108771, .T. ) ;
#110202 = FACE_OUTER_BOUND ( 'NONE', #72229, .T. ) ;
#110203 = DIRECTION ( 'NONE',  ( 0.6830127018922180770, 0.6830127018922202975, -0.2588190451025213501 ) ) ;
#110204 = CARTESIAN_POINT ( 'NONE',  ( 24.20969143188526118, 6.176090689687629975, 5.000000000000000000 ) ) ;
#110205 = LINE ( 'NONE', #131268, #74660 ) ;
#110206 = CARTESIAN_POINT ( 'NONE',  ( 18.95159235450331892, 9.902892378096218942E-16, 0.000000000000000000 ) ) ;
#110207 = CARTESIAN_POINT ( 'NONE',  ( 152.8142135623730837, 26.96999999999993847, 34.92499999999998295 ) ) ;
#110208 = CARTESIAN_POINT ( 'NONE',  ( 6.489213562373093325, -27.52281430457059841, 5.000000000000000000 ) ) ;
#110209 = ORIENTED_EDGE ( 'NONE', *, *, #136897, .T. ) ;
#110210 = VERTEX_POINT ( 'NONE', #142870 ) ;
#110211 = CARTESIAN_POINT ( 'NONE',  ( 121.6254301918981184, 5.291415217122919401, 3.055000000000002824 ) ) ;
#110212 = ORIENTED_EDGE ( 'NONE', *, *, #94565, .F. ) ;
#110213 = CARTESIAN_POINT ( 'NONE',  ( 26.99451991528749417, 28.92564299267956685, 4.000000000000000000 ) ) ;
#110214 = DIRECTION ( 'NONE',  ( 0.7071067811865486830, -0.7071067811865464625, -0.000000000000000000 ) ) ;
#110215 = AXIS2_PLACEMENT_3D ( 'NONE', #112200, #71548, #91174 ) ;
#110216 = DIRECTION ( 'NONE',  ( -0.7071067811865486830, -0.7071067811865463515, 0.000000000000000000 ) ) ;
#110217 = LINE ( 'NONE', #98645, #60582 ) ;
#110218 = LINE ( 'NONE', #77641, #60418 ) ;
#110219 = CARTESIAN_POINT ( 'NONE',  ( 117.0162635252314374, -4.472830434245839371, 4.472830434245839371 ) ) ;
#110220 = VERTEX_POINT ( 'NONE', #86365 ) ;
#110221 = ORIENTED_EDGE ( 'NONE', *, *, #110862, .T. ) ;
#110222 = CARTESIAN_POINT ( 'NONE',  ( 4.499999999999968914, -8.568876922607726598, 4.000000000000000000 ) ) ;
#110223 = VERTEX_POINT ( 'NONE', #66747 ) ;
#110224 = ORIENTED_EDGE ( 'NONE', *, *, #60751, .F. ) ;
#110225 = CARTESIAN_POINT ( 'NONE',  ( 39.81293019189809712, -1.637169565754159617, -6.110000000000001208 ) ) ;
#110226 = ORIENTED_EDGE ( 'NONE', *, *, #10728, .T. ) ;
#110227 = PLANE ( 'NONE',  #123211 ) ;
#110228 = EDGE_CURVE ( 'NONE', #11327, #77069, #105806, .T. ) ;
#110229 = LINE ( 'NONE', #65361, #126520 ) ;
#110230 = PLANE ( 'NONE',  #15941 ) ;
#110231 = AXIS2_PLACEMENT_3D ( 'NONE', #85146, #52518, #96703 ) ;
#110232 = ADVANCED_FACE ( 'NONE', ( #67483 ), #9463, .F. ) ;
#110233 = CARTESIAN_POINT ( 'NONE',  ( 29.51626352523143737, -4.472830434245839371, 4.472830434245839371 ) ) ;
#110234 = EDGE_CURVE ( 'NONE', #143094, #94959, #132009, .T. ) ;
#110235 = EDGE_LOOP ( 'NONE', ( #66208, #12316, #40870, #127809 ) ) ;
#110237 = ADVANCED_FACE ( 'NONE', ( #76934 ), #121107, .F. ) ;
#110236 = DIRECTION ( 'NONE',  ( -0.000000000000000000, -0.3543493200069152693, 0.9351131265310292928 ) ) ;
#110238 = ORIENTED_EDGE ( 'NONE', *, *, #122185, .T. ) ;
#110239 = ORIENTED_EDGE ( 'NONE', *, *, #41024, .F. ) ;
#110240 = EDGE_LOOP ( 'NONE', ( #46179, #130393, #87200, #31775 ) ) ;
#110241 = ADVANCED_FACE ( 'NONE', ( #10893 ), #13752, .T. ) ;
#110242 = CARTESIAN_POINT ( 'NONE',  ( 11.99451991528749417, 28.92564299267946382, 4.000000000000000000 ) ) ;
#110243 = ORIENTED_EDGE ( 'NONE', *, *, #12697, .T. ) ;
#110244 = LINE ( 'NONE', #86403, #59889 ) ;
#110246 = ADVANCED_FACE ( 'NONE', ( #60162 ), #123988, .F. ) ;
#110245 = VECTOR ( 'NONE', #120048, 999.9999999999998863 ) ;
#110247 = DIRECTION ( 'NONE',  ( -0.6830127018922180770, -0.6830127018922204085, -0.2588190451025213501 ) ) ;
#110248 = DIRECTION ( 'NONE',  ( 0.000000000000000000, 0.000000000000000000, 1.000000000000000000 ) ) ;
#110249 = DIRECTION ( 'NONE',  ( -0.7071067811865487940, 0.7071067811865463515, -0.000000000000000000 ) ) ;
#110250 = ADVANCED_FACE ( 'NONE', ( #57321 ), #136266, .F. ) ;
#110252 = FACE_BOUND ( 'NONE', #88241, .T. ) ;
#110251 = AXIS2_PLACEMENT_3D ( 'NONE', #128960, #117345, #139869 ) ;
#110253 = EDGE_LOOP ( 'NONE', ( #122956, #100989, #67443, #52693 ) ) ;
#110254 = EDGE_CURVE ( 'NONE', #133807, #31371, #4258, .T. ) ;
#110255 = DIRECTION ( 'NONE',  ( -1.000000000000000000, -0.000000000000000000, -0.000000000000000000 ) ) ;
#110256 = LINE ( 'NONE', #66786, #32884 ) ;
#110257 = PLANE ( 'NONE',  #99503 ) ;
#110258 = EDGE_LOOP ( 'NONE', ( #97199, #91189, #32106, #4403 ) ) ;
#110259 = CARTESIAN_POINT ( 'NONE',  ( -20.81601139373100295, 28.73617430169773002, 5.000000000000000000 ) ) ;
#110260 = ORIENTED_EDGE ( 'NONE', *, *, #921, .F. ) ;
#110261 = VERTEX_POINT ( 'NONE', #45733 ) ;
#110262 = CARTESIAN_POINT ( 'NONE',  ( 13.49999999999990408, 19.39370406404968250, 1.459788787078170502 ) ) ;
#110263 = EDGE_CURVE ( 'NONE', #96071, #94260, #37699, .T. ) ;
#110264 = AXIS2_PLACEMENT_3D ( 'NONE', #66934, #98823, #143055 ) ;
#110265 = ORIENTED_EDGE ( 'NONE', *, *, #4991, .T. ) ;
#110266 = VECTOR ( 'NONE', #77821, 1000.000000000000114 ) ;
#110267 = VECTOR ( 'NONE', #129865, 999.9999999999998863 ) ;
#110268 = CARTESIAN_POINT ( 'NONE',  ( 49.34959685856478728, 6.109999999999996767, 1.637169565754163836 ) ) ;
#110269 = VERTEX_POINT ( 'NONE', #134149 ) ;
#110270 = LINE ( 'NONE', #19709, #83519 ) ;
#110271 = FACE_OUTER_BOUND ( 'NONE', #53489, .T. ) ;
#110272 = DIRECTION ( 'NONE',  ( 0.7071067811865486830, -0.7071067811865464625, -0.000000000000000000 ) ) ;
#110273 = ORIENTED_EDGE ( 'NONE', *, *, #115950, .F. ) ;
#110274 = CARTESIAN_POINT ( 'NONE',  ( -21.18398860626899349, 28.73617430169802134, 5.000000000000000000 ) ) ;
#110275 = LINE ( 'NONE', #55215, #94471 ) ;
#110276 = VECTOR ( 'NONE', #90606, 999.9999999999998863 ) ;
#110277 = CARTESIAN_POINT ( 'NONE',  ( -31.92499999999997584, 2.729999999999987104, -36.39086428169088094 ) ) ;
#110278 = PLANE ( 'NONE',  #136581 ) ;
#110279 = CYLINDRICAL_SURFACE ( 'NONE', #136252, 0.5000000000000004441 ) ;
#110280 = DIRECTION ( 'NONE',  ( -0.7071067811865486830, 0.7071067811865464625, 0.000000000000000000 ) ) ;
#110281 = FACE_OUTER_BOUND ( 'NONE', #42675, .T. ) ;
#110282 = VERTEX_POINT ( 'NONE', #79082 ) ;
#110283 = EDGE_CURVE ( 'NONE', #120806, #118332, #36262, .T. ) ;
#110284 = ORIENTED_EDGE ( 'NONE', *, *, #72994, .T. ) ;
#110285 = ORIENTED_EDGE ( 'NONE', *, *, #104943, .F. ) ;
#110286 = CARTESIAN_POINT ( 'NONE',  ( -42.18398860626899705, 28.73617430169816700, 5.000000000000000000 ) ) ;
#110287 = PLANE ( 'NONE',  #5068 ) ;
#110288 = ORIENTED_EDGE ( 'NONE', *, *, #12717, .T. ) ;
#110289 = ORIENTED_EDGE ( 'NONE', *, *, #3651, .T. ) ;
#110290 = CARTESIAN_POINT ( 'NONE',  ( 7.939999999999994174, -35.76999999999998892, -10.00000000000000178 ) ) ;
#110291 = DIRECTION ( 'NONE',  ( -0.6830127018922181881, 0.6830127018922202975, -0.2588190451025214056 ) ) ;
#110292 = CARTESIAN_POINT ( 'NONE',  ( 47.99451991528749062, 28.92564299267971251, 4.000000000000000000 ) ) ;
#110293 = ORIENTED_EDGE ( 'NONE', *, *, #110082, .T. ) ;
#110294 = DIRECTION ( 'NONE',  ( 0.6830127018922181881, 0.6830127018922202975, -0.2588190451025214056 ) ) ;
#110295 = EDGE_CURVE ( 'NONE', #142173, #123033, #92750, .T. ) ;
#110296 = DIRECTION ( 'NONE',  ( -0.3543493200069162685, -0.000000000000000000, -0.9351131265310288487 ) ) ;
#110297 = CARTESIAN_POINT ( 'NONE',  ( 24.42123647476855552, -9.717572351234235426E-16, -7.934999999999990727 ) ) ;
#110298 = CIRCLE ( 'NONE', #94173, 2.500000000000000444 ) ;
#110299 = CARTESIAN_POINT ( 'NONE',  ( -30.18398860626900060, 28.73617430169808173, 5.000000000000000000 ) ) ;
#110300 = ORIENTED_EDGE ( 'NONE', *, *, #28044, .T. ) ;
#110301 = CARTESIAN_POINT ( 'NONE',  ( 123.4329301918981088, 1.637169565754156730, 6.110000000000001208 ) ) ;
#110303 = EDGE_CURVE ( 'NONE', #48102, #98765, #101496, .T. ) ;
#110302 = CARTESIAN_POINT ( 'NONE',  ( -77.99451991528749772, 28.92564299267992567, 4.000000000000000000 ) ) ;
#110304 = DIRECTION ( 'NONE',  ( 0.7071067811865486830, -0.7071067811865464625, -0.000000000000000000 ) ) ;
#110306 = EDGE_LOOP ( 'NONE', ( #142399, #92526, #74898, #93673 ) ) ;
#110305 = DIRECTION ( 'NONE',  ( -0.3543493200069163240, 0.000000000000000000, -0.9351131265310288487 ) ) ;
#110307 = VECTOR ( 'NONE', #122529, 1000.000000000000000 ) ;
#110308 = CARTESIAN_POINT ( 'NONE',  ( 67.89169371712955581, 2.130196079827421762, 7.950000000000000178 ) ) ;
#110309 = EDGE_LOOP ( 'NONE', ( #87267, #38266, #36651, #39006 ) ) ;
#110310 = PLANE ( 'NONE',  #100687 ) ;
#110311 = PLANE ( 'NONE',  #120998 ) ;
#110312 = DIRECTION ( 'NONE',  ( 0.7071067811865487940, 0.7071067811865463515, 0.000000000000000000 ) ) ;
#110313 = VERTEX_POINT ( 'NONE', #125409 ) ;
#110314 = EDGE_CURVE ( 'NONE', #49875, #140112, #13046, .T. ) ;
#110315 = CARTESIAN_POINT ( 'NONE',  ( -19.05000000000000071, 3.174999999999997158, 4.000000000000000000 ) ) ;
#110316 = CARTESIAN_POINT ( 'NONE',  ( -34.92500000000001137, 21.72500000000000142, 5.000000000000000000 ) ) ;
#110317 = VECTOR ( 'NONE', #127121, 1000.000000000000000 ) ;
#110318 = VERTEX_POINT ( 'NONE', #2149 ) ;
#110319 = CARTESIAN_POINT ( 'NONE',  ( -25.39999999999996305, 0.000000000000000000, 0.000000000000000000 ) ) ;
#110320 = LINE ( 'NONE', #131397, #109412 ) ;
#110321 = EDGE_LOOP ( 'NONE', ( #125563, #37630, #42998, #26285, #102551 ) ) ;
#110322 = CARTESIAN_POINT ( 'NONE',  ( 27.18398860626900060, 28.73617430169806042, 5.000000000000000000 ) ) ;
#110323 = VECTOR ( 'NONE', #16661, 1000.000000000000000 ) ;
#110326 = EDGE_CURVE ( 'NONE', #69443, #53276, #26797, .T. ) ;
#110325 = VERTEX_POINT ( 'NONE', #3586 ) ;
#110324 = DIRECTION ( 'NONE',  ( -0.000000000000000000, 0.000000000000000000, 1.000000000000000000 ) ) ;
#110327 = ORIENTED_EDGE ( 'NONE', *, *, #94380, .T. ) ;
#110328 = CARTESIAN_POINT ( 'NONE',  ( -13.10332671766740020, 3.690788593506699300, 4.000000000000000000 ) ) ;
#110329 = DIRECTION ( 'NONE',  ( -0.000000000000000000, -0.3543493200069152693, 0.9351131265310292928 ) ) ;
#110330 = ORIENTED_EDGE ( 'NONE', *, *, #94940, .T. ) ;
#110331 = VECTOR ( 'NONE', #19714, 1000.000000000000000 ) ;
#110332 = DIRECTION ( 'NONE',  ( 0.000000000000000000, -1.000000000000000000, 0.000000000000000000 ) ) ;
#110333 = DIRECTION ( 'NONE',  ( 0.6830127018922181881, 0.6830127018922202975, -0.2588190451025214056 ) ) ;
#110334 = DIRECTION ( 'NONE',  ( -0.000000000000000000, -0.000000000000000000, 1.000000000000000000 ) ) ;
#110335 = AXIS2_PLACEMENT_3D ( 'NONE', #103995, #138820, #28636 ) ;
#110336 = ORIENTED_EDGE ( 'NONE', *, *, #11969, .T. ) ;
#110337 = PRODUCT ( '1.7 Special Key', '1.7 Special Key', '', ( #136657 ) ) ;
#110338 = DIRECTION ( 'NONE',  ( 0.7071067811865487940, -0.7071067811865463515, 0.000000000000000000 ) ) ;
#110340 = VECTOR ( 'NONE', #140178, 1000.000000000000000 ) ;
#110339 = DIRECTION ( 'NONE',  ( 1.000000000000000000, 0.000000000000000000, 0.000000000000000000 ) ) ;
#110341 = DIRECTION ( 'NONE',  ( -0.6830127018922181881, 0.6830127018922202975, -0.2588190451025214056 ) ) ;
#110342 = LINE ( 'NONE', #22607, #101522 ) ;
#110343 = CARTESIAN_POINT ( 'NONE',  ( 27.91209685856478728, 5.291415217122922066, -3.054999999999995275 ) ) ;
#110344 = CARTESIAN_POINT ( 'NONE',  ( 8.148183550381396856, 17.25929247661554911, 8.802941693769220421 ) ) ;
#110345 = ORIENTED_EDGE ( 'NONE', *, *, #115035, .T. ) ;
#110346 = VERTEX_POINT ( 'NONE', #70355 ) ;
#110347 = PLANE ( 'NONE',  #106775 ) ;
#110348 = EDGE_CURVE ( 'NONE', #61052, #32802, #80490, .T. ) ;
#110349 = ORIENTED_EDGE ( 'NONE', *, *, #59592, .F. ) ;
#110350 = VECTOR ( 'NONE', #74465, 1000.000000000000114 ) ;
#110351 = VERTEX_POINT ( 'NONE', #59461 ) ;
#110352 = LINE ( 'NONE', #121244, #73416 ) ;
#110353 = DIRECTION ( 'NONE',  ( -0.7071067811865487940, 0.7071067811865463515, -0.000000000000000000 ) ) ;
#110354 = EDGE_LOOP ( 'NONE', ( #95620, #19371, #85914, #59979 ) ) ;
#110355 = PLANE ( 'NONE',  #23036 ) ;
#110356 = DIRECTION ( 'NONE',  ( 0.6830127018922180770, -0.6830127018922204085, -0.2588190451025213501 ) ) ;
#110357 = CARTESIAN_POINT ( 'NONE',  ( 2.293207492759234523, 20.25929247661550647, 20.83292124670813905 ) ) ;
#110358 = AXIS2_PLACEMENT_3D ( 'NONE', #86005, #88159, #142544 ) ;
#110359 = DIRECTION ( 'NONE',  ( 1.000000000000000000, 1.224606353822377258E-16, 0.000000000000000000 ) ) ;
#110360 = CARTESIAN_POINT ( 'NONE',  ( 119.0004301918981184, -3.055000000000002380, 5.291415217122920289 ) ) ;
#110361 = ORIENTED_EDGE ( 'NONE', *, *, #81379, .T. ) ;
#110362 = EDGE_CURVE ( 'NONE', #36893, #109568, #41230, .T. ) ;
#110363 = PLANE ( 'NONE',  #14037 ) ;
#110364 = CARTESIAN_POINT ( 'NONE',  ( 0.000000000000000000, -1.600000000000013634, 20.40202195861969159 ) ) ;
#110365 = CARTESIAN_POINT ( 'NONE',  ( -14.51078643762690490, -27.52281430457045275, 5.000000000000000000 ) ) ;
#110366 = LINE ( 'NONE', #66897, #8001 ) ;
#110367 = VECTOR ( 'NONE', #4101, 999.9999999999998863 ) ;
#110368 = CARTESIAN_POINT ( 'NONE',  ( 42.48921356237308800, -27.52281430457085065, 5.000000000000000000 ) ) ;
#110369 = FACE_OUTER_BOUND ( 'NONE', #52384, .T. ) ;
#110371 = AXIS2_PLACEMENT_3D ( 'NONE', #7363, #62499, #106673 ) ;
#110370 = PRODUCT_DEFINITION ( 'UNKNOWN', '', #118833, #42901 ) ;
#110372 = CARTESIAN_POINT ( 'NONE',  ( 61.18336038379622011, -2.130196079827426203, 7.949999999999997513 ) ) ;
#110373 = FACE_OUTER_BOUND ( 'NONE', #64415, .T. ) ;
#110374 = AXIS2_PLACEMENT_3D ( 'NONE', #128935, #139850, #6389 ) ;
#110375 = DIRECTION ( 'NONE',  ( -0.7071067811865486830, -0.7071067811865464625, 0.000000000000000000 ) ) ;
#110376 = ORIENTED_EDGE ( 'NONE', *, *, #24690, .F. ) ;
#110377 = ORIENTED_EDGE ( 'NONE', *, *, #48253, .T. ) ;
#110378 = CARTESIAN_POINT ( 'NONE',  ( 46.20833333333332149, -3.974999999999999201, -6.884901960086287964 ) ) ;
#110379 = CARTESIAN_POINT ( 'NONE',  ( 34.49999999999975842, -10.04351517176474751, -1.623559851933744191 ) ) ;
#110380 = VECTOR ( 'NONE', #6401, 1000.000000000000114 ) ;
#110382 = DIRECTION ( 'NONE',  ( -0.7071067811865487940, 0.7071067811865463515, -0.000000000000000000 ) ) ;
#110381 = VECTOR ( 'NONE', #16987, 1000.000000000000000 ) ;
#110383 = ORIENTED_EDGE ( 'NONE', *, *, #75422, .F. ) ;
#110384 = CARTESIAN_POINT ( 'NONE',  ( -1.285610022887904380, -0.3484131577337185037, 3.788408042242219054 ) ) ;
#110385 = EDGE_CURVE ( 'NONE', #1646, #111099, #84070, .T. ) ;
#110386 = DIRECTION ( 'NONE',  ( -0.3543493200069162685, -0.000000000000000000, -0.9351131265310288487 ) ) ;
#110387 = CARTESIAN_POINT ( 'NONE',  ( 34.12543019189810423, 5.291415217122919401, 3.055000000000002824 ) ) ;
#110388 = ORIENTED_EDGE ( 'NONE', *, *, #77637, .F. ) ;
#110389 = SURFACE_SIDE_STYLE ('',( #32887 ) ) ;
#110390 = VERTEX_POINT ( 'NONE', #49299 ) ;
#110391 = VERTEX_POINT ( 'NONE', #107203 ) ;
#110392 = DIRECTION ( 'NONE',  ( 0.7071067811865486830, -0.7071067811865464625, -0.000000000000000000 ) ) ;
#110393 = DIRECTION ( 'NONE',  ( 1.000000000000000000, 1.224606353822377258E-16, 0.000000000000000000 ) ) ;
#110394 = DIRECTION ( 'NONE',  ( 0.3543493200069162685, -0.000000000000000000, -0.9351131265310288487 ) ) ;
#110395 = DIRECTION ( 'NONE',  ( 1.000000000000000000, -0.000000000000000000, 0.000000000000000000 ) ) ;
#110396 = VERTEX_POINT ( 'NONE', #129664 ) ;
#110397 = LINE ( 'NONE', #51780, #99733 ) ;
#110399 = EDGE_LOOP ( 'NONE', ( #63674, #135639, #52261, #117161, #75746 ) ) ;
#110398 = DIRECTION ( 'NONE',  ( 0.000000000000000000, -1.000000000000000000, 0.000000000000000000 ) ) ;
#110400 = CARTESIAN_POINT ( 'NONE',  ( 82.97959685856476142, 6.109999999999999432, 1.637169565754164280 ) ) ;
#110401 = CARTESIAN_POINT ( 'NONE',  ( 127.1386022459138019, -7.776507174585692163E-16, 6.349999999999999645 ) ) ;
#110402 = CARTESIAN_POINT ( 'NONE',  ( -66.48921356237309510, -27.52281430457101763, 5.000000000000000000 ) ) ;
#110403 = CIRCLE ( 'NONE', #128946, 1.249999999999969802 ) ;
#110404 = DIRECTION ( 'NONE',  ( 0.6830127018922181881, 0.6830127018922202975, -0.2588190451025214056 ) ) ;
#110405 = FACE_OUTER_BOUND ( 'NONE', #79732, .T. ) ;
#110406 = EDGE_CURVE ( 'NONE', #121985, #93231, #52115, .T. ) ;
#110407 = ORIENTED_EDGE ( 'NONE', *, *, #83795, .F. ) ;
#110408 = AXIS2_PLACEMENT_3D ( 'NONE', #100363, #68475, #36524 ) ;
#110409 = DIRECTION ( 'NONE',  ( -0.7071067811865486830, -0.7071067811865464625, 0.000000000000000000 ) ) ;
#110410 = CARTESIAN_POINT ( 'NONE',  ( 68.30793019189809456, -6.109999999999998543, 1.637169565754158063 ) ) ;
#110411 = EDGE_CURVE ( 'NONE', #78193, #140787, #16618, .T. ) ;
#110412 = DIRECTION ( 'NONE',  ( -0.3543493200069162685, -0.000000000000000000, -0.9351131265310288487 ) ) ;
#110413 = LINE ( 'NONE', #66240, #33944 ) ;
#110414 = ORIENTED_EDGE ( 'NONE', *, *, #133552, .F. ) ;
#110415 = EDGE_LOOP ( 'NONE', ( #54834, #81030, #20809, #128638 ) ) ;
#110416 = LINE ( 'NONE', #141657, #137124 ) ;
#110417 = ORIENTED_EDGE ( 'NONE', *, *, #43165, .T. ) ;
#110418 = EDGE_CURVE ( 'NONE', #43072, #125864, #19484, .T. ) ;
#110419 = EDGE_CURVE ( 'NONE', #35082, #68842, #128265, .T. ) ;
#110420 = DIRECTION ( 'NONE',  ( -0.3543493200069162685, -0.000000000000000000, -0.9351131265310288487 ) ) ;
#110421 = VERTEX_POINT ( 'NONE', #28231 ) ;
#110422 = CARTESIAN_POINT ( 'NONE',  ( 0.8348608954644654023, -0.3999999999999997446, -2.317232259782045833 ) ) ;
#110423 = CARTESIAN_POINT ( 'NONE',  ( 10.49999999999992895, 0.4311230773921849169, 4.000000000000000000 ) ) ;
#110424 = VECTOR ( 'NONE', #119107, 1000.000000000000000 ) ;
#110425 = CARTESIAN_POINT ( 'NONE',  ( 0.000000000000000000, 0.000000000000000000, 5.000000000000000000 ) ) ;
#110426 = DIRECTION ( 'NONE',  ( 0.7071067811865486830, -0.7071067811865464625, -0.000000000000000000 ) ) ;
#110427 = EDGE_CURVE ( 'NONE', #33991, #99416, #116654, .T. ) ;
#110428 = FACE_BOUND ( 'NONE', #26385, .T. ) ;
#110429 = EDGE_CURVE ( 'NONE', #58244, #101765, #4995, .T. ) ;
#110430 = DIRECTION ( 'NONE',  ( 0.6830127018922180770, -0.6830127018922202975, -0.2588190451025213501 ) ) ;
#110431 = DIRECTION ( 'NONE',  ( 0.000000000000000000, -1.000000000000000000, 0.000000000000000000 ) ) ;
#110432 = CARTESIAN_POINT ( 'NONE',  ( 32.67183060077624646, 14.25929247661557397, 4.000000000000000000 ) ) ;
#110433 = DIRECTION ( 'NONE',  ( 1.000000000000000000, 0.000000000000000000, 0.000000000000000000 ) ) ;
#110435 = ORIENTED_EDGE ( 'NONE', *, *, #104754, .T. ) ;
#110434 = CARTESIAN_POINT ( 'NONE',  ( -6.330102185472606280, 17.25929247661554555, 19.83885114516072790 ) ) ;
#110436 = DIRECTION ( 'NONE',  ( -0.7071067811865486830, -0.7071067811865464625, 0.000000000000000000 ) ) ;
#110437 = EDGE_CURVE ( 'NONE', #42984, #29429, #6410, .T. ) ;
#110438 = EDGE_LOOP ( 'NONE', ( #58849, #94436, #22377, #116007 ) ) ;
#110439 = ORIENTED_EDGE ( 'NONE', *, *, #22890, .T. ) ;
#110440 = CARTESIAN_POINT ( 'NONE',  ( 73.84959685856479439, 6.109999999999996767, 1.637169565754163836 ) ) ;
#110441 = VERTEX_POINT ( 'NONE', #93486 ) ;
#110442 = DIRECTION ( 'NONE',  ( -0.6830127018922180770, -0.6830127018922204085, -0.2588190451025213501 ) ) ;
#110443 = VERTEX_POINT ( 'NONE', #96297 ) ;
#110444 = DIRECTION ( 'NONE',  ( -0.7071067811865486830, -0.7071067811865464625, -0.000000000000000000 ) ) ;
#110445 = EDGE_CURVE ( 'NONE', #32743, #88536, #38395, .T. ) ;
#110446 = CARTESIAN_POINT ( 'NONE',  ( 123.5000000000000000, 0.000000000000000000, -7.950000000000000178 ) ) ;
#110447 = CARTESIAN_POINT ( 'NONE',  ( -34.17183060077623225, 21.75929247661550292, 4.000000000000000000 ) ) ;
#110448 = DIRECTION ( 'NONE',  ( -0.7071067811865486830, 0.7071067811865464625, 0.000000000000000000 ) ) ;
#110449 = FACE_OUTER_BOUND ( 'NONE', #119226, .T. ) ;
#110450 = DIRECTION ( 'NONE',  ( 0.6830127018922180770, -0.6830127018922204085, -0.2588190451025213501 ) ) ;
#110451 = CARTESIAN_POINT ( 'NONE',  ( 20.99999999999985434, -6.412538124160692909, 4.000000000000000000 ) ) ;
#110452 = DIRECTION ( 'NONE',  ( -0.7071067811865486830, -0.7071067811865464625, 0.000000000000000000 ) ) ;
#110453 = VERTEX_POINT ( 'NONE', #39105 ) ;
#110454 = EDGE_CURVE ( 'NONE', #40966, #92630, #18750, .T. ) ;
#110455 = CARTESIAN_POINT ( 'NONE',  ( 8.031592354503320763, -3.851859888774471706E-31, 2.500000000000001332 ) ) ;
#110456 = VERTEX_POINT ( 'NONE', #18017 ) ;
#110457 = CARTESIAN_POINT ( 'NONE',  ( 0.000000000000000000, 0.000000000000000000, 5.000000000000000000 ) ) ;
#110458 = CARTESIAN_POINT ( 'NONE',  ( 16.27785539607886633, -2.500000000000000000, 3.061616997868383634E-16 ) ) ;
#110459 = ORIENTED_EDGE ( 'NONE', *, *, #62026, .T. ) ;
#110461 = ORIENTED_EDGE ( 'NONE', *, *, #120572, .T. ) ;
#110460 = VECTOR ( 'NONE', #132594, 999.9999999999998863 ) ;
#110462 = CARTESIAN_POINT ( 'NONE',  ( 30.04209685856476497, 5.291415217122923842, -3.054999999999996163 ) ) ;
#110463 = VERTEX_POINT ( 'NONE', #51419 ) ;
#110464 = DIRECTION ( 'NONE',  ( -0.7071067811865486830, -0.7071067811865464625, 0.000000000000000000 ) ) ;
#110465 = VECTOR ( 'NONE', #8246, 1000.000000000000000 ) ;
#110466 = VECTOR ( 'NONE', #86212, 1000.000000000000000 ) ;
#110467 = ADVANCED_FACE ( 'NONE', ( #27487 ), #50694, .F. ) ;
#110468 = CARTESIAN_POINT ( 'NONE',  ( 11.52487387214947212, 14.25929247661557575, 9.797011795316663552 ) ) ;
#110469 = VECTOR ( 'NONE', #73353, 1000.000000000000000 ) ;
#110470 = CARTESIAN_POINT ( 'NONE',  ( 21.33747294953710849, 6.094999999999989981, -1.119633336120465690E-15 ) ) ;
#110471 = CARTESIAN_POINT ( 'NONE',  ( 15.69968023028021520, 7.023557150533521920, -28.49217588184342986 ) ) ;
#110472 = VERTEX_POINT ( 'NONE', #40544 ) ;
#110473 = PLANE ( 'NONE',  #38819 ) ;
#110474 = ORIENTED_EDGE ( 'NONE', *, *, #84570, .T. ) ;
#110475 = LINE ( 'NONE', #53248, #44156 ) ;
#110476 = VECTOR ( 'NONE', #130240, 1000.000000000000000 ) ;
#110477 = FACE_OUTER_BOUND ( 'NONE', #137425, .T. ) ;
#110479 = ORIENTED_EDGE ( 'NONE', *, *, #26066, .F. ) ;
#110478 = PLANE ( 'NONE',  #63340 ) ;
#110480 = ORIENTED_EDGE ( 'NONE', *, *, #57566, .T. ) ;
#110481 = CARTESIAN_POINT ( 'NONE',  ( 30.75000000000000000, -9.735942053221458872E-16, 7.950000000000000178 ) ) ;
#110482 = CARTESIAN_POINT ( 'NONE',  ( 13.49999999999990763, 6.431123077392117082, 4.000000000000000000 ) ) ;
#110483 = PLANE ( 'NONE',  #37879 ) ;
#110484 = VERTEX_POINT ( 'NONE', #137720 ) ;
#110485 = FACE_OUTER_BOUND ( 'NONE', #10293, .T. ) ;
#110486 = VERTEX_POINT ( 'NONE', #139145 ) ;
#110487 = EDGE_CURVE ( 'NONE', #121754, #112625, #22452, .T. ) ;
#110488 = DIRECTION ( 'NONE',  ( -0.3543493200069163240, 0.000000000000000000, 0.9351131265310288487 ) ) ;
#110489 = DIRECTION ( 'NONE',  ( -0.7071067811865486830, -0.7071067811865464625, 0.000000000000000000 ) ) ;
#110490 = LINE ( 'NONE', #11161, #110984 ) ;
#110491 = SURFACE_STYLE_FILL_AREA ( #66322 ) ;
#110492 = CARTESIAN_POINT ( 'NONE',  ( 11.62000000000000099, 2.055000000000001492, 2.516649172247811554E-16 ) ) ;
#110493 = LINE ( 'NONE', #64896, #137417 ) ;
#110494 = CARTESIAN_POINT ( 'NONE',  ( 7.499999999999954703, -2.173586137069128732, -4.605770156576094898 ) ) ;
#110496 = EDGE_CURVE ( 'NONE', #132460, #41454, #20175, .T. ) ;
#110495 = VERTEX_POINT ( 'NONE', #54993 ) ;
#110497 = CARTESIAN_POINT ( 'NONE',  ( -23.51078643762690490, -27.52281430457038880, 5.000000000000000000 ) ) ;
#110498 = ORIENTED_EDGE ( 'NONE', *, *, #51399, .T. ) ;
#110499 = AXIS2_PLACEMENT_3D ( 'NONE', #111347, #109929, #10597 ) ;
#110500 = CARTESIAN_POINT ( 'NONE',  ( 25.89892480454907542, 0.000000000000000000, -6.350000000000003197 ) ) ;
#110501 = PRESENTATION_STYLE_ASSIGNMENT (( #66336 ) ) ;
#110502 = DIRECTION ( 'NONE',  ( 1.248002500702738701E-15, 1.000000000000000000, -0.000000000000000000 ) ) ;
#110503 = VECTOR ( 'NONE', #59392, 1000.000000000000000 ) ;
#110504 = EDGE_LOOP ( 'NONE', ( #110686, #124564, #15193, #17880 ) ) ;
#110505 = DIRECTION ( 'NONE',  ( 1.000000000000000000, 0.000000000000000000, 0.000000000000000000 ) ) ;
#110506 = CARTESIAN_POINT ( 'NONE',  ( -35.38161509397982485, -2.240707523384264377, 13.37739548510247189 ) ) ;
#110507 = DIRECTION ( 'NONE',  ( 0.7071067811865486830, -0.7071067811865464625, -0.000000000000000000 ) ) ;
#110508 = ORIENTED_EDGE ( 'NONE', *, *, #85138, .T. ) ;
#110509 = LINE ( 'NONE', #77926, #108931 ) ;
#110510 = CARTESIAN_POINT ( 'NONE',  ( 112.7083333333333286, -3.974999999999999201, -6.884901960086287964 ) ) ;
#110511 = DIRECTION ( 'NONE',  ( 0.000000000000000000, -1.000000000000000000, 0.000000000000000000 ) ) ;
#110512 = CIRCLE ( 'NONE', #59658, 2.500000000000000888 ) ;
#110513 = CARTESIAN_POINT ( 'NONE',  ( 53.35416666666665719, -2.130196079827501698, -7.949999999999956657 ) ) ;
#110514 = DIRECTION ( 'NONE',  ( -0.6830127018922180770, -0.6830127018922204085, -0.2588190451025213501 ) ) ;
#110515 = CARTESIAN_POINT ( 'NONE',  ( 68.16209685856478018, -5.291415217122919401, 3.054999999999998384 ) ) ;
#110516 =( BOUNDED_CURVE ( )  B_SPLINE_CURVE ( 3, ( #90717, #12407, #100854, #45793 ),
 .UNSPECIFIED., .F., .F. ) 
 B_SPLINE_CURVE_WITH_KNOTS ( ( 4, 4 ),
 ( 2.001653308786158991, 3.503810798801450854 ),
 .UNSPECIFIED. ) 
 CURVE ( )  GEOMETRIC_REPRESENTATION_ITEM ( )  RATIONAL_B_SPLINE_CURVE ( ( 1.000000000000000000, 0.8206354192515217250, 0.8206354192515217250, 1.000000000000000000 ) ) 
 REPRESENTATION_ITEM ( '' )  );
#110517 = CARTESIAN_POINT ( 'NONE',  ( 15.18398860626900237, 28.73617430169797871, 5.000000000000000000 ) ) ;
#110518 = CARTESIAN_POINT ( 'NONE',  ( 51.18398860626899705, 28.73617430169823095, 5.000000000000000000 ) ) ;
#110519 = CARTESIAN_POINT ( 'NONE',  ( -8.999999999999934275, -0.03360074219773377668, 5.000000000000000000 ) ) ;
#110520 = LINE ( 'NONE', #89509, #53435 ) ;
#110521 = EDGE_CURVE ( 'NONE', #142459, #95449, #58536, .T. ) ;
#110522 = EDGE_LOOP ( 'NONE', ( #32010, #96988, #42292, #33448, #131198, #4140 ) ) ;
#110523 = CARTESIAN_POINT ( 'NONE',  ( 18.32816939922340183, -9.740707523384180888, 4.000000000000000000 ) ) ;
#110524 = VECTOR ( 'NONE', #129820, 1000.000000000000000 ) ;
#110525 = VERTEX_POINT ( 'NONE', #141255 ) ;
#110526 = CARTESIAN_POINT ( 'NONE',  ( 128.0531643868628464, -51.20434817233914515, 36.87500513592859619 ) ) ;
#110527 = DIRECTION ( 'NONE',  ( -0.7071067811865486830, -0.7071067811865464625, 0.000000000000000000 ) ) ;
#110528 = LINE ( 'NONE', #11941, #71612 ) ;
#110529 = CARTESIAN_POINT ( 'NONE',  ( -25.39999999999996305, 0.000000000000000000, 2.500000000000000000 ) ) ;
#110530 = ADVANCED_FACE ( 'NONE', ( #98476 ), #64417, .F. ) ;
#110531 = LINE ( 'NONE', #33743, #46446 ) ;
#110532 = LINE ( 'NONE', #134469, #47721 ) ;
#110533 = ORIENTED_EDGE ( 'NONE', *, *, #22940, .F. ) ;
#110534 = ADVANCED_FACE ( 'NONE', ( #130411 ), #108596, .F. ) ;
#110535 = ORIENTED_EDGE ( 'NONE', *, *, #71162, .F. ) ;
#110536 = DIRECTION ( 'NONE',  ( 0.000000000000000000, 0.000000000000000000, -1.000000000000000000 ) ) ;
#110537 = CARTESIAN_POINT ( 'NONE',  ( 34.92499999999998295, -17.24070752338409562, 4.255531930566155197 ) ) ;
#110538 = DIRECTION ( 'NONE',  ( -0.7071067811865486830, -0.7071067811865464625, 0.000000000000000000 ) ) ;
#110539 = CYLINDRICAL_SURFACE ( 'NONE', #17920, 0.5000000000000004441 ) ;
#110540 = CARTESIAN_POINT ( 'NONE',  ( 81.89169371712955581, 2.130196079827421762, 7.950000000000001066 ) ) ;
#110541 = CARTESIAN_POINT ( 'NONE',  ( 7.637717201596474048, 0.000000000000000000, 2.500000000000000444 ) ) ;
#110542 = CARTESIAN_POINT ( 'NONE',  ( 20.81601139373100295, 28.73617430169773002, 5.000000000000000000 ) ) ;
#110543 = ORIENTED_EDGE ( 'NONE', *, *, #73633, .T. ) ;
#110544 = AXIS2_PLACEMENT_3D ( 'NONE', #94932, #118096, #63073 ) ;
#110545 = CARTESIAN_POINT ( 'NONE',  ( 69.68750000000000000, -5.819803920172573086, 5.819803920172572198 ) ) ;
#110546 = EDGE_CURVE ( 'NONE', #137862, #104351, #32520, .T. ) ;
#110547 = CARTESIAN_POINT ( 'NONE',  ( -27.72281430457040940, -21.72500000000000142, 5.000000000000000000 ) ) ;
#110548 = CARTESIAN_POINT ( 'NONE',  ( 7.014532492589830248, 3.061616997868383634E-16, -2.500000000000000444 ) ) ;
#110549 = CARTESIAN_POINT ( 'NONE',  ( -54.48921356237310221, -27.52281430457093236, 5.000000000000000000 ) ) ;
#110550 = ORIENTED_EDGE ( 'NONE', *, *, #124422, .T. ) ;
#110551 = EDGE_CURVE ( 'NONE', #129451, #96735, #97002, .T. ) ;
#110552 = DIRECTION ( 'NONE',  ( -1.000000000000000000, -0.000000000000000000, -0.000000000000000000 ) ) ;
#110553 = ORIENTED_EDGE ( 'NONE', *, *, #37793, .T. ) ;
#110554 = DIRECTION ( 'NONE',  ( -0.3543493200069162685, -0.000000000000000000, -0.9351131265310288487 ) ) ;
#110555 = CARTESIAN_POINT ( 'NONE',  ( 77.72959685856477563, -6.110000000000000320, -1.637169565754161393 ) ) ;
#110556 = FACE_OUTER_BOUND ( 'NONE', #100858, .T. ) ;
#110557 = ORIENTED_EDGE ( 'NONE', *, *, #109785, .T. ) ;
#110558 = PLANE ( 'NONE',  #16431 ) ;
#110559 = CIRCLE ( 'NONE', #24893, 6.000000000000000000 ) ;
#110560 = DIRECTION ( 'NONE',  ( -0.000000000000000000, 0.000000000000000000, 1.000000000000000000 ) ) ;
#110561 = FILL_AREA_STYLE_COLOUR ( '', #37428 ) ;
#110562 = AXIS2_PLACEMENT_3D ( 'NONE', #114192, #89583, #101892 ) ;
#110563 = LINE ( 'NONE', #66391, #136564 ) ;
#110564 = LINE ( 'NONE', #44672, #101817 ) ;
#110566 = ORIENTED_EDGE ( 'NONE', *, *, #59959, .T. ) ;
#110565 = LINE ( 'NONE', #21452, #1272 ) ;
#110567 = DIRECTION ( 'NONE',  ( -0.6830127018922181881, 0.6830127018922202975, -0.2588190451025214056 ) ) ;
#110568 = LINE ( 'NONE', #33779, #98590 ) ;
#110569 = CARTESIAN_POINT ( 'NONE',  ( 76.83333333333334281, -6.884901960086287964, 3.974999999999998312 ) ) ;
#110570 = CIRCLE ( 'NONE', #71200, 2.055000000000001048 ) ;
#110571 = CARTESIAN_POINT ( 'NONE',  ( 17.22560490425083657, 4.333342374871280669E-31, 2.500000000000000444 ) ) ;
#110572 = VECTOR ( 'NONE', #25576, 1000.000000000000000 ) ;
#110573 = ORIENTED_EDGE ( 'NONE', *, *, #12983, .T. ) ;
#110574 = ORIENTED_EDGE ( 'NONE', *, *, #68377, .T. ) ;
#110575 = CARTESIAN_POINT ( 'NONE',  ( 62.12543019189810423, 5.291415217122919401, 3.055000000000002824 ) ) ;
#110576 = ADVANCED_FACE ( 'NONE', ( #33955 ), #38473, .T. ) ;
#110577 = ORIENTED_EDGE ( 'NONE', *, *, #55450, .F. ) ;
#110578 = DIRECTION ( 'NONE',  ( -0.000000000000000000, 0.3543493200069153248, 0.9351131265310292928 ) ) ;
#110579 = EDGE_CURVE ( 'NONE', #120738, #95284, #77472, .T. ) ;
#110580 = CARTESIAN_POINT ( 'NONE',  ( 4.499999999999966249, 16.77039438581780217, 0.4657186855307644535 ) ) ;
#110581 = DIRECTION ( 'NONE',  ( 0.000000000000000000, -1.000000000000000000, 0.000000000000000000 ) ) ;
#110582 = CARTESIAN_POINT ( 'NONE',  ( 124.6208603837962272, -6.884901960086286188, 3.974999999999997424 ) ) ;
#110583 = CARTESIAN_POINT ( 'NONE',  ( 12.08314806772922978, 21.75929247661549937, 7.311836541448077931 ) ) ;
#110584 = ORIENTED_EDGE ( 'NONE', *, *, #130304, .T. ) ;
#110585 = ORIENTED_EDGE ( 'NONE', *, *, #22718, .T. ) ;
#110586 = PLANE ( 'NONE',  #44658 ) ;
#110587 = EDGE_CURVE ( 'NONE', #94901, #97018, #142009, .T. ) ;
#110588 = ADVANCED_FACE ( 'NONE', ( #76013 ), #31798, .F. ) ;
#110589 = VERTEX_POINT ( 'NONE', #43392 ) ;
#110590 = DIRECTION ( 'NONE',  ( -0.7071067811865486830, -0.7071067811865464625, 0.000000000000000000 ) ) ;
#110591 = LINE ( 'NONE', #12003, #68819 ) ;
#110592 = CARTESIAN_POINT ( 'NONE',  ( 24.75720643176650171, 22.22500000000000142, 27.61581905502973555 ) ) ;
#110593 = VERTEX_POINT ( 'NONE', #131830 ) ;
#110594 = EDGE_CURVE ( 'NONE', #93815, #764, #76755, .T. ) ;
#110595 = FACE_BOUND ( 'NONE', #55856, .T. ) ;
#110596 = EDGE_CURVE ( 'NONE', #46122, #73650, #66325, .T. ) ;
#110597 = CARTESIAN_POINT ( 'NONE',  ( -66.29974487139159578, -27.71228299555252406, 4.000000000000000000 ) ) ;
#110598 = DIRECTION ( 'NONE',  ( 0.000000000000000000, 1.000000000000000000, 0.000000000000000000 ) ) ;
#110599 = CARTESIAN_POINT ( 'NONE',  ( 24.87999999999999901, -2.055000000000000160, 2.789133085058098087E-16 ) ) ;
#110600 = AXIS2_PLACEMENT_3D ( 'NONE', #41290, #52865, #73238 ) ;
#110601 = CARTESIAN_POINT ( 'NONE',  ( 0.4000000000000001887, 0.000000000000000000, 0.000000000000000000 ) ) ;
#110602 = SURFACE_STYLE_FILL_AREA ( #66433 ) ;
#110603 = DIRECTION ( 'NONE',  ( 0.000000000000000000, 0.000000000000000000, 1.000000000000000000 ) ) ;
#110604 = ORIENTED_EDGE ( 'NONE', *, *, #102721, .T. ) ;
#110605 = EDGE_LOOP ( 'NONE', ( #28996, #132182, #138317, #129616 ) ) ;
#110606 = CARTESIAN_POINT ( 'NONE',  ( 98.93293019189810877, 1.637169565754156508, 6.110000000000000320 ) ) ;
#110607 = VERTEX_POINT ( 'NONE', #22308 ) ;
#110608 = ADVANCED_FACE ( 'NONE', ( #11431 ), #55709, .T. ) ;
#110609 = ORIENTED_EDGE ( 'NONE', *, *, #130594, .F. ) ;
#110610 = DIRECTION ( 'NONE',  ( -0.7071067811865486830, -0.7071067811865464625, 0.000000000000000000 ) ) ;
#110611 = EDGE_CURVE ( 'NONE', #29818, #41501, #123825, .T. ) ;
#110612 = LINE ( 'NONE', #99031, #128793 ) ;
#110613 = DIRECTION ( 'NONE',  ( 0.000000000000000000, -1.000000000000000000, -2.242629915582281933E-16 ) ) ;
#110614 = ORIENTED_EDGE ( 'NONE', *, *, #29899, .T. ) ;
#110615 = LINE ( 'NONE', #23635, #41440 ) ;
#110616 = CARTESIAN_POINT ( 'NONE',  ( 39.18398860626899705, 28.73617430169814568, 5.000000000000000000 ) ) ;
#110617 = FACE_BOUND ( 'NONE', #96240, .T. ) ;
#110619 = CARTESIAN_POINT ( 'NONE',  ( -45.29974487139158867, -27.71228299555237840, 4.000000000000000000 ) ) ;
#110618 = DIRECTION ( 'NONE',  ( -0.7071067811865486830, -0.7071067811865464625, 0.000000000000000000 ) ) ;
#110620 = DIRECTION ( 'NONE',  ( 0.7071067811865486830, -0.7071067811865464625, -0.000000000000000000 ) ) ;
#110621 = EDGE_CURVE ( 'NONE', #13795, #27559, #113626, .T. ) ;
#110622 = CARTESIAN_POINT ( 'NONE',  ( 0.1731953514540064132, 1.320799999999990648, 4.000000000000000000 ) ) ;
#110623 = ORIENTED_EDGE ( 'NONE', *, *, #102274, .F. ) ;
#110624 = CARTESIAN_POINT ( 'NONE',  ( 87.91666666666667140, -6.884901960086287076, -3.975000000000000977 ) ) ;
#110625 = FACE_OUTER_BOUND ( 'NONE', #127041, .T. ) ;
#110626 = ORIENTED_EDGE ( 'NONE', *, *, #88359, .T. ) ;
#110627 = ORIENTED_EDGE ( 'NONE', *, *, #50976, .F. ) ;
#110628 = ORIENTED_EDGE ( 'NONE', *, *, #50992, .F. ) ;
#110629 = CARTESIAN_POINT ( 'NONE',  ( 56.58376352523143993, -6.110000000000001208, -3.741295971395164515E-16 ) ) ;
#110630 = EDGE_CURVE ( 'NONE', #52088, #68553, #135420, .T. ) ;
#110631 = ORIENTED_EDGE ( 'NONE', *, *, #81799, .F. ) ;
#110632 = CARTESIAN_POINT ( 'NONE',  ( 1.499999999999994449, -7.420205493532897378, -2.617629953481250382 ) ) ;
#110633 = EDGE_CURVE ( 'NONE', #104452, #64492, #1281, .T. ) ;
#110634 = CARTESIAN_POINT ( 'NONE',  ( -1.412527050462894396, -6.094999999999989981, 3.732111120401553285E-16 ) ) ;
#110635 = MECHANICAL_DESIGN_GEOMETRIC_PRESENTATION_REPRESENTATION (  '', ( #115276 ), #136121 ) ;
#110636 = CARTESIAN_POINT ( 'NONE',  ( 91.58376352523144703, -6.110000000000001208, -3.741295971395164515E-16 ) ) ;
#110637 = DIRECTION ( 'NONE',  ( 0.7071067811865486830, -0.7071067811865464625, -0.000000000000000000 ) ) ;
#110638 = ORIENTED_EDGE ( 'NONE', *, *, #141244, .T. ) ;
#110639 = DIRECTION ( 'NONE',  ( -0.7071067811865487940, 0.7071067811865463515, 0.000000000000000000 ) ) ;
#110640 = EDGE_CURVE ( 'NONE', #13412, #58969, #68734, .T. ) ;
#110641 = DIRECTION ( 'NONE',  ( -0.6830127018922181881, 0.6830127018922202975, -0.2588190451025214056 ) ) ;
#110642 = CARTESIAN_POINT ( 'NONE',  ( -26.99999999999980815, -7.447814304570759880, 5.000000000000000000 ) ) ;
#110643 = CARTESIAN_POINT ( 'NONE',  ( 54.48921356237310221, -27.52281430457093236, 5.000000000000000000 ) ) ;
#110644 = EDGE_LOOP ( 'NONE', ( #85585, #75668, #27430, #69337 ) ) ;
#110645 = CARTESIAN_POINT ( 'NONE',  ( 0.000000000000000000, 9.735942053221458872E-16, -7.950000000000000178 ) ) ;
#110646 = VERTEX_POINT ( 'NONE', #101331 ) ;
#110647 = ORIENTED_EDGE ( 'NONE', *, *, #87003, .F. ) ;
#110648 = EDGE_LOOP ( 'NONE', ( #100292, #10131, #140830, #123606 ) ) ;
#110649 = CARTESIAN_POINT ( 'NONE',  ( 124.7454301918981230, -5.291415217122918513, -3.055000000000000160 ) ) ;
#110650 = LINE ( 'NONE', #55611, #9799 ) ;
#110651 = VECTOR ( 'NONE', #68423, 1000.000000000000000 ) ;
#110652 = CARTESIAN_POINT ( 'NONE',  ( 1.353980332882009030, 2.500000000000000888, 0.000000000000000000 ) ) ;
#110653 = ORIENTED_EDGE ( 'NONE', *, *, #119105, .F. ) ;
#110654 = DIRECTION ( 'NONE',  ( -1.000000000000000000, -1.224606353822377258E-16, -0.000000000000000000 ) ) ;
#110655 = CARTESIAN_POINT ( 'NONE',  ( -45.48921356237309510, -27.52281430457087197, 5.000000000000000000 ) ) ;
#110656 = ORIENTED_EDGE ( 'NONE', *, *, #81922, .T. ) ;
#110657 = VECTOR ( 'NONE', #93727, 1000.000000000000227 ) ;
#110659 = VECTOR ( 'NONE', #7318, 999.9999999999998863 ) ;
#110658 = VECTOR ( 'NONE', #32573, 1000.000000000000000 ) ;
#110660 = CARTESIAN_POINT ( 'NONE',  ( 15.87456980810188867, 6.871911579029510442, -3.967499999999998916 ) ) ;
#110661 = FACE_OUTER_BOUND ( 'NONE', #90888, .T. ) ;
#110662 = DIRECTION ( 'NONE',  ( 1.000000000000000000, 1.224606353822377258E-16, 0.000000000000000000 ) ) ;
#110663 =( BOUNDED_CURVE ( )  B_SPLINE_CURVE ( 3, ( #17397, #62360, #61654, #105810 ),
 .UNSPECIFIED., .F., .T. ) 
 B_SPLINE_CURVE_WITH_KNOTS ( ( 4, 4 ),
 ( 4.712388980384689674, 6.283185307179586232 ),
 .UNSPECIFIED. ) 
 CURVE ( )  GEOMETRIC_REPRESENTATION_ITEM ( )  RATIONAL_B_SPLINE_CURVE ( ( 1.000000000000000000, 0.8047378541243649375, 0.8047378541243649375, 1.000000000000000000 ) ) 
 REPRESENTATION_ITEM ( '' )  );
#110664 = DIRECTION ( 'NONE',  ( 0.000000000000000000, -1.000000000000000000, 0.000000000000000000 ) ) ;
#110665 = ORIENTED_EDGE ( 'NONE', *, *, #118015, .T. ) ;
#110666 = VERTEX_POINT ( 'NONE', #112921 ) ;
#110667 = EDGE_CURVE ( 'NONE', #52975, #40545, #48377, .T. ) ;
#110668 = ORIENTED_EDGE ( 'NONE', *, *, #14057, .T. ) ;
#110669 = CYLINDRICAL_SURFACE ( 'NONE', #129752, 3.999999999999996447 ) ;
#110670 = CARTESIAN_POINT ( 'NONE',  ( 57.43750000000000000, 5.819803920172574863, -5.819803920172573086 ) ) ;
#110671 = DIRECTION ( 'NONE',  ( -0.7071067811865487940, 0.7071067811865463515, 0.000000000000000000 ) ) ;
#110672 = DIRECTION ( 'NONE',  ( -0.7071067811865487940, 0.7071067811865463515, 0.000000000000000000 ) ) ;
#110673 = DIRECTION ( 'NONE',  ( 0.7071067811865486830, -0.7071067811865464625, -0.000000000000000000 ) ) ;
#110674 = LINE ( 'NONE', #133898, #87331 ) ;
#110675 = CARTESIAN_POINT ( 'NONE',  ( 7.014532492589830248, -2.499999999999999112, 0.000000000000000000 ) ) ;
#110676 = LINE ( 'NONE', #22951, #85894 ) ;
#110677 = ORIENTED_EDGE ( 'NONE', *, *, #140711, .T. ) ;
#110678 = FACE_OUTER_BOUND ( 'NONE', #85075, .T. ) ;
#110679 = ORIENTED_EDGE ( 'NONE', *, *, #17458, .F. ) ;
#110680 = VECTOR ( 'NONE', #82574, 1000.000000000000000 ) ;
#110681 = CARTESIAN_POINT ( 'NONE',  ( -7.940000000000001279, -60.26999999999998892, -11.89864999999999640 ) ) ;
#110682 = VERTEX_POINT ( 'NONE', #25916 ) ;
#110683 = VECTOR ( 'NONE', #135860, 999.9999999999998863 ) ;
#110684 = LINE ( 'NONE', #65104, #90010 ) ;
#110686 = ORIENTED_EDGE ( 'NONE', *, *, #62327, .F. ) ;
#110685 = FACE_OUTER_BOUND ( 'NONE', #141437, .T. ) ;
#110687 = EDGE_CURVE ( 'NONE', #131877, #17685, #136098, .T. ) ;
#110688 = CARTESIAN_POINT ( 'NONE',  ( 0.7928932188134528714, 6.759292476615656575, 5.000000000000000000 ) ) ;
#110689 = CARTESIAN_POINT ( 'NONE',  ( 25.49999999999982947, 8.319652575858409449, -8.582050562765768831 ) ) ;
#110690 = EDGE_LOOP ( 'NONE', ( #125345, #22195, #20448, #24573 ) ) ;
#110691 = EDGE_CURVE ( 'NONE', #536, #22939, #57865, .T. ) ;
#110692 = AXIS2_PLACEMENT_3D ( 'NONE', #1340, #34722, #101390 ) ;
#110693 = VERTEX_POINT ( 'NONE', #112225 ) ;
#110694 = CARTESIAN_POINT ( 'NONE',  ( 20.99999999999985434, -22.06887692260758982, 4.000000000000000000 ) ) ;
#110695 = ORIENTED_EDGE ( 'NONE', *, *, #57784, .F. ) ;
#110696 =( BOUNDED_CURVE ( )  B_SPLINE_CURVE ( 3, ( #15776, #112991, #49202, #71654 ),
 .UNSPECIFIED., .F., .F. ) 
 B_SPLINE_CURVE_WITH_KNOTS ( ( 4, 4 ),
 ( 1.610468072580459209, 1.654543780452488067 ),
 .UNSPECIFIED. ) 
 CURVE ( )  GEOMETRIC_REPRESENTATION_ITEM ( )  RATIONAL_B_SPLINE_CURVE ( ( 1.000000000000000000, 0.9998381175498711748, 0.9998381175498711748, 1.000000000000000000 ) ) 
 REPRESENTATION_ITEM ( '' )  );
#110697 = EDGE_CURVE ( 'NONE', #3334, #43398, #25186, .T. ) ;
#110698 = DIRECTION ( 'NONE',  ( -1.301042606982605074E-16, 1.000000000000000000, 0.000000000000000000 ) ) ;
#110699 = CARTESIAN_POINT ( 'NONE',  ( 114.5583603837962414, -7.949999999999997513, -2.130196079827425759 ) ) ;
#110700 = FILL_AREA_STYLE ('',( #98436 ) ) ;
#110701 = ADVANCED_FACE ( 'NONE', ( #81761 ), #69442, .F. ) ;
#110702 = DIRECTION ( 'NONE',  ( -0.5735764363510503783, -0.8191520442889886899, 0.000000000000000000 ) ) ;
#110703 = DIRECTION ( 'NONE',  ( 0.000000000000000000, -1.000000000000000000, 0.000000000000000000 ) ) ;
#110704 = DIRECTION ( 'NONE',  ( 0.7071067811865487940, 0.7071067811865463515, -0.000000000000000000 ) ) ;
#110705 = CARTESIAN_POINT ( 'NONE',  ( 18.08333333333333215, -5.278424836066144543, 3.047499999999995879 ) ) ;
#110706 = CARTESIAN_POINT ( 'NONE',  ( 17.47873647476855652, -5.808823158059033709, 5.808823158059035485 ) ) ;
#110707 = VECTOR ( 'NONE', #8287, 999.9999999999998863 ) ;
#110708 = DIRECTION ( 'NONE',  ( -1.000000000000000000, -0.000000000000000000, -0.000000000000000000 ) ) ;
#110709 = DIRECTION ( 'NONE',  ( 0.7071067811865487940, -0.7071067811865463515, 0.000000000000000000 ) ) ;
#110710 = VERTEX_POINT ( 'NONE', #2720 ) ;
#110712 = ORIENTED_EDGE ( 'NONE', *, *, #3980, .F. ) ;
#110711 = PRESENTATION_LAYER_ASSIGNMENT (  '', '', ( #62131 ) ) ;
#110713 = ADVANCED_FACE ( 'NONE', ( #34662 ), #136814, .T. ) ;
#110714 = LINE ( 'NONE', #109322, #134721 ) ;
#110715 = ORIENTED_EDGE ( 'NONE', *, *, #18606, .F. ) ;
#110716 = CARTESIAN_POINT ( 'NONE',  ( 103.9795968585647756, 6.109999999999999432, 1.637169565754164280 ) ) ;
#110717 = DIRECTION ( 'NONE',  ( -0.7071067811865486830, -0.7071067811865464625, 0.000000000000000000 ) ) ;
#110718 = CARTESIAN_POINT ( 'NONE',  ( -63.29974487139158867, -27.71228299555250274, 4.000000000000000000 ) ) ;
#110719 = PLANE ( 'NONE',  #123435 ) ;
#110720 = ORIENTED_EDGE ( 'NONE', *, *, #56680, .T. ) ;
#110721 = ADVANCED_FACE ( 'NONE', ( #47714 ), #125955, .F. ) ;
#110722 = PLANE ( 'NONE',  #91448 ) ;
#110723 = FACE_OUTER_BOUND ( 'NONE', #138342, .T. ) ;
#110724 = DIRECTION ( 'NONE',  ( -0.000000000000000000, -0.000000000000000000, 1.000000000000000000 ) ) ;
#110725 = LINE ( 'NONE', #95058, #9134 ) ;
#110726 = FILL_AREA_STYLE_COLOUR ( '', #98111 ) ;
#110728 = ORIENTED_EDGE ( 'NONE', *, *, #71745, .T. ) ;
#110727 = CARTESIAN_POINT ( 'NONE',  ( 17.81601139373099940, 28.73617430169775133, 5.000000000000000000 ) ) ;
#110729 =( NAMED_UNIT ( * ) SI_UNIT ( $, .STERADIAN. ) SOLID_ANGLE_UNIT ( ) );
#110730 = EDGE_CURVE ( 'NONE', #65560, #85199, #12172, .T. ) ;
#110731 = LINE ( 'NONE', #55695, #73174 ) ;
#110732 = LINE ( 'NONE', #31087, #63293 ) ;
#110733 = DIRECTION ( 'NONE',  ( 1.049727191138614875E-16, -0.5150380749100594846, 0.8571673007021091140 ) ) ;
#110734 = FACE_OUTER_BOUND ( 'NONE', #120127, .T. ) ;
#110735 = ORIENTED_EDGE ( 'NONE', *, *, #40111, .T. ) ;
#110736 = VERTEX_POINT ( 'NONE', #1966 ) ;
#110737 = VERTEX_POINT ( 'NONE', #45567 ) ;
#110738 = CARTESIAN_POINT ( 'NONE',  ( 92.75043019189810423, 3.055000000000002824, -5.291415217122919401 ) ) ;
#110739 = EDGE_LOOP ( 'NONE', ( #53934, #112367, #74606, #90675 ) ) ;
#110740 = DIRECTION ( 'NONE',  ( 0.6830127018922180770, -0.6830127018922204085, -0.2588190451025213501 ) ) ;
#110741 = EDGE_CURVE ( 'NONE', #131451, #118193, #91877, .T. ) ;
#110742 = LINE ( 'NONE', #68046, #43391 ) ;
#110743 = DIRECTION ( 'NONE',  ( 0.7071067811865486830, -0.7071067811865464625, -0.000000000000000000 ) ) ;
#110744 = DIRECTION ( 'NONE',  ( 0.000000000000000000, -1.000000000000000000, 0.000000000000000000 ) ) ;
#110745 = ORIENTED_EDGE ( 'NONE', *, *, #29808, .F. ) ;
#110746 = CARTESIAN_POINT ( 'NONE',  ( 8.999999999999936051, -19.22509904557635707, 1.855685503482199294 ) ) ;
#110747 = CARTESIAN_POINT ( 'NONE',  ( 39.18398860626899705, 28.73617430169814568, 5.000000000000000000 ) ) ;
#110748 = ADVANCED_FACE ( 'NONE', ( #79647 ), #36101, .F. ) ;
#110749 = ADVANCED_FACE ( 'NONE', ( #90464 ), #91209, .F. ) ;
#110750 = CARTESIAN_POINT ( 'NONE',  ( 89.45376352523146579, -6.109999999999998543, -3.741295971395162543E-16 ) ) ;
#110751 = EDGE_LOOP ( 'NONE', ( #40617, #84337, #124432, #33745 ) ) ;
#110752 = DIRECTION ( 'NONE',  ( -0.3543493200069162685, -0.000000000000000000, -0.9351131265310288487 ) ) ;
#110753 = DIRECTION ( 'NONE',  ( -0.000000000000000000, 0.000000000000000000, 1.000000000000000000 ) ) ;
#110754 = VECTOR ( 'NONE', #56492, 1000.000000000000000 ) ;
#110755 = VECTOR ( 'NONE', #47107, 1000.000000000000000 ) ;
#110756 = VECTOR ( 'NONE', #12377, 1000.000000000000000 ) ;
#110757 = EDGE_CURVE ( 'NONE', #109724, #73565, #139705, .T. ) ;
#110758 = ORIENTED_EDGE ( 'NONE', *, *, #81574, .T. ) ;
#110759 = ORIENTED_EDGE ( 'NONE', *, *, #4528, .F. ) ;
#110760 = AXIS2_PLACEMENT_3D ( 'NONE', #108442, #96855, #121491 ) ;
#110761 = ORIENTED_EDGE ( 'NONE', *, *, #10399, .T. ) ;
#110762 = CARTESIAN_POINT ( 'NONE',  ( -15.31657961132780166, -6.740707523384212863, 11.88629033278127878 ) ) ;
#110763 = EDGE_CURVE ( 'NONE', #23712, #70432, #140381, .T. ) ;
#110764 = VECTOR ( 'NONE', #24413, 999.9999999999998863 ) ;
#110765 = CARTESIAN_POINT ( 'NONE',  ( 17.29289321881333663, 11.25929247661560062, 5.000000000000000000 ) ) ;
#110766 = CARTESIAN_POINT ( 'NONE',  ( 34.92499999999998295, -21.72500000000000142, 5.000000000000000000 ) ) ;
#110767 = VECTOR ( 'NONE', #104699, 1000.000000000000000 ) ;
#110768 = LINE ( 'NONE', #98493, #73458 ) ;
#110769 = CARTESIAN_POINT ( 'NONE',  ( 12.85005128541016894, -8.240707523384193323, 17.25253755692241953 ) ) ;
#110770 = DIRECTION ( 'NONE',  ( 1.000000000000000000, -0.000000000000000000, 0.000000000000000000 ) ) ;
#110771 = SURFACE_STYLE_FILL_AREA ( #43412 ) ;
#110772 = ORIENTED_EDGE ( 'NONE', *, *, #131628, .F. ) ;
#110773 = EDGE_LOOP ( 'NONE', ( #75759, #69022, #20398, #1820 ) ) ;
#110774 = EDGE_CURVE ( 'NONE', #57808, #125073, #95441, .T. ) ;
#110775 = DIRECTION ( 'NONE',  ( -0.000000000000000000, -5.075120898959323014E-15, -1.000000000000000000 ) ) ;
#110776 = ORIENTED_EDGE ( 'NONE', *, *, #118092, .F. ) ;
#110777 = VERTEX_POINT ( 'NONE', #29468 ) ;
#110778 = VECTOR ( 'NONE', #138002, 1000.000000000000000 ) ;
#110779 = EDGE_CURVE ( 'NONE', #118230, #84933, #6250, .T. ) ;
#110780 = VECTOR ( 'NONE', #72105, 1000.000000000000000 ) ;
#110781 = DIRECTION ( 'NONE',  ( -0.000000000000000000, 0.000000000000000000, 1.000000000000000000 ) ) ;
#110782 = ORIENTED_EDGE ( 'NONE', *, *, #129977, .F. ) ;
#110783 = LINE ( 'NONE', #25223, #117683 ) ;
#110784 = LINE ( 'NONE', #80361, #30999 ) ;
#110785 = CARTESIAN_POINT ( 'NONE',  ( -3.183988606268992161, 28.73617430169789699, 5.000000000000000000 ) ) ;
#110786 = LINE ( 'NONE', #133310, #55441 ) ;
#110787 = AXIS2_PLACEMENT_3D ( 'NONE', #35388, #136085, #112905 ) ;
#110788 = PLANE ( 'NONE',  #88368 ) ;
#110789 = ORIENTED_EDGE ( 'NONE', *, *, #59601, .T. ) ;
#110790 = AXIS2_PLACEMENT_3D ( 'NONE', #35338, #79580, #68672 ) ;
#110791 = CARTESIAN_POINT ( 'NONE',  ( 29.67183060077626422, -18.74070752338408852, 4.000000000000000000 ) ) ;
#110792 = EDGE_LOOP ( 'NONE', ( #99377, #4048, #109797, #50097 ) ) ;
#110793 = LINE ( 'NONE', #23066, #64248 ) ;
#110794 = ORIENTED_EDGE ( 'NONE', *, *, #6760, .F. ) ;
#110795 = DIRECTION ( 'NONE',  ( -1.000000000000000000, -0.000000000000000000, -0.000000000000000000 ) ) ;
#110796 = ORIENTED_EDGE ( 'NONE', *, *, #26490, .T. ) ;
#110797 = CARTESIAN_POINT ( 'NONE',  ( 21.32816939922338051, 11.25929247661560240, 4.000000000000000000 ) ) ;
#110798 = ORIENTED_EDGE ( 'NONE', *, *, #110917, .F. ) ;
#110799 = VERTEX_POINT ( 'NONE', #72323 ) ;
#110800 = VECTOR ( 'NONE', #7839, 1000.000000000000227 ) ;
#110801 = VERTEX_POINT ( 'NONE', #60729 ) ;
#110802 = PLANE ( 'NONE',  #97440 ) ;
#110803 = FACE_OUTER_BOUND ( 'NONE', #95458, .T. ) ;
#110804 = DIRECTION ( 'NONE',  ( -0.6830127018922180770, -0.6830127018922204085, -0.2588190451025213501 ) ) ;
#110805 = CARTESIAN_POINT ( 'NONE',  ( 125.2712635252314328, 4.472830434245838482, 4.472830434245842035 ) ) ;
#110806 = CARTESIAN_POINT ( 'NONE',  ( 26.67183060077628198, 2.259292476615699652, 4.000000000000000000 ) ) ;
#110807 = CARTESIAN_POINT ( 'NONE',  ( 2.816011393730999401, 28.73617430169785436, 5.000000000000000000 ) ) ;
#110808 = PLANE ( 'NONE',  #121998 ) ;
#110809 = VECTOR ( 'NONE', #67784, 1000.000000000000114 ) ;
#110810 = DIRECTION ( 'NONE',  ( 1.000000000000000000, 1.224606353822377258E-16, 0.000000000000000000 ) ) ;
#110811 = DIRECTION ( 'NONE',  ( -0.7071067811865486830, -0.7071067811865464625, 0.000000000000000000 ) ) ;
#110812 = ORIENTED_EDGE ( 'NONE', *, *, #82825, .F. ) ;
#110813 = CARTESIAN_POINT ( 'NONE',  ( 25.19159235450331735, 9.902892378096218942E-16, 0.000000000000000000 ) ) ;
#110814 = DIRECTION ( 'NONE',  ( 1.000000000000000000, 0.000000000000000000, 0.000000000000000000 ) ) ;
#110815 = EDGE_LOOP ( 'NONE', ( #115390, #66714, #23418, #67620 ) ) ;
#110816 = VERTEX_POINT ( 'NONE', #104897 ) ;
#110817 = VERTEX_POINT ( 'NONE', #73028 ) ;
#110818 = DIRECTION ( 'NONE',  ( -0.5150380749100710309, 1.049727191138606123E-16, -0.8571673007021021196 ) ) ;
#110819 = ORIENTED_EDGE ( 'NONE', *, *, #39444, .T. ) ;
#110820 = ORIENTED_EDGE ( 'NONE', *, *, #88539, .F. ) ;
#110821 = FACE_OUTER_BOUND ( 'NONE', #129581, .T. ) ;
#110822 = DIRECTION ( 'NONE',  ( -0.6830127018922181881, 0.6830127018922202975, -0.2588190451025214056 ) ) ;
#110823 = LINE ( 'NONE', #40113, #82023 ) ;
#110824 = CARTESIAN_POINT ( 'NONE',  ( -6.183988606268994381, 28.73617430169791476, 5.000000000000000000 ) ) ;
#110825 = ORIENTED_EDGE ( 'NONE', *, *, #98008, .F. ) ;
#110826 = LINE ( 'NONE', #12256, #23275 ) ;
#110827 = EDGE_LOOP ( 'NONE', ( #137900, #13113, #49353, #14151 ) ) ;
#110828 = FACE_OUTER_BOUND ( 'NONE', #28031, .T. ) ;
#110829 = CARTESIAN_POINT ( 'NONE',  ( 17.42123647476855908, -9.717572351234235426E-16, -7.934999999999990727 ) ) ;
#110830 = ORIENTED_EDGE ( 'NONE', *, *, #26668, .T. ) ;
#110831 = CARTESIAN_POINT ( 'NONE',  ( 80.41209685856479439, 5.291415217122922066, -3.054999999999995275 ) ) ;
#110832 = CARTESIAN_POINT ( 'NONE',  ( 27.29974487139158512, -27.71228299555225405, 4.000000000000000000 ) ) ;
#110833 = CARTESIAN_POINT ( 'NONE',  ( 14.99999999999989697, 18.08204922493374411, 0.9627537363044524898 ) ) ;
#110834 = ORIENTED_EDGE ( 'NONE', *, *, #8486, .F. ) ;
#110835 = ORIENTED_EDGE ( 'NONE', *, *, #10399, .F. ) ;
#110836 = EDGE_CURVE ( 'NONE', #32567, #4325, #117179, .T. ) ;
#110837 = ORIENTED_EDGE ( 'NONE', *, *, #41876, .T. ) ;
#110838 = CARTESIAN_POINT ( 'NONE',  ( -33.18398860626899705, 28.73617430169810305, 5.000000000000000000 ) ) ;
#110839 = FACE_OUTER_BOUND ( 'NONE', #74916, .T. ) ;
#110840 = CARTESIAN_POINT ( 'NONE',  ( 156.1499999999997783, -57.14999999999999147, -34.92499999999975557 ) ) ;
#110841 = DIRECTION ( 'NONE',  ( -0.7071067811865487940, 0.7071067811865463515, -0.000000000000000000 ) ) ;
#110842 = CARTESIAN_POINT ( 'NONE',  ( -13.49999999999990763, -5.947814304570766986, 5.000000000000000000 ) ) ;
#110843 = ORIENTED_EDGE ( 'NONE', *, *, #91631, .T. ) ;
#110844 = CARTESIAN_POINT ( 'NONE',  ( -13.11547925347946908, 3.815643823912585386, 4.000000000000000000 ) ) ;
#110845 = CARTESIAN_POINT ( 'NONE',  ( 15.56584921360887108, 8.021612662230191759, 4.000000000000000000 ) ) ;
#110846 = CYLINDRICAL_SURFACE ( 'NONE', #63066, 6.350000000000004086 ) ;
#110847 = EDGE_CURVE ( 'NONE', #5368, #80916, #137545, .T. ) ;
#110848 = ORIENTED_EDGE ( 'NONE', *, *, #138569, .T. ) ;
#110849 = LINE ( 'NONE', #55822, #44335 ) ;
#110850 = VECTOR ( 'NONE', #141469, 1000.000000000000000 ) ;
#110851 = VECTOR ( 'NONE', #119197, 1000.000000000000000 ) ;
#110852 = AXIS2_PLACEMENT_3D ( 'NONE', #141756, #42458, #130885 ) ;
#110853 = MECHANICAL_DESIGN_GEOMETRIC_PRESENTATION_REPRESENTATION (  '', ( #92345 ), #85414 ) ;
#110854 = LINE ( 'NONE', #133377, #28509 ) ;
#110855 = ORIENTED_EDGE ( 'NONE', *, *, #34650, .T. ) ;
#110857 = ADVANCED_FACE ( 'NONE', ( #128788 ), #106287, .F. ) ;
#110856 = VECTOR ( 'NONE', #40584, 999.9999999999998863 ) ;
#110859 = ORIENTED_EDGE ( 'NONE', *, *, #77823, .F. ) ;
#110858 = CARTESIAN_POINT ( 'NONE',  ( -6.639999999999999680, -25.33999999999998920, 15.47043909406156281 ) ) ;
#110860 = VERTEX_POINT ( 'NONE', #84592 ) ;
#110861 = EDGE_CURVE ( 'NONE', #132460, #92286, #82449, .T. ) ;
#110862 = EDGE_CURVE ( 'NONE', #43034, #43627, #62849, .T. ) ;
#110863 = LINE ( 'NONE', #100742, #79522 ) ;
#110864 = CARTESIAN_POINT ( 'NONE',  ( -5.010880286539445727, -22.02621442084248216, 4.990779571109223767 ) ) ;
#110865 = ORIENTED_EDGE ( 'NONE', *, *, #77283, .F. ) ;
#110866 = LINE ( 'NONE', #35526, #113783 ) ;
#110867 =( GEOMETRIC_REPRESENTATION_CONTEXT ( 3 ) GLOBAL_UNCERTAINTY_ASSIGNED_CONTEXT ( ( #143330 ) ) GLOBAL_UNIT_ASSIGNED_CONTEXT ( ( #116059, #15293, #104468 ) ) REPRESENTATION_CONTEXT ( 'NONE', 'WORKASPACE' ) );
#110868 = ADVANCED_FACE ( 'NONE', ( #51251 ), #127360, .F. ) ;
#110869 = EDGE_CURVE ( 'NONE', #55041, #56871, #36204, .T. ) ;
#110870 = DIRECTION ( 'NONE',  ( -0.7071067811865487940, 0.7071067811865463515, 0.000000000000000000 ) ) ;
#110871 = DIRECTION ( 'NONE',  ( 0.7071067811865486830, -0.7071067811865464625, -0.000000000000000000 ) ) ;
#110872 = DIRECTION ( 'NONE',  ( 0.7071067811865487940, -0.7071067811865463515, 0.000000000000000000 ) ) ;
#110873 = FACE_OUTER_BOUND ( 'NONE', #98394, .T. ) ;
#110874 = EDGE_CURVE ( 'NONE', #66673, #63704, #128103, .T. ) ;
#110875 = DIRECTION ( 'NONE',  ( -0.6830127018922180770, -0.6830127018922204085, -0.2588190451025213501 ) ) ;
#110876 = DIRECTION ( 'NONE',  ( 0.7071067811865487940, 0.7071067811865463515, -0.000000000000000000 ) ) ;
#110877 = DIRECTION ( 'NONE',  ( 0.6830127018922181881, 0.6830127018922202975, -0.2588190451025214056 ) ) ;
#110878 = CARTESIAN_POINT ( 'NONE',  ( 18.20790314143522082, -6.871911579029513106, -3.967499999999993587 ) ) ;
#110880 = VECTOR ( 'NONE', #66694, 999.9999999999998863 ) ;
#110879 = DIRECTION ( 'NONE',  ( -0.7071067811865487940, 0.7071067811865463515, -0.000000000000000000 ) ) ;
#110881 = DIRECTION ( 'NONE',  ( -0.000000000000000000, 0.000000000000000000, 1.000000000000000000 ) ) ;
#110882 = CIRCLE ( 'NONE', #48406, 1.000000000000000000 ) ;
#110883 = FACE_OUTER_BOUND ( 'NONE', #141828, .T. ) ;
#110884 = DIRECTION ( 'NONE',  ( 0.6830127018922181881, 0.6830127018922202975, -0.2588190451025214056 ) ) ;
#110885 = VERTEX_POINT ( 'NONE', #28060 ) ;
#110886 = ORIENTED_EDGE ( 'NONE', *, *, #82722, .F. ) ;
#110888 = EDGE_CURVE ( 'NONE', #49530, #86149, #50525, .T. ) ;
#110887 = CARTESIAN_POINT ( 'NONE',  ( 100.3124999999999858, 5.819803920172571310, 5.819803920172575751 ) ) ;
#110889 = VECTOR ( 'NONE', #48726, 1000.000000000000000 ) ;
#110890 = VERTEX_POINT ( 'NONE', #49118 ) ;
#110891 = ORIENTED_EDGE ( 'NONE', *, *, #84447, .T. ) ;
#110892 = ORIENTED_EDGE ( 'NONE', *, *, #62092, .F. ) ;
#110893 = LINE ( 'NONE', #714, #8567 ) ;
#110894 = LINE ( 'NONE', #101469, #39325 ) ;
#110895 = ORIENTED_EDGE ( 'NONE', *, *, #10947, .T. ) ;
#110896 = VECTOR ( 'NONE', #16998, 999.9999999999998863 ) ;
#110897 = LINE ( 'NONE', #120334, #46396 ) ;
#110898 = VECTOR ( 'NONE', #109121, 1000.000000000000227 ) ;
#110899 = DIRECTION ( 'NONE',  ( 0.7071067811865487940, 0.7071067811865463515, -0.000000000000000000 ) ) ;
#110900 = AXIS2_PLACEMENT_3D ( 'NONE', #46942, #78100, #57078 ) ;
#110901 = CARTESIAN_POINT ( 'NONE',  ( -26.99999999999981526, 12.83542986846994793, -1.025386466790308315 ) ) ;
#110902 = CARTESIAN_POINT ( 'NONE',  ( -27.29974487139158512, -27.71228299555225405, 4.000000000000000000 ) ) ;
#110903 = ORIENTED_EDGE ( 'NONE', *, *, #94161, .F. ) ;
#110904 = CARTESIAN_POINT ( 'NONE',  ( 19.49999999999985789, -2.777013188829488666, 4.549262955118046570 ) ) ;
#110905 =( NAMED_UNIT ( * ) PLANE_ANGLE_UNIT ( ) SI_UNIT ( $, .RADIAN. ) );
#110906 = VECTOR ( 'NONE', #42498, 1000.000000000000000 ) ;
#110907 = EDGE_CURVE ( 'NONE', #100760, #111455, #93312, .T. ) ;
#110908 = DIRECTION ( 'NONE',  ( -1.000000000000000000, -0.000000000000000000, -0.000000000000000000 ) ) ;
#110909 = DIRECTION ( 'NONE',  ( 0.6830127018922180770, -0.6830127018922204085, -0.2588190451025213501 ) ) ;
#110910 = DIRECTION ( 'NONE',  ( 0.000000000000000000, 1.000000000000000000, 0.000000000000000000 ) ) ;
#110911 = CARTESIAN_POINT ( 'NONE',  ( 86.41252705046289861, -7.949999999999998401, -4.867971026610728450E-16 ) ) ;
#110912 = LINE ( 'NONE', #1439, #116294 ) ;
#110913 = EDGE_LOOP ( 'NONE', ( #135484, #125325, #106908, #18046 ) ) ;
#110914 = ORIENTED_EDGE ( 'NONE', *, *, #90288, .F. ) ;
#110915 = CARTESIAN_POINT ( 'NONE',  ( 117.5420968585647756, 5.291415217122923842, -3.054999999999996163 ) ) ;
#110916 = ORIENTED_EDGE ( 'NONE', *, *, #23536, .F. ) ;
#110917 = EDGE_CURVE ( 'NONE', #62936, #93695, #61445, .T. ) ;
#110918 = CARTESIAN_POINT ( 'NONE',  ( -23.99999999999984013, -13.97847968911262484, -0.1324546996127346499 ) ) ;
#110919 = COLOUR_RGB ( '', 0.09019608, 0.27058824, 0.51372549) ;
#110920 = PLANE ( 'NONE',  #87326 ) ;
#110921 = DIRECTION ( 'NONE',  ( -0.7071067811865487940, 0.7071067811865463515, 0.000000000000000000 ) ) ;
#110922 = FILL_AREA_STYLE_COLOUR ( '', #115926 ) ;
#110923 = ADVANCED_FACE ( 'NONE', ( #7709 ), #10801, .T. ) ;
#110924 = CARTESIAN_POINT ( 'NONE',  ( 112.7870968585647802, 3.054999999999997495, 5.291415217122919401 ) ) ;
#110925 = ORIENTED_EDGE ( 'NONE', *, *, #69926, .F. ) ;
#110926 = EDGE_CURVE ( 'NONE', #118674, #129502, #5567, .T. ) ;
#110927 = ORIENTED_EDGE ( 'NONE', *, *, #65099, .F. ) ;
#110928 = DIRECTION ( 'NONE',  ( 1.000000000000000000, 0.000000000000000000, 0.000000000000000000 ) ) ;
#110929 = DIRECTION ( 'NONE',  ( 0.6830127018922181881, 0.6830127018922202975, -0.2588190451025214056 ) ) ;
#110930 = EDGE_CURVE ( 'NONE', #24156, #42638, #54132, .T. ) ;
#110931 = ADVANCED_FACE ( 'NONE', ( #54822 ), #121478, .F. ) ;
#110932 = ORIENTED_EDGE ( 'NONE', *, *, #59045, .T. ) ;
#110933 = ORIENTED_EDGE ( 'NONE', *, *, #74113, .T. ) ;
#110934 = CARTESIAN_POINT ( 'NONE',  ( 35.14626352523143993, -4.472830434245840259, 4.472830434245839371 ) ) ;
#110935 = ORIENTED_EDGE ( 'NONE', *, *, #115950, .T. ) ;
#110936 = CARTESIAN_POINT ( 'NONE',  ( -75.18398860626899705, 28.73617430169839793, 5.000000000000000000 ) ) ;
#110937 = CARTESIAN_POINT ( 'NONE',  ( -32.99999999999977973, 4.965500833774297185, -4.007596771432582194 ) ) ;
#110938 = DIRECTION ( 'NONE',  ( 0.6830127018922181881, 0.6830127018922202975, -0.2588190451025214056 ) ) ;
#110939 = ADVANCED_FACE ( 'NONE', ( #87448 ), #82554, .T. ) ;
#110940 = CARTESIAN_POINT ( 'NONE',  ( 20.67183060077632462, -6.740707523384212863, 4.000000000000000000 ) ) ;
#110941 = ORIENTED_EDGE ( 'NONE', *, *, #110151, .F. ) ;
#110942 = EDGE_CURVE ( 'NONE', #26469, #87228, #99725, .T. ) ;
#110943 = DIRECTION ( 'NONE',  ( -1.000000000000000000, -0.000000000000000000, -0.000000000000000000 ) ) ;
#110944 = EDGE_LOOP ( 'NONE', ( #16325, #17595, #10705 ) ) ;
#110945 = VERTEX_POINT ( 'NONE', #397 ) ;
#110946 = ORIENTED_EDGE ( 'NONE', *, *, #20749, .T. ) ;
#110947 = FILL_AREA_STYLE ('',( #34874 ) ) ;
#110948 = LINE ( 'NONE', #69655, #18666 ) ;
#110949 = EDGE_CURVE ( 'NONE', #109570, #134004, #19320, .T. ) ;
#110950 = ORIENTED_EDGE ( 'NONE', *, *, #109132, .T. ) ;
#110951 = DIRECTION ( 'NONE',  ( -0.6830127018922180770, -0.6830127018922204085, -0.2588190451025213501 ) ) ;
#110952 = CARTESIAN_POINT ( 'NONE',  ( 0.000000000000000000, 0.000000000000000000, 5.000000000000000000 ) ) ;
#110953 = FACE_OUTER_BOUND ( 'NONE', #137000, .T. ) ;
#110954 = MECHANICAL_DESIGN_GEOMETRIC_PRESENTATION_REPRESENTATION (  '', ( #32250 ), #94719 ) ;
#110955 = VECTOR ( 'NONE', #47472, 1000.000000000000000 ) ;
#110956 = AXIS2_PLACEMENT_3D ( 'NONE', #66232, #33615, #99531 ) ;
#110957 =( BOUNDED_CURVE ( )  B_SPLINE_CURVE ( 3, ( #103634, #72511, #59477, #115206 ),
 .UNSPECIFIED., .F., .T. ) 
 B_SPLINE_CURVE_WITH_KNOTS ( ( 4, 4 ),
 ( 0.4286956587950772612, 0.5111536932531051125 ),
 .UNSPECIFIED. ) 
 CURVE ( )  GEOMETRIC_REPRESENTATION_ITEM ( )  RATIONAL_B_SPLINE_CURVE ( ( 1.000000000000000000, 0.9994334696367943582, 0.9994334696367943582, 1.000000000000000000 ) ) 
 REPRESENTATION_ITEM ( '' )  );
#110958 = DIRECTION ( 'NONE',  ( -0.7071067811865486830, -0.7071067811865464625, 0.000000000000000000 ) ) ;
#110959 = AXIS2_PLACEMENT_3D ( 'NONE', #17890, #86046, #41827 ) ;
#110960 = EDGE_CURVE ( 'NONE', #65337, #73728, #129492, .T. ) ;
#110961 = FACE_BOUND ( 'NONE', #45293, .T. ) ;
#110962 = VERTEX_POINT ( 'NONE', #11262 ) ;
#110963 = CARTESIAN_POINT ( 'NONE',  ( 12.69999999999999574, -40.43000000000000682, 19.06900128115122683 ) ) ;
#110964 = DIRECTION ( 'NONE',  ( 1.000000000000000000, 0.000000000000000000, 0.000000000000000000 ) ) ;
#110965 = LINE ( 'NONE', #45077, #25411 ) ;
#110966 = EDGE_CURVE ( 'NONE', #53919, #10232, #31633, .T. ) ;
#110967 = ORIENTED_EDGE ( 'NONE', *, *, #56181, .F. ) ;
#110968 = CARTESIAN_POINT ( 'NONE',  ( 4.911592354503321545, 2.500000000000001776, 0.000000000000000000 ) ) ;
#110969 = ORIENTED_EDGE ( 'NONE', *, *, #116123, .T. ) ;
#110970 = ORIENTED_EDGE ( 'NONE', *, *, #72717, .F. ) ;
#110971 = AXIS2_PLACEMENT_3D ( 'NONE', #32475, #20138, #9228 ) ;
#110972 = PRESENTATION_STYLE_ASSIGNMENT (( #99382 ) ) ;
#110973 = ORIENTED_EDGE ( 'NONE', *, *, #9915, .F. ) ;
#110974 = CARTESIAN_POINT ( 'NONE',  ( 47.16209685856477307, -5.291415217122919401, 3.054999999999997939 ) ) ;
#110975 = ORIENTED_EDGE ( 'NONE', *, *, #131576, .F. ) ;
#110976 = AXIS2_PLACEMENT_3D ( 'NONE', #114443, #136198, #91980 ) ;
#110977 = PLANE ( 'NONE',  #125088 ) ;
#110978 = CARTESIAN_POINT ( 'NONE',  ( 9.119999999999999218, 1.116877880822386018E-15, 10.00000000000000000 ) ) ;
#110979 = DIRECTION ( 'NONE',  ( 0.7071067811865487940, 0.7071067811865463515, 0.000000000000000000 ) ) ;
#110980 = ORIENTED_EDGE ( 'NONE', *, *, #86127, .F. ) ;
#110981 = PLANE ( 'NONE',  #69998 ) ;
#110982 = LINE ( 'NONE', #55946, #31984 ) ;
#110983 = AXIS2_PLACEMENT_3D ( 'NONE', #14968, #59939, #49065 ) ;
#110984 = VECTOR ( 'NONE', #98910, 1000.000000000000000 ) ;
#110985 = ADVANCED_FACE ( 'NONE', ( #30186 ), #80304, .T. ) ;
#110986 = AXIS2_PLACEMENT_3D ( 'NONE', #23762, #12854, #1949 ) ;
#110987 = EDGE_CURVE ( 'NONE', #109374, #2192, #53370, .T. ) ;
#110988 = PLANE ( 'NONE',  #20096 ) ;
#110989 = CARTESIAN_POINT ( 'NONE',  ( 5.700255128608413102, -27.71228299555201957, 4.000000000000000000 ) ) ;
#110990 = DIRECTION ( 'NONE',  ( -0.000000000000000000, -0.3543493200069152693, 0.9351131265310292928 ) ) ;
#110991 = DIRECTION ( 'NONE',  ( 0.3543493200069162685, -0.000000000000000000, -0.9351131265310288487 ) ) ;
#110992 = FILL_AREA_STYLE_COLOUR ( '', #14 ) ;
#110993 = EDGE_LOOP ( 'NONE', ( #50388, #12777, #74716 ) ) ;
#110994 = ORIENTED_EDGE ( 'NONE', *, *, #46020, .T. ) ;
#110995 = ORIENTED_EDGE ( 'NONE', *, *, #89621, .T. ) ;
#110996 = VECTOR ( 'NONE', #119670, 999.9999999999998863 ) ;
#110997 = CARTESIAN_POINT ( 'NONE',  ( 131.8806778009765708, -52.14999999999999147, 40.92499999999998295 ) ) ;
#110998 = ORIENTED_EDGE ( 'NONE', *, *, #19455, .F. ) ;
#110999 = VECTOR ( 'NONE', #50306, 1000.000000000000000 ) ;
#111000 = VECTOR ( 'NONE', #64198, 1000.000000000000000 ) ;
#111001 = ORIENTED_EDGE ( 'NONE', *, *, #127989, .T. ) ;
#111002 = DIRECTION ( 'NONE',  ( 0.7071067811865487940, -0.7071067811865463515, 0.000000000000000000 ) ) ;
#111003 = DIRECTION ( 'NONE',  ( -0.6830127018922180770, -0.6830127018922204085, -0.2588190451025213501 ) ) ;
#111004 = EDGE_CURVE ( 'NONE', #29906, #87047, #118620, .T. ) ;
#111005 = VECTOR ( 'NONE', #60500, 1000.000000000000227 ) ;
#111006 = DIRECTION ( 'NONE',  ( -0.000000000000000000, -0.3543493200069152693, 0.9351131265310292928 ) ) ;
#111007 = EDGE_LOOP ( 'NONE', ( #12650, #78415, #36092, #2117, #135137 ) ) ;
#111008 = AXIS2_PLACEMENT_3D ( 'NONE', #13208, #133602, #21960 ) ;
#111009 = LINE ( 'NONE', #142948, #136609 ) ;
#111010 = DIRECTION ( 'NONE',  ( -0.000000000000000000, -0.3543493200069152693, 0.9351131265310292928 ) ) ;
#111011 = CARTESIAN_POINT ( 'NONE',  ( 31.85873647476855552, 5.808823158059031044, -5.808823158059038150 ) ) ;
#111012 = PLANE ( 'NONE',  #131852 ) ;
#111013 = ORIENTED_EDGE ( 'NONE', *, *, #68554, .F. ) ;
#111014 = CARTESIAN_POINT ( 'NONE',  ( 109.8704301918981230, -3.055000000000001936, 5.291415217122918513 ) ) ;
#111015 = CARTESIAN_POINT ( 'NONE',  ( 29.99999999999979750, -19.22509904557633575, 1.855685503482247034 ) ) ;
#111016 = CARTESIAN_POINT ( 'NONE',  ( 9.489213562373095101, -27.52281430457062328, 5.000000000000000000 ) ) ;
#111017 = VECTOR ( 'NONE', #65200, 1000.000000000000227 ) ;
#111019 = ORIENTED_EDGE ( 'NONE', *, *, #3423, .F. ) ;
#111018 = DIRECTION ( 'NONE',  ( 0.000000000000000000, 0.000000000000000000, 1.000000000000000000 ) ) ;
#111020 = CARTESIAN_POINT ( 'NONE',  ( 29.20710678118634007, 3.759292476615678336, 5.000000000000000000 ) ) ;
#111021 = ORIENTED_EDGE ( 'NONE', *, *, #60367, .T. ) ;
#111022 = FILL_AREA_STYLE ('',( #123389 ) ) ;
#111023 = DIRECTION ( 'NONE',  ( 0.6830127018922181881, 0.6830127018922202975, -0.2588190451025214056 ) ) ;
#111024 = ORIENTED_EDGE ( 'NONE', *, *, #42239, .F. ) ;
#111025 = CARTESIAN_POINT ( 'NONE',  ( 1.771493228613341575, 20.25929247661551003, 7.808871592221773739 ) ) ;
#111026 = FACE_OUTER_BOUND ( 'NONE', #75270, .T. ) ;
#111027 = ORIENTED_EDGE ( 'NONE', *, *, #66758, .T. ) ;
#111028 = DIRECTION ( 'NONE',  ( -0.000000000000000000, -0.3543493200069152693, 0.9351131265310292928 ) ) ;
#111029 = ORIENTED_EDGE ( 'NONE', *, *, #19160, .T. ) ;
#111030 = DIRECTION ( 'NONE',  ( -0.7071067811865487940, 0.7071067811865463515, -0.000000000000000000 ) ) ;
#111032 = ORIENTED_EDGE ( 'NONE', *, *, #14963, .T. ) ;
#111031 = DIRECTION ( 'NONE',  ( 1.000000000000000000, 0.000000000000000000, 0.000000000000000000 ) ) ;
#111033 = EDGE_CURVE ( 'NONE', #20222, #20849, #42532, .T. ) ;
#111034 = VERTEX_POINT ( 'NONE', #20011 ) ;
#111035 = DIRECTION ( 'NONE',  ( -1.000000000000000000, -0.000000000000000000, -0.000000000000000000 ) ) ;
#111036 = CARTESIAN_POINT ( 'NONE',  ( 45.29974487139158867, -27.71228299555237840, 4.000000000000000000 ) ) ;
#111037 = VERTEX_POINT ( 'NONE', #141833 ) ;
#111038 = CARTESIAN_POINT ( 'NONE',  ( 6.299744871391586898, -27.71228299555210484, 4.000000000000000000 ) ) ;
#111039 = ADVANCED_FACE ( 'NONE', ( #86736 ), #130960, .F. ) ;
#111040 = EDGE_CURVE ( 'NONE', #89322, #128406, #133112, .T. ) ;
#111041 = DIRECTION ( 'NONE',  ( 0.6830127018922180770, -0.6830127018922204085, -0.2588190451025213501 ) ) ;
#111042 = DIRECTION ( 'NONE',  ( -0.7071067811865486830, 0.7071067811865464625, 0.000000000000000000 ) ) ;
#111043 = EDGE_CURVE ( 'NONE', #37138, #114295, #91706, .T. ) ;
#111044 = ORIENTED_EDGE ( 'NONE', *, *, #19864, .F. ) ;
#111045 = DIRECTION ( 'NONE',  ( -0.000000000000000000, 0.000000000000000000, 1.000000000000000000 ) ) ;
#111046 = EDGE_CURVE ( 'NONE', #42984, #70961, #124343, .T. ) ;
#111047 = DIRECTION ( 'NONE',  ( -0.000000000000000000, 0.000000000000000000, -1.000000000000000000 ) ) ;
#111048 = LINE ( 'NONE', #56752, #93306 ) ;
#111049 = DIRECTION ( 'NONE',  ( 0.7071067811865487940, 0.7071067811865463515, 0.000000000000000000 ) ) ;
#111050 = EDGE_CURVE ( 'NONE', #111882, #5092, #70981, .T. ) ;
#111051 = CARTESIAN_POINT ( 'NONE',  ( 127.8291937171295558, -3.975000000000001865, 6.884901960086284411 ) ) ;
#111052 = DIRECTION ( 'NONE',  ( 0.5735764363510453823, -0.8191520442889923537, 1.003171929053525486E-16 ) ) ;
#111053 = VERTEX_POINT ( 'NONE', #3934 ) ;
#111054 = ORIENTED_EDGE ( 'NONE', *, *, #72093, .F. ) ;
#111056 = EDGE_CURVE ( 'NONE', #7898, #75827, #63171, .T. ) ;
#111055 = CARTESIAN_POINT ( 'NONE',  ( 127.0000000000000000, 0.000000000000000000, -7.950000000000000178 ) ) ;
#111057 = EDGE_LOOP ( 'NONE', ( #89444, #12923, #120289, #53937 ) ) ;
#111058 = EDGE_LOOP ( 'NONE', ( #89115, #78056, #3644, #119219 ) ) ;
#111059 = CARTESIAN_POINT ( 'NONE',  ( 20.32505044418271467, 22.22500000000000142, 25.93630946864303866 ) ) ;
#111060 = DIRECTION ( 'NONE',  ( -1.000000000000000000, -1.224606353822377258E-16, -0.000000000000000000 ) ) ;
#111061 = VECTOR ( 'NONE', #77013, 1000.000000000000000 ) ;
#111062 = AXIS2_PLACEMENT_3D ( 'NONE', #88970, #12792, #135333 ) ;
#111063 = VECTOR ( 'NONE', #67403, 1000.000000000000000 ) ;
#111064 = VERTEX_POINT ( 'NONE', #112053 ) ;
#111065 = SURFACE_STYLE_FILL_AREA ( #22620 ) ;
#111066 = FACE_OUTER_BOUND ( 'NONE', #2193, .T. ) ;
#111067 = CIRCLE ( 'NONE', #87916, 2.500000000000000444 ) ;
#111068 = ADVANCED_FACE ( 'NONE', ( #135930 ), #68563, .F. ) ;
#111069 = DIRECTION ( 'NONE',  ( -0.6830127018922181881, 0.6830127018922202975, -0.2588190451025214056 ) ) ;
#111070 = DIRECTION ( 'NONE',  ( 0.7071067811865486830, -0.7071067811865464625, -0.000000000000000000 ) ) ;
#111071 = CARTESIAN_POINT ( 'NONE',  ( 122.5004301918981184, -3.055000000000002380, 5.291415217122920289 ) ) ;
#111072 = ORIENTED_EDGE ( 'NONE', *, *, #4720, .F. ) ;
#111073 = FACE_OUTER_BOUND ( 'NONE', #140244, .T. ) ;
#111074 = CARTESIAN_POINT ( 'NONE',  ( 44.75000000000000000, -9.735942053221458872E-16, 7.950000000000000178 ) ) ;
#111075 = DIRECTION ( 'NONE',  ( -0.000000000000000000, -0.3543493200069152693, 0.9351131265310292928 ) ) ;
#111076 = VECTOR ( 'NONE', #37479, 1000.000000000000000 ) ;
#111077 = DIRECTION ( 'NONE',  ( 0.000000000000000000, -1.000000000000000000, 0.000000000000000000 ) ) ;
#111078 = PLANE ( 'NONE',  #26553 ) ;
#111079 = EDGE_CURVE ( 'NONE', #18068, #139716, #112750, .T. ) ;
#111080 = DIRECTION ( 'NONE',  ( -0.7071067811865486830, -0.7071067811865464625, 0.000000000000000000 ) ) ;
#111081 = DIRECTION ( 'NONE',  ( -0.7071067811865487940, 0.7071067811865463515, 0.000000000000000000 ) ) ;
#111082 = CARTESIAN_POINT ( 'NONE',  ( 47.76669371712954870, -7.949999999999999289, 2.130196079827424427 ) ) ;
#111083 = DIRECTION ( 'NONE',  ( -0.000000000000000000, -0.3543493200069152693, 0.9351131265310292928 ) ) ;
#111084 = CARTESIAN_POINT ( 'NONE',  ( -3.005480084712505828, 28.92564299267936079, 4.000000000000000000 ) ) ;
#111085 = ORIENTED_EDGE ( 'NONE', *, *, #7640, .F. ) ;
#111086 = VERTEX_POINT ( 'NONE', #101153 ) ;
#111087 = CARTESIAN_POINT ( 'NONE',  ( 44.89583333333332149, -2.130196079827427091, 7.949999999999999289 ) ) ;
#111088 = DIRECTION ( 'NONE',  ( -0.000000000000000000, 0.000000000000000000, 1.000000000000000000 ) ) ;
#111089 = AXIS2_PLACEMENT_3D ( 'NONE', #40687, #76909, #75459 ) ;
#111090 = CARTESIAN_POINT ( 'NONE',  ( -21.72281430457044493, -21.72500000000000142, 5.000000000000000000 ) ) ;
#111091 = VERTEX_POINT ( 'NONE', #1798 ) ;
#111092 = CARTESIAN_POINT ( 'NONE',  ( -0.8736642903051350384, -0.9942593280178064763, 3.903919091990571300 ) ) ;
#111093 = CARTESIAN_POINT ( 'NONE',  ( 54.18398860626899705, 28.73617430169825226, 5.000000000000000000 ) ) ;
#111094 = VECTOR ( 'NONE', #53351, 999.9999999999998863 ) ;
#111095 = CARTESIAN_POINT ( 'NONE',  ( 37.18793019189810423, 6.110000000000002984, -1.637169565754156730 ) ) ;
#111096 = ORIENTED_EDGE ( 'NONE', *, *, #93949, .F. ) ;
#111097 = EDGE_CURVE ( 'NONE', #5504, #35419, #90273, .T. ) ;
#111098 = FACE_OUTER_BOUND ( 'NONE', #122856, .T. ) ;
#111099 = VERTEX_POINT ( 'NONE', #22850 ) ;
#111100 = ORIENTED_EDGE ( 'NONE', *, *, #86072, .T. ) ;
#111101 = DIRECTION ( 'NONE',  ( -0.3543493200069162685, -0.000000000000000000, -0.9351131265310288487 ) ) ;
#111102 = VECTOR ( 'NONE', #116636, 1000.000000000000227 ) ;
#111103 = CARTESIAN_POINT ( 'NONE',  ( -18.70710678118640402, -12.74070752338415780, 5.000000000000000000 ) ) ;
#111104 = LINE ( 'NONE', #121290, #95262 ) ;
#111105 = CARTESIAN_POINT ( 'NONE',  ( -34.82816939922329169, 21.75929247661549937, 4.000000000000000000 ) ) ;
#111106 = ORIENTED_EDGE ( 'NONE', *, *, #105221, .T. ) ;
#111107 = LINE ( 'NONE', #34295, #115952 ) ;
#111108 = ORIENTED_EDGE ( 'NONE', *, *, #81548, .F. ) ;
#111109 = VECTOR ( 'NONE', #50059, 1000.000000000000000 ) ;
#111110 = CARTESIAN_POINT ( 'NONE',  ( 86.47959685856477563, 6.109999999999999432, 1.637169565754164280 ) ) ;
#111111 = CARTESIAN_POINT ( 'NONE',  ( 18.01107201284014536, 3.061616997868387579E-16, -2.500000000000000444 ) ) ;
#111112 = CARTESIAN_POINT ( 'NONE',  ( 39.48921356237310221, -27.52281430457082934, 5.000000000000000000 ) ) ;
#111113 = DIRECTION ( 'NONE',  ( 0.6830127018922180770, -0.6830127018922204085, -0.2588190451025213501 ) ) ;
#111114 = AXIS2_PLACEMENT_3D ( 'NONE', #19657, #31267, #130585 ) ;
#111115 = CARTESIAN_POINT ( 'NONE',  ( 21.48921356237309155, -27.52281430457070499, 5.000000000000000000 ) ) ;
#111116 = DIRECTION ( 'NONE',  ( 0.000000000000000000, -1.000000000000000000, 0.000000000000000000 ) ) ;
#111117 = EDGE_CURVE ( 'NONE', #142920, #81300, #36608, .T. ) ;
#111118 = ORIENTED_EDGE ( 'NONE', *, *, #139782, .F. ) ;
#111119 = CIRCLE ( 'NONE', #67170, 2.500000000000000888 ) ;
#111120 = DIRECTION ( 'NONE',  ( 0.000000000000000000, -1.000000000000000000, 0.000000000000000000 ) ) ;
#111121 = CARTESIAN_POINT ( 'NONE',  ( 58.82876352523144448, 0.000000000000000000, -6.109999999999998543 ) ) ;
#111122 = DIRECTION ( 'NONE',  ( 0.7071067811865487940, -0.7071067811865463515, 0.000000000000000000 ) ) ;
#111123 = EDGE_CURVE ( 'NONE', #80245, #94584, #100460, .T. ) ;
#111124 = CARTESIAN_POINT ( 'NONE',  ( 34.17183060077623225, -17.24070752338410628, 4.000000000000000000 ) ) ;
#111125 = DIRECTION ( 'NONE',  ( -0.000000000000000000, -0.000000000000000000, -1.000000000000000000 ) ) ;
#111126 = ORIENTED_EDGE ( 'NONE', *, *, #53526, .F. ) ;
#111127 = VECTOR ( 'NONE', #26940, 1000.000000000000000 ) ;
#111128 = CARTESIAN_POINT ( 'NONE',  ( 3.489213562373097322, -27.52281430457057709, 5.000000000000000000 ) ) ;
#111129 = FILL_AREA_STYLE ('',( #33627 ) ) ;
#111130 = EDGE_LOOP ( 'NONE', ( #74930, #87499, #48753, #84075 ) ) ;
#111131 = EDGE_CURVE ( 'NONE', #74472, #113129, #78701, .T. ) ;
#111132 = CARTESIAN_POINT ( 'NONE',  ( 23.51078643762690490, -27.52281430457038880, 5.000000000000000000 ) ) ;
#111133 = ORIENTED_EDGE ( 'NONE', *, *, #78011, .T. ) ;
#111134 = LINE ( 'NONE', #32926, #23739 ) ;
#111135 = CARTESIAN_POINT ( 'NONE',  ( 0.2997448713915885632, -27.71228299555206220, 4.000000000000000000 ) ) ;
#111136 = CIRCLE ( 'NONE', #74121, 31.92999999999999972 ) ;
#111137 = LINE ( 'NONE', #89414, #39644 ) ;
#111138 = EDGE_CURVE ( 'NONE', #39654, #12388, #37306, .T. ) ;
#111139 = FACE_BOUND ( 'NONE', #95105, .T. ) ;
#111140 = CARTESIAN_POINT ( 'NONE',  ( -63.29974487139158867, -27.71228299555250274, 4.000000000000000000 ) ) ;
#111141 = FACE_OUTER_BOUND ( 'NONE', #94957, .T. ) ;
#111142 = DIRECTION ( 'NONE',  ( -1.000000000000000000, -0.000000000000000000, -0.000000000000000000 ) ) ;
#111144 = ORIENTED_EDGE ( 'NONE', *, *, #109865, .F. ) ;
#111143 = CARTESIAN_POINT ( 'NONE',  ( 36.29974487139159578, -27.71228299555231445, 4.000000000000000000 ) ) ;
#111145 = VECTOR ( 'NONE', #20685, 1000.000000000000000 ) ;
#111146 = FACE_OUTER_BOUND ( 'NONE', #129960, .T. ) ;
#111147 = CONTEXT_DEPENDENT_SHAPE_REPRESENTATION ( #116203, #28450 ) ;
#111148 = ORIENTED_EDGE ( 'NONE', *, *, #50698, .F. ) ;
#111149 = EDGE_CURVE ( 'NONE', #1315, #2318, #13410, .T. ) ;
#111150 = EDGE_LOOP ( 'NONE', ( #17227, #82931, #26039, #15528 ) ) ;
#111151 = CARTESIAN_POINT ( 'NONE',  ( 74.57876352523145158, -7.482591942790325086E-16, 6.109999999999998543 ) ) ;
#111152 = ORIENTED_EDGE ( 'NONE', *, *, #135104, .T. ) ;
#111153 = LINE ( 'NONE', #56851, #117020 ) ;
#111154 = DIRECTION ( 'NONE',  ( 0.000000000000000000, -1.000000000000000000, 0.000000000000000000 ) ) ;
#111155 = ORIENTED_EDGE ( 'NONE', *, *, #137941, .T. ) ;
#111156 = LINE ( 'NONE', #66980, #132393 ) ;
#111157 = STYLED_ITEM ( 'NONE', ( #6350 ), #72546 ) ;
#111158 = EDGE_CURVE ( 'NONE', #105448, #142261, #80857, .T. ) ;
#111159 = DIRECTION ( 'NONE',  ( -0.000000000000000000, 0.3543493200069153248, 0.9351131265310292928 ) ) ;
#111160 = VECTOR ( 'NONE', #41318, 1000.000000000000000 ) ;
#111161 = FACE_OUTER_BOUND ( 'NONE', #114671, .T. ) ;
#111162 = VECTOR ( 'NONE', #73096, 1000.000000000000000 ) ;
#111163 = ADVANCED_FACE ( 'NONE', ( #6796 ), #39493, .T. ) ;
#111164 = FACE_OUTER_BOUND ( 'NONE', #114351, .T. ) ;
#111165 = PRESENTATION_STYLE_ASSIGNMENT (( #67728 ) ) ;
#111166 = LINE ( 'NONE', #129537, #140789 ) ;
#111167 = DIRECTION ( 'NONE',  ( 0.7071067811865487940, 0.7071067811865463515, 0.000000000000000000 ) ) ;
#111168 = FACE_OUTER_BOUND ( 'NONE', #99510, .T. ) ;
#111170 = ORIENTED_EDGE ( 'NONE', *, *, #38770, .F. ) ;
#111169 = VECTOR ( 'NONE', #118437, 1000.000000000000227 ) ;
#111171 = AXIS2_PLACEMENT_3D ( 'NONE', #117422, #18099, #62382 ) ;
#111172 = CIRCLE ( 'NONE', #118087, 6.499999999999999112 ) ;
#111173 = COLOUR_RGB ( '', 0.31764706, 0.68627451, 0.89019608) ;
#111174 = VERTEX_POINT ( 'NONE', #106120 ) ;
#111175 = LINE ( 'NONE', #89441, #119152 ) ;
#111176 = LINE ( 'NONE', #56151, #132334 ) ;
#111177 = ORIENTED_EDGE ( 'NONE', *, *, #127528, .F. ) ;
#111178 = VECTOR ( 'NONE', #42597, 1000.000000000000000 ) ;
#111179 = ORIENTED_EDGE ( 'NONE', *, *, #50492, .T. ) ;
#111180 = ORIENTED_EDGE ( 'NONE', *, *, #41550, .T. ) ;
#111181 = EDGE_CURVE ( 'NONE', #130625, #110318, #83727, .T. ) ;
#111182 = CARTESIAN_POINT ( 'NONE',  ( 29.60459685856477208, 1.637169565754164946, -6.109999999999999432 ) ) ;
#111183 = ORIENTED_EDGE ( 'NONE', *, *, #12528, .F. ) ;
#111184 = VECTOR ( 'NONE', #72647, 1000.000000000000000 ) ;
#111185 = DIRECTION ( 'NONE',  ( -0.3543493200069162685, -0.000000000000000000, -0.9351131265310288487 ) ) ;
#111186 = CARTESIAN_POINT ( 'NONE',  ( 1.499999999999990896, 11.52377502935403619, -1.522421517564086502 ) ) ;
#111187 = CARTESIAN_POINT ( 'NONE',  ( 4.150403141435219823, 7.934999999999989839, -2.126176841940961904 ) ) ;
#111188 = CARTESIAN_POINT ( 'NONE',  ( 13.89686957642768306, 5.764391331494414850, -29.07691927642787633 ) ) ;
#111189 = ORIENTED_EDGE ( 'NONE', *, *, #114486, .F. ) ;
#111190 = DIRECTION ( 'NONE',  ( -0.7071067811865486830, -0.7071067811865464625, 0.000000000000000000 ) ) ;
#111191 = CARTESIAN_POINT ( 'NONE',  ( -20.00492477221182241, -5.240707523384225297, 12.38332538355500745 ) ) ;
#111192 = AXIS2_PLACEMENT_3D ( 'NONE', #121783, #124656, #22462 ) ;
#111193 = CARTESIAN_POINT ( 'NONE',  ( -5.994519915287488843, 28.92564299267942118, 4.000000000000000000 ) ) ;
#111195 = ORIENTED_EDGE ( 'NONE', *, *, #58973, .F. ) ;
#111194 = CARTESIAN_POINT ( 'NONE',  ( 8.125146193092287916, -14.24070752338413470, 9.401115078912640755 ) ) ;
#111196 = ORIENTED_EDGE ( 'NONE', *, *, #36107, .T. ) ;
#111197 = CARTESIAN_POINT ( 'NONE',  ( -6.489213562373093325, -27.52281430457059841, 5.000000000000000000 ) ) ;
#111198 = DIRECTION ( 'NONE',  ( 0.7071067811865486830, -0.7071067811865464625, -0.000000000000000000 ) ) ;
#111199 = ORIENTED_EDGE ( 'NONE', *, *, #20898, .T. ) ;
#111200 = AXIS2_PLACEMENT_3D ( 'NONE', #65910, #11455, #52828 ) ;
#111201 = PLANE ( 'NONE',  #34224 ) ;
#111202 = CARTESIAN_POINT ( 'NONE',  ( -12.70000000000000284, -35.14999999999999147, -39.50000000000000000 ) ) ;
#111203 = VECTOR ( 'NONE', #54513, 1000.000000000000000 ) ;
#111204 = ORIENTED_EDGE ( 'NONE', *, *, #140677, .F. ) ;
#111206 = CARTESIAN_POINT ( 'NONE',  ( -23.67183060077630330, 8.259292476615630818, 4.000000000000000000 ) ) ;
#111205 = VECTOR ( 'NONE', #23368, 1000.000000000000000 ) ;
#111207 = SURFACE_STYLE_USAGE ( .BOTH. , #12620 ) ;
#111208 = LINE ( 'NONE', #135844, #42562 ) ;
#111209 = DIRECTION ( 'NONE',  ( -0.000000000000000000, -0.3543493200069152693, 0.9351131265310292928 ) ) ;
#111210 = AXIS2_PLACEMENT_3D ( 'NONE', #64728, #74183, #108912 ) ;
#111211 = CARTESIAN_POINT ( 'NONE',  ( -18.32816939922340183, -9.740707523384182664, 4.000000000000000000 ) ) ;
#111212 = DIRECTION ( 'NONE',  ( -0.7071067811865486830, -0.7071067811865464625, 0.000000000000000000 ) ) ;
#111213 = LINE ( 'NONE', #78617, #33247 ) ;
#111214 = DIRECTION ( 'NONE',  ( 1.000000000000000000, 0.000000000000000000, 0.000000000000000000 ) ) ;
#111215 = ORIENTED_EDGE ( 'NONE', *, *, #52806, .F. ) ;
#111216 = VECTOR ( 'NONE', #94103, 999.9999999999998863 ) ;
#111217 = PLANE ( 'NONE',  #67518 ) ;
#111218 = VERTEX_POINT ( 'NONE', #103983 ) ;
#111219 = FACE_OUTER_BOUND ( 'NONE', #107640, .T. ) ;
#111220 = CARTESIAN_POINT ( 'NONE',  ( 27.48921356237309155, -27.52281430457074762, 5.000000000000000000 ) ) ;
#111221 = LINE ( 'NONE', #119940, #92182 ) ;
#111222 = EDGE_CURVE ( 'NONE', #114427, #131551, #73314, .T. ) ;
#111223 = ORIENTED_EDGE ( 'NONE', *, *, #115466, .F. ) ;
#111224 = VECTOR ( 'NONE', #41725, 1000.000000000000000 ) ;
#111225 = LINE ( 'NONE', #11917, #73948 ) ;
#111226 = DIRECTION ( 'NONE',  ( -0.6830127018922180770, -0.6830127018922204085, -0.2588190451025213501 ) ) ;
#111227 = DIRECTION ( 'NONE',  ( -0.6830127018922180770, -0.6830127018922204085, -0.2588190451025213501 ) ) ;
#111228 = EDGE_CURVE ( 'NONE', #36893, #22361, #138806, .T. ) ;
#111229 = ORIENTED_EDGE ( 'NONE', *, *, #887, .F. ) ;
#111230 = CARTESIAN_POINT ( 'NONE',  ( 55.32830738432641482, -52.14999999996970814, 41.05175048930647819 ) ) ;
#111231 = CARTESIAN_POINT ( 'NONE',  ( 111.2500000000000000, -9.735942053221458872E-16, 7.950000000000000178 ) ) ;
#111232 = EDGE_CURVE ( 'NONE', #99152, #41615, #49671, .T. ) ;
#111233 = AXIS2_PLACEMENT_3D ( 'NONE', #68195, #25338, #112369 ) ;
#111234 = CARTESIAN_POINT ( 'NONE',  ( 7.251592354503322291, 9.902892378096218942E-16, 0.000000000000000000 ) ) ;
#111235 = CARTESIAN_POINT ( 'NONE',  ( -34.92500000000001137, -21.18334561358935986, 4.500000000000000888 ) ) ;
#111236 = EDGE_CURVE ( 'NONE', #135809, #5049, #13142, .T. ) ;
#111237 = CARTESIAN_POINT ( 'NONE',  ( 60.43293019189810877, 1.637169565754156730, 6.110000000000001208 ) ) ;
#111238 = DIRECTION ( 'NONE',  ( -1.000000000000000000, -0.000000000000000000, -0.000000000000000000 ) ) ;
#111239 = LINE ( 'NONE', #80610, #6774 ) ;
#111240 = FILL_AREA_STYLE ('',( #11930 ) ) ;
#111241 = DIRECTION ( 'NONE',  ( 0.7071067811865486830, -0.7071067811865464625, -0.000000000000000000 ) ) ;
#111242 = ORIENTED_EDGE ( 'NONE', *, *, #35061, .T. ) ;
#111243 = ORIENTED_EDGE ( 'NONE', *, *, #112708, .F. ) ;
#111244 = VECTOR ( 'NONE', #117425, 1000.000000000000000 ) ;
#111245 = CARTESIAN_POINT ( 'NONE',  ( -8.999999999999921840, -16.44781430457067373, 5.000000000000000000 ) ) ;
#111246 = CARTESIAN_POINT ( 'NONE',  ( 15.49238828748955576, 4.584330080086930965E-16, 0.000000000000000000 ) ) ;
#111247 = CARTESIAN_POINT ( 'NONE',  ( 0.000000000000000000, -10.77435723561695902, -9.972017380717231205 ) ) ;
#111248 = ADVANCED_FACE ( 'NONE', ( #137373 ), #73544, .F. ) ;
#111249 = DIRECTION ( 'NONE',  ( -0.000000000000000000, 0.000000000000000000, 1.000000000000000000 ) ) ;
#111250 = EDGE_CURVE ( 'NONE', #62294, #135455, #113084, .T. ) ;
#111251 = DIRECTION ( 'NONE',  ( -1.000000000000000000, -0.000000000000000000, -0.000000000000000000 ) ) ;
#111252 = DIRECTION ( 'NONE',  ( 1.000000000000000000, 0.000000000000000000, 0.000000000000000000 ) ) ;
#111253 = ORIENTED_EDGE ( 'NONE', *, *, #81699, .T. ) ;
#111254 = VERTEX_POINT ( 'NONE', #81582 ) ;
#111255 = LINE ( 'NONE', #34432, #34771 ) ;
#111256 = DIRECTION ( 'NONE',  ( 0.7071067811865487940, -0.7071067811865463515, 0.000000000000000000 ) ) ;
#111257 = UNCERTAINTY_MEASURE_WITH_UNIT (LENGTH_MEASURE( 1.000000000000000082E-05 ), #93309, 'distance_accuracy_value', 'NONE');
#111258 = AXIS2_PLACEMENT_3D ( 'NONE', #138749, #69960, #17642 ) ;
#111259 = CARTESIAN_POINT ( 'NONE',  ( -25.39999999999996305, 0.000000000000000000, 0.000000000000000000 ) ) ;
#111260 = ADVANCED_FACE ( 'NONE', ( #84435 ), #128629, .T. ) ;
#111261 = DIRECTION ( 'NONE',  ( -0.7071067811865486830, -0.7071067811865464625, 0.000000000000000000 ) ) ;
#111262 = CARTESIAN_POINT ( 'NONE',  ( 72.41252705046288440, -7.949999999999998401, -4.867971026610728450E-16 ) ) ;
#111263 = DIRECTION ( 'NONE',  ( 0.7071067811865487940, -0.7071067811865463515, 0.000000000000000000 ) ) ;
#111264 = CARTESIAN_POINT ( 'NONE',  ( -24.48921356237309510, -27.52281430457072631, 5.000000000000000000 ) ) ;
#111265 = VERTEX_POINT ( 'NONE', #72147 ) ;
#111266 = CARTESIAN_POINT ( 'NONE',  ( 68.95833333333332860, 3.974999999999997424, 6.884901960086288852 ) ) ;
#111267 = DIRECTION ( 'NONE',  ( 0.7071067811865486830, -0.7071067811865464625, -0.000000000000000000 ) ) ;
#111268 = CARTESIAN_POINT ( 'NONE',  ( 69.29974487139159578, -27.71228299555254537, 4.000000000000000000 ) ) ;
#111269 = LINE ( 'NONE', #88852, #17362 ) ;
#111270 = EDGE_CURVE ( 'NONE', #49451, #44722, #29301, .T. ) ;
#111271 = ORIENTED_EDGE ( 'NONE', *, *, #24125, .T. ) ;
#111272 = AXIS2_PLACEMENT_3D ( 'NONE', #141773, #44629, #23534 ) ;
#111273 = DIRECTION ( 'NONE',  ( 0.7071067811865486830, -0.7071067811865464625, -0.000000000000000000 ) ) ;
#111274 = AXIS2_PLACEMENT_3D ( 'NONE', #82489, #48420, #81801 ) ;
#111275 = ORIENTED_EDGE ( 'NONE', *, *, #97819, .F. ) ;
#111276 = AXIS2_PLACEMENT_3D ( 'NONE', #98834, #53189, #64805 ) ;
#111277 = PLANE ( 'NONE',  #60608 ) ;
#111278 = CARTESIAN_POINT ( 'NONE',  ( 63.00043019189810423, -3.055000000000002380, 5.291415217122920289 ) ) ;
#111279 = LINE ( 'NONE', #88130, #19982 ) ;
#111280 = EDGE_CURVE ( 'NONE', #24661, #18835, #38065, .T. ) ;
#111281 = ORIENTED_EDGE ( 'NONE', *, *, #38939, .F. ) ;
#111282 = VECTOR ( 'NONE', #22583, 1000.000000000000000 ) ;
#111283 = VECTOR ( 'NONE', #127302, 999.9999999999998863 ) ;
#111284 = VECTOR ( 'NONE', #95533, 1000.000000000000000 ) ;
#111285 = VECTOR ( 'NONE', #54467, 1000.000000000000000 ) ;
#111287 = LINE ( 'NONE', #77288, #107787 ) ;
#111286 = AXIS2_PLACEMENT_3D ( 'NONE', #142602, #43290, #87500 ) ;
#111288 = LINE ( 'NONE', #67099, #6968 ) ;
#111289 = FACE_OUTER_BOUND ( 'NONE', #95307, .T. ) ;
#111291 = ORIENTED_EDGE ( 'NONE', *, *, #112424, .F. ) ;
#111290 = CARTESIAN_POINT ( 'NONE',  ( -15.48921356237309510, -27.52281430457066236, 5.000000000000000000 ) ) ;
#111292 = CARTESIAN_POINT ( 'NONE',  ( -5.999999999999963585, 14.87792677143808362, -11.06722581663441218 ) ) ;
#111293 = CARTESIAN_POINT ( 'NONE',  ( 8.994519915287490619, 28.92564299267944250, 4.000000000000000000 ) ) ;
#111294 = DIRECTION ( 'NONE',  ( -1.000000000000000000, 0.000000000000000000, 0.000000000000000000 ) ) ;
#111295 = CIRCLE ( 'NONE', #58169, 2.500000000000000444 ) ;
#111296 = FACE_OUTER_BOUND ( 'NONE', #92670, .T. ) ;
#111297 = VERTEX_POINT ( 'NONE', #104723 ) ;
#111298 = EDGE_LOOP ( 'NONE', ( #71828, #94931, #88203, #38364 ) ) ;
#111299 = CARTESIAN_POINT ( 'NONE',  ( 61.97959685856476852, 6.109999999999999432, 1.637169565754164280 ) ) ;
#111300 = ORIENTED_EDGE ( 'NONE', *, *, #23521, .F. ) ;
#111301 = VECTOR ( 'NONE', #56659, 1000.000000000000000 ) ;
#111302 = CARTESIAN_POINT ( 'NONE',  ( 8.500000000000000000, -2.055000000000000160, 2.789133085058098087E-16 ) ) ;
#111303 = CARTESIAN_POINT ( 'NONE',  ( 16.49999999999988276, 12.43112307739205669, 4.000000000000000000 ) ) ;
#111304 = LINE ( 'NONE', #13408, #13237 ) ;
#111305 = ADVANCED_FACE ( 'NONE', ( #94546 ), #114856, .T. ) ;
#111306 = VECTOR ( 'NONE', #124282, 999.9999999999998863 ) ;
#111307 = DIRECTION ( 'NONE',  ( 1.000000000000000000, 0.000000000000000000, 0.000000000000000000 ) ) ;
#111308 = CARTESIAN_POINT ( 'NONE',  ( 51.18398860626899705, 28.73617430169823095, 5.000000000000000000 ) ) ;
#111309 = ORIENTED_EDGE ( 'NONE', *, *, #52655, .T. ) ;
#111310 = VERTEX_POINT ( 'NONE', #41608 ) ;
#111311 = CARTESIAN_POINT ( 'NONE',  ( -45.18398860626900415, 28.73617430169818832, 5.000000000000000000 ) ) ;
#111312 = FILL_AREA_STYLE ('',( #79471 ) ) ;
#111313 = CIRCLE ( 'NONE', #111200, 1.000000000000000888 ) ;
#111314 = EDGE_LOOP ( 'NONE', ( #73428, #55102, #48360, #14979 ) ) ;
#111315 = AXIS2_PLACEMENT_3D ( 'NONE', #64790, #119838, #30746 ) ;
#111316 = ADVANCED_FACE ( 'NONE', ( #63408 ), #119851, .T. ) ;
#111317 = DIRECTION ( 'NONE',  ( -1.000000000000000000, 0.000000000000000000, -0.000000000000000000 ) ) ;
#111318 = VECTOR ( 'NONE', #44455, 1000.000000000000000 ) ;
#111319 = DIRECTION ( 'NONE',  ( 0.7071067811865487940, -0.7071067811865463515, 0.000000000000000000 ) ) ;
#111320 = DIRECTION ( 'NONE',  ( -0.7071067811865486830, 0.7071067811865464625, 0.000000000000000000 ) ) ;
#111321 = AXIS2_PLACEMENT_3D ( 'NONE', #10855, #56593, #55122 ) ;
#111322 = ORIENTED_EDGE ( 'NONE', *, *, #48619, .T. ) ;
#111323 = EDGE_CURVE ( 'NONE', #11268, #142123, #64084, .T. ) ;
#111324 = FACE_BOUND ( 'NONE', #24784, .T. ) ;
#111325 = CARTESIAN_POINT ( 'NONE',  ( -17.81601139373099940, 28.73617430169775133, 5.000000000000000000 ) ) ;
#111326 = CARTESIAN_POINT ( 'NONE',  ( 72.18398860626899705, 28.73617430169837661, 5.000000000000000000 ) ) ;
#111327 = CARTESIAN_POINT ( 'NONE',  ( -10.49999999999992895, -5.568876922607761237, 4.000000000000000000 ) ) ;
#111328 = DIRECTION ( 'NONE',  ( 0.3543493200069162685, -0.000000000000000000, -0.9351131265310288487 ) ) ;
#111329 = DIRECTION ( 'NONE',  ( 1.000000000000000000, 0.000000000000000000, 0.000000000000000000 ) ) ;
#111330 = EDGE_LOOP ( 'NONE', ( #7296, #67158, #93513, #5610, #125141 ) ) ;
#111331 = VECTOR ( 'NONE', #100920, 1000.000000000000000 ) ;
#111332 = VERTEX_POINT ( 'NONE', #21294 ) ;
#111333 = CARTESIAN_POINT ( 'NONE',  ( 104.9120968585647802, 5.291415217122921177, -3.054999999999994831 ) ) ;
#111334 = ORIENTED_EDGE ( 'NONE', *, *, #104569, .F. ) ;
#111335 = B_SPLINE_CURVE_WITH_KNOTS ( 'NONE', 3,
 ( #38107, #28662, #126506, #27198, #16301, #30047, #17730, #51836, #104769, #39539, #74301, #83769 ),
 .UNSPECIFIED., .F., .F.,
 ( 4, 2, 2, 2, 2, 4 ),
 ( 0.000000000000000000, 0.001125297245559203976, 0.002250594491118407953, 0.002813243113898006905, 0.003375891736677605857, 0.004501188982236803762 ),
 .UNSPECIFIED. ) ;
#111336 = PLANE ( 'NONE',  #141541 ) ;
#111337 = ORIENTED_EDGE ( 'NONE', *, *, #38779, .F. ) ;
#111338 = CARTESIAN_POINT ( 'NONE',  ( -25.49999999999982236, -14.70932175296479549, -11.46312253303831064 ) ) ;
#111339 = AXIS2_PLACEMENT_3D ( 'NONE', #135679, #25459, #81311 ) ;
#111340 = CARTESIAN_POINT ( 'NONE',  ( 4.129139616203772789, 5.278424836066147208, 3.047499999999990550 ) ) ;
#111341 = ORIENTED_EDGE ( 'NONE', *, *, #29379, .F. ) ;
#111342 = DIRECTION ( 'NONE',  ( 0.6830127018922180770, -0.6830127018922204085, -0.2588190451025213501 ) ) ;
#111343 = LINE ( 'NONE', #90315, #119029 ) ;
#111344 = ADVANCED_FACE ( 'NONE', ( #9682 ), #30010, .F. ) ;
#111345 = CARTESIAN_POINT ( 'NONE',  ( 29.12514619309216712, -14.24070752338413293, 9.401115078912591017 ) ) ;
#111346 = CARTESIAN_POINT ( 'NONE',  ( 8.188407645496676324, 3.061616997868380183E-16, -2.500000000000001332 ) ) ;
#111347 = CARTESIAN_POINT ( 'NONE',  ( -66.48921356237309510, -27.52281430457101763, 5.000000000000000000 ) ) ;
#111348 = CARTESIAN_POINT ( 'NONE',  ( 6.489213562373093325, -27.52281430457059841, 5.000000000000000000 ) ) ;
#111349 = VECTOR ( 'NONE', #49914, 1000.000000000000000 ) ;
#111350 = DIRECTION ( 'NONE',  ( -0.6830127018922181881, 0.6830127018922202975, -0.2588190451025214056 ) ) ;
#111351 = VERTEX_POINT ( 'NONE', #54650 ) ;
#111352 = LINE ( 'NONE', #46145, #963 ) ;
#111353 = DIRECTION ( 'NONE',  ( 0.7071067811865487940, 0.7071067811865463515, -0.000000000000000000 ) ) ;
#111354 = VERTEX_POINT ( 'NONE', #119164 ) ;
#111355 = EDGE_CURVE ( 'NONE', #22968, #83246, #40907, .T. ) ;
#111356 = VERTEX_POINT ( 'NONE', #98836 ) ;
#111357 = ADVANCED_FACE ( 'NONE', ( #85821 ), #65553, .F. ) ;
#111358 = ORIENTED_EDGE ( 'NONE', *, *, #29107, .T. ) ;
#111359 = CARTESIAN_POINT ( 'NONE',  ( 55.85459685856476142, -1.637169565754161615, 6.110000000000000320 ) ) ;
#111360 = VECTOR ( 'NONE', #105218, 999.9999999999998863 ) ;
#111361 = VERTEX_POINT ( 'NONE', #64808 ) ;
#111362 = PLANE ( 'NONE',  #92906 ) ;
#111363 = CARTESIAN_POINT ( 'NONE',  ( 10.69163961620377279, 6.094999999999988205, -1.633150327867694651 ) ) ;
#111364 = CARTESIAN_POINT ( 'NONE',  ( 88.52126352523143282, -4.472830434245838482, -4.472830434245840259 ) ) ;
#111365 = PLANE ( 'NONE',  #88844 ) ;
#111366 = LINE ( 'NONE', #78771, #68852 ) ;
#111367 = ORIENTED_EDGE ( 'NONE', *, *, #67327, .T. ) ;
#111368 = CARTESIAN_POINT ( 'NONE',  ( 28.82816939922333077, -2.240707523384257716, 4.000000000000000000 ) ) ;
#111369 = PRESENTATION_LAYER_ASSIGNMENT (  '', '', ( #127648 ) ) ;
#111370 = CARTESIAN_POINT ( 'NONE',  ( 1.199999999999999956, -0.5999999999999993117, -4.543283425070392845 ) ) ;
#111371 = EDGE_LOOP ( 'NONE', ( #59082, #139039, #73899, #110946 ) ) ;
#111372 = EDGE_CURVE ( 'NONE', #90846, #118847, #129321, .T. ) ;
#111373 =( BOUNDED_CURVE ( )  B_SPLINE_CURVE ( 2, ( #49918, #138338, #18664, #32228, #76463, #130851, #56876, #12599, #23481, #9739, #43816, #99594, #111941 ),
 .UNSPECIFIED., .F., .F. ) 
 B_SPLINE_CURVE_WITH_KNOTS ( ( 3, 2, 2, 2, 2, 2, 3 ),
 ( 0.3666666666666666408, 0.3694444444444444642, 0.3722222222222222321, 0.3750000000000000000, 0.3777777777777777679, 0.3805555555555555358, 0.3833333333333333592 ),
 .UNSPECIFIED. ) 
 CURVE ( )  GEOMETRIC_REPRESENTATION_ITEM ( )  RATIONAL_B_SPLINE_CURVE ( ( 1.000000000000000000, 0.9659258262890683122, 1.000000000000000000, 0.9659258262890683122, 1.000000000000000000, 0.9659258262890683122, 1.000000000000000000, 0.9659258262890683122, 1.000000000000000000, 0.9659258262890683122, 1.000000000000000000, 0.9659258262890683122, 1.000000000000000000 ) ) 
 REPRESENTATION_ITEM ( '' )  );
#111374 = DIRECTION ( 'NONE',  ( 1.000000000000000000, -2.496005001405478586E-15, 6.809571051365719919E-16 ) ) ;
#111376 = CARTESIAN_POINT ( 'NONE',  ( 29.91508676806220990, -12.74070752338414536, 18.74364270924360909 ) ) ;
#111375 = VECTOR ( 'NONE', #54001, 1000.000000000000000 ) ;
#111378 = ORIENTED_EDGE ( 'NONE', *, *, #142075, .T. ) ;
#111377 = CIRCLE ( 'NONE', #48912, 2.500000000000000888 ) ;
#111379 = LINE ( 'NONE', #4710, #108265 ) ;
#111380 = VERTEX_POINT ( 'NONE', #19147 ) ;
#111381 = ORIENTED_EDGE ( 'NONE', *, *, #17629, .F. ) ;
#111382 = VERTEX_POINT ( 'NONE', #130060 ) ;
#111383 = VECTOR ( 'NONE', #91306, 1000.000000000000000 ) ;
#111384 = AXIS2_PLACEMENT_3D ( 'NONE', #11942, #35887, #113393 ) ;
#111385 = VECTOR ( 'NONE', #31215, 1000.000000000000000 ) ;
#111386 = VECTOR ( 'NONE', #100800, 1000.000000000000000 ) ;
#111387 = VECTOR ( 'NONE', #103028, 1000.000000000000000 ) ;
#111388 = DIRECTION ( 'NONE',  ( 0.6830127018922181881, 0.6830127018922202975, -0.2588190451025214056 ) ) ;
#111389 = CARTESIAN_POINT ( 'NONE',  ( 1.499999999999994449, -9.462702396501011748, -9.474982329943516746 ) ) ;
#111390 = DIRECTION ( 'NONE',  ( -0.6830127018922181881, 0.6830127018922202975, -0.2588190451025214056 ) ) ;
#111391 = ADVANCED_FACE ( 'NONE', ( #143067 ), #43758, .F. ) ;
#111393 = ORIENTED_EDGE ( 'NONE', *, *, #119098, .T. ) ;
#111392 = CIRCLE ( 'NONE', #51302, 5.968999999999998529 ) ;
#111394 = LINE ( 'NONE', #79552, #132992 ) ;
#111395 = CARTESIAN_POINT ( 'NONE',  ( 11.64540314143521904, -2.126176841940958351, -7.934999999999989839 ) ) ;
#111396 = CARTESIAN_POINT ( 'NONE',  ( -7.499999999999940492, 7.087461875839172087, 4.000000000000000000 ) ) ;
#111397 = EDGE_CURVE ( 'NONE', #61782, #123748, #19848, .T. ) ;
#111398 = LINE ( 'NONE', #134618, #96875 ) ;
#111399 = VECTOR ( 'NONE', #46124, 1000.000000000000000 ) ;
#111400 = DIRECTION ( 'NONE',  ( -0.6830127018922181881, 0.6830127018922202975, -0.2588190451025214056 ) ) ;
#111401 = ORIENTED_EDGE ( 'NONE', *, *, #114012, .T. ) ;
#111402 = ADVANCED_FACE ( 'NONE', ( #42355 ), #86565, .F. ) ;
#111403 = EDGE_LOOP ( 'NONE', ( #49418, #140148, #77861, #84578 ) ) ;
#111404 = ORIENTED_EDGE ( 'NONE', *, *, #135573, .F. ) ;
#111405 = FACE_OUTER_BOUND ( 'NONE', #69705, .T. ) ;
#111406 = UNCERTAINTY_MEASURE_WITH_UNIT (LENGTH_MEASURE( 1.000000000000000082E-05 ), #8051, 'distance_accuracy_value', 'NONE');
#111407 = DIRECTION ( 'NONE',  ( -0.7071067811865486830, -0.7071067811865464625, -0.000000000000000000 ) ) ;
#111408 = DIRECTION ( 'NONE',  ( 0.7071067811865486830, -0.7071067811865464625, -0.000000000000000000 ) ) ;
#111409 = EDGE_CURVE ( 'NONE', #82317, #17208, #32167, .T. ) ;
#111411 = EDGE_CURVE ( 'NONE', #117995, #27223, #941, .T. ) ;
#111410 = CARTESIAN_POINT ( 'NONE',  ( 6.401278309935243271, 9.300261028980425948, -1.956595482711489531 ) ) ;
#111412 = VECTOR ( 'NONE', #108267, 999.9999999999998863 ) ;
#111413 = VECTOR ( 'NONE', #30369, 999.9999999999998863 ) ;
#111414 = CARTESIAN_POINT ( 'NONE',  ( 16.17183060077637791, 9.759292476615634371, 4.000000000000000000 ) ) ;
#111415 = LINE ( 'NONE', #25112, #58826 ) ;
#111416 = CARTESIAN_POINT ( 'NONE',  ( 12.79333936457838483, 21.75929247661549937, 4.998822639870715179 ) ) ;
#111417 = DIRECTION ( 'NONE',  ( 0.7071067811865487940, 0.7071067811865463515, 0.000000000000000000 ) ) ;
#111418 = VECTOR ( 'NONE', #3472, 1000.000000000000000 ) ;
#111419 = ORIENTED_EDGE ( 'NONE', *, *, #140053, .F. ) ;
#111420 = CARTESIAN_POINT ( 'NONE',  ( -34.17183060077623225, -2.240707523384260824, 4.000000000000000000 ) ) ;
#111421 = ORIENTED_EDGE ( 'NONE', *, *, #39546, .T. ) ;
#111423 = AXIS2_PLACEMENT_3D ( 'NONE', #15668, #125194, #34617 ) ;
#111422 = CARTESIAN_POINT ( 'NONE',  ( 19.88391014386735023, -2.827406561154159448, -34.10461866340826731 ) ) ;
#111424 = VERTEX_POINT ( 'NONE', #68406 ) ;
#111425 = LINE ( 'NONE', #121585, #115436 ) ;
#111427 = ORIENTED_EDGE ( 'NONE', *, *, #17798, .T. ) ;
#111426 = CARTESIAN_POINT ( 'NONE',  ( 41.39583333333331439, -2.130196079827427091, 7.949999999999998401 ) ) ;
#111428 = EDGE_CURVE ( 'NONE', #5925, #34100, #57226, .T. ) ;
#111429 = AXIS2_PLACEMENT_3D ( 'NONE', #67432, #113033, #1402 ) ;
#111430 = EDGE_CURVE ( 'NONE', #14195, #57153, #137741, .T. ) ;
#111431 = LINE ( 'NONE', #56397, #55616 ) ;
#111432 = LINE ( 'NONE', #46219, #908 ) ;
#111433 = EDGE_LOOP ( 'NONE', ( #36564, #78221, #90586, #77360 ) ) ;
#111434 = LINE ( 'NONE', #109298, #48513 ) ;
#111435 = ORIENTED_EDGE ( 'NONE', *, *, #115762, .F. ) ;
#111436 = DIRECTION ( 'NONE',  ( -0.7071067811865487940, 0.7071067811865463515, -0.000000000000000000 ) ) ;
#111437 = UNCERTAINTY_MEASURE_WITH_UNIT (LENGTH_MEASURE( 1.000000000000000082E-05 ), #91839, 'distance_accuracy_value', 'NONE');
#111438 = ORIENTED_EDGE ( 'NONE', *, *, #69630, .T. ) ;
#111439 = CARTESIAN_POINT ( 'NONE',  ( 6.722814304570563948, -21.72499999999999432, 5.000000000000000000 ) ) ;
#111440 = EDGE_CURVE ( 'NONE', #69673, #63944, #38415, .T. ) ;
#111441 = CARTESIAN_POINT ( 'NONE',  ( 115.4333603837961988, 2.130196079827431532, -7.949999999999997513 ) ) ;
#111442 = MECHANICAL_DESIGN_GEOMETRIC_PRESENTATION_REPRESENTATION (  '', ( #11873 ), #74429 ) ;
#111443 = DIRECTION ( 'NONE',  ( -0.7071067811865486830, -0.7071067811865464625, -0.000000000000000000 ) ) ;
#111444 = FACE_OUTER_BOUND ( 'NONE', #115387, .T. ) ;
#111445 = CARTESIAN_POINT ( 'NONE',  ( -3.489213562373097322, -27.52281430457057709, 5.000000000000000000 ) ) ;
#111446 = DIRECTION ( 'NONE',  ( 0.000000000000000000, -1.000000000000000000, 0.000000000000000000 ) ) ;
#111448 = VECTOR ( 'NONE', #89545, 1000.000000000000000 ) ;
#111447 = CARTESIAN_POINT ( 'NONE',  ( 11.37500000000000178, -6.094999999999989981, 3.732111120401553285E-16 ) ) ;
#111449 = DIRECTION ( 'NONE',  ( 0.7071067811865486830, -0.7071067811865464625, -0.000000000000000000 ) ) ;
#111450 = ADVANCED_FACE ( 'NONE', ( #24149 ), #112585, .T. ) ;
#111452 = AXIS2_PLACEMENT_3D ( 'NONE', #12813, #1212, #45495 ) ;
#111451 = DIRECTION ( 'NONE',  ( 0.7071067811865487940, 0.7071067811865463515, 0.000000000000000000 ) ) ;
#111453 = CARTESIAN_POINT ( 'NONE',  ( 0.000000000000000000, 0.000000000000000000, 10.00000000000000000 ) ) ;
#111454 = ORIENTED_EDGE ( 'NONE', *, *, #91513, .T. ) ;
#111455 = VERTEX_POINT ( 'NONE', #82635 ) ;
#111456 = CARTESIAN_POINT ( 'NONE',  ( 42.48921356237308800, -27.52281430457085065, 5.000000000000000000 ) ) ;
#111457 = VERTEX_POINT ( 'NONE', #55363 ) ;
#111459 = VECTOR ( 'NONE', #131718, 999.9999999999998863 ) ;
#111458 = CARTESIAN_POINT ( 'NONE',  ( 89.83376352523143282, 6.110000000000001208, 1.122388791418549305E-15 ) ) ;
#111460 = CARTESIAN_POINT ( 'NONE',  ( -25.39999999999996305, 0.000000000000000000, 0.000000000000000000 ) ) ;
#111461 = LINE ( 'NONE', #3394, #90306 ) ;
#111462 = EDGE_CURVE ( 'NONE', #40635, #134689, #27512, .T. ) ;
#111464 = AXIS2_PLACEMENT_3D ( 'NONE', #27606, #17448, #39220 ) ;
#111463 = CARTESIAN_POINT ( 'NONE',  ( 17.81601139373099940, 28.73617430169775133, 5.000000000000000000 ) ) ;
#111465 = DIRECTION ( 'NONE',  ( 0.7071067811865487940, 0.7071067811865463515, 0.000000000000000000 ) ) ;
#111466 = VERTEX_POINT ( 'NONE', #35777 ) ;
#111467 = DIRECTION ( 'NONE',  ( -0.000000000000000000, 1.000000000000000000, 0.000000000000000000 ) ) ;
#111468 = CYLINDRICAL_SURFACE ( 'NONE', #132292, 2.999999999999999112 ) ;
#111469 = CARTESIAN_POINT ( 'NONE',  ( 5.999999999999960032, 4.965500833774338929, -4.007596771432669236 ) ) ;
#111470 = DIRECTION ( 'NONE',  ( -0.7071067811865486830, 0.7071067811865464625, 0.000000000000000000 ) ) ;
#111471 = PLANE ( 'NONE',  #93450 ) ;
#111474 = EDGE_LOOP ( 'NONE', ( #22958, #40642, #73048, #91086 ) ) ;
#111473 = ADVANCED_FACE ( 'NONE', ( #44510 ), #33624, .F. ) ;
#111472 = CARTESIAN_POINT ( 'NONE',  ( 68.99451991528748351, 28.92564299267986172, 4.000000000000000000 ) ) ;
#111475 = CARTESIAN_POINT ( 'NONE',  ( -29.67183060077625711, -15.74070752338412404, 4.000000000000000000 ) ) ;
#111476 = EDGE_CURVE ( 'NONE', #61191, #30378, #38998, .T. ) ;
#111477 = VECTOR ( 'NONE', #60300, 1000.000000000000000 ) ;
#111478 = DIRECTION ( 'NONE',  ( -0.7071067811865486830, -0.7071067811865464625, -0.000000000000000000 ) ) ;
#111479 = DIRECTION ( 'NONE',  ( 0.7071067811865487940, 0.7071067811865463515, 0.000000000000000000 ) ) ;
#111480 = CARTESIAN_POINT ( 'NONE',  ( 17.20710678118642889, 9.759292476615620160, 5.000000000000000000 ) ) ;
#111481 = VERTEX_POINT ( 'NONE', #77822 ) ;
#111482 = ADVANCED_FACE ( 'NONE', ( #12544 ), #26813, .T. ) ;
#111483 = ORIENTED_EDGE ( 'NONE', *, *, #89600, .F. ) ;
#111484 = ORIENTED_EDGE ( 'NONE', *, *, #14047, .T. ) ;
#111485 = CARTESIAN_POINT ( 'NONE',  ( 88.37543019189811844, -5.291415217122920289, -3.055000000000001492 ) ) ;
#111486 = ORIENTED_EDGE ( 'NONE', *, *, #91474, .F. ) ;
#111487 = PLANE ( 'NONE',  #43988 ) ;
#111488 = DIRECTION ( 'NONE',  ( 1.000000000000000000, 0.000000000000000000, 0.000000000000000000 ) ) ;
#111489 = CARTESIAN_POINT ( 'NONE',  ( 39.29974487139159578, -27.71228299555233576, 4.000000000000000000 ) ) ;
#111490 = DIRECTION ( 'NONE',  ( 0.6830127018922181881, 0.6830127018922202975, -0.2588190451025214056 ) ) ;
#111491 = ORIENTED_EDGE ( 'NONE', *, *, #19671, .F. ) ;
#111492 = VECTOR ( 'NONE', #53744, 1000.000000000000000 ) ;
#111493 = CARTESIAN_POINT ( 'NONE',  ( 8.700255128608413102, -27.71228299555199825, 4.000000000000000000 ) ) ;
#111494 = CARTESIAN_POINT ( 'NONE',  ( -12.29974487139158512, -27.71228299555214747, 4.000000000000000000 ) ) ;
#111495 = AXIS2_PLACEMENT_3D ( 'NONE', #117583, #18269, #7409 ) ;
#111497 = VECTOR ( 'NONE', #71419, 1000.000000000000000 ) ;
#111496 = DIRECTION ( 'NONE',  ( -0.000000000000000000, -0.3543493200069152693, 0.9351131265310292928 ) ) ;
#111498 = CARTESIAN_POINT ( 'NONE',  ( 87.12043019189812298, 3.055000000000001936, -5.291415217122916737 ) ) ;
#111499 = ORIENTED_EDGE ( 'NONE', *, *, #3250, .T. ) ;
#111500 = CARTESIAN_POINT ( 'NONE',  ( -6.938893903907228378E-15, -13.39766691384883579, -10.96608748226465835 ) ) ;
#111501 = VECTOR ( 'NONE', #141223, 1000.000000000000000 ) ;
#111502 = FACE_OUTER_BOUND ( 'NONE', #81945, .T. ) ;
#111503 = COLOUR_RGB ( '', 0.08235294, 0.09019608, 0.10196078) ;
#111504 = PRESENTATION_LAYER_ASSIGNMENT (  '', '', ( #60638 ) ) ;
#111505 = AXIS2_PLACEMENT_3D ( 'NONE', #113897, #24743, #136356 ) ;
#111506 = ORIENTED_EDGE ( 'NONE', *, *, #43720, .F. ) ;
#111507 = ORIENTED_EDGE ( 'NONE', *, *, #112539, .F. ) ;
#111508 = DIRECTION ( 'NONE',  ( 0.7071067811865487940, 0.7071067811865463515, 0.000000000000000000 ) ) ;
#111509 = LINE ( 'NONE', #134731, #121827 ) ;
#111510 = DIRECTION ( 'NONE',  ( 0.7071067811865487940, 0.7071067811865463515, 0.000000000000000000 ) ) ;
#111511 = AXIS2_PLACEMENT_3D ( 'NONE', #68739, #78903, #13585 ) ;
#111512 = LINE ( 'NONE', #33972, #48013 ) ;
#111513 = DIRECTION ( 'NONE',  ( 0.000000000000000000, 0.000000000000000000, -1.000000000000000000 ) ) ;
#111514 = DIRECTION ( 'NONE',  ( 0.6830127018922181881, 0.6830127018922202975, -0.2588190451025214056 ) ) ;
#111515 =( NAMED_UNIT ( * ) PLANE_ANGLE_UNIT ( ) SI_UNIT ( $, .RADIAN. ) );
#111516 = ORIENTED_EDGE ( 'NONE', *, *, #133768, .F. ) ;
#111517 = VERTEX_POINT ( 'NONE', #90856 ) ;
#111518 = CARTESIAN_POINT ( 'NONE',  ( -21.80077440930739030, -2.123201397992801276, 4.669108085256719498 ) ) ;
#111519 = ORIENTED_EDGE ( 'NONE', *, *, #135081, .T. ) ;
#111520 = EDGE_CURVE ( 'NONE', #50968, #35420, #135089, .T. ) ;
#111521 = ORIENTED_EDGE ( 'NONE', *, *, #111372, .T. ) ;
#111522 = AXIS2_PLACEMENT_3D ( 'NONE', #10929, #89245, #75519 ) ;
#111523 = COLOUR_RGB ( '', 0.72549020, 0.75294118, 0.79215686) ;
#111524 = DIRECTION ( 'NONE',  ( -0.7071067811865486830, -0.7071067811865464625, 0.000000000000000000 ) ) ;
#111525 = ORIENTED_EDGE ( 'NONE', *, *, #130028, .T. ) ;
#111526 = CARTESIAN_POINT ( 'NONE',  ( 24.48921356237309510, -27.52281430457072631, 5.000000000000000000 ) ) ;
#111527 = PLANE ( 'NONE',  #74996 ) ;
#111528 = DIRECTION ( 'NONE',  ( -1.000000000000000000, -0.000000000000000000, -0.000000000000000000 ) ) ;
#111529 = CIRCLE ( 'NONE', #67594, 2.500000000000000444 ) ;
#111530 = CARTESIAN_POINT ( 'NONE',  ( -12.69999999999998153, 0.000000000000000000, 0.000000000000000000 ) ) ;
#111531 = ORIENTED_EDGE ( 'NONE', *, *, #121105, .F. ) ;
#111532 = DIRECTION ( 'NONE',  ( -0.000000000000000000, -0.3543493200069152693, 0.9351131265310292928 ) ) ;
#111533 = ORIENTED_EDGE ( 'NONE', *, *, #66163, .F. ) ;
#111534 = ADVANCED_FACE ( 'NONE', ( #11812 ), #56099, .F. ) ;
#111535 = CARTESIAN_POINT ( 'NONE',  ( 5.999999999999957367, 16.55218569542900298, 5.000000000000000000 ) ) ;
#111536 = VERTEX_POINT ( 'NONE', #45227 ) ;
#111537 = CARTESIAN_POINT ( 'NONE',  ( 12.18398860626900060, 28.73617430169795739, 5.000000000000000000 ) ) ;
#111538 = ORIENTED_EDGE ( 'NONE', *, *, #116674, .T. ) ;
#111540 = EDGE_CURVE ( 'NONE', #110325, #11989, #124357, .T. ) ;
#111539 = CARTESIAN_POINT ( 'NONE',  ( -36.48921356237310221, -27.52281430457080802, 5.000000000000000000 ) ) ;
#111541 = ORIENTED_EDGE ( 'NONE', *, *, #94915, .F. ) ;
#111542 = ORIENTED_EDGE ( 'NONE', *, *, #27395, .T. ) ;
#111543 = VECTOR ( 'NONE', #32949, 1000.000000000000000 ) ;
#111544 = ORIENTED_EDGE ( 'NONE', *, *, #104328, .F. ) ;
#111545 = DIRECTION ( 'NONE',  ( -0.000000000000000000, -0.3543493200069153248, 0.9351131265310292928 ) ) ;
#111546 = CARTESIAN_POINT ( 'NONE',  ( 8.994519915287490619, 28.92564299267944250, 4.000000000000000000 ) ) ;
#111547 = DIRECTION ( 'NONE',  ( 0.7071067811865487940, 0.7071067811865463515, 0.000000000000000000 ) ) ;
#111548 = CARTESIAN_POINT ( 'NONE',  ( 116.3754301918981042, -5.291415217122920289, -3.055000000000001492 ) ) ;
#111549 = CARTESIAN_POINT ( 'NONE',  ( 0.000000000000000000, 0.000000000000000000, 0.000000000000000000 ) ) ;
#111550 = EDGE_CURVE ( 'NONE', #122875, #46067, #134352, .T. ) ;
#111551 = LINE ( 'NONE', #11489, #11146 ) ;
#111553 = FACE_OUTER_BOUND ( 'NONE', #3712, .T. ) ;
#111552 = AXIS2_PLACEMENT_3D ( 'NONE', #46458, #81939, #136993 ) ;
#111554 = VECTOR ( 'NONE', #96424, 1000.000000000000000 ) ;
#111555 = DIRECTION ( 'NONE',  ( 0.000000000000000000, 0.000000000000000000, -1.000000000000000000 ) ) ;
#111556 = EDGE_CURVE ( 'NONE', #34663, #140587, #52119, .T. ) ;
#111557 = FILL_AREA_STYLE_COLOUR ( '', #55269 ) ;
#111558 = ORIENTED_EDGE ( 'NONE', *, *, #92284, .F. ) ;
#111559 = LINE ( 'NONE', #125302, #31833 ) ;
#111560 = CARTESIAN_POINT ( 'NONE',  ( 6.707106781186501721, 11.25929247661560240, 5.000000000000000000 ) ) ;
#111561 = CARTESIAN_POINT ( 'NONE',  ( 6.540657738503846907, -2.055000000000000160, 2.789133085058097101E-16 ) ) ;
#111562 = VERTEX_POINT ( 'NONE', #139173 ) ;
#111563 = ORIENTED_EDGE ( 'NONE', *, *, #4165, .T. ) ;
#111564 = ORIENTED_EDGE ( 'NONE', *, *, #19754, .T. ) ;
#111565 = VECTOR ( 'NONE', #132119, 1000.000000000000227 ) ;
#111566 = CARTESIAN_POINT ( 'NONE',  ( -18.29974487139159223, -27.71228299555219010, 4.000000000000000000 ) ) ;
#111567 = ADVANCED_FACE ( 'NONE', ( #107909 ), #119666, .T. ) ;
#111568 = ORIENTED_EDGE ( 'NONE', *, *, #64836, .T. ) ;
#111569 = ORIENTED_EDGE ( 'NONE', *, *, #14387, .T. ) ;
#111570 = PLANE ( 'NONE',  #74612 ) ;
#111571 = DIRECTION ( 'NONE',  ( -0.000000000000000000, 0.3543493200069153248, 0.9351131265310292928 ) ) ;
#111572 = DIRECTION ( 'NONE',  ( 0.7071067811865487940, -0.7071067811865463515, 0.000000000000000000 ) ) ;
#111573 = ORIENTED_EDGE ( 'NONE', *, *, #42304, .T. ) ;
#111574 = LINE ( 'NONE', #23865, #7004 ) ;
#111575 = EDGE_CURVE ( 'NONE', #70270, #101548, #18041, .T. ) ;
#111576 = MECHANICAL_DESIGN_GEOMETRIC_PRESENTATION_REPRESENTATION (  '', ( #97709 ), #49106 ) ;
#111577 = ADVANCED_FACE ( 'NONE', ( #83349 ), #16641, .F. ) ;
#111578 = ORIENTED_EDGE ( 'NONE', *, *, #14738, .F. ) ;
#111579 =( BOUNDED_CURVE ( )  B_SPLINE_CURVE ( 3, ( #12292, #121755, #79759, #113023 ),
 .UNSPECIFIED., .F., .T. ) 
 B_SPLINE_CURVE_WITH_KNOTS ( ( 4, 4 ),
 ( 2.779374508378134045, 4.199602562396863803 ),
 .UNSPECIFIED. ) 
 CURVE ( )  GEOMETRIC_REPRESENTATION_ITEM ( )  RATIONAL_B_SPLINE_CURVE ( ( 1.000000000000000000, 0.8388583629366570538, 0.8388583629366570538, 1.000000000000000000 ) ) 
 REPRESENTATION_ITEM ( '' )  );
#111580 = CARTESIAN_POINT ( 'NONE',  ( -31.49999999999977973, -19.53360074219753884, 5.000000000000000000 ) ) ;
#111581 = CARTESIAN_POINT ( 'NONE',  ( 19.17123647476855197, 0.000000000000000000, 7.934999999999990727 ) ) ;
#111582 = ORIENTED_EDGE ( 'NONE', *, *, #3777, .F. ) ;
#111583 = CARTESIAN_POINT ( 'NONE',  ( 83.76626352523145158, 4.472830434245839371, -4.472830434245839371 ) ) ;
#111584 = DIRECTION ( 'NONE',  ( -0.7071067811865486830, 0.7071067811865464625, 0.000000000000000000 ) ) ;
#111585 = DIRECTION ( 'NONE',  ( 0.6830127018922181881, 0.6830127018922202975, -0.2588190451025214056 ) ) ;
#111586 = ORIENTED_EDGE ( 'NONE', *, *, #96118, .T. ) ;
#111587 = EDGE_CURVE ( 'NONE', #45393, #77014, #72515, .T. ) ;
#111588 = DIRECTION ( 'NONE',  ( 0.6830127018922180770, -0.6830127018922204085, -0.2588190451025213501 ) ) ;
#111589 = ORIENTED_EDGE ( 'NONE', *, *, #40467, .T. ) ;
#111590 = ORIENTED_EDGE ( 'NONE', *, *, #7460, .T. ) ;
#111591 = DIRECTION ( 'NONE',  ( -0.7071067811865486830, 0.7071067811865464625, 0.000000000000000000 ) ) ;
#111592 = CARTESIAN_POINT ( 'NONE',  ( -34.92500000000001137, -22.22500000000000142, 4.000000000000000000 ) ) ;
#111593 = DIRECTION ( 'NONE',  ( -0.7071067811865486830, -0.7071067811865464625, 0.000000000000000000 ) ) ;
#111594 = AXIS2_PLACEMENT_3D ( 'NONE', #108184, #52403, #8844 ) ;
#111596 = CARTESIAN_POINT ( 'NONE',  ( -4.171830600776447184, 3.759292476615681888, 4.000000000000000000 ) ) ;
#111595 = AXIS2_PLACEMENT_3D ( 'NONE', #92843, #79887, #45806 ) ;
#111597 = VECTOR ( 'NONE', #15890, 1000.000000000000000 ) ;
#111598 = CARTESIAN_POINT ( 'NONE',  ( 15.29974487139158867, -27.71228299555216879, 4.000000000000000000 ) ) ;
#111599 = ORIENTED_EDGE ( 'NONE', *, *, #84472, .T. ) ;
#111600 = EDGE_CURVE ( 'NONE', #56418, #76475, #131294, .T. ) ;
#111602 = ADVANCED_FACE ( 'NONE', ( #63050 ), #86204, .T. ) ;
#111601 =( GEOMETRIC_REPRESENTATION_CONTEXT ( 3 ) GLOBAL_UNCERTAINTY_ASSIGNED_CONTEXT ( ( #91125 ) ) GLOBAL_UNIT_ASSIGNED_CONTEXT ( ( #138315, #104219, #139032 ) ) REPRESENTATION_CONTEXT ( 'NONE', 'WORKASPACE' ) );
#111603 = DIRECTION ( 'NONE',  ( 0.7071067811865486830, -0.7071067811865464625, -0.000000000000000000 ) ) ;
#111604 = DIRECTION ( 'NONE',  ( -0.6830127018922181881, 0.6830127018922202975, -0.2588190451025214056 ) ) ;
#111605 = CARTESIAN_POINT ( 'NONE',  ( 16.75173015016484968, -2.055000000000000160, 2.789133085058097101E-16 ) ) ;
#111606 = ORIENTED_EDGE ( 'NONE', *, *, #19515, .F. ) ;
#111607 = LINE ( 'NONE', #100734, #7344 ) ;
#111608 = VECTOR ( 'NONE', #88123, 1000.000000000000000 ) ;
#111609 = VECTOR ( 'NONE', #43185, 1000.000000000000000 ) ;
#111610 = VECTOR ( 'NONE', #53955, 1000.000000000000000 ) ;
#111611 = AXIS2_PLACEMENT_3D ( 'NONE', #69609, #77621, #113066 ) ;
#111613 = EDGE_CURVE ( 'NONE', #115452, #16626, #28256, .T. ) ;
#111612 = DIRECTION ( 'NONE',  ( -1.000000000000000000, -0.000000000000000000, -0.000000000000000000 ) ) ;
#111614 = ORIENTED_EDGE ( 'NONE', *, *, #27897, .F. ) ;
#111616 = ORIENTED_EDGE ( 'NONE', *, *, #83690, .T. ) ;
#111615 = DIRECTION ( 'NONE',  ( -0.000000000000000000, -0.3543493200069152693, 0.9351131265310292928 ) ) ;
#111618 = ORIENTED_EDGE ( 'NONE', *, *, #105807, .F. ) ;
#111617 = ADVANCED_FACE ( 'NONE', ( #115939 ), #106479, .T. ) ;
#111619 = EDGE_CURVE ( 'NONE', #101569, #27362, #74626, .T. ) ;
#111620 = PLANE ( 'NONE',  #86420 ) ;
#111621 = CARTESIAN_POINT ( 'NONE',  ( 24.18398860626899705, 28.73617430169804265, 5.000000000000000000 ) ) ;
#111622 = EDGE_LOOP ( 'NONE', ( #134653, #109608, #55130 ) ) ;
#111623 = CARTESIAN_POINT ( 'NONE',  ( -42.29974487139158157, -27.71228299555235708, 4.000000000000000000 ) ) ;
#111624 = UNCERTAINTY_MEASURE_WITH_UNIT (LENGTH_MEASURE( 1.000000000000000082E-05 ), #118874, 'distance_accuracy_value', 'NONE');
#111625 = CARTESIAN_POINT ( 'NONE',  ( -30.18398860626900060, 28.73617430169808173, 5.000000000000000000 ) ) ;
#111626 = CARTESIAN_POINT ( 'NONE',  ( 3.005480084712505828, 28.92564299267936079, 4.000000000000000000 ) ) ;
#111627 = DIRECTION ( 'NONE',  ( -0.000000000000000000, -0.3543493200069152693, 0.9351131265310292928 ) ) ;
#111628 = EDGE_CURVE ( 'NONE', #53028, #82630, #7166, .T. ) ;
#111629 = DIRECTION ( 'NONE',  ( -0.7071067811865487940, 0.7071067811865463515, 0.000000000000000000 ) ) ;
#111630 = CARTESIAN_POINT ( 'NONE',  ( -12.12147316337139813, -20.24070752338407431, 7.412974875817818443 ) ) ;
#111631 = FACE_OUTER_BOUND ( 'NONE', #2286, .T. ) ;
#111632 = DIRECTION ( 'NONE',  ( -0.000000000000000000, -0.000000000000000000, 1.000000000000000000 ) ) ;
#111633 = CARTESIAN_POINT ( 'NONE',  ( -22.96836484077793727, 2.259292476615697876, 13.77329220150631883 ) ) ;
#111634 = CARTESIAN_POINT ( 'NONE',  ( 24.33290314143522437, -3.967499999999994476, 6.871911579029513106 ) ) ;
#111635 = DIRECTION ( 'NONE',  ( -0.7071067811865487940, 0.7071067811865463515, -0.000000000000000000 ) ) ;
#111636 = CARTESIAN_POINT ( 'NONE',  ( 0.000000000000000000, 0.000000000000000000, 5.000000000000000000 ) ) ;
#111637 = EDGE_CURVE ( 'NONE', #30838, #78485, #6435, .T. ) ;
#111638 = CARTESIAN_POINT ( 'NONE',  ( 10.74845587132417890, -11.24070752338416490, 10.39518518046006790 ) ) ;
#111639 = DIRECTION ( 'NONE',  ( -0.7071067811865486830, 0.7071067811865464625, 0.000000000000000000 ) ) ;
#111640 = ORIENTED_EDGE ( 'NONE', *, *, #130147, .T. ) ;
#111641 = AXIS2_PLACEMENT_3D ( 'NONE', #123149, #4126, #134753 ) ;
#111642 = ORIENTED_EDGE ( 'NONE', *, *, #140232, .F. ) ;
#111643 = CARTESIAN_POINT ( 'NONE',  ( 105.8541666666666430, -2.130196079827425315, -7.950000000000001066 ) ) ;
#111644 = VECTOR ( 'NONE', #63926, 999.9999999999998863 ) ;
#111645 = ORIENTED_EDGE ( 'NONE', *, *, #24055, .F. ) ;
#111646 = ORIENTED_EDGE ( 'NONE', *, *, #108765, .T. ) ;
#111647 = VECTOR ( 'NONE', #34031, 1000.000000000000114 ) ;
#111648 = EDGE_LOOP ( 'NONE', ( #118784, #4599, #91365, #16045 ) ) ;
#111649 = DIRECTION ( 'NONE',  ( -0.000000000000000000, -0.3543493200069152693, 0.9351131265310292928 ) ) ;
#111650 = CARTESIAN_POINT ( 'NONE',  ( 19.05000000000000071, 3.174999999999997158, 4.000000000000000000 ) ) ;
#111651 = VECTOR ( 'NONE', #54288, 1000.000000000000000 ) ;
#111652 = PLANE ( 'NONE',  #119479 ) ;
#111653 = VERTEX_POINT ( 'NONE', #30386 ) ;
#111654 = CARTESIAN_POINT ( 'NONE',  ( 2.139447441471317823, -2.500000000000000000, 3.061616997868383634E-16 ) ) ;
#111655 = CARTESIAN_POINT ( 'NONE',  ( 4.499999999999968914, 22.22500000000000142, 4.362957392718803007 ) ) ;
#111656 = PLANE ( 'NONE',  #60327 ) ;
#111657 = DIRECTION ( 'NONE',  ( -0.7071067811865486830, 0.7071067811865464625, 0.000000000000000000 ) ) ;
#111658 = ORIENTED_EDGE ( 'NONE', *, *, #44779, .T. ) ;
#111659 = CARTESIAN_POINT ( 'NONE',  ( -33.18398860626899705, 28.73617430169810305, 5.000000000000000000 ) ) ;
#111660 = CARTESIAN_POINT ( 'NONE',  ( -63.29974487139158867, -27.71228299555250274, 4.000000000000000000 ) ) ;
#111661 = PLANE ( 'NONE',  #42720 ) ;
#111662 = CARTESIAN_POINT ( 'NONE',  ( 34.92499999999998295, 14.81665438641030264, 4.500000000000000888 ) ) ;
#111663 = CARTESIAN_POINT ( 'NONE',  ( 27.00000000000000000, 5.807595119381032234, 2.946028100216067092 ) ) ;
#111664 = PLANE ( 'NONE',  #9849 ) ;
#111665 = LINE ( 'NONE', #56619, #133395 ) ;
#111666 = DIRECTION ( 'NONE',  ( 0.7071067811865486830, -0.7071067811865464625, -0.000000000000000000 ) ) ;
#111667 = FACE_OUTER_BOUND ( 'NONE', #61625, .T. ) ;
#111668 = EDGE_CURVE ( 'NONE', #13978, #12164, #97025, .T. ) ;
#111669 = EDGE_CURVE ( 'NONE', #107040, #114480, #127562, .T. ) ;
#111670 = ORIENTED_EDGE ( 'NONE', *, *, #45968, .T. ) ;
#111671 = ORIENTED_EDGE ( 'NONE', *, *, #5030, .F. ) ;
#111672 = CARTESIAN_POINT ( 'NONE',  ( 124.5420968585647756, 5.291415217122923842, -3.054999999999996163 ) ) ;
#111673 = ORIENTED_EDGE ( 'NONE', *, *, #87375, .T. ) ;
#111674 = VECTOR ( 'NONE', #78704, 1000.000000000000227 ) ;
#111675 = CARTESIAN_POINT ( 'NONE',  ( 100.0208333333333286, 7.949999999999998401, 2.130196079827431532 ) ) ;
#111676 = VECTOR ( 'NONE', #107854, 1000.000000000000227 ) ;
#111677 = CARTESIAN_POINT ( 'NONE',  ( -2.816011393730999401, 28.73617430169785436, 5.000000000000000000 ) ) ;
#111678 = LINE ( 'NONE', #100799, #2676 ) ;
#111679 = CARTESIAN_POINT ( 'NONE',  ( 5.443598275411213550, 3.821174125832445049E-16, 0.000000000000000000 ) ) ;
#111680 = CARTESIAN_POINT ( 'NONE',  ( 116.2870968585647802, 3.054999999999997495, 5.291415217122919401 ) ) ;
#111681 = ORIENTED_EDGE ( 'NONE', *, *, #108494, .T. ) ;
#111682 = ORIENTED_EDGE ( 'NONE', *, *, #27767, .T. ) ;
#111683 = VECTOR ( 'NONE', #139976, 1000.000000000000114 ) ;
#111684 = CARTESIAN_POINT ( 'NONE',  ( -21.48921356237309155, -27.52281430457070499, 5.000000000000000000 ) ) ;
#111685 = VECTOR ( 'NONE', #48565, 1000.000000000000227 ) ;
#111686 = DIRECTION ( 'NONE',  ( 0.7071067811865487940, -0.7071067811865463515, 0.000000000000000000 ) ) ;
#111687 = VERTEX_POINT ( 'NONE', #94907 ) ;
#111688 = ORIENTED_EDGE ( 'NONE', *, *, #139362, .T. ) ;
#111689 = CARTESIAN_POINT ( 'NONE',  ( 40.97959685856477563, 6.109999999999999432, 1.637169565754164280 ) ) ;
#111690 = ORIENTED_EDGE ( 'NONE', *, *, #137756, .F. ) ;
#111691 = CARTESIAN_POINT ( 'NONE',  ( -4.499999999999968914, -14.56887692260766265, 4.000000000000000000 ) ) ;
#111692 = SURFACE_SIDE_STYLE ('',( #23970 ) ) ;
#111693 = CARTESIAN_POINT ( 'NONE',  ( 30.97459685856477662, 1.637169565754164058, -6.109999999999996767 ) ) ;
#111694 = EDGE_LOOP ( 'NONE', ( #3462, #41680, #40787, #25859 ) ) ;
#111695 = LINE ( 'NONE', #120381, #94128 ) ;
#111696 = EDGE_LOOP ( 'NONE', ( #121775, #134470, #35224, #13920 ) ) ;
#111697 = ORIENTED_EDGE ( 'NONE', *, *, #8166, .T. ) ;
#111698 = AXIS2_PLACEMENT_3D ( 'NONE', #44429, #122654, #131414 ) ;
#111699 = VECTOR ( 'NONE', #107652, 999.9999999999998863 ) ;
#111700 = VERTEX_POINT ( 'NONE', #139890 ) ;
#111701 = VECTOR ( 'NONE', #98157, 1000.000000000000000 ) ;
#111702 = VECTOR ( 'NONE', #104794, 1000.000000000000000 ) ;
#111703 = VECTOR ( 'NONE', #88556, 1000.000000000000000 ) ;
#111704 = DIRECTION ( 'NONE',  ( 1.000000000000000000, 0.000000000000000000, 0.000000000000000000 ) ) ;
#111705 = DIRECTION ( 'NONE',  ( 0.3543493200069162685, -0.000000000000000000, -0.9351131265310288487 ) ) ;
#111706 = ORIENTED_EDGE ( 'NONE', *, *, #143283, .T. ) ;
#111707 = PLANE ( 'NONE',  #64532 ) ;
#111709 = CARTESIAN_POINT ( 'NONE',  ( -53.99451991528749062, 28.92564299267975869, 4.000000000000000000 ) ) ;
#111708 = AXIS2_PLACEMENT_3D ( 'NONE', #53922, #41573, #85794 ) ;
#111710 = AXIS2_PLACEMENT_3D ( 'NONE', #130006, #29959, #63361 ) ;
#111711 = PRESENTATION_LAYER_ASSIGNMENT (  '', '', ( #107047 ) ) ;
#111712 = DIRECTION ( 'NONE',  ( -0.000000000000000000, 0.000000000000000000, 1.000000000000000000 ) ) ;
#111713 = EDGE_CURVE ( 'NONE', #76630, #137730, #7895, .T. ) ;
#111714 = FACE_BOUND ( 'NONE', #67009, .T. ) ;
#111715 = ORIENTED_EDGE ( 'NONE', *, *, #3238, .T. ) ;
#111716 = CYLINDRICAL_SURFACE ( 'NONE', #94311, 2.500000000000000000 ) ;
#111717 = EDGE_CURVE ( 'NONE', #1213, #61607, #63749, .T. ) ;
#111719 = EDGE_CURVE ( 'NONE', #85558, #84409, #89070, .T. ) ;
#111718 = LINE ( 'NONE', #26137, #53023 ) ;
#111720 = PLANE ( 'NONE',  #37530 ) ;
#111721 = DIRECTION ( 'NONE',  ( 1.000000000000000000, 0.000000000000000000, 0.000000000000000000 ) ) ;
#111722 = ORIENTED_EDGE ( 'NONE', *, *, #88658, .F. ) ;
#111723 = CARTESIAN_POINT ( 'NONE',  ( 24.83747294953710849, 6.094999999999989981, -1.119633336120465690E-15 ) ) ;
#111724 = ORIENTED_EDGE ( 'NONE', *, *, #36798, .F. ) ;
#111725 = ORIENTED_EDGE ( 'NONE', *, *, #48801, .T. ) ;
#111726 = VERTEX_POINT ( 'NONE', #120952 ) ;
#111727 = EDGE_CURVE ( 'NONE', #52145, #40163, #54315, .T. ) ;
#111728 = ADVANCED_FACE ( 'NONE', ( #43409 ), #65184, .T. ) ;
#111729 = CARTESIAN_POINT ( 'NONE',  ( 49.78709685856478018, 3.054999999999997495, 5.291415217122919401 ) ) ;
#111730 = EDGE_LOOP ( 'NONE', ( #122743, #120878, #92206, #90538 ) ) ;
#111731 = VECTOR ( 'NONE', #131588, 1000.000000000000000 ) ;
#111732 = FACE_OUTER_BOUND ( 'NONE', #56548, .T. ) ;
#111733 = DIRECTION ( 'NONE',  ( 0.7071067811865487940, -0.7071067811865463515, 0.000000000000000000 ) ) ;
#111734 = EDGE_CURVE ( 'NONE', #142281, #68447, #142029, .T. ) ;
#111735 = VERTEX_POINT ( 'NONE', #119501 ) ;
#111736 = DIRECTION ( 'NONE',  ( -1.000000000000000000, -0.000000000000000000, -0.000000000000000000 ) ) ;
#111737 = AXIS2_PLACEMENT_3D ( 'NONE', #84811, #18825, #84132 ) ;
#111738 = ADVANCED_FACE ( 'NONE', ( #31816 ), #76038, .F. ) ;
#111739 = CARTESIAN_POINT ( 'NONE',  ( 0.000000000000000000, 0.000000000000000000, 5.000000000000000000 ) ) ;
#111740 = CARTESIAN_POINT ( 'NONE',  ( 25.49999999999982236, 4.466399257802211586, 5.000000000000000000 ) ) ;
#111741 = FACE_OUTER_BOUND ( 'NONE', #25200, .T. ) ;
#111742 = VECTOR ( 'NONE', #59890, 1000.000000000000000 ) ;
#111743 = DIRECTION ( 'NONE',  ( 0.6830127018922181881, 0.6830127018922202975, -0.2588190451025214056 ) ) ;
#111744 = ORIENTED_EDGE ( 'NONE', *, *, #31110, .T. ) ;
#111745 = EDGE_LOOP ( 'NONE', ( #136726, #90554, #69574, #10687 ) ) ;
#111746 = VERTEX_POINT ( 'NONE', #89755 ) ;
#111747 = VECTOR ( 'NONE', #52453, 1000.000000000000000 ) ;
#111748 = EDGE_LOOP ( 'NONE', ( #39366, #42722, #107101, #111281 ) ) ;
#111749 =( GEOMETRIC_REPRESENTATION_CONTEXT ( 3 ) GLOBAL_UNCERTAINTY_ASSIGNED_CONTEXT ( ( #7090 ) ) GLOBAL_UNIT_ASSIGNED_CONTEXT ( ( #95434, #29457, #387 ) ) REPRESENTATION_CONTEXT ( 'NONE', 'WORKASPACE' ) );
#111750 = DIRECTION ( 'NONE',  ( -0.7071067811865486830, 0.7071067811865464625, 0.000000000000000000 ) ) ;
#111751 = EDGE_CURVE ( 'NONE', #82218, #13451, #110768, .T. ) ;
#111752 = CARTESIAN_POINT ( 'NONE',  ( 36.10002705046289151, 5.819803920172570422, 5.819803920172575751 ) ) ;
#111753 = ORIENTED_EDGE ( 'NONE', *, *, #43235, .F. ) ;
#111754 = ORIENTED_EDGE ( 'NONE', *, *, #10040, .T. ) ;
#111755 = DIRECTION ( 'NONE',  ( -0.7071067811865486830, -0.7071067811865464625, -0.000000000000000000 ) ) ;
#111756 = DIRECTION ( 'NONE',  ( -1.000000000000000000, -1.224606353822377258E-16, -0.000000000000000000 ) ) ;
#111757 = VERTEX_POINT ( 'NONE', #11454 ) ;
#111758 = CARTESIAN_POINT ( 'NONE',  ( -1.499999999999987566, -19.53360074219753884, 5.000000000000000000 ) ) ;
#111759 = EDGE_CURVE ( 'NONE', #19965, #40586, #111512, .T. ) ;
#111760 = CARTESIAN_POINT ( 'NONE',  ( 26.29298673570676215, -21.74070752338406365, 4.999753212805220670 ) ) ;
#111761 = CARTESIAN_POINT ( 'NONE',  ( 23.25456980810188767, -6.871911579029512218, 3.967499999999996252 ) ) ;
#111762 = CARTESIAN_POINT ( 'NONE',  ( 0.000000000000000000, 0.000000000000000000, 5.000000000000000000 ) ) ;
#111763 = ORIENTED_EDGE ( 'NONE', *, *, #140662, .T. ) ;
#111765 = LINE ( 'NONE', #46554, #22120 ) ;
#111764 = CARTESIAN_POINT ( 'NONE',  ( 110.1620968585647944, -5.291415217122919401, 3.054999999999998384 ) ) ;
#111766 = DIRECTION ( 'NONE',  ( 0.000000000000000000, -1.000000000000000000, 0.000000000000000000 ) ) ;
#111767 = CARTESIAN_POINT ( 'NONE',  ( -34.45011844616455221, -7.483719188362438324, 5.000000000000000888 ) ) ;
#111768 = AXIS2_PLACEMENT_3D ( 'NONE', #57715, #22877, #110610 ) ;
#111769 = EDGE_CURVE ( 'NONE', #59176, #60739, #22326, .T. ) ;
#111770 = FACE_OUTER_BOUND ( 'NONE', #57408, .T. ) ;
#111772 = ORIENTED_EDGE ( 'NONE', *, *, #4654, .F. ) ;
#111771 = CARTESIAN_POINT ( 'NONE',  ( 12.18398860626900060, 28.73617430169795739, 5.000000000000000000 ) ) ;
#111774 = AXIS2_PLACEMENT_3D ( 'NONE', #24282, #104687, #103254 ) ;
#111773 = FACE_OUTER_BOUND ( 'NONE', #45288, .T. ) ;
#111775 = ORIENTED_EDGE ( 'NONE', *, *, #19772, .T. ) ;
#111776 = FACE_OUTER_BOUND ( 'NONE', #112313, .T. ) ;
#111777 = VERTEX_POINT ( 'NONE', #20195 ) ;
#111778 = EDGE_CURVE ( 'NONE', #15594, #29105, #100654, .T. ) ;
#111779 = LINE ( 'NONE', #113909, #25079 ) ;
#111780 = EDGE_CURVE ( 'NONE', #119924, #66688, #27409, .T. ) ;
#111781 = LINE ( 'NONE', #58153, #136741 ) ;
#111782 = CARTESIAN_POINT ( 'NONE',  ( 4.771493228613326032, 20.25929247661551003, 7.808871592221780844 ) ) ;
#111783 = VERTEX_POINT ( 'NONE', #133291 ) ;
#111784 = CIRCLE ( 'NONE', #63181, 0.5000000000000004441 ) ;
#111786 = EDGE_CURVE ( 'NONE', #69422, #71281, #66977, .T. ) ;
#111785 = CARTESIAN_POINT ( 'NONE',  ( -16.49999999999988276, -20.53675388469232033, 2.352720554255855134 ) ) ;
#111787 = EDGE_LOOP ( 'NONE', ( #113511, #50500 ) ) ;
#111788 = LINE ( 'NONE', #88621, #117849 ) ;
#111790 = ORIENTED_EDGE ( 'NONE', *, *, #60928, .T. ) ;
#111789 = DIRECTION ( 'NONE',  ( 0.6830127018922180770, -0.6830127018922204085, -0.2588190451025213501 ) ) ;
#111791 = ORIENTED_EDGE ( 'NONE', *, *, #17580, .T. ) ;
#111792 = AXIS2_PLACEMENT_3D ( 'NONE', #104318, #128255, #4986 ) ;
#111793 = CARTESIAN_POINT ( 'NONE',  ( -13.10530833935383299, 3.713635273109021639, 4.055062020558137803 ) ) ;
#111794 = ORIENTED_EDGE ( 'NONE', *, *, #93006, .F. ) ;
#111795 = LINE ( 'NONE', #12461, #108502 ) ;
#111796 = PRESENTATION_STYLE_ASSIGNMENT (( #45150 ) ) ;
#111797 = DIRECTION ( 'NONE',  ( 0.7071067811865486830, -0.7071067811865464625, -0.000000000000000000 ) ) ;
#111798 = ORIENTED_EDGE ( 'NONE', *, *, #99841, .T. ) ;
#111799 = EDGE_CURVE ( 'NONE', #43144, #62908, #23800, .T. ) ;
#111800 = CARTESIAN_POINT ( 'NONE',  ( -31.49999999999977973, -16.53360074219757792, 5.000000000000000000 ) ) ;
#111801 = LINE ( 'NONE', #89330, #139337 ) ;
#111802 = CARTESIAN_POINT ( 'NONE',  ( 12.19999999999999574, -22.26999999999999247, 0.000000000000000000 ) ) ;
#111803 = VECTOR ( 'NONE', #13860, 999.9999999999998863 ) ;
#111804 = CARTESIAN_POINT ( 'NONE',  ( 7.499999999999944045, -8.568876922607730151, 4.000000000000000000 ) ) ;
#111805 = CARTESIAN_POINT ( 'NONE',  ( -8.999999999999937828, 10.21212019023808004, -2.019456568337778979 ) ) ;
#111806 = CARTESIAN_POINT ( 'NONE',  ( 30.97459685856477662, 1.637169565754164280, -6.109999999999997655 ) ) ;
#111807 = EDGE_CURVE ( 'NONE', #23719, #115183, #136831, .T. ) ;
#111808 = DIRECTION ( 'NONE',  ( 0.000000000000000000, 0.000000000000000000, -1.000000000000000000 ) ) ;
#111810 = ORIENTED_EDGE ( 'NONE', *, *, #38769, .F. ) ;
#111809 = AXIS2_PLACEMENT_3D ( 'NONE', #60270, #71861, #103037 ) ;
#111811 = VECTOR ( 'NONE', #22715, 1000.000000000000000 ) ;
#111812 = ORIENTED_EDGE ( 'NONE', *, *, #127048, .T. ) ;
#111813 = ORIENTED_EDGE ( 'NONE', *, *, #78186, .T. ) ;
#111814 = DIRECTION ( 'NONE',  ( -0.000000000000000000, 0.000000000000000000, 1.000000000000000000 ) ) ;
#111815 = ORIENTED_EDGE ( 'NONE', *, *, #899, .T. ) ;
#111816 = ORIENTED_EDGE ( 'NONE', *, *, #105961, .T. ) ;
#111817 = ORIENTED_EDGE ( 'NONE', *, *, #108494, .F. ) ;
#111818 = VECTOR ( 'NONE', #101756, 1000.000000000000000 ) ;
#111819 = VECTOR ( 'NONE', #118598, 1000.000000000000000 ) ;
#111820 = CARTESIAN_POINT ( 'NONE',  ( 1.598550070791607602, -0.6056895305754137482, -6.475271963048705892 ) ) ;
#111821 = STYLED_ITEM ( 'NONE', ( #105608 ), #96673 ) ;
#111822 = CARTESIAN_POINT ( 'NONE',  ( 17.29289321881334018, -12.74070752338414714, 5.000000000000000000 ) ) ;
#111823 = EDGE_LOOP ( 'NONE', ( #107476, #39746, #76166, #15622 ) ) ;
#111824 = CARTESIAN_POINT ( 'NONE',  ( -17.99999999999986500, 14.58746187583909126, 4.000000000000000000 ) ) ;
#111825 = DIRECTION ( 'NONE',  ( -0.000000000000000000, -0.3543493200069152693, 0.9351131265310292928 ) ) ;
#111826 = CARTESIAN_POINT ( 'NONE',  ( 0.000000000000000000, 0.000000000000000000, 0.000000000000000000 ) ) ;
#111827 = EDGE_CURVE ( 'NONE', #16613, #17766, #14344, .T. ) ;
#111828 = CARTESIAN_POINT ( 'NONE',  ( -57.48921356237308800, -27.52281430457095368, 5.000000000000000000 ) ) ;
#111829 = CARTESIAN_POINT ( 'NONE',  ( 124.3962635252314470, 4.472830434245840259, -4.472830434245839371 ) ) ;
#111830 = EDGE_LOOP ( 'NONE', ( #45101, #63123, #82828, #53798 ) ) ;
#111831 = ADVANCED_FACE ( 'NONE', ( #90485 ), #134733, .F. ) ;
#111832 = LINE ( 'NONE', #80636, #11750 ) ;
#111833 = CARTESIAN_POINT ( 'NONE',  ( 28.78501580275792548, -3.740707523384241728, 15.76143240460130635 ) ) ;
#111834 = AXIS2_PLACEMENT_3D ( 'NONE', #108048, #85599, #63886 ) ;
#111835 = CARTESIAN_POINT ( 'NONE',  ( -29.16347128873433192, 15.75929247661555443, 9.299976744542854945 ) ) ;
#111836 = DIRECTION ( 'NONE',  ( 0.000000000000000000, -0.3543493200069153248, -0.9351131265310291818 ) ) ;
#111837 = DIRECTION ( 'NONE',  ( -0.6830127018922180770, -0.6830127018922204085, -0.2588190451025213501 ) ) ;
#111838 = CARTESIAN_POINT ( 'NONE',  ( 0.3605399447480615582, -0.3999999999999998002, -2.166563668000045517 ) ) ;
#111839 = DIRECTION ( 'NONE',  ( 0.7071067811865487940, -0.7071067811865463515, 0.000000000000000000 ) ) ;
#111840 = CARTESIAN_POINT ( 'NONE',  ( 51.55836038379622011, -7.949999999999997513, -2.130196079827425759 ) ) ;
#111841 = CARTESIAN_POINT ( 'NONE',  ( -10.49999999999993250, 7.087461875839178305, 4.000000000000000000 ) ) ;
#111843 = CARTESIAN_POINT ( 'NONE',  ( 0.000000000000000000, 0.000000000000000000, 5.000000000000000000 ) ) ;
#111842 = VECTOR ( 'NONE', #52245, 1000.000000000000227 ) ;
#111844 = ORIENTED_EDGE ( 'NONE', *, *, #105743, .T. ) ;
#111845 = ORIENTED_EDGE ( 'NONE', *, *, #31276, .F. ) ;
#111846 = CARTESIAN_POINT ( 'NONE',  ( 41.39583333333331439, -2.130196079827427091, 7.949999999999999289 ) ) ;
#111847 = LINE ( 'NONE', #77096, #67167 ) ;
#111848 = VERTEX_POINT ( 'NONE', #35425 ) ;
#111849 = LINE ( 'NONE', #53920, #84944 ) ;
#111850 = EDGE_CURVE ( 'NONE', #110456, #39448, #104171, .T. ) ;
#111851 = AXIS2_PLACEMENT_3D ( 'NONE', #74504, #73766, #141147 ) ;
#111852 = CARTESIAN_POINT ( 'NONE',  ( 6.066782984417857350, -9.629649721936179265E-32, 2.500000000000000444 ) ) ;
#111853 = EDGE_CURVE ( 'NONE', #6385, #103176, #34684, .T. ) ;
#111854 = CARTESIAN_POINT ( 'NONE',  ( 42.14626352523143282, -4.472830434245840259, 4.472830434245839371 ) ) ;
#111855 = VECTOR ( 'NONE', #126382, 1000.000000000000000 ) ;
#111856 = ORIENTED_EDGE ( 'NONE', *, *, #104590, .F. ) ;
#111857 = DIRECTION ( 'NONE',  ( 0.3543493200069162685, -0.000000000000000000, -0.9351131265310288487 ) ) ;
#111858 = ORIENTED_EDGE ( 'NONE', *, *, #142705, .F. ) ;
#111859 = ORIENTED_EDGE ( 'NONE', *, *, #18728, .T. ) ;
#111860 = CARTESIAN_POINT ( 'NONE',  ( -34.92500000000001137, -4.662012949885770752, -5.188494296035321973 ) ) ;
#111861 = DIRECTION ( 'NONE',  ( 0.3543493200069163240, 0.000000000000000000, 0.9351131265310288487 ) ) ;
#111862 = CARTESIAN_POINT ( 'NONE',  ( 48.18398860626899705, 28.73617430169820608, 5.000000000000000000 ) ) ;
#111863 = ORIENTED_EDGE ( 'NONE', *, *, #138540, .F. ) ;
#111864 = ADVANCED_FACE ( 'NONE', ( #57173 ), #69466, .F. ) ;
#111865 = CARTESIAN_POINT ( 'NONE',  ( 5.510786437626906675, -27.52281430457051314, 5.000000000000000000 ) ) ;
#111866 = ORIENTED_EDGE ( 'NONE', *, *, #48641, .T. ) ;
#111867 = DIRECTION ( 'NONE',  ( -1.000000000000000000, -0.000000000000000000, 0.000000000000000000 ) ) ;
#111868 = CARTESIAN_POINT ( 'NONE',  ( -23.67183060077630685, -3.740707523384246613, 4.000000000000000000 ) ) ;
#111869 = LINE ( 'NONE', #133622, #96286 ) ;
#111870 = DIRECTION ( 'NONE',  ( -0.6830127018922180770, -0.6830127018922204085, -0.2588190451025213501 ) ) ;
#111871 = CARTESIAN_POINT ( 'NONE',  ( -14.29298673570684919, -21.74070752338405299, 4.999753212805220670 ) ) ;
#111872 = VECTOR ( 'NONE', #139984, 1000.000000000000000 ) ;
#111873 = VERTEX_POINT ( 'NONE', #81780 ) ;
#111874 = AXIS2_PLACEMENT_3D ( 'NONE', #3182, #68487, #33709 ) ;
#111875 = CARTESIAN_POINT ( 'NONE',  ( 51.18398860626899705, 28.73617430169823095, 5.000000000000000000 ) ) ;
#111876 = CARTESIAN_POINT ( 'NONE',  ( 57.22459685856476597, -1.637169565754160949, 6.109999999999997655 ) ) ;
#111877 = PLANE ( 'NONE',  #129815 ) ;
#111878 = PLANE ( 'NONE',  #61679 ) ;
#111879 = DIRECTION ( 'NONE',  ( 0.7071067811865486830, -0.7071067811865464625, -0.000000000000000000 ) ) ;
#111880 = ORIENTED_EDGE ( 'NONE', *, *, #12751, .T. ) ;
#111881 = PLANE ( 'NONE',  #603 ) ;
#111882 = VERTEX_POINT ( 'NONE', #91896 ) ;
#111883 = CARTESIAN_POINT ( 'NONE',  ( 33.03650004940865870, 22.27000000000000668, -14.29932321514968763 ) ) ;
#111884 = B_SPLINE_CURVE_WITH_KNOTS ( 'NONE', 3,
 ( #44159, #107247, #88382, #43433, #63775, #86235, #20947, #18805, #120228, #10768, #33313, #20221, #7921, #52161, #55036, #10072 ),
 .UNSPECIFIED., .F., .F.,
 ( 4, 2, 2, 2, 2, 2, 2, 4 ),
 ( 2.034069612461835805E-16, 0.0009871449549440356516, 0.001974289909887867907, 0.002961434864831699945, 0.003948579819775532851, 0.004935724774719364889, 0.005922869729663196928, 0.007897159639550867943 ),
 .UNSPECIFIED. ) ;
#111885 = ORIENTED_EDGE ( 'NONE', *, *, #100917, .F. ) ;
#111886 = PLANE ( 'NONE',  #9863 ) ;
#111888 = EDGE_CURVE ( 'NONE', #81966, #14111, #112936, .T. ) ;
#111887 = DIRECTION ( 'NONE',  ( 1.000000000000000000, 0.000000000000000000, 0.000000000000000000 ) ) ;
#111889 = LINE ( 'NONE', #24160, #136535 ) ;
#111890 = VECTOR ( 'NONE', #91718, 1000.000000000000000 ) ;
#111891 = ADVANCED_FACE ( 'NONE', ( #125249 ), #70208, .F. ) ;
#111892 = CARTESIAN_POINT ( 'NONE',  ( -15.48921356237309510, -27.52281430457066236, 5.000000000000000000 ) ) ;
#111893 = FACE_BOUND ( 'NONE', #46281, .T. ) ;
#111894 = CARTESIAN_POINT ( 'NONE',  ( 34.17183060077623225, 18.75929247661552068, 4.000000000000000000 ) ) ;
#111895 = ADVANCED_FACE ( 'NONE', ( #114368 ), #15039, .T. ) ;
#111896 = EDGE_CURVE ( 'NONE', #131061, #66262, #71593, .T. ) ;
#111897 = PLANE ( 'NONE',  #44475 ) ;
#111898 = VECTOR ( 'NONE', #20001, 999.9999999999998863 ) ;
#111899 = FACE_OUTER_BOUND ( 'NONE', #130133, .T. ) ;
#111901 = ORIENTED_EDGE ( 'NONE', *, *, #81250, .T. ) ;
#111900 = LINE ( 'NONE', #56841, #13392 ) ;
#111902 = FACE_OUTER_BOUND ( 'NONE', #92627, .T. ) ;
#111903 = ORIENTED_EDGE ( 'NONE', *, *, #131913, .F. ) ;
#111904 = ADVANCED_FACE ( 'NONE', ( #72345 ), #115755, .F. ) ;
#111905 = EDGE_CURVE ( 'NONE', #4663, #113019, #13990, .T. ) ;
#111906 = VERTEX_POINT ( 'NONE', #84610 ) ;
#111907 = CARTESIAN_POINT ( 'NONE',  ( 75.01626352523142316, -4.472830434245838482, 4.472830434245838482 ) ) ;
#111908 = VERTEX_POINT ( 'NONE', #40402 ) ;
#111909 = DIRECTION ( 'NONE',  ( 0.000000000000000000, -1.000000000000000000, 0.000000000000000000 ) ) ;
#111910 = EDGE_CURVE ( 'NONE', #81140, #59816, #127379, .T. ) ;
#111911 = DIRECTION ( 'NONE',  ( 0.7071067811865486830, -0.7071067811865464625, -0.000000000000000000 ) ) ;
#111912 = ADVANCED_FACE ( 'NONE', ( #105604 ), #7727, .T. ) ;
#111913 = ORIENTED_EDGE ( 'NONE', *, *, #77217, .F. ) ;
#111914 = CARTESIAN_POINT ( 'NONE',  ( 0.000000000000000000, 0.000000000000000000, 5.000000000000000000 ) ) ;
#111915 = CIRCLE ( 'NONE', #130440, 0.5000000000000000000 ) ;
#111916 = EDGE_CURVE ( 'NONE', #62052, #21546, #48103, .T. ) ;
#111917 = VECTOR ( 'NONE', #2959, 1000.000000000000000 ) ;
#111918 = LINE ( 'NONE', #22025, #98201 ) ;
#111919 = EDGE_CURVE ( 'NONE', #142250, #28108, #19341, .T. ) ;
#111920 = CARTESIAN_POINT ( 'NONE',  ( -34.49999999999976552, -8.945670655168967755, 4.994342998332164996 ) ) ;
#111921 =( NAMED_UNIT ( * ) SI_UNIT ( $, .STERADIAN. ) SOLID_ANGLE_UNIT ( ) );
#111923 = CARTESIAN_POINT ( 'NONE',  ( -28.49999999999979750, -11.56887692260769640, 4.000000000000000000 ) ) ;
#111922 = CARTESIAN_POINT ( 'NONE',  ( -24.99581563014004715, 3.703558271726549833, 4.317415941188012418 ) ) ;
#111924 = FACE_OUTER_BOUND ( 'NONE', #112875, .T. ) ;
#111925 = LINE ( 'NONE', #36492, #76340 ) ;
#111926 = ORIENTED_EDGE ( 'NONE', *, *, #98195, .F. ) ;
#111927 = AXIS2_PLACEMENT_3D ( 'NONE', #108396, #95421, #84571 ) ;
#111928 = PRODUCT_DEFINITION_FORMATION_WITH_SPECIFIED_SOURCE ( 'ANY', '', #118763, .NOT_KNOWN. ) ;
#111929 = ORIENTED_EDGE ( 'NONE', *, *, #46698, .T. ) ;
#111930 = DIRECTION ( 'NONE',  ( 1.000000000000000000, 1.224606353822377258E-16, 0.000000000000000000 ) ) ;
#111931 = LINE ( 'NONE', #56868, #139260 ) ;
#111932 = EDGE_LOOP ( 'NONE', ( #70770, #53945, #1159, #50397 ) ) ;
#111933 = EDGE_CURVE ( 'NONE', #49793, #78390, #28805, .T. ) ;
#111934 = EDGE_LOOP ( 'NONE', ( #60573, #25017, #141661, #76276 ) ) ;
#111935 = EDGE_LOOP ( 'NONE', ( #22275, #6622, #72956, #104893 ) ) ;
#111936 = CARTESIAN_POINT ( 'NONE',  ( 0.000000000000000000, 0.000000000000000000, 5.000000000000000000 ) ) ;
#111937 = ORIENTED_EDGE ( 'NONE', *, *, #110326, .T. ) ;
#111938 = FACE_OUTER_BOUND ( 'NONE', #59198, .T. ) ;
#111940 = EDGE_CURVE ( 'NONE', #79668, #27936, #30208, .T. ) ;
#111939 = AXIS2_PLACEMENT_3D ( 'NONE', #80018, #24874, #82152 ) ;
#111941 = CARTESIAN_POINT ( 'NONE',  ( 89.03752705046288440, -9.735942053221456900E-16, 7.949999999999998401 ) ) ;
#111942 = AXIS2_PLACEMENT_3D ( 'NONE', #47840, #134842, #80449 ) ;
#111943 = CARTESIAN_POINT ( 'NONE',  ( 29.94163961620377279, -6.094999999999989093, 1.633150327867691765 ) ) ;
#111944 = CARTESIAN_POINT ( 'NONE',  ( 17.06332250466817158, 4.584330080086930965E-16, 0.000000000000000000 ) ) ;
#111945 = ORIENTED_EDGE ( 'NONE', *, *, #114974, .T. ) ;
#111946 = CARTESIAN_POINT ( 'NONE',  ( -5.816011393731002066, 28.73617430169783304, 5.000000000000000000 ) ) ;
#111947 = CARTESIAN_POINT ( 'NONE',  ( 30.48921356237309510, -27.52281430457076894, 5.000000000000000000 ) ) ;
#111948 = DIRECTION ( 'NONE',  ( 0.3543493200069162685, -0.000000000000000000, -0.9351131265310288487 ) ) ;
#111950 = VERTEX_POINT ( 'NONE', #106310 ) ;
#111949 = DIRECTION ( 'NONE',  ( 0.6830127018922181881, 0.6830127018922202975, -0.2588190451025214056 ) ) ;
#111951 = ORIENTED_EDGE ( 'NONE', *, *, #27028, .F. ) ;
#111952 = SURFACE_STYLE_FILL_AREA ( #57583 ) ;
#111953 = DIRECTION ( 'NONE',  ( -0.7071067811865487940, 0.7071067811865463515, -0.000000000000000000 ) ) ;
#111954 = AXIS2_PLACEMENT_3D ( 'NONE', #27218, #104790, #96045 ) ;
#111955 = FACE_OUTER_BOUND ( 'NONE', #95126, .T. ) ;
#111956 = ORIENTED_EDGE ( 'NONE', *, *, #50956, .F. ) ;
#111957 = DIRECTION ( 'NONE',  ( 1.000000000000000000, 0.000000000000000000, 0.000000000000000000 ) ) ;
#111958 = EDGE_CURVE ( 'NONE', #15581, #39740, #74457, .T. ) ;
#111959 = DIRECTION ( 'NONE',  ( 0.7071067811865487940, -0.7071067811865463515, 0.000000000000000000 ) ) ;
#111960 = ORIENTED_EDGE ( 'NONE', *, *, #60446, .F. ) ;
#111961 = CIRCLE ( 'NONE', #68015, 2.500000000000000888 ) ;
#111962 = EDGE_CURVE ( 'NONE', #70329, #45800, #120780, .T. ) ;
#111963 = DIRECTION ( 'NONE',  ( 0.3543493200069162685, -0.000000000000000000, -0.9351131265310288487 ) ) ;
#111964 = CARTESIAN_POINT ( 'NONE',  ( 0.4892135623730947680, -27.52281430457055578, 5.000000000000000000 ) ) ;
#111965 = CARTESIAN_POINT ( 'NONE',  ( 5.999999999999956479, 13.93112307739204425, 4.000000000000000000 ) ) ;
#111966 = CARTESIAN_POINT ( 'NONE',  ( -12.20000000000000107, -34.64999999999999147, 17.99210858042621908 ) ) ;
#111967 = CARTESIAN_POINT ( 'NONE',  ( -48.29974487139158867, -27.71228299555239971, 4.000000000000000000 ) ) ;
#111968 = EDGE_CURVE ( 'NONE', #93963, #95860, #88906, .T. ) ;
#111970 = VECTOR ( 'NONE', #61356, 1000.000000000000000 ) ;
#111969 = CARTESIAN_POINT ( 'NONE',  ( -20.20710678118641113, -17.24070752338409918, 5.000000000000000000 ) ) ;
#111971 = DIRECTION ( 'NONE',  ( 0.7071067811865486830, -0.7071067811865464625, -0.000000000000000000 ) ) ;
#111972 = CARTESIAN_POINT ( 'NONE',  ( 18.85005128541013164, -8.240707523384189770, 17.25253755692243374 ) ) ;
#111973 = ORIENTED_EDGE ( 'NONE', *, *, #63946, .T. ) ;
#111974 = EDGE_LOOP ( 'NONE', ( #76018, #5702, #49590, #33886 ) ) ;
#111975 = CARTESIAN_POINT ( 'NONE',  ( 19.49999999999986144, -17.56887692260763956, 4.000000000000000000 ) ) ;
#111976 = CARTESIAN_POINT ( 'NONE',  ( -28.01987774928530683, -17.24070752338410983, 20.23474786156463168 ) ) ;
#111977 = VECTOR ( 'NONE', #68592, 1000.000000000000000 ) ;
#111978 = CARTESIAN_POINT ( 'NONE',  ( 24.32816939922335919, -0.7407075233842735917, 4.000000000000000000 ) ) ;
#111979 = DIRECTION ( 'NONE',  ( 0.000000000000000000, -0.3543493200069153248, -0.9351131265310291818 ) ) ;
#111981 = EDGE_LOOP ( 'NONE', ( #66287, #69216, #9650 ) ) ;
#111980 = AXIS2_PLACEMENT_3D ( 'NONE', #105828, #94259, #107273 ) ;
#111982 = CARTESIAN_POINT ( 'NONE',  ( -42.48921356237308800, -27.52281430457085065, 5.000000000000000000 ) ) ;
#111983 =( BOUNDED_CURVE ( )  B_SPLINE_CURVE ( 3, ( #135365, #36048, #14266, #88997 ),
 .UNSPECIFIED., .F., .T. ) 
 B_SPLINE_CURVE_WITH_KNOTS ( ( 4, 4 ),
 ( 5.005968288816726286, 5.074607125596334534 ),
 .UNSPECIFIED. ) 
 CURVE ( )  GEOMETRIC_REPRESENTATION_ITEM ( )  RATIONAL_B_SPLINE_CURVE ( ( 1.000000000000000000, 0.9996074310407765395, 0.9996074310407765395, 1.000000000000000000 ) ) 
 REPRESENTATION_ITEM ( '' )  );
#111984 = CARTESIAN_POINT ( 'NONE',  ( 11.99451991528749417, 28.92564299267946382, 4.000000000000000000 ) ) ;
#111985 = VERTEX_POINT ( 'NONE', #20030 ) ;
#111986 = ADVANCED_FACE ( 'NONE', ( #130977 ), #143257, .T. ) ;
#111987 = CARTESIAN_POINT ( 'NONE',  ( -8.510786437626906675, -27.52281430457049183, 5.000000000000000000 ) ) ;
#111988 = CARTESIAN_POINT ( 'NONE',  ( 6.183988606268994381, 28.73617430169791476, 5.000000000000000000 ) ) ;
#111989 = CARTESIAN_POINT ( 'NONE',  ( 2.293876922608031332, 22.22500000000000142, 4.000000000000000000 ) ) ;
#111990 = STYLED_ITEM ( 'NONE', ( #67275 ), #32540 ) ;
#111991 = SURFACE_STYLE_USAGE ( .BOTH. , #67800 ) ;
#111992 = CARTESIAN_POINT ( 'NONE',  ( 52.41209685856478018, 5.291415217122922066, -3.054999999999995275 ) ) ;
#111993 = FACE_OUTER_BOUND ( 'NONE', #10375, .T. ) ;
#111994 = SURFACE_STYLE_USAGE ( .BOTH. , #67804 ) ;
#111995 = LINE ( 'NONE', #115314, #72001 ) ;
#111996 = EDGE_CURVE ( 'NONE', #79129, #131121, #99747, .T. ) ;
#111997 = EDGE_LOOP ( 'NONE', ( #98282, #110192, #43414, #129882 ) ) ;
#111998 = PLANE ( 'NONE',  #65086 ) ;
#111999 = VERTEX_POINT ( 'NONE', #98341 ) ;
#112000 = MECHANICAL_DESIGN_GEOMETRIC_PRESENTATION_REPRESENTATION (  '', ( #77250 ), #77354 ) ;
#112001 = DIRECTION ( 'NONE',  ( -0.7071067811865486830, -0.7071067811865464625, -0.000000000000000000 ) ) ;
#112002 = DIRECTION ( 'NONE',  ( -0.7071067811865486830, 0.7071067811865464625, 0.000000000000000000 ) ) ;
#112003 = LINE ( 'NONE', #80800, #18764 ) ;
#112004 =( NAMED_UNIT ( * ) PLANE_ANGLE_UNIT ( ) SI_UNIT ( $, .RADIAN. ) );
#112005 = ADVANCED_FACE ( 'NONE', ( #86026 ), #64276, .F. ) ;
#112006 = LINE ( 'NONE', #56924, #74242 ) ;
#112007 = CARTESIAN_POINT ( 'NONE',  ( -0.1839886062690032631, 28.73617430169787568, 5.000000000000000000 ) ) ;
#112008 = VERTEX_POINT ( 'NONE', #41811 ) ;
#112010 = ORIENTED_EDGE ( 'NONE', *, *, #16544, .F. ) ;
#112009 = AXIS2_PLACEMENT_3D ( 'NONE', #128971, #118804, #115924 ) ;
#112011 = CARTESIAN_POINT ( 'NONE',  ( 34.92499999999998295, 22.22500000000000142, 4.500000000000000888 ) ) ;
#112012 = CARTESIAN_POINT ( 'NONE',  ( 2.999999999999999112, -43.14999999999999147, 34.92499999999998295 ) ) ;
#112013 = CARTESIAN_POINT ( 'NONE',  ( 32.99451991528749062, 28.92564299267960948, 4.000000000000000000 ) ) ;
#112014 = CARTESIAN_POINT ( 'NONE',  ( -47.99451991528749062, 28.92564299267971251, 4.000000000000000000 ) ) ;
#112015 = CARTESIAN_POINT ( 'NONE',  ( 76.64169371712954160, -2.130196079827424871, -7.949999999999999289 ) ) ;
#112016 = DIRECTION ( 'NONE',  ( -0.6830127018922180770, -0.6830127018922204085, -0.2588190451025213501 ) ) ;
#112017 = VECTOR ( 'NONE', #61497, 999.9999999999998863 ) ;
#112018 = CARTESIAN_POINT ( 'NONE',  ( -7.171830600776425868, -8.240707523384207533, 4.000000000000000000 ) ) ;
#112019 = ORIENTED_EDGE ( 'NONE', *, *, #122457, .T. ) ;
#112020 = CARTESIAN_POINT ( 'NONE',  ( 76.97916666666665719, -7.950000000000001066, 2.130196079827424427 ) ) ;
#112021 = DIRECTION ( 'NONE',  ( 0.5735764363510448272, -0.8191520442889927978, 1.003171929053526103E-16 ) ) ;
#112022 = DIRECTION ( 'NONE',  ( -0.7071067811865486830, -0.7071067811865464625, 0.000000000000000000 ) ) ;
#112023 = LINE ( 'NONE', #76547, #121466 ) ;
#112024 = ORIENTED_EDGE ( 'NONE', *, *, #41035, .F. ) ;
#112026 = ADVANCED_FACE ( 'NONE', ( #108443 ), #20218, .T. ) ;
#112025 = CIRCLE ( 'NONE', #24053, 2.500000000000000000 ) ;
#112027 = DIRECTION ( 'NONE',  ( -0.3543493200069162685, -0.000000000000000000, -0.9351131265310288487 ) ) ;
#112028 = EDGE_CURVE ( 'NONE', #44279, #52361, #67136, .T. ) ;
#112029 = LINE ( 'NONE', #68536, #86025 ) ;
#112030 = CARTESIAN_POINT ( 'NONE',  ( 67.52126352523141861, -4.472830434245839371, -4.472830434245840259 ) ) ;
#112031 = ORIENTED_EDGE ( 'NONE', *, *, #61401, .F. ) ;
#112032 = ORIENTED_EDGE ( 'NONE', *, *, #35864, .T. ) ;
#112033 = DIRECTION ( 'NONE',  ( 0.7071067811865487940, 0.7071067811865463515, 0.000000000000000000 ) ) ;
#112034 = DIRECTION ( 'NONE',  ( 1.000000000000000000, 1.224606353822377258E-16, 0.000000000000000000 ) ) ;
#112035 = CARTESIAN_POINT ( 'NONE',  ( 44.60416666666665719, 2.130196079827422206, 7.950000000000001954 ) ) ;
#112036 = EDGE_CURVE ( 'NONE', #57693, #89225, #88177, .T. ) ;
#112037 = PLANE ( 'NONE',  #122928 ) ;
#112039 = VERTEX_POINT ( 'NONE', #414 ) ;
#112038 = LINE ( 'NONE', #67852, #5915 ) ;
#112040 = CARTESIAN_POINT ( 'NONE',  ( 18.63999999999999702, 9.521314400968980422E-16, 0.000000000000000000 ) ) ;
#112041 = CARTESIAN_POINT ( 'NONE',  ( -7.171830600776411657, 6.759292476615649470, 4.000000000000000000 ) ) ;
#112042 = CARTESIAN_POINT ( 'NONE',  ( 3.183988606268992161, 28.73617430169789699, 5.000000000000000000 ) ) ;
#112043 = VECTOR ( 'NONE', #133841, 1000.000000000000000 ) ;
#112044 = ORIENTED_EDGE ( 'NONE', *, *, #45338, .T. ) ;
#112045 = VERTEX_POINT ( 'NONE', #130265 ) ;
#112046 = CARTESIAN_POINT ( 'NONE',  ( 57.02126352523143993, -4.472830434245839371, -4.472830434245840259 ) ) ;
#112047 = VECTOR ( 'NONE', #132895, 1000.000000000000000 ) ;
#112048 = ORIENTED_EDGE ( 'NONE', *, *, #85641, .T. ) ;
#112049 = DIRECTION ( 'NONE',  ( 1.000000000000000000, 0.000000000000000000, 0.000000000000000000 ) ) ;
#112050 = CARTESIAN_POINT ( 'NONE',  ( 12.29974487139158512, -27.71228299555214747, 4.000000000000000000 ) ) ;
#112051 = CARTESIAN_POINT ( 'NONE',  ( -31.92499999999997584, -3.270000000000012452, -36.39086428169088094 ) ) ;
#112052 = CARTESIAN_POINT ( 'NONE',  ( 0.000000000000000000, 0.000000000000000000, 5.000000000000000000 ) ) ;
#112053 = CARTESIAN_POINT ( 'NONE',  ( -33.79333936457824450, 21.75929247661549581, 4.998822639870701856 ) ) ;
#112054 = ORIENTED_EDGE ( 'NONE', *, *, #15291, .F. ) ;
#112055 = VERTEX_POINT ( 'NONE', #131681 ) ;
#112056 = CARTESIAN_POINT ( 'NONE',  ( -17.70822291016941463, -15.74070752338411694, 19.73771281079093143 ) ) ;
#112057 =( LENGTH_UNIT ( ) NAMED_UNIT ( * ) SI_UNIT ( .MILLI., .METRE. ) );
#112058 = VECTOR ( 'NONE', #45817, 999.9999999999998863 ) ;
#112059 = VERTEX_POINT ( 'NONE', #132430 ) ;
#112060 = VECTOR ( 'NONE', #55257, 1000.000000000000227 ) ;
#112061 = DIRECTION ( 'NONE',  ( -0.3543493200069162685, -0.000000000000000000, -0.9351131265310288487 ) ) ;
#112062 = EDGE_CURVE ( 'NONE', #16561, #59489, #33119, .T. ) ;
#112063 = CARTESIAN_POINT ( 'NONE',  ( 112.0791937171295558, 3.975000000000002753, -6.884901960086283523 ) ) ;
#112064 = DIRECTION ( 'NONE',  ( 0.6830127018922181881, 0.6830127018922202975, -0.2588190451025214056 ) ) ;
#112065 = EDGE_LOOP ( 'NONE', ( #121720, #12437, #72510, #40154 ) ) ;
#112066 = AXIS2_PLACEMENT_3D ( 'NONE', #28269, #72530, #17375 ) ;
#112067 = STYLED_ITEM ( 'NONE', ( #125505 ), #45918 ) ;
#112068 = FACE_BOUND ( 'NONE', #38840, .T. ) ;
#112069 = CARTESIAN_POINT ( 'NONE',  ( -15.88837638105231775, 9.759292476615614831, 17.35367589129216270 ) ) ;
#112070 = CARTESIAN_POINT ( 'NONE',  ( 3.489213562373097322, -27.52281430457057709, 5.000000000000000000 ) ) ;
#112071 = DIRECTION ( 'NONE',  ( 0.000000000000000000, 0.000000000000000000, 1.000000000000000000 ) ) ;
#112072 = LINE ( 'NONE', #46114, #45743 ) ;
#112073 = VECTOR ( 'NONE', #132632, 1000.000000000000000 ) ;
#112074 = LINE ( 'NONE', #22870, #7202 ) ;
#112075 = DIRECTION ( 'NONE',  ( 0.000000000000000000, 1.000000000000000000, 0.000000000000000000 ) ) ;
#112076 = VERTEX_POINT ( 'NONE', #44715 ) ;
#112077 = EDGE_CURVE ( 'NONE', #108713, #9196, #32365, .T. ) ;
#112078 = ORIENTED_EDGE ( 'NONE', *, *, #50710, .F. ) ;
#112079 = CARTESIAN_POINT ( 'NONE',  ( 104.1829301918981088, -1.637169565754158951, -6.109999999999998543 ) ) ;
#112080 = ORIENTED_EDGE ( 'NONE', *, *, #4499, .F. ) ;
#112081 = ADVANCED_FACE ( 'NONE', ( #96856 ), #66620, .T. ) ;
#112082 = CARTESIAN_POINT ( 'NONE',  ( -23.99451991528749062, 28.92564299267954908, 4.000000000000000000 ) ) ;
#112083 = ORIENTED_EDGE ( 'NONE', *, *, #15862, .T. ) ;
#112084 = EDGE_CURVE ( 'NONE', #128697, #103370, #77329, .T. ) ;
#112085 = CONICAL_SURFACE ( 'NONE', #49605, 8.094999999999991758, 0.7853981633974466137 ) ;
#112086 = LINE ( 'NONE', #101184, #16875 ) ;
#112087 = EDGE_CURVE ( 'NONE', #140745, #114242, #14877, .T. ) ;
#112088 = PLANE ( 'NONE',  #43239 ) ;
#112089 = VECTOR ( 'NONE', #31498, 1000.000000000000227 ) ;
#112090 = LINE ( 'NONE', #1142, #81887 ) ;
#112091 = ORIENTED_EDGE ( 'NONE', *, *, #78375, .T. ) ;
#112092 = CARTESIAN_POINT ( 'NONE',  ( -4.499999999999968914, 13.08746187583912146, 4.000000000000000000 ) ) ;
#112093 = FACE_OUTER_BOUND ( 'NONE', #9194, .T. ) ;
#112094 = PRESENTATION_STYLE_ASSIGNMENT (( #67908 ) ) ;
#112095 = ADVANCED_FACE ( 'NONE', ( #79487 ), #48226, .T. ) ;
#112096 =( NAMED_UNIT ( * ) PLANE_ANGLE_UNIT ( ) SI_UNIT ( $, .RADIAN. ) );
#112098 = CARTESIAN_POINT ( 'NONE',  ( 34.42499999999998295, 11.97718569542927014, 5.000000000000000000 ) ) ;
#112097 = CARTESIAN_POINT ( 'NONE',  ( 67.93750000000000000, 5.819803920172574863, -5.819803920172573086 ) ) ;
#112099 = CARTESIAN_POINT ( 'NONE',  ( 27.81246187583927565, -22.22500000000000142, 4.000000000000000000 ) ) ;
#112100 = TOROIDAL_SURFACE ( 'NONE', #119007, 3.500000000000000000, 0.5000000000000000000 ) ;
#112101 = CARTESIAN_POINT ( 'NONE',  ( 23.00840764549667483, 2.500000000000003553, 3.061616997868386099E-16 ) ) ;
#112102 = ORIENTED_EDGE ( 'NONE', *, *, #132480, .F. ) ;
#112103 = LINE ( 'NONE', #56328, #49558 ) ;
#112104 = CYLINDRICAL_SURFACE ( 'NONE', #108993, 2.500000000000000444 ) ;
#112105 = EDGE_CURVE ( 'NONE', #120482, #39654, #90295, .T. ) ;
#112106 = ORIENTED_EDGE ( 'NONE', *, *, #55511, .T. ) ;
#112107 = VERTEX_POINT ( 'NONE', #135270 ) ;
#112108 = EDGE_CURVE ( 'NONE', #46507, #118828, #56300, .T. ) ;
#112109 = ORIENTED_EDGE ( 'NONE', *, *, #137310, .T. ) ;
#112110 = CARTESIAN_POINT ( 'NONE',  ( 55.70876352523143282, -7.482591942790329030E-16, 6.110000000000001208 ) ) ;
#112111 = EDGE_LOOP ( 'NONE', ( #49374, #70085, #59591, #19518 ) ) ;
#112112 = ADVANCED_FACE ( 'NONE', ( #100482 ), #3277, .F. ) ;
#112113 = CYLINDRICAL_SURFACE ( 'NONE', #35090, 0.5000000000000004441 ) ;
#112114 = CARTESIAN_POINT ( 'NONE',  ( 10.98330628287044064, 6.094999999999991758, 1.633150327867687102 ) ) ;
#112115 = CARTESIAN_POINT ( 'NONE',  ( 89.54209685856477563, 5.291415217122923842, -3.054999999999996163 ) ) ;
#112116 = CARTESIAN_POINT ( 'NONE',  ( -34.49999999999975131, 19.46425560840030400, 4.994342998332171213 ) ) ;
#112117 = EDGE_LOOP ( 'NONE', ( #6405, #30735, #90881, #59031 ) ) ;
#112118 = ORIENTED_EDGE ( 'NONE', *, *, #15404, .F. ) ;
#112119 = PLANE ( 'NONE',  #108889 ) ;
#112120 = DIRECTION ( 'NONE',  ( 0.000000000000000000, 2.921639538487157626E-15, -1.000000000000000000 ) ) ;
#112121 = VERTEX_POINT ( 'NONE', #37362 ) ;
#112122 = PRESENTATION_LAYER_ASSIGNMENT (  '', '', ( #72841 ) ) ;
#112123 = CARTESIAN_POINT ( 'NONE',  ( -6.640000000000001457, -34.64999999999999147, -40.00000000000000000 ) ) ;
#112124 = DIRECTION ( 'NONE',  ( 0.6830127018922181881, 0.6830127018922202975, -0.2588190451025214056 ) ) ;
#112125 = CARTESIAN_POINT ( 'NONE',  ( 3.005480084712505828, 28.92564299267936079, 4.000000000000000000 ) ) ;
#112126 = ORIENTED_EDGE ( 'NONE', *, *, #108525, .F. ) ;
#112127 = DIRECTION ( 'NONE',  ( -0.3543493200069162685, -0.000000000000000000, -0.9351131265310288487 ) ) ;
#112128 = ORIENTED_EDGE ( 'NONE', *, *, #109148, .F. ) ;
#112129 = ORIENTED_EDGE ( 'NONE', *, *, #121194, .F. ) ;
#112130 = ORIENTED_EDGE ( 'NONE', *, *, #108416, .F. ) ;
#112131 = EDGE_CURVE ( 'NONE', #137290, #86612, #112072, .T. ) ;
#112132 = DIRECTION ( 'NONE',  ( -0.7071067811865486830, -0.7071067811865464625, 0.000000000000000000 ) ) ;
#112133 = CARTESIAN_POINT ( 'NONE',  ( -15.29974487139158867, -27.71228299555216879, 4.000000000000000000 ) ) ;
#112134 = CARTESIAN_POINT ( 'NONE',  ( -26.70822291016936134, -15.74070752338412404, 19.73771281079091366 ) ) ;
#112135 = DIRECTION ( 'NONE',  ( 1.000000000000000000, 0.000000000000000000, 0.000000000000000000 ) ) ;
#112136 = B_SPLINE_CURVE_WITH_KNOTS ( 'NONE', 3,
 ( #6345, #86829, #117971, #107126 ),
 .UNSPECIFIED., .F., .F.,
 ( 4, 4 ),
 ( 0.008851590069444708123, 0.009100162336955337078 ),
 .UNSPECIFIED. ) ;
#112137 = LINE ( 'NONE', #12786, #48879 ) ;
#112138 = ORIENTED_EDGE ( 'NONE', *, *, #59166, .F. ) ;
#112139 = AXIS2_PLACEMENT_3D ( 'NONE', #11675, #34190, #109594 ) ;
#112140 = DIRECTION ( 'NONE',  ( -0.7071067811865486830, 0.7071067811865464625, 0.000000000000000000 ) ) ;
#112141 = EDGE_CURVE ( 'NONE', #21912, #50218, #47567, .T. ) ;
#112142 = AXIS2_PLACEMENT_3D ( 'NONE', #133422, #87761, #725 ) ;
#112143 = CARTESIAN_POINT ( 'NONE',  ( 20.39540314143521726, 2.126176841940962348, 7.934999999999989839 ) ) ;
#112144 = LINE ( 'NONE', #22935, #16162 ) ;
#112145 = CARTESIAN_POINT ( 'NONE',  ( 13.49999999999990763, -20.56887692260759337, 4.000000000000000000 ) ) ;
#112146 = LINE ( 'NONE', #36023, #81418 ) ;
#112147 = ORIENTED_EDGE ( 'NONE', *, *, #99933, .F. ) ;
#112148 = VECTOR ( 'NONE', #4771, 1000.000000000000000 ) ;
#112149 = VERTEX_POINT ( 'NONE', #81598 ) ;
#112150 = ADVANCED_FACE ( 'NONE', ( #26478 ), #12013, .F. ) ;
#112151 = ORIENTED_EDGE ( 'NONE', *, *, #105519, .T. ) ;
#112152 = CARTESIAN_POINT ( 'NONE',  ( -10.49999999999991651, 4.087461875839196956, 4.000000000000000000 ) ) ;
#112153 = DIRECTION ( 'NONE',  ( 0.7071067811865486830, -0.7071067811865464625, -0.000000000000000000 ) ) ;
#112154 = DIRECTION ( 'NONE',  ( 0.7071067811865487940, 0.7071067811865463515, -0.000000000000000000 ) ) ;
#112155 = DIRECTION ( 'NONE',  ( 0.000000000000000000, 1.000000000000000000, 0.000000000000000000 ) ) ;
#112156 = CARTESIAN_POINT ( 'NONE',  ( 5.950172325297302223, 9.499920639676602718, 0.2930115638150264101 ) ) ;
#112157 = CARTESIAN_POINT ( 'NONE',  ( -18.18398860626898994, 28.73617430169800002, 5.000000000000000000 ) ) ;
#112158 = VECTOR ( 'NONE', #40481, 999.9999999999998863 ) ;
#112159 = CARTESIAN_POINT ( 'NONE',  ( 128.5894344200537489, -49.14999999999999147, 39.86617647058822911 ) ) ;
#112160 = ADVANCED_FACE ( 'NONE', ( #34500 ), #78725, .T. ) ;
#112161 = CARTESIAN_POINT ( 'NONE',  ( 30.48921356237309510, -27.52281430457076894, 5.000000000000000000 ) ) ;
#112162 = CARTESIAN_POINT ( 'NONE',  ( -16.36246187583889622, 22.22500000000000853, 4.000000000000000000 ) ) ;
#112163 = ORIENTED_EDGE ( 'NONE', *, *, #29195, .F. ) ;
#112164 = CARTESIAN_POINT ( 'NONE',  ( -30.32816939922331656, -9.740707523384182664, 4.000000000000000000 ) ) ;
#112165 = EDGE_LOOP ( 'NONE', ( #6802, #140409, #107884, #16514 ) ) ;
#112166 = SURFACE_STYLE_FILL_AREA ( #35336 ) ;
#112167 = VERTEX_POINT ( 'NONE', #56996 ) ;
#112168 = CARTESIAN_POINT ( 'NONE',  ( 16.96247294953710849, -7.464222240803106570E-16, -6.094999999999989981 ) ) ;
#112170 = ORIENTED_EDGE ( 'NONE', *, *, #39835, .T. ) ;
#112169 = CARTESIAN_POINT ( 'NONE',  ( -19.05000000000000071, 3.174999999999997158, 4.000000000000000000 ) ) ;
#112171 = CIRCLE ( 'NONE', #49682, 2.500000000000000444 ) ;
#112172 = EDGE_CURVE ( 'NONE', #134224, #77753, #101170, .T. ) ;
#112173 = PRESENTATION_STYLE_ASSIGNMENT (( #1913 ) ) ;
#112174 = DIRECTION ( 'NONE',  ( 1.000000000000000000, 0.000000000000000000, 0.000000000000000000 ) ) ;
#112175 = ORIENTED_EDGE ( 'NONE', *, *, #105470, .T. ) ;
#112176 = FACE_OUTER_BOUND ( 'NONE', #24792, .T. ) ;
#112177 = EDGE_LOOP ( 'NONE', ( #111658, #5415, #140876, #44919 ) ) ;
#112178 = DIRECTION ( 'NONE',  ( 0.7071067811865486830, -0.7071067811865464625, -0.000000000000000000 ) ) ;
#112179 = EDGE_LOOP ( 'NONE', ( #143548, #15197, #23858, #23898 ) ) ;
#112180 = VECTOR ( 'NONE', #28835, 1000.000000000000000 ) ;
#112181 = DIRECTION ( 'NONE',  ( 0.3543493200069162685, -0.000000000000000000, -0.9351131265310288487 ) ) ;
#112182 = CARTESIAN_POINT ( 'NONE',  ( 101.2875270504628986, 0.000000000000000000, -7.949999999999998401 ) ) ;
#112184 = AXIS2_PLACEMENT_3D ( 'NONE', #47044, #112243, #33292 ) ;
#112183 =( NAMED_UNIT ( * ) PLANE_ANGLE_UNIT ( ) SI_UNIT ( $, .RADIAN. ) );
#112185 = DIRECTION ( 'NONE',  ( 0.000000000000000000, -1.000000000000000000, 0.000000000000000000 ) ) ;
#112186 = ORIENTED_EDGE ( 'NONE', *, *, #82166, .T. ) ;
#112187 = LINE ( 'NONE', #32477, #116219 ) ;
#112188 = CARTESIAN_POINT ( 'NONE',  ( 4.499999999999968914, -16.53360074219757081, 5.000000000000000000 ) ) ;
#112189 = FACE_OUTER_BOUND ( 'NONE', #15379, .T. ) ;
#112190 = CARTESIAN_POINT ( 'NONE',  ( 10.20833333333333570, 3.047499999999997655, 5.278424836066143655 ) ) ;
#112191 = PLANE ( 'NONE',  #46861 ) ;
#112192 = CYLINDRICAL_SURFACE ( 'NONE', #139411, 2.500000000000000444 ) ;
#112193 = CARTESIAN_POINT ( 'NONE',  ( 12.00548008471251293, 28.92564299267929684, 4.000000000000000000 ) ) ;
#112194 = ORIENTED_EDGE ( 'NONE', *, *, #132032, .T. ) ;
#112195 = ORIENTED_EDGE ( 'NONE', *, *, #20898, .F. ) ;
#112196 = DIRECTION ( 'NONE',  ( 0.7071067811865486830, -0.7071067811865464625, -0.000000000000000000 ) ) ;
#112197 = EDGE_LOOP ( 'NONE', ( #23385, #101814, #57046, #113341 ) ) ;
#112198 = EDGE_CURVE ( 'NONE', #123070, #101563, #35244, .T. ) ;
#112199 = CARTESIAN_POINT ( 'NONE',  ( 93.47959685856474721, 6.109999999999999432, 1.637169565754164280 ) ) ;
#112200 = CARTESIAN_POINT ( 'NONE',  ( 0.000000000000000000, 0.000000000000000000, 5.000000000000000000 ) ) ;
#112201 = PLANE ( 'NONE',  #33111 ) ;
#112202 = CARTESIAN_POINT ( 'NONE',  ( 128.0580420323230157, -46.73296206246060791, -36.09967824800569502 ) ) ;
#112203 = ORIENTED_EDGE ( 'NONE', *, *, #2753, .F. ) ;
#112204 = FACE_OUTER_BOUND ( 'NONE', #51667, .T. ) ;
#112205 = CARTESIAN_POINT ( 'NONE',  ( 16.27785539607886633, 4.584330080086930965E-16, 0.000000000000000000 ) ) ;
#112206 = EDGE_CURVE ( 'NONE', #131140, #90151, #123679, .T. ) ;
#112207 = ORIENTED_EDGE ( 'NONE', *, *, #36894, .F. ) ;
#112208 = CARTESIAN_POINT ( 'NONE',  ( -25.39999999999996305, 3.061616997868383141E-16, -2.500000000000000000 ) ) ;
#112209 = EDGE_CURVE ( 'NONE', #29743, #77065, #125070, .T. ) ;
#112210 = CARTESIAN_POINT ( 'NONE',  ( 39.18398860626899705, 28.73617430169814568, 5.000000000000000000 ) ) ;
#112212 = ORIENTED_EDGE ( 'NONE', *, *, #93613, .F. ) ;
#112211 = DIRECTION ( 'NONE',  ( -1.000000000000000000, -1.224606353822377258E-16, -0.000000000000000000 ) ) ;
#112213 = DIRECTION ( 'NONE',  ( -0.7071067811865487940, 0.7071067811865463515, 0.000000000000000000 ) ) ;
#112214 = FACE_OUTER_BOUND ( 'NONE', #142701, .T. ) ;
#112215 = CARTESIAN_POINT ( 'NONE',  ( 0.1161069444170879233, 0.4000000000000001332, -2.220360628129161462 ) ) ;
#112216 = DIRECTION ( 'NONE',  ( 0.6830127018922180770, -0.6830127018922204085, -0.2588190451025213501 ) ) ;
#112217 = VERTEX_POINT ( 'NONE', #57706 ) ;
#112218 = ORIENTED_EDGE ( 'NONE', *, *, #137302, .F. ) ;
#112219 = ORIENTED_EDGE ( 'NONE', *, *, #89012, .F. ) ;
#112220 = CARTESIAN_POINT ( 'NONE',  ( 79.33376352523144703, 6.110000000000001208, 1.122388791418549305E-15 ) ) ;
#112221 = ORIENTED_EDGE ( 'NONE', *, *, #133227, .T. ) ;
#112222 = PLANE ( 'NONE',  #92593 ) ;
#112223 = CARTESIAN_POINT ( 'NONE',  ( -12.32816939922344268, 20.25929247661551713, 4.000000000000000000 ) ) ;
#112224 = PLANE ( 'NONE',  #133694 ) ;
#112225 = CARTESIAN_POINT ( 'NONE',  ( 18.32840764549667512, -2.499999999999996003, 0.000000000000000000 ) ) ;
#112226 = ORIENTED_EDGE ( 'NONE', *, *, #22857, .F. ) ;
#112227 = EDGE_CURVE ( 'NONE', #95905, #51588, #13289, .T. ) ;
#112228 = CARTESIAN_POINT ( 'NONE',  ( -11.99999999999992006, 8.587461875839165870, 4.000000000000000000 ) ) ;
#112230 = CIRCLE ( 'NONE', #49736, 2.055000000000001048 ) ;
#112229 = DIRECTION ( 'NONE',  ( 0.7071067811865487940, 0.7071067811865463515, -0.000000000000000000 ) ) ;
#112231 = CARTESIAN_POINT ( 'NONE',  ( -5.816011393731002066, 28.73617430169783304, 5.000000000000000000 ) ) ;
#112232 = CARTESIAN_POINT ( 'NONE',  ( 83.62043019189812298, 3.055000000000001936, -5.291415217122916737 ) ) ;
#112233 = EDGE_LOOP ( 'NONE', ( #112774, #98188, #37344, #21541 ) ) ;
#112234 = CARTESIAN_POINT ( 'NONE',  ( -44.99451991528749772, 28.92564299267969474, 4.000000000000000000 ) ) ;
#112235 = DIRECTION ( 'NONE',  ( -0.7071067811865487940, 0.7071067811865463515, 0.000000000000000000 ) ) ;
#112236 = ORIENTED_EDGE ( 'NONE', *, *, #80541, .F. ) ;
#112237 = ORIENTED_EDGE ( 'NONE', *, *, #110295, .F. ) ;
#112238 = CARTESIAN_POINT ( 'NONE',  ( 12.19999999999999574, 0.000000000000000000, -40.00000000000000000 ) ) ;
#112239 = PRESENTATION_STYLE_ASSIGNMENT (( #103467 ) ) ;
#112240 = CARTESIAN_POINT ( 'NONE',  ( 22.52540314143522338, 2.126176841940962348, 7.934999999999988951 ) ) ;
#112241 = CARTESIAN_POINT ( 'NONE',  ( -5.671830600776431197, -0.7407075233842770334, 4.000000000000000000 ) ) ;
#112242 = LINE ( 'NONE', #58630, #60344 ) ;
#112243 = DIRECTION ( 'NONE',  ( -1.000000000000000000, -0.000000000000000000, -0.000000000000000000 ) ) ;
#112244 = VECTOR ( 'NONE', #105224, 1000.000000000000000 ) ;
#112245 = EDGE_CURVE ( 'NONE', #46125, #32348, #61977, .T. ) ;
#112246 = ORIENTED_EDGE ( 'NONE', *, *, #21487, .F. ) ;
#112247 = ORIENTED_EDGE ( 'NONE', *, *, #19814, .T. ) ;
#112248 = EDGE_CURVE ( 'NONE', #97043, #93479, #95293, .T. ) ;
#112249 = CIRCLE ( 'NONE', #49763, 2.500000000000000888 ) ;
#112250 = CARTESIAN_POINT ( 'NONE',  ( 6.628407645496676714, 2.500000000000003553, 3.061616997868386099E-16 ) ) ;
#112251 = ORIENTED_EDGE ( 'NONE', *, *, #94425, .F. ) ;
#112252 = ORIENTED_EDGE ( 'NONE', *, *, #128583, .F. ) ;
#112253 = EDGE_CURVE ( 'NONE', #129025, #18833, #106138, .T. ) ;
#112254 = ADVANCED_FACE ( 'NONE', ( #29318 ), #82304, .F. ) ;
#112255 =( BOUNDED_CURVE ( )  B_SPLINE_CURVE ( 3, ( #17171, #49827, #93299, #94699 ),
 .UNSPECIFIED., .F., .F. ) 
 B_SPLINE_CURVE_WITH_KNOTS ( ( 4, 4 ),
 ( 4.767201131347619025, 4.812229608965456151 ),
 .UNSPECIFIED. ) 
 CURVE ( )  GEOMETRIC_REPRESENTATION_ITEM ( )  RATIONAL_B_SPLINE_CURVE ( ( 1.000000000000000000, 0.9998310434873430852, 0.9998310434873430852, 1.000000000000000000 ) ) 
 REPRESENTATION_ITEM ( '' )  );
#112256 = CARTESIAN_POINT ( 'NONE',  ( 51.18398860626899705, 28.73617430169823095, 5.000000000000000000 ) ) ;
#112257 = ORIENTED_EDGE ( 'NONE', *, *, #1682, .F. ) ;
#112258 = CIRCLE ( 'NONE', #54436, 2.500000000000000444 ) ;
#112259 = LINE ( 'NONE', #111526, #50559 ) ;
#112260 = CARTESIAN_POINT ( 'NONE',  ( 34.92499999999998295, -21.72500000000000142, 4.500000000000000888 ) ) ;
#112261 = CARTESIAN_POINT ( 'NONE',  ( 8.968407645496675684, -2.499999999999998224, 0.000000000000000000 ) ) ;
#112262 =( BOUNDED_CURVE ( )  B_SPLINE_CURVE ( 3, ( #24134, #66927, #35033, #13224 ),
 .UNSPECIFIED., .F., .T. ) 
 B_SPLINE_CURVE_WITH_KNOTS ( ( 4, 4 ),
 ( 3.101920907804234684, 3.199716232068803734 ),
 .UNSPECIFIED. ) 
 CURVE ( )  GEOMETRIC_REPRESENTATION_ITEM ( )  RATIONAL_B_SPLINE_CURVE ( ( 1.000000000000000000, 0.9992031649997841214, 0.9992031649997841214, 1.000000000000000000 ) ) 
 REPRESENTATION_ITEM ( '' )  );
#112263 = CARTESIAN_POINT ( 'NONE',  ( -6.299744871391586898, -27.71228299555210484, 4.000000000000000000 ) ) ;
#112264 = ORIENTED_EDGE ( 'NONE', *, *, #18426, .F. ) ;
#112265 = DIRECTION ( 'NONE',  ( 0.3543493200069163240, 0.000000000000000000, -0.9351131265310288487 ) ) ;
#112266 = EDGE_CURVE ( 'NONE', #68252, #64405, #27176, .T. ) ;
#112267 = ORIENTED_EDGE ( 'NONE', *, *, #120626, .F. ) ;
#112268 = DIRECTION ( 'NONE',  ( 1.055184596092948005E-16, -1.000000000000000000, 0.000000000000000000 ) ) ;
#112269 = ORIENTED_EDGE ( 'NONE', *, *, #76253, .F. ) ;
#112270 = DIRECTION ( 'NONE',  ( -0.3543493200069162685, -0.000000000000000000, -0.9351131265310288487 ) ) ;
#112271 = EDGE_CURVE ( 'NONE', #82619, #42670, #71421, .T. ) ;
#112272 = EDGE_LOOP ( 'NONE', ( #56970, #59454 ) ) ;
#112273 = DIRECTION ( 'NONE',  ( 1.000000000000000000, 0.000000000000000000, 0.000000000000000000 ) ) ;
#112274 = ORIENTED_EDGE ( 'NONE', *, *, #105216, .F. ) ;
#112275 = VERTEX_POINT ( 'NONE', #17710 ) ;
#112276 = ORIENTED_EDGE ( 'NONE', *, *, #122617, .F. ) ;
#112277 = EDGE_CURVE ( 'NONE', #88210, #120409, #83748, .T. ) ;
#112278 = AXIS2_PLACEMENT_3D ( 'NONE', #142857, #43544, #54450 ) ;
#112279 = DIRECTION ( 'NONE',  ( -1.000000000000000000, -1.224606353822377258E-16, -0.000000000000000000 ) ) ;
#112280 = VECTOR ( 'NONE', #137264, 1000.000000000000000 ) ;
#112281 = VECTOR ( 'NONE', #129842, 1000.000000000000227 ) ;
#112282 = CARTESIAN_POINT ( 'NONE',  ( 25.49999999999982947, -4.912538124160710673, 4.000000000000000000 ) ) ;
#112283 = CARTESIAN_POINT ( 'NONE',  ( 14.99451991528749595, 28.92564299267948513, 4.000000000000000000 ) ) ;
#112284 = CARTESIAN_POINT ( 'NONE',  ( 114.0420968585647898, 5.291415217122923842, -3.054999999999996163 ) ) ;
#112285 = LINE ( 'NONE', #134771, #17309 ) ;
#112286 = AXIS2_PLACEMENT_3D ( 'NONE', #107067, #128134, #95472 ) ;
#112287 = CARTESIAN_POINT ( 'NONE',  ( 14.92733143757284786, -1.141545485034857643, 4.000000000000000000 ) ) ;
#112288 = FACE_OUTER_BOUND ( 'NONE', #49907, .T. ) ;
#112289 = EDGE_CURVE ( 'NONE', #117339, #121372, #64337, .T. ) ;
#112290 = CARTESIAN_POINT ( 'NONE',  ( -17.20666063542140378, 21.75929247661549937, 4.998822639870711626 ) ) ;
#112291 = DIRECTION ( 'NONE',  ( 0.000000000000000000, -1.000000000000000000, 0.000000000000000000 ) ) ;
#112292 = EDGE_LOOP ( 'NONE', ( #54082, #86779, #138857 ) ) ;
#112293 = CARTESIAN_POINT ( 'NONE',  ( -24.48921356237309510, -27.52281430457072631, 5.000000000000000000 ) ) ;
#112294 = CARTESIAN_POINT ( 'NONE',  ( -13.82816939922344091, 12.75929247661558641, 4.000000000000000000 ) ) ;
#112295 = LINE ( 'NONE', #79709, #56489 ) ;
#112296 = ORIENTED_EDGE ( 'NONE', *, *, #13510, .F. ) ;
#112297 = ORIENTED_EDGE ( 'NONE', *, *, #129943, .F. ) ;
#112298 = ADVANCED_FACE ( 'NONE', ( #114874 ), #17031, .T. ) ;
#112299 = FACE_OUTER_BOUND ( 'NONE', #85505, .T. ) ;
#112300 = ORIENTED_EDGE ( 'NONE', *, *, #12806, .T. ) ;
#112301 = LINE ( 'NONE', #655, #39855 ) ;
#112302 = CARTESIAN_POINT ( 'NONE',  ( 107.4125270504628986, -7.949999999999998401, -4.867971026610728450E-16 ) ) ;
#112303 = CARTESIAN_POINT ( 'NONE',  ( 18.63311396761903538, -2.779424156541560276, 4.000000000000000000 ) ) ;
#112304 = CARTESIAN_POINT ( 'NONE',  ( 4.495848767239241539, 4.584330080086930965E-16, 0.000000000000000000 ) ) ;
#112305 = CARTESIAN_POINT ( 'NONE',  ( -22.46236777640751114, 22.22500000000000142, 9.722557227176030992 ) ) ;
#112306 = EDGE_CURVE ( 'NONE', #80065, #81768, #51100, .T. ) ;
#112307 = ORIENTED_EDGE ( 'NONE', *, *, #34640, .F. ) ;
#112308 = LINE ( 'NONE', #86970, #85800 ) ;
#112309 = ORIENTED_EDGE ( 'NONE', *, *, #23839, .F. ) ;
#112310 = LINE ( 'NONE', #56543, #137174 ) ;
#112311 = EDGE_CURVE ( 'NONE', #35940, #26671, #60572, .T. ) ;
#112312 = CARTESIAN_POINT ( 'NONE',  ( 17.12956980810188767, -3.967499999999998028, -6.871911579029511330 ) ) ;
#112313 = EDGE_LOOP ( 'NONE', ( #64830, #92810, #49677, #118818 ) ) ;
#112314 = CARTESIAN_POINT ( 'NONE',  ( 80.84959685856478018, 6.109999999999997655, 1.637169565754163836 ) ) ;
#112315 = DIRECTION ( 'NONE',  ( -1.000000000000000000, -1.224606353822377258E-16, -0.000000000000000000 ) ) ;
#112316 = CARTESIAN_POINT ( 'NONE',  ( 98.66252705046289861, 7.949999999999998401, 1.460391307983218338E-15 ) ) ;
#112317 = ORIENTED_EDGE ( 'NONE', *, *, #115448, .F. ) ;
#112318 = ORIENTED_EDGE ( 'NONE', *, *, #81875, .F. ) ;
#112319 = VERTEX_POINT ( 'NONE', #129344 ) ;
#112320 = DIRECTION ( 'NONE',  ( 0.7071067811865486830, -0.7071067811865464625, -0.000000000000000000 ) ) ;
#112321 = DIRECTION ( 'NONE',  ( -0.7071067811865487940, 0.7071067811865463515, -0.000000000000000000 ) ) ;
#112322 = DIRECTION ( 'NONE',  ( -0.7071067811865486830, -0.7071067811865464625, -0.000000000000000000 ) ) ;
#112323 = CARTESIAN_POINT ( 'NONE',  ( -18.18398860626898994, 28.73617430169800002, 5.000000000000000000 ) ) ;
#112324 = ORIENTED_EDGE ( 'NONE', *, *, #114218, .T. ) ;
#112325 = SURFACE_STYLE_FILL_AREA ( #679 ) ;
#112326 = DIRECTION ( 'NONE',  ( -0.000000000000000000, -0.3543493200069152693, 0.9351131265310292928 ) ) ;
#112327 = DIRECTION ( 'NONE',  ( 0.7071067811865487940, 0.7071067811865463515, 0.000000000000000000 ) ) ;
#112328 = ORIENTED_EDGE ( 'NONE', *, *, #119971, .F. ) ;
#112329 = FACE_OUTER_BOUND ( 'NONE', #42015, .T. ) ;
#112330 = FACE_OUTER_BOUND ( 'NONE', #9082, .T. ) ;
#112331 = EDGE_LOOP ( 'NONE', ( #40722, #14781, #113876, #92852 ) ) ;
#112333 = VERTEX_POINT ( 'NONE', #128646 ) ;
#112332 = CARTESIAN_POINT ( 'NONE',  ( 60.59549430335705011, -44.02090675800599939, -34.92500000000512728 ) ) ;
#112334 = ORIENTED_EDGE ( 'NONE', *, *, #72882, .T. ) ;
#112335 = ADVANCED_FACE ( 'NONE', ( #15551 ), #30029, .F. ) ;
#112336 = DIRECTION ( 'NONE',  ( -0.000000000000000000, 0.000000000000000000, 1.000000000000000000 ) ) ;
#112337 = FACE_OUTER_BOUND ( 'NONE', #89751, .T. ) ;
#112338 = ORIENTED_EDGE ( 'NONE', *, *, #105638, .T. ) ;
#112339 = FACE_OUTER_BOUND ( 'NONE', #61528, .T. ) ;
#112340 = ORIENTED_EDGE ( 'NONE', *, *, #50119, .T. ) ;
#112341 = DIRECTION ( 'NONE',  ( 0.000000000000000000, -0.000000000000000000, 1.000000000000000000 ) ) ;
#112342 = CARTESIAN_POINT ( 'NONE',  ( 83.99451991528748351, 28.92564299267996830, 4.000000000000000000 ) ) ;
#112343 = VECTOR ( 'NONE', #7123, 1000.000000000000000 ) ;
#112344 = DIRECTION ( 'NONE',  ( 0.7071067811865486830, -0.7071067811865464625, -0.000000000000000000 ) ) ;
#112345 = LINE ( 'NONE', #24606, #97016 ) ;
#112347 = CARTESIAN_POINT ( 'NONE',  ( 34.49999999999975842, 6.054329344830883031, 4.994342998332162331 ) ) ;
#112346 = AXIS2_PLACEMENT_3D ( 'NONE', #94706, #15697, #28783 ) ;
#112348 = CARTESIAN_POINT ( 'NONE',  ( 34.42499999999998295, 0.000000000000000000, 4.500000000000000888 ) ) ;
#112349 = CARTESIAN_POINT ( 'NONE',  ( 27.00548008471251293, 28.92564299267919381, 4.000000000000000000 ) ) ;
#112350 = EDGE_CURVE ( 'NONE', #20421, #122494, #127950, .T. ) ;
#112351 = CARTESIAN_POINT ( 'NONE',  ( 0.000000000000000000, 0.000000000000000000, 5.000000000000000000 ) ) ;
#112352 = CARTESIAN_POINT ( 'NONE',  ( 18.93706980810188867, 2.126176841940952134, -7.934999999999993392 ) ) ;
#112353 = CARTESIAN_POINT ( 'NONE',  ( 48.29974487139158867, -27.71228299555239971, 4.000000000000000000 ) ) ;
#112354 = CARTESIAN_POINT ( 'NONE',  ( -17.99999999999986855, -3.033600742197710254, 5.000000000000000000 ) ) ;
#112355 = FACE_OUTER_BOUND ( 'NONE', #21383, .T. ) ;
#112356 = EDGE_LOOP ( 'NONE', ( #118536, #43743, #140569, #37621 ) ) ;
#112357 = ORIENTED_EDGE ( 'NONE', *, *, #17378, .F. ) ;
#112358 = CARTESIAN_POINT ( 'NONE',  ( 92.29166666666665719, 3.975000000000003642, -6.884901960086285300 ) ) ;
#112359 = ORIENTED_EDGE ( 'NONE', *, *, #91541, .F. ) ;
#112360 = VECTOR ( 'NONE', #54415, 1000.000000000000000 ) ;
#112361 = ORIENTED_EDGE ( 'NONE', *, *, #101227, .F. ) ;
#112362 = ADVANCED_FACE ( 'NONE', ( #93866 ), #48961, .T. ) ;
#112363 = VERTEX_POINT ( 'NONE', #137391 ) ;
#112364 = CARTESIAN_POINT ( 'NONE',  ( 4.499999999999968914, -9.462702396501006419, -9.474982329943523851 ) ) ;
#112365 = DIRECTION ( 'NONE',  ( -0.7071067811865486830, -0.7071067811865464625, 0.000000000000000000 ) ) ;
#112366 = DIRECTION ( 'NONE',  ( -0.000000000000000000, 0.000000000000000000, 1.000000000000000000 ) ) ;
#112367 = ORIENTED_EDGE ( 'NONE', *, *, #117660, .T. ) ;
#112368 = CARTESIAN_POINT ( 'NONE',  ( 17.99999999999987566, -21.03360074219752462, 5.000000000000000000 ) ) ;
#112369 = DIRECTION ( 'NONE',  ( 0.000000000000000000, 0.000000000000000000, 1.000000000000000000 ) ) ;
#112370 = DIRECTION ( 'NONE',  ( 0.000000000000000000, 1.000000000000000000, 0.000000000000000000 ) ) ;
#112371 = DIRECTION ( 'NONE',  ( -8.817971600062199903E-18, 0.3543493200069153248, 0.9351131265310292928 ) ) ;
#112372 = EDGE_CURVE ( 'NONE', #71967, #115239, #18414, .T. ) ;
#112373 = ORIENTED_EDGE ( 'NONE', *, *, #37225, .F. ) ;
#112374 = DIRECTION ( 'NONE',  ( 0.3543493200069162685, -0.000000000000000000, -0.9351131265310288487 ) ) ;
#112375 = EDGE_CURVE ( 'NONE', #131250, #109962, #55137, .T. ) ;
#112376 = FACE_OUTER_BOUND ( 'NONE', #86168, .T. ) ;
#112377 = DIRECTION ( 'NONE',  ( -0.5735764363510501562, 0.8191520442889890230, 1.003171929053521419E-16 ) ) ;
#112378 = CARTESIAN_POINT ( 'NONE',  ( 16.37176554955605567, -8.240707523384193323, 11.38925528200748971 ) ) ;
#112379 = CARTESIAN_POINT ( 'NONE',  ( 15.71230993966017664, -21.73547319004781286, 4.999917730833664642 ) ) ;
#112380 = CARTESIAN_POINT ( 'NONE',  ( 34.49999999999976552, -11.56887692260769640, 4.000000000000000000 ) ) ;
#112381 = PLANE ( 'NONE',  #31352 ) ;
#112382 = VECTOR ( 'NONE', #138405, 1000.000000000000227 ) ;
#112383 = LINE ( 'NONE', #55879, #7515 ) ;
#112384 = ORIENTED_EDGE ( 'NONE', *, *, #120122, .F. ) ;
#112385 = ORIENTED_EDGE ( 'NONE', *, *, #18143, .F. ) ;
#112386 = VECTOR ( 'NONE', #114838, 999.9999999999998863 ) ;
#112387 = CARTESIAN_POINT ( 'NONE',  ( 122.5004301918981184, -3.055000000000002380, 5.291415217122920289 ) ) ;
#112388 = ORIENTED_EDGE ( 'NONE', *, *, #86910, .T. ) ;
#112390 = EDGE_CURVE ( 'NONE', #28496, #117668, #40929, .T. ) ;
#112389 = VECTOR ( 'NONE', #135603, 999.9999999999998863 ) ;
#112391 = CARTESIAN_POINT ( 'NONE',  ( -81.18398860626899705, 28.73617430169844056, 5.000000000000000000 ) ) ;
#112392 =( NAMED_UNIT ( * ) PLANE_ANGLE_UNIT ( ) SI_UNIT ( $, .RADIAN. ) );
#112393 = EDGE_CURVE ( 'NONE', #49213, #60654, #138096, .T. ) ;
#112394 = FACE_OUTER_BOUND ( 'NONE', #133546, .T. ) ;
#112395 = DIRECTION ( 'NONE',  ( -0.7071067811865486830, -0.7071067811865464625, -0.000000000000000000 ) ) ;
#112396 = CARTESIAN_POINT ( 'NONE',  ( 114.0995968585647660, -6.109999999999997655, -1.637169565754160283 ) ) ;
#112397 = ORIENTED_EDGE ( 'NONE', *, *, #4882, .T. ) ;
#112398 = ORIENTED_EDGE ( 'NONE', *, *, #84852, .F. ) ;
#112399 = EDGE_CURVE ( 'NONE', #113019, #8484, #43656, .T. ) ;
#112400 = ADVANCED_FACE ( 'NONE', ( #132961 ), #53971, .F. ) ;
#112401 = DIRECTION ( 'NONE',  ( 0.7071067811865487940, 0.7071067811865463515, -0.000000000000000000 ) ) ;
#112402 = VERTEX_POINT ( 'NONE', #130081 ) ;
#112403 = ORIENTED_EDGE ( 'NONE', *, *, #24236, .T. ) ;
#112404 = VERTEX_POINT ( 'NONE', #96687 ) ;
#112405 = CARTESIAN_POINT ( 'NONE',  ( 25.19159235450331735, -2.500000000000000444, 3.061616997868384620E-16 ) ) ;
#112406 = APPLICATION_CONTEXT ( 'automotive_design' ) ;
#112407 = CARTESIAN_POINT ( 'NONE',  ( 2.692069808101885897, -7.934999999999990727, -2.126176841940955242 ) ) ;
#112408 = CARTESIAN_POINT ( 'NONE',  ( 30.24543019189811233, -5.291415217122918513, -3.055000000000000160 ) ) ;
#112409 = VERTEX_POINT ( 'NONE', #21314 ) ;
#112410 = ORIENTED_EDGE ( 'NONE', *, *, #33764, .T. ) ;
#112411 = EDGE_CURVE ( 'NONE', #128596, #88238, #22008, .T. ) ;
#112412 = CARTESIAN_POINT ( 'NONE',  ( -26.28769006033953559, -21.73547319004780931, 4.999917730833664642 ) ) ;
#112413 = ORIENTED_EDGE ( 'NONE', *, *, #20596, .F. ) ;
#112414 = ORIENTED_EDGE ( 'NONE', *, *, #68907, .T. ) ;
#112415 = ORIENTED_EDGE ( 'NONE', *, *, #15645, .F. ) ;
#112416 = ADVANCED_FACE ( 'NONE', ( #109742 ), #97418, .F. ) ;
#112417 = EDGE_CURVE ( 'NONE', #13922, #45110, #19169, .T. ) ;
#112418 = CARTESIAN_POINT ( 'NONE',  ( -5.816011393731002066, 28.73617430169783304, 5.000000000000000000 ) ) ;
#112419 = FACE_OUTER_BOUND ( 'NONE', #60261, .T. ) ;
#112420 = LINE ( 'NONE', #14531, #19010 ) ;
#112421 = ORIENTED_EDGE ( 'NONE', *, *, #34197, .F. ) ;
#112422 = FACE_OUTER_BOUND ( 'NONE', #16131, .T. ) ;
#112423 = SURFACE_SIDE_STYLE ('',( #22520 ) ) ;
#112424 = EDGE_CURVE ( 'NONE', #118741, #56485, #63427, .T. ) ;
#112425 = DIRECTION ( 'NONE',  ( -0.7071067811865486830, -0.7071067811865464625, 0.000000000000000000 ) ) ;
#112426 = FACE_BOUND ( 'NONE', #39568, .T. ) ;
#112427 = EDGE_CURVE ( 'NONE', #110220, #117528, #66258, .T. ) ;
#112428 = ORIENTED_EDGE ( 'NONE', *, *, #100954, .T. ) ;
#112429 = DIRECTION ( 'NONE',  ( -0.7071067811865487940, 0.7071067811865463515, -0.000000000000000000 ) ) ;
#112430 = DIRECTION ( 'NONE',  ( -0.000000000000000000, -0.3543493200069153803, -0.9351131265310292928 ) ) ;
#112431 = CARTESIAN_POINT ( 'NONE',  ( -34.42500000000001137, -1.458600742197974087, 5.000000000000000000 ) ) ;
#112432 = ADVANCED_FACE ( 'NONE', ( #52500 ), #9703, .F. ) ;
#112433 = VERTEX_POINT ( 'NONE', #119182 ) ;
#112434 = CARTESIAN_POINT ( 'NONE',  ( 57.18398860626899705, 28.73617430169827358, 5.000000000000000000 ) ) ;
#112435 = ORIENTED_EDGE ( 'NONE', *, *, #39889, .T. ) ;
#112436 = EDGE_LOOP ( 'NONE', ( #91452, #87080, #129756, #113134 ) ) ;
#112437 =( BOUNDED_CURVE ( )  B_SPLINE_CURVE ( 3, ( #11568, #32659, #132713, #65302 ),
 .UNSPECIFIED., .F., .T. ) 
 B_SPLINE_CURVE_WITH_KNOTS ( ( 4, 4 ),
 ( 1.964434688349483871, 3.503810798801452187 ),
 .UNSPECIFIED. ) 
 CURVE ( )  GEOMETRIC_REPRESENTATION_ITEM ( )  RATIONAL_B_SPLINE_CURVE ( ( 1.000000000000000000, 0.8120851936182270636, 0.8120851936182270636, 1.000000000000000000 ) ) 
 REPRESENTATION_ITEM ( '' )  );
#112438 = VERTEX_POINT ( 'NONE', #98164 ) ;
#112439 = VECTOR ( 'NONE', #107724, 1000.000000000000000 ) ;
#112440 = CARTESIAN_POINT ( 'NONE',  ( 46.14126352523144448, 4.472830434245835818, 4.472830434245840259 ) ) ;
#112441 = EDGE_CURVE ( 'NONE', #36808, #118785, #133778, .T. ) ;
#112442 = EDGE_LOOP ( 'NONE', ( #49548, #73176, #142588, #85052 ) ) ;
#112443 = EDGE_CURVE ( 'NONE', #67143, #89687, #71380, .T. ) ;
#112444 = DIRECTION ( 'NONE',  ( 0.000000000000000000, 1.000000000000000000, 0.000000000000000000 ) ) ;
#112445 = VECTOR ( 'NONE', #8395, 1000.000000000000227 ) ;
#112446 = DIRECTION ( 'NONE',  ( 0.000000000000000000, -1.000000000000000000, 0.000000000000000000 ) ) ;
#112447 = ORIENTED_EDGE ( 'NONE', *, *, #4926, .T. ) ;
#112448 = DIRECTION ( 'NONE',  ( -0.000000000000000000, 1.000000000000000000, -0.000000000000000000 ) ) ;
#112449 = DIRECTION ( 'NONE',  ( 0.7071067811865487940, 0.7071067811865463515, -0.000000000000000000 ) ) ;
#112450 = EDGE_CURVE ( 'NONE', #123033, #8173, #19868, .T. ) ;
#112451 = DIRECTION ( 'NONE',  ( -0.6830127018922181881, 0.6830127018922202975, -0.2588190451025214056 ) ) ;
#112452 = VECTOR ( 'NONE', #23725, 999.9999999999998863 ) ;
#112453 = DIRECTION ( 'NONE',  ( -0.3543493200069162685, -0.000000000000000000, -0.9351131265310288487 ) ) ;
#112454 = DIRECTION ( 'NONE',  ( -0.6830127018922181881, 0.6830127018922202975, -0.2588190451025214056 ) ) ;
#112455 = ORIENTED_EDGE ( 'NONE', *, *, #43880, .F. ) ;
#112456 = ORIENTED_EDGE ( 'NONE', *, *, #29548, .T. ) ;
#112458 = ORIENTED_EDGE ( 'NONE', *, *, #63553, .F. ) ;
#112457 = EDGE_CURVE ( 'NONE', #121270, #115355, #130814, .T. ) ;
#112459 = ORIENTED_EDGE ( 'NONE', *, *, #125688, .T. ) ;
#112460 = CARTESIAN_POINT ( 'NONE',  ( -35.99451991528749772, 28.92564299267963079, 4.000000000000000000 ) ) ;
#112461 = VERTEX_POINT ( 'NONE', #75703 ) ;
#112462 = EDGE_LOOP ( 'NONE', ( #85982, #61669, #77204, #12890, #4372, #93766 ) ) ;
#112463 = PLANE ( 'NONE',  #30526 ) ;
#112464 = CARTESIAN_POINT ( 'NONE',  ( -4.499999999999968914, 11.52377502935402198, -1.522421517564075399 ) ) ;
#112465 = ORIENTED_EDGE ( 'NONE', *, *, #89786, .T. ) ;
#112466 = DIRECTION ( 'NONE',  ( -0.000000000000000000, 0.3543493200069152138, -0.9351131265310292928 ) ) ;
#112467 = VECTOR ( 'NONE', #67855, 1000.000000000000000 ) ;
#112468 = EDGE_CURVE ( 'NONE', #116410, #29922, #55383, .T. ) ;
#112469 = CARTESIAN_POINT ( 'NONE',  ( 0.5685132242927012358, 0.4000000000000001887, -2.467792535850613866 ) ) ;
#112470 = EDGE_CURVE ( 'NONE', #33848, #135001, #140782, .T. ) ;
#112471 = CARTESIAN_POINT ( 'NONE',  ( 28.94206980810188767, 7.934999999999993392, 2.126176841940951689 ) ) ;
#112472 = VECTOR ( 'NONE', #128451, 1000.000000000000000 ) ;
#112473 = PLANE ( 'NONE',  #69352 ) ;
#112474 = ORIENTED_EDGE ( 'NONE', *, *, #134238, .T. ) ;
#112475 = CARTESIAN_POINT ( 'NONE',  ( 106.2245968585647802, -1.637169565754161171, 6.109999999999998543 ) ) ;
#112476 = VECTOR ( 'NONE', #71130, 999.9999999999998863 ) ;
#112477 = DIRECTION ( 'NONE',  ( 0.000000000000000000, 0.9976538855070752332, -0.06845965770171351383 ) ) ;
#112478 = ORIENTED_EDGE ( 'NONE', *, *, #55104, .T. ) ;
#112479 = DIRECTION ( 'NONE',  ( 0.7071067811865486830, -0.7071067811865464625, -0.000000000000000000 ) ) ;
#112481 = ORIENTED_EDGE ( 'NONE', *, *, #3855, .F. ) ;
#112480 = DIRECTION ( 'NONE',  ( 0.6830127018922180770, -0.6830127018922204085, -0.2588190451025213501 ) ) ;
#112482 = DIRECTION ( 'NONE',  ( -0.6830127018922181881, 0.6830127018922202975, -0.2588190451025214056 ) ) ;
#112483 = ORIENTED_EDGE ( 'NONE', *, *, #122029, .T. ) ;
#112484 = DIRECTION ( 'NONE',  ( 0.7071067811865487940, -0.7071067811865463515, 0.000000000000000000 ) ) ;
#112485 = EDGE_CURVE ( 'NONE', #786, #71528, #101000, .T. ) ;
#112486 = DIRECTION ( 'NONE',  ( 0.7071067811865487940, 0.7071067811865463515, 0.000000000000000000 ) ) ;
#112487 = DIRECTION ( 'NONE',  ( -0.7071067811865487940, 0.7071067811865463515, -0.000000000000000000 ) ) ;
#112488 = ORIENTED_EDGE ( 'NONE', *, *, #95665, .F. ) ;
#112489 = CARTESIAN_POINT ( 'NONE',  ( 15.01966765291686734, -22.22500000000000142, -13.92590160340912853 ) ) ;
#112490 = FACE_OUTER_BOUND ( 'NONE', #75154, .T. ) ;
#112491 = CARTESIAN_POINT ( 'NONE',  ( -3.489213562373097322, -27.52281430457057709, 5.000000000000000000 ) ) ;
#112492 = ORIENTED_EDGE ( 'NONE', *, *, #91940, .F. ) ;
#112493 = CARTESIAN_POINT ( 'NONE',  ( 2.999999999999975131, 12.83542986846997458, -1.025386466790376927 ) ) ;
#112494 = VERTEX_POINT ( 'NONE', #135108 ) ;
#112495 = LINE ( 'NONE', #77040, #18291 ) ;
#112497 = ORIENTED_EDGE ( 'NONE', *, *, #102947, .T. ) ;
#112496 = FACE_OUTER_BOUND ( 'NONE', #114557, .T. ) ;
#112498 = ORIENTED_EDGE ( 'NONE', *, *, #86418, .F. ) ;
#112499 = DIRECTION ( 'NONE',  ( -1.000000000000000000, 0.000000000000000000, 0.000000000000000000 ) ) ;
#112500 = LINE ( 'NONE', #57429, #71403 ) ;
#112501 = EDGE_LOOP ( 'NONE', ( #137860, #122668, #78729, #47260 ) ) ;
#112502 = PLANE ( 'NONE',  #87643 ) ;
#112503 = PLANE ( 'NONE',  #120177 ) ;
#112504 = DIRECTION ( 'NONE',  ( -0.7071067811865486830, 0.7071067811865464625, 0.000000000000000000 ) ) ;
#112505 = ORIENTED_EDGE ( 'NONE', *, *, #95376, .T. ) ;
#112506 = DIRECTION ( 'NONE',  ( -0.7071067811865486830, 0.7071067811865464625, -0.000000000000000000 ) ) ;
#112507 = EDGE_CURVE ( 'NONE', #58911, #46933, #36472, .T. ) ;
#112509 = EDGE_CURVE ( 'NONE', #69167, #44746, #92254, .T. ) ;
#112508 = DIRECTION ( 'NONE',  ( 0.7071067811865486830, -0.7071067811865464625, -0.000000000000000000 ) ) ;
#112510 = CARTESIAN_POINT ( 'NONE',  ( -5.207106781186500832, -8.240707523384196875, 5.000000000000000000 ) ) ;
#112511 = CARTESIAN_POINT ( 'NONE',  ( -1.499999999999994449, -14.70932175296477418, -11.46312253303836926 ) ) ;
#112512 = LINE ( 'NONE', #125549, #131668 ) ;
#112513 = LINE ( 'NONE', #68342, #7184 ) ;
#112514 = ORIENTED_EDGE ( 'NONE', *, *, #58532, .F. ) ;
#112515 = EDGE_LOOP ( 'NONE', ( #78985, #27950, #28952, #19372 ) ) ;
#112516 = ORIENTED_EDGE ( 'NONE', *, *, #28608, .F. ) ;
#112517 = CARTESIAN_POINT ( 'NONE',  ( 3.005480084712505828, 28.92564299267936079, 4.000000000000000000 ) ) ;
#112518 = EDGE_LOOP ( 'NONE', ( #110118, #64307, #47300, #123430, #101539, #73086 ) ) ;
#112519 = ORIENTED_EDGE ( 'NONE', *, *, #104905, .T. ) ;
#112520 = ORIENTED_EDGE ( 'NONE', *, *, #98642, .T. ) ;
#112521 = FACE_OUTER_BOUND ( 'NONE', #15245, .T. ) ;
#112522 = CARTESIAN_POINT ( 'NONE',  ( -8.483345613589495571, 22.22500000000000142, 4.500000000000000888 ) ) ;
#112523 = VERTEX_POINT ( 'NONE', #124191 ) ;
#112524 = DIRECTION ( 'NONE',  ( -1.000000000000000000, -1.224606353822377258E-16, -0.000000000000000000 ) ) ;
#112525 = CARTESIAN_POINT ( 'NONE',  ( 0.000000000000000000, 0.000000000000000000, 5.000000000000000000 ) ) ;
#112526 = EDGE_CURVE ( 'NONE', #124292, #67057, #22694, .T. ) ;
#112527 = DIRECTION ( 'NONE',  ( -0.6830127018922181881, 0.6830127018922202975, -0.2588190451025214056 ) ) ;
#112528 = LINE ( 'NONE', #101644, #88110 ) ;
#112529 = CARTESIAN_POINT ( 'NONE',  ( 120.4587635252314328, 0.000000000000000000, -6.110000000000001208 ) ) ;
#112530 = EDGE_CURVE ( 'NONE', #75880, #105769, #123515, .T. ) ;
#112531 = VERTEX_POINT ( 'NONE', #58992 ) ;
#112532 = LINE ( 'NONE', #136415, #7075 ) ;
#112533 = CARTESIAN_POINT ( 'NONE',  ( 106.2458603837962272, 3.974999999999996980, 6.884901960086287964 ) ) ;
#112534 = CARTESIAN_POINT ( 'NONE',  ( 3.087196949643289834, -4.814824860968089633E-32, 2.500000000000000444 ) ) ;
#112535 = CARTESIAN_POINT ( 'NONE',  ( 0.7137474236366083691, 7.354941029308180056, 0.7481386797838406322 ) ) ;
#112536 = LINE ( 'NONE', #80641, #59097 ) ;
#112537 = LINE ( 'NONE', #93652, #49205 ) ;
#112538 = PLANE ( 'NONE',  #94418 ) ;
#112539 = EDGE_CURVE ( 'NONE', #40982, #445, #80015, .T. ) ;
#112541 = EDGE_CURVE ( 'NONE', #5483, #89397, #45243, .T. ) ;
#112540 = CARTESIAN_POINT ( 'NONE',  ( 51.12086038379622011, -6.884901960086286188, 3.974999999999997424 ) ) ;
#112542 = VECTOR ( 'NONE', #92762, 1000.000000000000000 ) ;
#112543 = FACE_OUTER_BOUND ( 'NONE', #139237, .T. ) ;
#112544 = CARTESIAN_POINT ( 'NONE',  ( -4.171830600776443632, -11.24070752338417556, 4.000000000000000000 ) ) ;
#112545 = VERTEX_POINT ( 'NONE', #91568 ) ;
#112546 = VERTEX_POINT ( 'NONE', #961 ) ;
#112547 = CARTESIAN_POINT ( 'NONE',  ( 46.06249999999999289, -5.819803920172572198, -5.819803920172573086 ) ) ;
#112548 = ORIENTED_EDGE ( 'NONE', *, *, #135777, .T. ) ;
#112549 = VECTOR ( 'NONE', #76033, 1000.000000000000227 ) ;
#112550 = EDGE_CURVE ( 'NONE', #140889, #34230, #89773, .T. ) ;
#112551 = DIRECTION ( 'NONE',  ( 0.000000000000000000, 0.000000000000000000, 1.000000000000000000 ) ) ;
#112552 = EDGE_LOOP ( 'NONE', ( #59660, #92648, #84965, #115067, #86787 ) ) ;
#112553 = FACE_OUTER_BOUND ( 'NONE', #116477, .T. ) ;
#112554 = CARTESIAN_POINT ( 'NONE',  ( -5.999999999999956479, -9.412538124160663600, 4.000000000000000000 ) ) ;
#112555 = ADVANCED_FACE ( 'NONE', ( #133652 ), #33641, .F. ) ;
#112556 = CARTESIAN_POINT ( 'NONE',  ( 39.81293019189809712, -1.637169565754159617, -6.110000000000001208 ) ) ;
#112558 = ORIENTED_EDGE ( 'NONE', *, *, #66035, .T. ) ;
#112557 = AXIS2_PLACEMENT_3D ( 'NONE', #38018, #138750, #82937 ) ;
#112559 = FACE_OUTER_BOUND ( 'NONE', #28850, .T. ) ;
#112560 = VERTEX_POINT ( 'NONE', #102465 ) ;
#112561 = CARTESIAN_POINT ( 'NONE',  ( 30.32816939922332367, 11.25929247661560773, 4.000000000000000000 ) ) ;
#112562 = EDGE_CURVE ( 'NONE', #34094, #88720, #14717, .T. ) ;
#112563 = CARTESIAN_POINT ( 'NONE',  ( 152.8142135623730837, 26.96999999999993847, -34.92499999999998295 ) ) ;
#112564 = CARTESIAN_POINT ( 'NONE',  ( -21.70710678118638626, -3.740707523384246613, 5.000000000000000000 ) ) ;
#112565 = CARTESIAN_POINT ( 'NONE',  ( 12.40000000000000213, 2.055000000000001492, 0.000000000000000000 ) ) ;
#112566 = ORIENTED_EDGE ( 'NONE', *, *, #68214, .T. ) ;
#112567 = VECTOR ( 'NONE', #67295, 1000.000000000000000 ) ;
#112568 = CARTESIAN_POINT ( 'NONE',  ( 31.17183060077625711, 0.7592924766157104211, 4.000000000000000000 ) ) ;
#112569 = ORIENTED_EDGE ( 'NONE', *, *, #89811, .T. ) ;
#112570 = PLANE ( 'NONE',  #35478 ) ;
#112571 = CARTESIAN_POINT ( 'NONE',  ( -34.92500000000001137, -9.415263340095652467, 16.98967855471612509 ) ) ;
#112572 = CARTESIAN_POINT ( 'NONE',  ( 9.183988606268997046, 28.73617430169793607, 5.000000000000000000 ) ) ;
#112573 = ADVANCED_FACE ( 'NONE', ( #77840 ), #135786, .T. ) ;
#112574 = DIRECTION ( 'NONE',  ( -1.000000000000000000, -0.000000000000000000, -0.000000000000000000 ) ) ;
#112576 = EDGE_CURVE ( 'NONE', #43058, #54084, #122025, .T. ) ;
#112575 = CARTESIAN_POINT ( 'NONE',  ( 24.48921356237309510, -27.52281430457072631, 5.000000000000000000 ) ) ;
#112577 = VECTOR ( 'NONE', #22664, 1000.000000000000000 ) ;
#112578 = VECTOR ( 'NONE', #100804, 1000.000000000000000 ) ;
#112579 = ORIENTED_EDGE ( 'NONE', *, *, #99875, .T. ) ;
#112580 = CARTESIAN_POINT ( 'NONE',  ( 11.93159235450332112, 9.902892378096218942E-16, 0.000000000000000000 ) ) ;
#112581 = CARTESIAN_POINT ( 'NONE',  ( 60.57876352523145158, -7.482591942790325086E-16, 6.109999999999998543 ) ) ;
#112582 = FACE_OUTER_BOUND ( 'NONE', #70233, .T. ) ;
#112583 = EDGE_CURVE ( 'NONE', #60173, #102939, #1656, .T. ) ;
#112584 = CARTESIAN_POINT ( 'NONE',  ( 39.48921356237310221, -27.52281430457082934, 5.000000000000000000 ) ) ;
#112586 = ORIENTED_EDGE ( 'NONE', *, *, #44494, .F. ) ;
#112585 = PLANE ( 'NONE',  #68812 ) ;
#112587 = ORIENTED_EDGE ( 'NONE', *, *, #6273, .F. ) ;
#112588 = VECTOR ( 'NONE', #142837, 1000.000000000000227 ) ;
#112589 = LINE ( 'NONE', #80000, #77133 ) ;
#112590 = ORIENTED_EDGE ( 'NONE', *, *, #140798, .F. ) ;
#112591 = EDGE_CURVE ( 'NONE', #131877, #37393, #45835, .T. ) ;
#112592 = EDGE_CURVE ( 'NONE', #101850, #117764, #23442, .T. ) ;
#112593 = CARTESIAN_POINT ( 'NONE',  ( 11.51078643762690490, -27.52281430457047406, 5.000000000000000000 ) ) ;
#112595 = ORIENTED_EDGE ( 'NONE', *, *, #106155, .F. ) ;
#112594 = ADVANCED_FACE ( 'NONE', ( #45941 ), #69854, .T. ) ;
#112596 = PLANE ( 'NONE',  #12132 ) ;
#112597 = CARTESIAN_POINT ( 'NONE',  ( -34.92500000000001137, -2.143876922607542035, 4.000000000000000000 ) ) ;
#112598 = EDGE_CURVE ( 'NONE', #103813, #114933, #111900, .T. ) ;
#112599 = DIRECTION ( 'NONE',  ( -0.000000000000000000, 0.3543493200069153248, 0.9351131265310292928 ) ) ;
#112600 = FACE_BOUND ( 'NONE', #141335, .T. ) ;
#112601 = EDGE_CURVE ( 'NONE', #40143, #133528, #38616, .T. ) ;
#112602 = PLANE ( 'NONE',  #96559 ) ;
#112603 = PLANE ( 'NONE',  #97730 ) ;
#112604 = DIRECTION ( 'NONE',  ( -0.000000000000000000, 0.000000000000000000, 1.000000000000000000 ) ) ;
#112606 = ORIENTED_EDGE ( 'NONE', *, *, #92850, .F. ) ;
#112605 = CARTESIAN_POINT ( 'NONE',  ( 2.999999999999981792, 10.21212019023809781, -2.019456568337804292 ) ) ;
#112607 = CARTESIAN_POINT ( 'NONE',  ( -39.48921356237310221, -27.52281430457082934, 5.000000000000000000 ) ) ;
#112608 = ORIENTED_EDGE ( 'NONE', *, *, #24534, .F. ) ;
#112609 = ORIENTED_EDGE ( 'NONE', *, *, #21616, .T. ) ;
#112610 = CARTESIAN_POINT ( 'NONE',  ( 77.34959685856478018, 6.109999999999996767, 1.637169565754163836 ) ) ;
#112611 = ORIENTED_EDGE ( 'NONE', *, *, #99707, .T. ) ;
#112612 = EDGE_CURVE ( 'NONE', #49875, #100624, #61815, .T. ) ;
#112613 = CARTESIAN_POINT ( 'NONE',  ( 17.67183060077634593, 20.25929247661551003, 4.000000000000000000 ) ) ;
#112614 = ORIENTED_EDGE ( 'NONE', *, *, #82602, .F. ) ;
#112615 = CARTESIAN_POINT ( 'NONE',  ( -21.48921356237309155, -27.52281430457070499, 5.000000000000000000 ) ) ;
#112616 = AXIS2_PLACEMENT_3D ( 'NONE', #54965, #133938, #122315 ) ;
#112617 = EDGE_CURVE ( 'NONE', #41413, #99874, #59673, .T. ) ;
#112618 = LINE ( 'NONE', #88748, #44955 ) ;
#112619 = DIRECTION ( 'NONE',  ( -0.6830127018922181881, 0.6830127018922202975, -0.2588190451025214056 ) ) ;
#112620 = CARTESIAN_POINT ( 'NONE',  ( -34.47516574401891631, 10.49051761211550726, 4.998110765256836174 ) ) ;
#112622 = CARTESIAN_POINT ( 'NONE',  ( 17.01299345043647193, -0.9444868035624202074, -36.99999999997771738 ) ) ;
#112621 = DIRECTION ( 'NONE',  ( -0.000000000000000000, 0.000000000000000000, 1.000000000000000000 ) ) ;
#112623 = CARTESIAN_POINT ( 'NONE',  ( -8.999999999999934275, 4.931123077392131293, 4.000000000000000000 ) ) ;
#112624 = FACE_OUTER_BOUND ( 'NONE', #77446, .T. ) ;
#112625 = VERTEX_POINT ( 'NONE', #103828 ) ;
#112626 = VECTOR ( 'NONE', #84379, 1000.000000000000000 ) ;
#112627 = ORIENTED_EDGE ( 'NONE', *, *, #37606, .T. ) ;
#112628 = CARTESIAN_POINT ( 'NONE',  ( -13.49999999999990230, 18.05218569542898521, 5.000000000000000000 ) ) ;
#112629 = SURFACE_STYLE_USAGE ( .BOTH. , #109770 ) ;
#112630 = ORIENTED_EDGE ( 'NONE', *, *, #18424, .T. ) ;
#112631 = ORIENTED_EDGE ( 'NONE', *, *, #115942, .F. ) ;
#112632 = VERTEX_POINT ( 'NONE', #49525 ) ;
#112633 = CARTESIAN_POINT ( 'NONE',  ( 29.75043019189810423, 3.055000000000002824, -5.291415217122919401 ) ) ;
#112634 = ORIENTED_EDGE ( 'NONE', *, *, #141162, .T. ) ;
#112635 = CARTESIAN_POINT ( 'NONE',  ( 0.000000000000000000, 0.000000000000000000, 5.000000000000000000 ) ) ;
#112636 = VECTOR ( 'NONE', #27918, 1000.000000000000000 ) ;
#112637 = EDGE_CURVE ( 'NONE', #19510, #103200, #95116, .T. ) ;
#112638 = LINE ( 'NONE', #25616, #67540 ) ;
#112639 = CARTESIAN_POINT ( 'NONE',  ( 32.71247294953710849, 0.000000000000000000, 6.094999999999989981 ) ) ;
#112640 = DIRECTION ( 'NONE',  ( -0.7071067811865486830, 0.7071067811865464625, 0.000000000000000000 ) ) ;
#112641 = VERTEX_POINT ( 'NONE', #81436 ) ;
#112642 = VECTOR ( 'NONE', #54311, 1000.000000000000000 ) ;
#112643 = DIRECTION ( 'NONE',  ( 1.000000000000000000, 0.000000000000000000, 0.000000000000000000 ) ) ;
#112644 = CARTESIAN_POINT ( 'NONE',  ( -12.48921356237309155, -27.52281430457064104, 5.000000000000000000 ) ) ;
#112645 = LINE ( 'NONE', #2423, #10416 ) ;
#112647 = ORIENTED_EDGE ( 'NONE', *, *, #79086, .F. ) ;
#112646 = DIRECTION ( 'NONE',  ( 0.7071067811865487940, 0.7071067811865463515, 0.000000000000000000 ) ) ;
#112648 = ORIENTED_EDGE ( 'NONE', *, *, #65616, .T. ) ;
#112649 = CARTESIAN_POINT ( 'NONE',  ( 1.199999999999999956, -0.5999999999999993117, -4.750000000000000000 ) ) ;
#112650 = DIRECTION ( 'NONE',  ( 0.3543493200069162685, -0.000000000000000000, -0.9351131265310288487 ) ) ;
#112651 = LINE ( 'NONE', #25630, #77207 ) ;
#112652 = ORIENTED_EDGE ( 'NONE', *, *, #54945, .F. ) ;
#112653 = FACE_OUTER_BOUND ( 'NONE', #54799, .T. ) ;
#112654 = CARTESIAN_POINT ( 'NONE',  ( -0.7061230773919507930, 22.22500000000000142, 4.000000000000000000 ) ) ;
#112655 =( GEOMETRIC_REPRESENTATION_CONTEXT ( 3 ) GLOBAL_UNCERTAINTY_ASSIGNED_CONTEXT ( ( #46407 ) ) GLOBAL_UNIT_ASSIGNED_CONTEXT ( ( #4278, #48575, #104358 ) ) REPRESENTATION_CONTEXT ( 'NONE', 'WORKASPACE' ) );
#112656 = CARTESIAN_POINT ( 'NONE',  ( -12.70000000000000462, -27.68200100598810565, 15.59110741220538188 ) ) ;
#112657 = FACE_OUTER_BOUND ( 'NONE', #20224, .T. ) ;
#112658 = CARTESIAN_POINT ( 'NONE',  ( 54.48921356237310221, -27.52281430457093236, 5.000000000000000000 ) ) ;
#112659 = CARTESIAN_POINT ( 'NONE',  ( 8.999999999999934275, 10.21212019023809425, -2.019456568337821611 ) ) ;
#112660 = FACE_OUTER_BOUND ( 'NONE', #85968, .T. ) ;
#112661 = DIRECTION ( 'NONE',  ( -0.000000000000000000, -0.3543493200069152693, 0.9351131265310292928 ) ) ;
#112662 = LINE ( 'NONE', #124253, #42444 ) ;
#112663 = STYLED_ITEM ( 'NONE', ( #98323 ), #110939 ) ;
#112664 = CARTESIAN_POINT ( 'NONE',  ( 71.99451991528749772, 28.92564299267988304, 4.000000000000000000 ) ) ;
#112665 = ORIENTED_EDGE ( 'NONE', *, *, #106503, .T. ) ;
#112666 = ORIENTED_EDGE ( 'NONE', *, *, #10555, .T. ) ;
#112667 = CARTESIAN_POINT ( 'NONE',  ( 25.31559147121573972, -5.499261314031187453, -3.175000000000002487 ) ) ;
#112668 = CARTESIAN_POINT ( 'NONE',  ( 21.79333936457832266, 21.75929247661549226, 4.998822639870715179 ) ) ;
#112669 = VECTOR ( 'NONE', #86012, 1000.000000000000000 ) ;
#112670 = DIRECTION ( 'NONE',  ( -0.3543493200069163240, 4.681814790819596721E-17, -0.9351131265310288487 ) ) ;
#112671 = CARTESIAN_POINT ( 'NONE',  ( 6.852250093007166143, 0.000000000000000000, 2.500000000000000444 ) ) ;
#112672 = VECTOR ( 'NONE', #68702, 1000.000000000000000 ) ;
#112673 = ORIENTED_EDGE ( 'NONE', *, *, #25788, .T. ) ;
#112674 = CARTESIAN_POINT ( 'NONE',  ( -25.49999999999981881, -8.947814304570739452, 5.000000000000000000 ) ) ;
#112675 = DIRECTION ( 'NONE',  ( 0.7071067811865486830, -0.7071067811865464625, -0.000000000000000000 ) ) ;
#112676 = DIRECTION ( 'NONE',  ( -0.000000000000000000, -0.000000000000000000, 1.000000000000000000 ) ) ;
#112677 = ORIENTED_EDGE ( 'NONE', *, *, #74290, .T. ) ;
#112678 = CARTESIAN_POINT ( 'NONE',  ( -8.999999999999932498, 1.761378380278673994, -6.096875308897274692 ) ) ;
#112679 = VECTOR ( 'NONE', #129629, 1000.000000000000000 ) ;
#112680 = CARTESIAN_POINT ( 'NONE',  ( 52.12043019189811588, 3.055000000000002380, -5.291415217122917625 ) ) ;
#112681 = CARTESIAN_POINT ( 'NONE',  ( -63.29974487139158867, -27.71228299555250274, 4.000000000000000000 ) ) ;
#112682 = EDGE_CURVE ( 'NONE', #72848, #62221, #125637, .T. ) ;
#112683 = CARTESIAN_POINT ( 'NONE',  ( 34.60428828362104525, 22.19175015946030172, 4.000000000000000000 ) ) ;
#112684 = LINE ( 'NONE', #13352, #51081 ) ;
#112685 = VERTEX_POINT ( 'NONE', #93710 ) ;
#112686 = FACE_OUTER_BOUND ( 'NONE', #31111, .T. ) ;
#112687 = EDGE_CURVE ( 'NONE', #88279, #95024, #26315, .T. ) ;
#112688 = EDGE_CURVE ( 'NONE', #116339, #103979, #138651, .T. ) ;
#112689 = ORIENTED_EDGE ( 'NONE', *, *, #136762, .F. ) ;
#112690 = CARTESIAN_POINT ( 'NONE',  ( 34.49999999999976552, 0.4311230773921780335, 4.000000000000000000 ) ) ;
#112691 = PRESENTATION_STYLE_ASSIGNMENT (( #68510 ) ) ;
#112692 = CARTESIAN_POINT ( 'NONE',  ( -7.940000000000007496, -32.12917598568331101, -10.00000000000000178 ) ) ;
#112693 = EDGE_CURVE ( 'NONE', #62248, #78479, #70572, .T. ) ;
#112694 = SURFACE_SIDE_STYLE ('',( #133057 ) ) ;
#112695 = DIRECTION ( 'NONE',  ( -1.000000000000000000, -0.000000000000000000, -0.000000000000000000 ) ) ;
#112696 = CARTESIAN_POINT ( 'NONE',  ( -7.499999999999940492, -11.94781430457070925, 5.000000000000000000 ) ) ;
#112697 = EDGE_CURVE ( 'NONE', #70428, #96891, #114716, .T. ) ;
#112698 = EDGE_CURVE ( 'NONE', #110453, #76657, #15390, .T. ) ;
#112699 = EDGE_LOOP ( 'NONE', ( #37462, #96463, #17072, #91770 ) ) ;
#112700 = EDGE_LOOP ( 'NONE', ( #98213, #90353, #109701, #102623 ) ) ;
#112701 = DIRECTION ( 'NONE',  ( 0.7071067811865487940, -0.7071067811865463515, 0.000000000000000000 ) ) ;
#112702 = CARTESIAN_POINT ( 'NONE',  ( -24.18398860626899705, 28.73617430169804265, 5.000000000000000000 ) ) ;
#112703 = UNCERTAINTY_MEASURE_WITH_UNIT (LENGTH_MEASURE( 1.000000000000000082E-05 ), #30024, 'distance_accuracy_value', 'NONE');
#112704 = CARTESIAN_POINT ( 'NONE',  ( 8.207106781186487510, -8.240707523384203981, 5.000000000000000000 ) ) ;
#112705 = DIRECTION ( 'NONE',  ( -1.000000000000000000, -1.224606353822377258E-16, -0.000000000000000000 ) ) ;
#112706 = EDGE_CURVE ( 'NONE', #77481, #86073, #6641, .T. ) ;
#112708 = EDGE_CURVE ( 'NONE', #26671, #16046, #37921, .T. ) ;
#112707 = CARTESIAN_POINT ( 'NONE',  ( 72.70419371712955581, -6.884901960086285300, -3.975000000000000089 ) ) ;
#112709 = CARTESIAN_POINT ( 'NONE',  ( -36.48921356237310221, -27.52281430457080802, 5.000000000000000000 ) ) ;
#112710 = VECTOR ( 'NONE', #33094, 1000.000000000000000 ) ;
#112711 = DIRECTION ( 'NONE',  ( -1.000000000000000000, 3.654646145370261567E-15, 0.000000000000000000 ) ) ;
#112712 = ORIENTED_EDGE ( 'NONE', *, *, #10098, .T. ) ;
#112713 = CARTESIAN_POINT ( 'NONE',  ( 70.27083333333334281, -7.949999999999999289, -2.130196079827426203 ) ) ;
#112714 = DIRECTION ( 'NONE',  ( -0.7071067811865486830, -0.7071067811865464625, -0.000000000000000000 ) ) ;
#112715 = EDGE_CURVE ( 'NONE', #63684, #7759, #16102, .T. ) ;
#112716 = CARTESIAN_POINT ( 'NONE',  ( 78.48921356237309510, -27.52281430457109934, 5.000000000000000000 ) ) ;
#112717 = DIRECTION ( 'NONE',  ( -0.7071067811865486830, -0.7071067811865464625, 0.000000000000000000 ) ) ;
#112718 = VECTOR ( 'NONE', #17340, 1000.000000000000227 ) ;
#112719 = EDGE_CURVE ( 'NONE', #48370, #42602, #87615, .T. ) ;
#112720 = ORIENTED_EDGE ( 'NONE', *, *, #96171, .F. ) ;
#112721 = EDGE_CURVE ( 'NONE', #25013, #132883, #62171, .T. ) ;
#112722 = DIRECTION ( 'NONE',  ( -0.000000000000000000, -0.000000000000000000, 1.000000000000000000 ) ) ;
#112723 = CARTESIAN_POINT ( 'NONE',  ( 70.00043019189810423, -3.055000000000002380, 5.291415217122920289 ) ) ;
#112724 = AXIS2_PLACEMENT_3D ( 'NONE', #14641, #62446, #39997 ) ;
#112725 = EDGE_LOOP ( 'NONE', ( #33342, #124242, #142811, #3524 ) ) ;
#112726 = ORIENTED_EDGE ( 'NONE', *, *, #1238, .F. ) ;
#112727 = DIRECTION ( 'NONE',  ( -0.7071067811865486830, -0.7071067811865464625, 0.000000000000000000 ) ) ;
#112728 = ADVANCED_FACE ( 'NONE', ( #5239 ), #27728, .T. ) ;
#112729 = CARTESIAN_POINT ( 'NONE',  ( 57.18398860626899705, 28.73617430169827358, 5.000000000000000000 ) ) ;
#112730 = FACE_OUTER_BOUND ( 'NONE', #111748, .T. ) ;
#112731 = DIRECTION ( 'NONE',  ( 1.000000000000000000, -0.000000000000000000, -0.000000000000000000 ) ) ;
#112733 = ORIENTED_EDGE ( 'NONE', *, *, #63152, .T. ) ;
#112732 = CARTESIAN_POINT ( 'NONE',  ( -69.29974487139159578, -27.71228299555254537, 4.000000000000000000 ) ) ;
#112734 = DIRECTION ( 'NONE',  ( 0.7071067811865487940, 0.7071067811865463515, 0.000000000000000000 ) ) ;
#112735 = DIRECTION ( 'NONE',  ( 0.7071067811865487940, 0.7071067811865463515, 0.000000000000000000 ) ) ;
#112736 = PLANE ( 'NONE',  #93365 ) ;
#112737 = EDGE_CURVE ( 'NONE', #4524, #96941, #65748, .T. ) ;
#112738 = LINE ( 'NONE', #57680, #71582 ) ;
#112739 = ORIENTED_EDGE ( 'NONE', *, *, #78765, .F. ) ;
#112740 = AXIS2_PLACEMENT_3D ( 'NONE', #5957, #115425, #27027 ) ;
#112741 = ORIENTED_EDGE ( 'NONE', *, *, #129727, .T. ) ;
#112742 = CARTESIAN_POINT ( 'NONE',  ( 56.58376352523143993, -6.110000000000001208, -3.741295971395164515E-16 ) ) ;
#112743 = ORIENTED_EDGE ( 'NONE', *, *, #39238, .F. ) ;
#112744 = VECTOR ( 'NONE', #122022, 1000.000000000000000 ) ;
#112745 = LINE ( 'NONE', #143236, #135535 ) ;
#112746 = CARTESIAN_POINT ( 'NONE',  ( 27.75860074219777118, 21.72500000000000142, 5.000000000000000000 ) ) ;
#112747 = DIRECTION ( 'NONE',  ( 0.5735764363510448272, -0.8191520442889927978, 1.003171929053526103E-16 ) ) ;
#112748 = EDGE_CURVE ( 'NONE', #21912, #85379, #86024, .T. ) ;
#112749 = LINE ( 'NONE', #101869, #55055 ) ;
#112750 = LINE ( 'NONE', #114172, #29343 ) ;
#112751 = ORIENTED_EDGE ( 'NONE', *, *, #88550, .T. ) ;
#112752 = ORIENTED_EDGE ( 'NONE', *, *, #31053, .T. ) ;
#112753 = CARTESIAN_POINT ( 'NONE',  ( -34.92499999999997584, 22.27000000000000668, -40.00000000000000000 ) ) ;
#112754 = CARTESIAN_POINT ( 'NONE',  ( -17.20366202404553135, -1.503341788956612968, -32.09416967367160112 ) ) ;
#112755 = ADVANCED_FACE ( 'NONE', ( #64274 ), #141856, .T. ) ;
#112756 = ORIENTED_EDGE ( 'NONE', *, *, #77391, .F. ) ;
#112757 = ADVANCED_FACE ( 'NONE', ( #53391 ), #97595, .F. ) ;
#112758 = DIRECTION ( 'NONE',  ( -0.7071067811865487940, 0.7071067811865463515, -0.000000000000000000 ) ) ;
#112759 = CARTESIAN_POINT ( 'NONE',  ( 14.56453960929607305, -0.7633378608190133363, 4.223415947001568860 ) ) ;
#112760 = VERTEX_POINT ( 'NONE', #43250 ) ;
#112761 = EDGE_CURVE ( 'NONE', #104374, #27773, #75181, .T. ) ;
#112762 = FACE_BOUND ( 'NONE', #89912, .T. ) ;
#112763 = CARTESIAN_POINT ( 'NONE',  ( 2.999999999999999112, -1.600000000000060929, 28.92500000000001847 ) ) ;
#112764 = CARTESIAN_POINT ( 'NONE',  ( -16.49999999999988276, -17.56887692260763956, 4.000000000000000000 ) ) ;
#112765 = CARTESIAN_POINT ( 'NONE',  ( 36.82919371712956291, -3.975000000000001865, 6.884901960086284411 ) ) ;
#112766 = EDGE_CURVE ( 'NONE', #47526, #83800, #109911, .T. ) ;
#112767 = AXIS2_PLACEMENT_3D ( 'NONE', #133642, #99549, #65299 ) ;
#112768 = DIRECTION ( 'NONE',  ( 0.7071067811865487940, -0.7071067811865463515, 0.000000000000000000 ) ) ;
#112769 = DIRECTION ( 'NONE',  ( 0.2853913524755786746, 0.7768309387288983014, 0.5613247443020290550 ) ) ;
#112770 = ORIENTED_EDGE ( 'NONE', *, *, #131111, .T. ) ;
#112771 = VECTOR ( 'NONE', #71215, 1000.000000000000000 ) ;
#112772 = VERTEX_POINT ( 'NONE', #142562 ) ;
#112773 = CARTESIAN_POINT ( 'NONE',  ( 104.6204301918981230, 3.055000000000001936, -5.291415217122916737 ) ) ;
#112774 = ORIENTED_EDGE ( 'NONE', *, *, #9108, .T. ) ;
#112775 = ADVANCED_FACE ( 'NONE', ( #67135 ), #8902, .T. ) ;
#112776 = PLANE ( 'NONE',  #116061 ) ;
#112777 = EDGE_LOOP ( 'NONE', ( #139951, #101421, #73647, #41602, #120809 ) ) ;
#112778 = VECTOR ( 'NONE', #17330, 1000.000000000000000 ) ;
#112779 = CARTESIAN_POINT ( 'NONE',  ( -30.48921356237309510, -27.52281430457076894, 5.000000000000000000 ) ) ;
#112780 = CARTESIAN_POINT ( 'NONE',  ( -34.17183060077622514, -11.24070752338416135, 4.000000000000000000 ) ) ;
#112781 = CARTESIAN_POINT ( 'NONE',  ( 10.94186803553636977, 2.500000000000003109, 3.061616997868386592E-16 ) ) ;
#112782 = ORIENTED_EDGE ( 'NONE', *, *, #108251, .F. ) ;
#112783 = PLANE ( 'NONE',  #13479 ) ;
#112784 = CARTESIAN_POINT ( 'NONE',  ( -83.99451991528748351, 28.92564299267996830, 4.000000000000000000 ) ) ;
#112785 = DIRECTION ( 'NONE',  ( 0.6830127018922180770, -0.6830127018922204085, -0.2588190451025213501 ) ) ;
#112786 = CARTESIAN_POINT ( 'NONE',  ( 27.35002705046288085, -5.819803920172573086, -5.819803920172573086 ) ) ;
#112787 = LINE ( 'NONE', #100506, #2752 ) ;
#112788 = EDGE_LOOP ( 'NONE', ( #1644, #126895, #21813, #50414, #69764 ) ) ;
#112789 = CARTESIAN_POINT ( 'NONE',  ( -39.48921356237310221, -27.52281430457082934, 5.000000000000000000 ) ) ;
#112790 = DIRECTION ( 'NONE',  ( -0.000000000000000000, 0.3543493200069153248, 0.9351131265310292928 ) ) ;
#112791 = ORIENTED_EDGE ( 'NONE', *, *, #107533, .T. ) ;
#112792 = EDGE_CURVE ( 'NONE', #32826, #85320, #42550, .T. ) ;
#112793 = VERTEX_POINT ( 'NONE', #111327 ) ;
#112794 = VERTEX_POINT ( 'NONE', #33118 ) ;
#112795 = CARTESIAN_POINT ( 'NONE',  ( 50.89626352523143993, 4.472830434245840259, -4.472830434245838482 ) ) ;
#112796 = VECTOR ( 'NONE', #115618, 1000.000000000000227 ) ;
#112797 = VERTEX_POINT ( 'NONE', #20752 ) ;
#112798 = CARTESIAN_POINT ( 'NONE',  ( -12.69999999999998153, 0.000000000000000000, 0.000000000000000000 ) ) ;
#112799 = VECTOR ( 'NONE', #116875, 1000.000000000000000 ) ;
#112800 = CARTESIAN_POINT ( 'NONE',  ( 6.024972949537104938, -4.461849672132299993, -4.461849672132299105 ) ) ;
#112802 =( BOUNDED_CURVE ( )  B_SPLINE_CURVE ( 3, ( #74582, #118770, #83309, #40523 ),
 .UNSPECIFIED., .F., .T. ) 
 B_SPLINE_CURVE_WITH_KNOTS ( ( 4, 4 ),
 ( 4.350170835173023498, 4.500739107949211615 ),
 .UNSPECIFIED. ) 
 CURVE ( )  GEOMETRIC_REPRESENTATION_ITEM ( )  RATIONAL_B_SPLINE_CURVE ( ( 1.000000000000000000, 0.9981116584018956406, 0.9981116584018956406, 1.000000000000000000 ) ) 
 REPRESENTATION_ITEM ( '' )  );
#112801 = CARTESIAN_POINT ( 'NONE',  ( 94.50043019189810423, -3.055000000000002380, 5.291415217122920289 ) ) ;
#112803 = CARTESIAN_POINT ( 'NONE',  ( -34.42500000000001137, 19.54139925780181386, 5.000000000000000000 ) ) ;
#112804 = ORIENTED_EDGE ( 'NONE', *, *, #28961, .F. ) ;
#112805 = LINE ( 'NONE', #91087, #43282 ) ;
#112806 = ORIENTED_EDGE ( 'NONE', *, *, #70204, .F. ) ;
#112807 = LINE ( 'NONE', #59871, #102102 ) ;
#112808 = VECTOR ( 'NONE', #47712, 1000.000000000000000 ) ;
#112809 = CARTESIAN_POINT ( 'NONE',  ( 12.70701326429294831, -21.74070752338406365, 4.999753212805217117 ) ) ;
#112810 = EDGE_LOOP ( 'NONE', ( #71844, #76226, #130236, #91888 ) ) ;
#112811 = ADVANCED_FACE ( 'NONE', ( #120778 ), #77328, .F. ) ;
#112812 = DIRECTION ( 'NONE',  ( -0.7071067811865487940, 0.7071067811865463515, -0.000000000000000000 ) ) ;
#112813 = CARTESIAN_POINT ( 'NONE',  ( -24.99033360189226372, 3.759292476615678336, 4.478963035907990609 ) ) ;
#112814 = CARTESIAN_POINT ( 'NONE',  ( 126.2037635252314658, 6.109999999999999432, 1.122388791418549108E-15 ) ) ;
#112815 = ORIENTED_EDGE ( 'NONE', *, *, #142292, .T. ) ;
#112816 = EDGE_CURVE ( 'NONE', #76633, #105676, #78017, .T. ) ;
#112817 = LINE ( 'NONE', #12068, #99066 ) ;
#112818 = ORIENTED_EDGE ( 'NONE', *, *, #1235, .T. ) ;
#112819 = ORIENTED_EDGE ( 'NONE', *, *, #59783, .T. ) ;
#112820 = ORIENTED_EDGE ( 'NONE', *, *, #140363, .T. ) ;
#112821 = CARTESIAN_POINT ( 'NONE',  ( 19.17183060077633883, 9.759292476615629042, 4.000000000000000000 ) ) ;
#112822 = LINE ( 'NONE', #15607, #65409 ) ;
#112823 = VECTOR ( 'NONE', #117914, 1000.000000000000000 ) ;
#112824 = DIRECTION ( 'NONE',  ( -0.3543493200069162685, -0.000000000000000000, -0.9351131265310288487 ) ) ;
#112825 = DIRECTION ( 'NONE',  ( -0.7071067811865487940, 0.7071067811865463515, -0.000000000000000000 ) ) ;
#112826 = ADVANCED_FACE ( 'NONE', ( #65010 ), #31650, .T. ) ;
#112827 = DIRECTION ( 'NONE',  ( 0.7071067811865487940, 0.7071067811865463515, 0.000000000000000000 ) ) ;
#112828 = ORIENTED_EDGE ( 'NONE', *, *, #14611, .F. ) ;
#112829 = FILL_AREA_STYLE ('',( #37430 ) ) ;
#112830 = CARTESIAN_POINT ( 'NONE',  ( 19.37456980810188867, 6.871911579029510442, -3.967499999999998916 ) ) ;
#112831 = DIRECTION ( 'NONE',  ( 0.3543493200069162685, -0.000000000000000000, -0.9351131265310288487 ) ) ;
#112832 = CARTESIAN_POINT ( 'NONE',  ( 23.86500426248363027, 3.759292476615681888, 15.36553568819720716 ) ) ;
#112833 = VECTOR ( 'NONE', #70568, 999.9999999999998863 ) ;
#112834 = CARTESIAN_POINT ( 'NONE',  ( -2.999999999999975131, -22.06887692260758271, 4.000000000000000000 ) ) ;
#112835 = ORIENTED_EDGE ( 'NONE', *, *, #59892, .T. ) ;
#112836 = ORIENTED_EDGE ( 'NONE', *, *, #120519, .T. ) ;
#112837 = VERTEX_POINT ( 'NONE', #110599 ) ;
#112838 =( LENGTH_UNIT ( ) NAMED_UNIT ( * ) SI_UNIT ( .MILLI., .METRE. ) );
#112839 = FACE_OUTER_BOUND ( 'NONE', #34805, .T. ) ;
#112840 = UNCERTAINTY_MEASURE_WITH_UNIT (LENGTH_MEASURE( 1.000000000000000082E-05 ), #37146, 'distance_accuracy_value', 'NONE');
#112841 = DIRECTION ( 'NONE',  ( -0.000000000000000000, -0.3543493200069152693, 0.9351131265310292928 ) ) ;
#112842 = DIRECTION ( 'NONE',  ( 1.000000000000000000, 0.000000000000000000, 0.000000000000000000 ) ) ;
#112843 = DIRECTION ( 'NONE',  ( -0.5735764363510507113, 0.8191520442889885789, 1.003171929053520926E-16 ) ) ;
#112844 = LINE ( 'NONE', #25111, #94660 ) ;
#112845 = CARTESIAN_POINT ( 'NONE',  ( 12.77004279457784186, 21.73644205237998150, 5.000000000000000888 ) ) ;
#112846 = DIRECTION ( 'NONE',  ( -1.000000000000000000, -0.000000000000000000, -0.000000000000000000 ) ) ;
#112847 = DIRECTION ( 'NONE',  ( 0.7071067811865487940, 0.7071067811865463515, 0.000000000000000000 ) ) ;
#112848 = EDGE_CURVE ( 'NONE', #112319, #67893, #138083, .T. ) ;
#112849 = ORIENTED_EDGE ( 'NONE', *, *, #69750, .T. ) ;
#112850 = CARTESIAN_POINT ( 'NONE',  ( 17.15336191800343002, -1.295666265796720840, -31.89410451029661075 ) ) ;
#112851 = ORIENTED_EDGE ( 'NONE', *, *, #83584, .F. ) ;
#112852 = VECTOR ( 'NONE', #83970, 1000.000000000000000 ) ;
#112853 = PLANE ( 'NONE',  #66857 ) ;
#112855 = EDGE_LOOP ( 'NONE', ( #92835, #129566, #118454, #59503 ) ) ;
#112854 = CARTESIAN_POINT ( 'NONE',  ( -23.20710678118637915, -5.240707523384227073, 5.000000000000000000 ) ) ;
#112856 = AXIS2_PLACEMENT_3D ( 'NONE', #2554, #46862, #91049 ) ;
#112857 = DIRECTION ( 'NONE',  ( 0.6830127018922180770, -0.6830127018922204085, -0.2588190451025213501 ) ) ;
#112858 = EDGE_CURVE ( 'NONE', #18692, #81729, #133125, .T. ) ;
#112859 = VERTEX_POINT ( 'NONE', #79486 ) ;
#112860 = FACE_OUTER_BOUND ( 'NONE', #17389, .T. ) ;
#112861 = ORIENTED_EDGE ( 'NONE', *, *, #76020, .T. ) ;
#112862 = LINE ( 'NONE', #12825, #76873 ) ;
#112863 = UNCERTAINTY_MEASURE_WITH_UNIT (LENGTH_MEASURE( 1.000000000000000082E-05 ), #130384, 'distance_accuracy_value', 'NONE');
#112864 = EDGE_LOOP ( 'NONE', ( #100061, #130033, #42935, #32244 ) ) ;
#112865 = CIRCLE ( 'NONE', #55043, 0.5000000000000000000 ) ;
#112866 = AXIS2_PLACEMENT_3D ( 'NONE', #94403, #26314, #82148 ) ;
#112867 = DIRECTION ( 'NONE',  ( -0.7071067811865486830, -0.7071067811865464625, 0.000000000000000000 ) ) ;
#112868 =( BOUNDED_SURFACE ( )  B_SPLINE_SURFACE ( 3, 2, ( 
 ( #93950, #128040, #5493 ),
 ( #75093, #6188, #96080 ),
 ( #7639, #129428, #138907 ),
 ( #96762, #119259, #83086 ),
 ( #39599, #60662, #62778 ),
 ( #49771, #41720, #117120 ),
 ( #17113, #29403, #138183 ),
 ( #117814, #17794, #38866 ),
 ( #30116, #62068, #127288 ),
 ( #27987, #72257, #51900 ),
 ( #74364, #118552, #51177 ),
 ( #116427, #61381, #28720 ) ),
 .UNSPECIFIED., .F., .F., .F. ) 
 B_SPLINE_SURFACE_WITH_KNOTS ( ( 4, 2, 2, 2, 2, 4 ),
 ( 3, 3 ),
 ( 4.336808689942017736E-19, 0.001647923167088038423, 0.002471884750632057526, 0.003295846334176076413, 0.004943769501264114186, 0.006591692668352152826 ),
 ( 0.000000000000000000, 1.000000000000000000 ),
 .UNSPECIFIED. ) 
 GEOMETRIC_REPRESENTATION_ITEM ( )  RATIONAL_B_SPLINE_SURFACE ( (
 ( 1.000000000000000000, 0.7071067811865475727, 1.000000000000000000),
 ( 1.000000000000000000, 0.7122033721489962055, 1.000000000000000000),
 ( 1.000000000000000000, 0.7158366153114927855, 1.000000000000000000),
 ( 1.000000000000000000, 0.7192720032935935315, 1.000000000000000000),
 ( 1.000000000000000000, 0.7200809050417179558, 1.000000000000000000),
 ( 1.000000000000000000, 0.7210491446665049375, 1.000000000000000000),
 ( 1.000000000000000000, 0.7212054070303647313, 1.000000000000000000),
 ( 1.000000000000000000, 0.7207522793907679137, 1.000000000000000000),
 ( 1.000000000000000000, 0.7192424821649830990, 1.000000000000000000),
 ( 1.000000000000000000, 0.7143802006614198286, 1.000000000000000000),
 ( 1.000000000000000000, 0.7109884861397212097, 1.000000000000000000),
 ( 1.000000000000000000, 0.7071067811865492381, 1.000000000000000000) ) ) 
 REPRESENTATION_ITEM ( '' )  SURFACE ( )  );
#112869 = EDGE_CURVE ( 'NONE', #49544, #47125, #1811, .T. ) ;
#112872 = ADVANCED_FACE ( 'NONE', ( #101890 ), #12011, .F. ) ;
#112871 = CARTESIAN_POINT ( 'NONE',  ( 105.0791937171295700, 3.975000000000002753, -6.884901960086283523 ) ) ;
#112870 = VECTOR ( 'NONE', #94009, 1000.000000000000000 ) ;
#112873 = FILL_AREA_STYLE ('',( #89695 ) ) ;
#112874 = CARTESIAN_POINT ( 'NONE',  ( 20.20710678118641113, -11.24070752338416845, 5.000000000000000000 ) ) ;
#112876 = ADVANCED_FACE ( 'NONE', ( #3275 ), #48225, .T. ) ;
#112875 = EDGE_LOOP ( 'NONE', ( #60989, #24461, #23809, #78386 ) ) ;
#112877 = CARTESIAN_POINT ( 'NONE',  ( -7.396568071053523319, -14.24070752338414358, 19.24067776001724539 ) ) ;
#112878 = EDGE_CURVE ( 'NONE', #20530, #97534, #122939, .T. ) ;
#112879 = DIRECTION ( 'NONE',  ( 0.000000000000000000, 0.000000000000000000, -1.000000000000000000 ) ) ;
#112880 = CARTESIAN_POINT ( 'NONE',  ( 16.47916666666667140, 6.094999999999988205, -1.633150327867694651 ) ) ;
#112881 = CARTESIAN_POINT ( 'NONE',  ( 27.48921356237309155, -27.52281430457074762, 5.000000000000000000 ) ) ;
#112882 = CIRCLE ( 'NONE', #87447, 2.500000000000000444 ) ;
#112883 = DIRECTION ( 'NONE',  ( -0.7071067811865486830, -0.7071067811865464625, 0.000000000000000000 ) ) ;
#112885 = EDGE_CURVE ( 'NONE', #50863, #62405, #56299, .T. ) ;
#112884 = CARTESIAN_POINT ( 'NONE',  ( 31.56687199751238992, -21.74070752338405654, 6.915939825044000955 ) ) ;
#112886 = EDGE_LOOP ( 'NONE', ( #38275, #80402, #132059, #140980 ) ) ;
#112887 = LINE ( 'NONE', #69404, #25813 ) ;
#112889 = EDGE_LOOP ( 'NONE', ( #3291, #75229, #2636, #127925 ) ) ;
#112888 = ADVANCED_FACE ( 'NONE', ( #125068 ), #67887, .T. ) ;
#112890 = CARTESIAN_POINT ( 'NONE',  ( 96.39626352523144703, 4.472830434245840259, -4.472830434245839371 ) ) ;
#112891 = CARTESIAN_POINT ( 'NONE',  ( -63.48921356237309510, -27.52281430457099631, 5.000000000000000000 ) ) ;
#112892 = DIRECTION ( 'NONE',  ( 0.3543493200069162685, -0.000000000000000000, -0.9351131265310288487 ) ) ;
#112893 = DIRECTION ( 'NONE',  ( -0.7071067811865487940, 0.7071067811865463515, 0.000000000000000000 ) ) ;
#112894 = ORIENTED_EDGE ( 'NONE', *, *, #53319, .F. ) ;
#112895 = DIRECTION ( 'NONE',  ( 0.5735764363510444941, 0.8191520442889929088, 0.000000000000000000 ) ) ;
#112896 = LINE ( 'NONE', #1257, #37269 ) ;
#112897 = EDGE_CURVE ( 'NONE', #121255, #143282, #88122, .T. ) ;
#112898 = DIRECTION ( 'NONE',  ( -0.7071067811865486830, 0.7071067811865464625, 0.000000000000000000 ) ) ;
#112899 = ORIENTED_EDGE ( 'NONE', *, *, #113230, .F. ) ;
#112900 = EDGE_CURVE ( 'NONE', #69033, #135404, #135945, .T. ) ;
#112901 = DIRECTION ( 'NONE',  ( -0.000000000000000000, -0.3543493200069152693, 0.9351131265310292928 ) ) ;
#112902 = DIRECTION ( 'NONE',  ( -0.7071067811865487940, 0.7071067811865463515, 0.000000000000000000 ) ) ;
#112904 = VERTEX_POINT ( 'NONE', #70024 ) ;
#112903 = CARTESIAN_POINT ( 'NONE',  ( 18.29974487139159223, -27.71228299555219010, 4.000000000000000000 ) ) ;
#112906 = AXIS2_PLACEMENT_3D ( 'NONE', #107633, #127997, #6858 ) ;
#112905 = DIRECTION ( 'NONE',  ( 0.7071067811865487940, 0.7071067811865463515, 0.000000000000000000 ) ) ;
#112907 = LINE ( 'NONE', #33939, #40768 ) ;
#112908 = FACE_OUTER_BOUND ( 'NONE', #41867, .T. ) ;
#112909 = LINE ( 'NONE', #55697, #40968 ) ;
#112910 = EDGE_CURVE ( 'NONE', #65084, #57387, #35242, .T. ) ;
#112911 = CARTESIAN_POINT ( 'NONE',  ( -16.49999999999988276, 10.94296225409025247, -9.576120664313295450 ) ) ;
#112912 = ORIENTED_EDGE ( 'NONE', *, *, #141831, .T. ) ;
#112913 = ORIENTED_EDGE ( 'NONE', *, *, #66274, .T. ) ;
#112914 = ORIENTED_EDGE ( 'NONE', *, *, #87439, .F. ) ;
#112915 = CARTESIAN_POINT ( 'NONE',  ( 87.50043019189810423, -3.055000000000002380, 5.291415217122920289 ) ) ;
#112916 = VECTOR ( 'NONE', #111603, 1000.000000000000000 ) ;
#112917 = ORIENTED_EDGE ( 'NONE', *, *, #126790, .T. ) ;
#112918 = CARTESIAN_POINT ( 'NONE',  ( -60.18398860626900415, 28.73617430169829490, 5.000000000000000000 ) ) ;
#112919 = LINE ( 'NONE', #80325, #98839 ) ;
#112920 = FACE_OUTER_BOUND ( 'NONE', #119293, .T. ) ;
#112921 = CARTESIAN_POINT ( 'NONE',  ( 8.999999999999932498, -0.4125381241607412042, 4.000000000000000000 ) ) ;
#112922 = ORIENTED_EDGE ( 'NONE', *, *, #79951, .F. ) ;
#112923 = CARTESIAN_POINT ( 'NONE',  ( -53.99451991528749062, 28.92564299267975869, 4.000000000000000000 ) ) ;
#112924 = DIRECTION ( 'NONE',  ( 0.7071067811865487940, 0.7071067811865463515, 0.000000000000000000 ) ) ;
#112925 = CARTESIAN_POINT ( 'NONE',  ( 81.28709685856478018, 3.054999999999997495, 5.291415217122919401 ) ) ;
#112926 = ORIENTED_EDGE ( 'NONE', *, *, #66917, .T. ) ;
#112927 = CARTESIAN_POINT ( 'NONE',  ( 36.48921356237310221, -27.52281430457080802, 5.000000000000000000 ) ) ;
#112928 = EDGE_CURVE ( 'NONE', #77145, #31809, #133813, .T. ) ;
#112929 = CARTESIAN_POINT ( 'NONE',  ( -13.49999999999990763, 10.94296225409025247, -9.576120664313284792 ) ) ;
#112930 = ORIENTED_EDGE ( 'NONE', *, *, #39678, .T. ) ;
#112931 = ORIENTED_EDGE ( 'NONE', *, *, #6004, .F. ) ;
#112932 = DIRECTION ( 'NONE',  ( 0.000000000000000000, 0.000000000000000000, -1.000000000000000000 ) ) ;
#112933 = LINE ( 'NONE', #13599, #73234 ) ;
#112934 = CARTESIAN_POINT ( 'NONE',  ( 22.96290314143522338, -3.967499999999994476, 6.871911579029513106 ) ) ;
#112935 = DIRECTION ( 'NONE',  ( -0.6830127018922180770, -0.6830127018922204085, -0.2588190451025213501 ) ) ;
#112936 = LINE ( 'NONE', #3440, #101164 ) ;
#112937 = ADVANCED_FACE ( 'NONE', ( #57705 ), #59149, .F. ) ;
#112938 = DIRECTION ( 'NONE',  ( 0.3543493200069163240, -0.000000000000000000, 0.9351131265310288487 ) ) ;
#112939 = DIRECTION ( 'NONE',  ( -0.6830127018922181881, 0.6830127018922202975, -0.2588190451025214056 ) ) ;
#112940 = ORIENTED_EDGE ( 'NONE', *, *, #127423, .T. ) ;
#112941 = AXIS2_PLACEMENT_3D ( 'NONE', #49706, #93179, #117747 ) ;
#112942 = ORIENTED_EDGE ( 'NONE', *, *, #83966, .T. ) ;
#112943 = DIRECTION ( 'NONE',  ( -0.6830127018922180770, -0.6830127018922204085, -0.2588190451025213501 ) ) ;
#112945 = ORIENTED_EDGE ( 'NONE', *, *, #46492, .T. ) ;
#112944 = ADVANCED_FACE ( 'NONE', ( #135269 ), #35955, .T. ) ;
#112946 = ORIENTED_EDGE ( 'NONE', *, *, #83510, .T. ) ;
#112947 = VECTOR ( 'NONE', #48023, 1000.000000000000000 ) ;
#112948 = DIRECTION ( 'NONE',  ( 0.000000000000000000, -1.000000000000000000, 0.000000000000000000 ) ) ;
#112949 = ORIENTED_EDGE ( 'NONE', *, *, #34574, .T. ) ;
#112950 = CARTESIAN_POINT ( 'NONE',  ( 4.499999999999971578, 22.01701374228155927, 2.453858888625620516 ) ) ;
#112951 = DIRECTION ( 'NONE',  ( -0.7071067811865487940, 0.7071067811865463515, -0.000000000000000000 ) ) ;
#112952 = EDGE_CURVE ( 'NONE', #119924, #47238, #113466, .T. ) ;
#112953 = PLANE ( 'NONE',  #138747 ) ;
#112954 = AXIS2_PLACEMENT_3D ( 'NONE', #18468, #62747, #106931 ) ;
#112955 = DIRECTION ( 'NONE',  ( 1.000000000000000000, 0.000000000000000000, 0.000000000000000000 ) ) ;
#112956 = ORIENTED_EDGE ( 'NONE', *, *, #52070, .F. ) ;
#112957 = FILL_AREA_STYLE ('',( #23064 ) ) ;
#112958 = VECTOR ( 'NONE', #82149, 1000.000000000000000 ) ;
#112959 = ORIENTED_EDGE ( 'NONE', *, *, #46848, .T. ) ;
#112961 = EDGE_CURVE ( 'NONE', #81784, #109346, #136652, .T. ) ;
#112960 = CARTESIAN_POINT ( 'NONE',  ( 34.42499999999998295, -21.72500000000000142, 0.4999999999999995559 ) ) ;
#112962 = ORIENTED_EDGE ( 'NONE', *, *, #115262, .T. ) ;
#112963 = CARTESIAN_POINT ( 'NONE',  ( 34.42499999999998295, 22.22500000000000142, 5.000000000000000000 ) ) ;
#112964 = VERTEX_POINT ( 'NONE', #86405 ) ;
#112965 = DIRECTION ( 'NONE',  ( -0.000000000000000000, 0.000000000000000000, 1.000000000000000000 ) ) ;
#112966 = VERTEX_POINT ( 'NONE', #142219 ) ;
#112967 = ORIENTED_EDGE ( 'NONE', *, *, #75289, .T. ) ;
#112968 = CONICAL_SURFACE ( 'NONE', #22696, 2.055000000000000604, 0.9599310885968764806 ) ;
#112969 = ORIENTED_EDGE ( 'NONE', *, *, #97898, .F. ) ;
#112970 =( GEOMETRIC_REPRESENTATION_CONTEXT ( 3 ) GLOBAL_UNCERTAINTY_ASSIGNED_CONTEXT ( ( #49040 ) ) GLOBAL_UNIT_ASSIGNED_CONTEXT ( ( #95115, #73396, #29154 ) ) REPRESENTATION_CONTEXT ( 'NONE', 'WORKASPACE' ) );
#112971 = CARTESIAN_POINT ( 'NONE',  ( -24.18398860626899705, 28.73617430169804265, 5.000000000000000000 ) ) ;
#112972 = ADVANCED_FACE ( 'NONE', ( #108816 ), #131318, .T. ) ;
#112973 = DIRECTION ( 'NONE',  ( -0.7071067811865487940, 0.7071067811865463515, -0.000000000000000000 ) ) ;
#112974 = DIRECTION ( 'NONE',  ( -0.000000000000000000, 0.3543493200069153248, 0.9351131265310292928 ) ) ;
#112975 = CARTESIAN_POINT ( 'NONE',  ( 117.9795968585647756, 6.109999999999999432, 1.637169565754164280 ) ) ;
#112976 = DIRECTION ( 'NONE',  ( -0.7071067811865486830, 0.7071067811865464625, 0.000000000000000000 ) ) ;
#112977 = CARTESIAN_POINT ( 'NONE',  ( -34.42500000000001137, -22.22500000000000142, 5.000000000000000000 ) ) ;
#112978 = FACE_OUTER_BOUND ( 'NONE', #13772, .T. ) ;
#112979 = CARTESIAN_POINT ( 'NONE',  ( 3.473360963642126098, -5.240707523384232402, 16.25846745537496574 ) ) ;
#112980 = ORIENTED_EDGE ( 'NONE', *, *, #101526, .F. ) ;
#112981 = EDGE_CURVE ( 'NONE', #20866, #52318, #93865, .T. ) ;
#112982 = DIRECTION ( 'NONE',  ( 0.000000000000000000, -1.000000000000000000, 0.000000000000000000 ) ) ;
#112983 = EDGE_LOOP ( 'NONE', ( #38947, #49016, #113047, #37889 ) ) ;
#112984 = ORIENTED_EDGE ( 'NONE', *, *, #111372, .F. ) ;
#112985 = DIRECTION ( 'NONE',  ( -0.7071067811865486830, 0.7071067811865464625, -0.000000000000000000 ) ) ;
#112986 = EDGE_LOOP ( 'NONE', ( #65866, #32110, #122792, #5004 ) ) ;
#112987 = VECTOR ( 'NONE', #109643, 1000.000000000000000 ) ;
#112988 = FACE_OUTER_BOUND ( 'NONE', #23225, .T. ) ;
#112989 = DIRECTION ( 'NONE',  ( -0.7071067811865487940, 0.7071067811865463515, -0.000000000000000000 ) ) ;
#112990 = EDGE_CURVE ( 'NONE', #71167, #139608, #40753, .T. ) ;
#112991 = CARTESIAN_POINT ( 'NONE',  ( -15.06442625288296178, 7.619305877646137759, 4.652854425660915894 ) ) ;
#112992 = ORIENTED_EDGE ( 'NONE', *, *, #110730, .F. ) ;
#112993 = COLOUR_RGB ( '', 0.72549020, 0.75294118, 0.79215686) ;
#112994 = DIRECTION ( 'NONE',  ( -0.7071067811865486830, -0.7071067811865464625, 0.000000000000000000 ) ) ;
#112995 = ORIENTED_EDGE ( 'NONE', *, *, #111759, .T. ) ;
#112996 = CARTESIAN_POINT ( 'NONE',  ( 51.18398860626899705, 28.73617430169823095, 5.000000000000000000 ) ) ;
#112997 = CARTESIAN_POINT ( 'NONE',  ( 32.87956980810189123, 3.967499999999998916, 6.871911579029510442 ) ) ;
#112998 = ORIENTED_EDGE ( 'NONE', *, *, #73920, .T. ) ;
#112999 = PLANE ( 'NONE',  #18130 ) ;
#113000 = CARTESIAN_POINT ( 'NONE',  ( 0.000000000000000000, 0.000000000000000000, 5.000000000000000000 ) ) ;
#113001 = ORIENTED_EDGE ( 'NONE', *, *, #72172, .F. ) ;
#113002 = ORIENTED_EDGE ( 'NONE', *, *, #114830, .F. ) ;
#113003 = ORIENTED_EDGE ( 'NONE', *, *, #95309, .F. ) ;
#113004 = CARTESIAN_POINT ( 'NONE',  ( 4.499999999999976019, 13.08746187583911080, 4.000000000000000000 ) ) ;
#113005 = FACE_OUTER_BOUND ( 'NONE', #107076, .T. ) ;
#113006 = LINE ( 'NONE', #13675, #121471 ) ;
#113007 = CARTESIAN_POINT ( 'NONE',  ( 5.999999999999955591, -18.03360074219755660, 5.000000000000000000 ) ) ;
#113008 = ORIENTED_EDGE ( 'NONE', *, *, #119303, .T. ) ;
#113009 = LINE ( 'NONE', #104257, #20758 ) ;
#113010 = CIRCLE ( 'NONE', #94487, 2.500000000000000888 ) ;
#113011 =( NAMED_UNIT ( * ) PLANE_ANGLE_UNIT ( ) SI_UNIT ( $, .RADIAN. ) );
#113012 = LINE ( 'NONE', #27421, #106713 ) ;
#113013 = DIRECTION ( 'NONE',  ( 1.000000000000000000, 0.000000000000000000, 0.000000000000000000 ) ) ;
#113014 = EDGE_LOOP ( 'NONE', ( #99358, #133375, #30812, #1118 ) ) ;
#113015 = DIRECTION ( 'NONE',  ( 0.6830127018922180770, -0.6830127018922204085, -0.2588190451025213501 ) ) ;
#113016 = ORIENTED_EDGE ( 'NONE', *, *, #71029, .T. ) ;
#113018 = ORIENTED_EDGE ( 'NONE', *, *, #122900, .T. ) ;
#113017 = CARTESIAN_POINT ( 'NONE',  ( -36.18398860626899705, 28.73617430169812437, 5.000000000000000000 ) ) ;
#113019 = VERTEX_POINT ( 'NONE', #140076 ) ;
#113020 = DIRECTION ( 'NONE',  ( -0.3543493200069162685, -0.000000000000000000, -0.9351131265310288487 ) ) ;
#113021 = PLANE ( 'NONE',  #92368 ) ;
#113022 = ORIENTED_EDGE ( 'NONE', *, *, #66125, .F. ) ;
#113023 = CARTESIAN_POINT ( 'NONE',  ( -34.49999999999975131, 9.054329344830845727, 4.994342998332165884 ) ) ;
#113024 = UNCERTAINTY_MEASURE_WITH_UNIT (LENGTH_MEASURE( 1.000000000000000082E-05 ), #133699, 'distance_accuracy_value', 'NONE');
#113025 = EDGE_LOOP ( 'NONE', ( #77556, #135378, #80539, #7827 ) ) ;
#113026 = DIRECTION ( 'NONE',  ( -0.7071067811865486830, -0.7071067811865464625, 0.000000000000000000 ) ) ;
#113027 = CARTESIAN_POINT ( 'NONE',  ( 25.97159235450331849, 3.061616997868380183E-16, -2.500000000000001332 ) ) ;
#113028 = EDGE_CURVE ( 'NONE', #9322, #98313, #84958, .T. ) ;
#113029 = LINE ( 'NONE', #13703, #13799 ) ;
#113030 = VECTOR ( 'NONE', #22028, 1000.000000000000000 ) ;
#113031 = DIRECTION ( 'NONE',  ( -0.000000000000000000, -0.3543493200069152693, 0.9351131265310292928 ) ) ;
#113032 = EDGE_CURVE ( 'NONE', #42509, #69887, #15550, .T. ) ;
#113033 = DIRECTION ( 'NONE',  ( 0.6830127018922181881, 0.6830127018922202975, -0.2588190451025214056 ) ) ;
#113034 = DIRECTION ( 'NONE',  ( -0.000000000000000000, -0.3543493200069152693, 0.9351131265310292928 ) ) ;
#113035 = CYLINDRICAL_SURFACE ( 'NONE', #23972, 2.500000000000000000 ) ;
#113036 = EDGE_CURVE ( 'NONE', #51846, #39954, #107419, .T. ) ;
#113037 = CARTESIAN_POINT ( 'NONE',  ( 18.06206980810188867, -7.934999999999991616, -2.126176841940955242 ) ) ;
#113038 = PLANE ( 'NONE',  #125460 ) ;
#113039 = CARTESIAN_POINT ( 'NONE',  ( 0.000000000000000000, 0.000000000000000000, 0.000000000000000000 ) ) ;
#113040 = DIRECTION ( 'NONE',  ( -0.6830127018922181881, 0.6830127018922202975, -0.2588190451025214056 ) ) ;
#113042 = EDGE_CURVE ( 'NONE', #17152, #130600, #60571, .T. ) ;
#113041 = CARTESIAN_POINT ( 'NONE',  ( -25.49999999999982236, -10.04351517176480613, -1.623559851933882081 ) ) ;
#113043 = ORIENTED_EDGE ( 'NONE', *, *, #38510, .T. ) ;
#113044 = VERTEX_POINT ( 'NONE', #119687 ) ;
#113045 = CARTESIAN_POINT ( 'NONE',  ( 93.45833333333334281, 3.974999999999997424, 6.884901960086288852 ) ) ;
#113046 = EDGE_LOOP ( 'NONE', ( #51625, #128279, #39043, #78409 ) ) ;
#113047 = ORIENTED_EDGE ( 'NONE', *, *, #11363, .T. ) ;
#113048 = AXIS2_PLACEMENT_3D ( 'NONE', #25457, #14600, #45131 ) ;
#113049 = EDGE_LOOP ( 'NONE', ( #134574, #36867, #8737, #119918 ) ) ;
#113050 = CARTESIAN_POINT ( 'NONE',  ( -25.62823445044369208, -8.240707523384207533, 11.38925528200758386 ) ) ;
#113051 = DIRECTION ( 'NONE',  ( -1.000000000000000000, -1.424048422229243832E-14, 0.000000000000000000 ) ) ;
#113052 = CARTESIAN_POINT ( 'NONE',  ( 10.91209335768108168, 8.448398485916262857, 4.344958105531096848 ) ) ;
#113053 = EDGE_LOOP ( 'NONE', ( #119852, #69657, #116944, #93586 ) ) ;
#113054 = VECTOR ( 'NONE', #60078, 1000.000000000000000 ) ;
#113055 = LINE ( 'NONE', #113787, #136572 ) ;
#113056 = CARTESIAN_POINT ( 'NONE',  ( 7.139999999999991687, -35.76999999999998892, -12.10072711459627293 ) ) ;
#113057 = VECTOR ( 'NONE', #37361, 1000.000000000000000 ) ;
#113058 = EDGE_CURVE ( 'NONE', #54027, #64418, #20388, .T. ) ;
#113059 = PLANE ( 'NONE',  #34862 ) ;
#113060 = CARTESIAN_POINT ( 'NONE',  ( -48.48921356237309510, -27.52281430457089328, 5.000000000000000000 ) ) ;
#113061 = EDGE_CURVE ( 'NONE', #92120, #54748, #64631, .T. ) ;
#113062 = VECTOR ( 'NONE', #30292, 999.9999999999998863 ) ;
#113063 = DIRECTION ( 'NONE',  ( -0.000000000000000000, 0.000000000000000000, 1.000000000000000000 ) ) ;
#113064 = CARTESIAN_POINT ( 'NONE',  ( 54.48921356237310221, -27.52281430457093236, 5.000000000000000000 ) ) ;
#113065 = CARTESIAN_POINT ( 'NONE',  ( 151.4000000000000057, -17.48000000000005016, -34.92499999999998295 ) ) ;
#113066 = DIRECTION ( 'NONE',  ( -0.7071067811865486830, 0.7071067811865464625, 0.000000000000000000 ) ) ;
#113068 = CARTESIAN_POINT ( 'NONE',  ( -25.39999999999996305, 0.000000000000000000, 2.500000000000000000 ) ) ;
#113067 = VECTOR ( 'NONE', #33336, 999.9999999999998863 ) ;
#113069 = LINE ( 'NONE', #13739, #7664 ) ;
#113070 = LINE ( 'NONE', #13740, #119482 ) ;
#113071 = AXIS2_PLACEMENT_3D ( 'NONE', #129005, #84796, #84118 ) ;
#113072 = PLANE ( 'NONE',  #29065 ) ;
#113073 = EDGE_CURVE ( 'NONE', #5941, #50102, #30600, .T. ) ;
#113074 = CARTESIAN_POINT ( 'NONE',  ( 52.69985579143948939, -48.99436351328167660, 39.52330221398018750 ) ) ;
#113075 = ORIENTED_EDGE ( 'NONE', *, *, #107656, .T. ) ;
#113076 = VERTEX_POINT ( 'NONE', #8078 ) ;
#113077 = CARTESIAN_POINT ( 'NONE',  ( 108.3545968585647472, -1.637169565754161615, 6.110000000000000320 ) ) ;
#113078 = EDGE_LOOP ( 'NONE', ( #96139, #52149, #95685, #105268 ) ) ;
#113079 = PLANE ( 'NONE',  #3800 ) ;
#113080 = EDGE_CURVE ( 'NONE', #17479, #11535, #129890, .T. ) ;
#113081 = VECTOR ( 'NONE', #34966, 1000.000000000000000 ) ;
#113082 = DIRECTION ( 'NONE',  ( 0.7071067811865486830, -0.7071067811865464625, -0.000000000000000000 ) ) ;
#113084 =( BOUNDED_CURVE ( )  B_SPLINE_CURVE ( 3, ( #82987, #61283, #40222, #117706 ),
 .UNSPECIFIED., .F., .F. ) 
 B_SPLINE_CURVE_WITH_KNOTS ( ( 4, 4 ),
 ( 5.920967161967927161, 7.341195215986639155 ),
 .UNSPECIFIED. ) 
 CURVE ( )  GEOMETRIC_REPRESENTATION_ITEM ( )  RATIONAL_B_SPLINE_CURVE ( ( 1.000000000000000000, 0.8388583629366609395, 0.8388583629366609395, 1.000000000000000000 ) ) 
 REPRESENTATION_ITEM ( '' )  );
#113083 = DIRECTION ( 'NONE',  ( 0.7071067811865487940, -0.7071067811865463515, 0.000000000000000000 ) ) ;
#113085 = VECTOR ( 'NONE', #47146, 1000.000000000000114 ) ;
#113086 = CARTESIAN_POINT ( 'NONE',  ( 109.8704301918981230, -3.055000000000001492, 5.291415217122917625 ) ) ;
#113087 = EDGE_LOOP ( 'NONE', ( #110973, #22218, #59839, #52309 ) ) ;
#113088 = VERTEX_POINT ( 'NONE', #93159 ) ;
#113090 = ADVANCED_FACE ( 'NONE', ( #53783 ), #19691, .T. ) ;
#113089 = CARTESIAN_POINT ( 'NONE',  ( -12.20000000000000284, -25.33999999999998209, 15.47043909406156104 ) ) ;
#113091 = CIRCLE ( 'NONE', #131638, 1.000000000000000888 ) ;
#113092 = CARTESIAN_POINT ( 'NONE',  ( 34.42499999999998295, 21.72500000000000142, 0.000000000000000000 ) ) ;
#113093 =( BOUNDED_CURVE ( )  B_SPLINE_CURVE ( 3, ( #42368, #26647, #140238, #119176 ),
 .UNSPECIFIED., .F., .T. ) 
 B_SPLINE_CURVE_WITH_KNOTS ( ( 4, 4 ),
 ( 4.350170835173027939, 4.500739107949208950 ),
 .UNSPECIFIED. ) 
 CURVE ( )  GEOMETRIC_REPRESENTATION_ITEM ( )  RATIONAL_B_SPLINE_CURVE ( ( 1.000000000000000000, 0.9981116584018958626, 0.9981116584018958626, 1.000000000000000000 ) ) 
 REPRESENTATION_ITEM ( '' )  );
#113094 = VECTOR ( 'NONE', #31737, 1000.000000000000000 ) ;
#113095 = MECHANICAL_DESIGN_GEOMETRIC_PRESENTATION_REPRESENTATION (  '', ( #126957 ), #25122 ) ;
#113096 = EDGE_LOOP ( 'NONE', ( #25178, #127987, #1817, #24002 ) ) ;
#113097 = ORIENTED_EDGE ( 'NONE', *, *, #5155, .F. ) ;
#113098 = ORIENTED_EDGE ( 'NONE', *, *, #126985, .T. ) ;
#113099 = DIRECTION ( 'NONE',  ( -0.3543493200069162685, -0.000000000000000000, -0.9351131265310288487 ) ) ;
#113100 = CARTESIAN_POINT ( 'NONE',  ( 0.6504031414352192675, 7.934999999999988951, -2.126176841940961904 ) ) ;
#113101 = ADVANCED_FACE ( 'NONE', ( #85652 ), #104743, .T. ) ;
#113102 = CARTESIAN_POINT ( 'NONE',  ( 27.47459685856478018, 1.637169565754164058, -6.109999999999996767 ) ) ;
#113103 = VERTEX_POINT ( 'NONE', #63930 ) ;
#113104 = ORIENTED_EDGE ( 'NONE', *, *, #16040, .F. ) ;
#113105 = LINE ( 'NONE', #137748, #138135 ) ;
#113106 = VERTEX_POINT ( 'NONE', #108101 ) ;
#113107 = ORIENTED_EDGE ( 'NONE', *, *, #54500, .F. ) ;
#113108 = VECTOR ( 'NONE', #4721, 1000.000000000000227 ) ;
#113109 = ORIENTED_EDGE ( 'NONE', *, *, #122077, .F. ) ;
#113110 = VECTOR ( 'NONE', #16943, 999.9999999999998863 ) ;
#113111 = DIRECTION ( 'NONE',  ( -0.7071067811865486830, 0.7071067811865464625, 0.000000000000000000 ) ) ;
#113112 = DIRECTION ( 'NONE',  ( -1.000000000000000000, -0.000000000000000000, -0.000000000000000000 ) ) ;
#113113 = CARTESIAN_POINT ( 'NONE',  ( 78.53752705046289861, -9.735942053221456900E-16, 7.949999999999998401 ) ) ;
#113114 = ORIENTED_EDGE ( 'NONE', *, *, #7950, .T. ) ;
#113115 = LINE ( 'NONE', #70393, #69208 ) ;
#113116 = EDGE_CURVE ( 'NONE', #124115, #99111, #27175, .T. ) ;
#113117 = CARTESIAN_POINT ( 'NONE',  ( 8.510786437626906675, -27.52281430457049183, 5.000000000000000000 ) ) ;
#113118 =( NAMED_UNIT ( * ) PLANE_ANGLE_UNIT ( ) SI_UNIT ( $, .RADIAN. ) );
#113119 = FACE_BOUND ( 'NONE', #17385, .T. ) ;
#113120 = ORIENTED_EDGE ( 'NONE', *, *, #13172, .T. ) ;
#113121 = CARTESIAN_POINT ( 'NONE',  ( 64.53752705046289861, -9.735942053221456900E-16, 7.949999999999998401 ) ) ;
#113123 = EDGE_CURVE ( 'NONE', #12722, #25035, #16271, .T. ) ;
#113122 = FACE_OUTER_BOUND ( 'NONE', #1516, .T. ) ;
#113124 = FACE_OUTER_BOUND ( 'NONE', #129788, .T. ) ;
#113125 = EDGE_LOOP ( 'NONE', ( #103387, #66098, #138812, #122181 ) ) ;
#113126 = LINE ( 'NONE', #125457, #115209 ) ;
#113127 = ORIENTED_EDGE ( 'NONE', *, *, #114540, .F. ) ;
#113128 = VERTEX_POINT ( 'NONE', #130634 ) ;
#113129 = VERTEX_POINT ( 'NONE', #9503 ) ;
#113130 = CARTESIAN_POINT ( 'NONE',  ( 38.41209685856478018, 5.291415217122921177, -3.054999999999994831 ) ) ;
#113131 = ORIENTED_EDGE ( 'NONE', *, *, #8587, .T. ) ;
#113132 = LINE ( 'NONE', #2948, #78862 ) ;
#113133 = DIRECTION ( 'NONE',  ( -0.7071067811865486830, -0.7071067811865464625, 0.000000000000000000 ) ) ;
#113134 = ORIENTED_EDGE ( 'NONE', *, *, #41635, .F. ) ;
#113135 = DIRECTION ( 'NONE',  ( -0.7071067811865486830, -0.7071067811865464625, 0.000000000000000000 ) ) ;
#113136 = LINE ( 'NONE', #34906, #6209 ) ;
#113137 = CARTESIAN_POINT ( 'NONE',  ( -12.29974487139158512, -27.71228299555214747, 4.000000000000000000 ) ) ;
#113138 = EDGE_CURVE ( 'NONE', #114619, #36553, #97980, .T. ) ;
#113139 = DIRECTION ( 'NONE',  ( -0.7071067811865486830, 0.7071067811865464625, 0.000000000000000000 ) ) ;
#113140 = FACE_OUTER_BOUND ( 'NONE', #113280, .T. ) ;
#113141 = ORIENTED_EDGE ( 'NONE', *, *, #43361, .T. ) ;
#113142 = ORIENTED_EDGE ( 'NONE', *, *, #24351, .T. ) ;
#113143 = EDGE_LOOP ( 'NONE', ( #35546, #9159, #284, #68947 ) ) ;
#113144 = ORIENTED_EDGE ( 'NONE', *, *, #130272, .T. ) ;
#113145 = PLANE ( 'NONE',  #49506 ) ;
#113146 = VECTOR ( 'NONE', #88749, 1000.000000000000000 ) ;
#113147 = AXIS2_PLACEMENT_3D ( 'NONE', #19940, #41710, #76503 ) ;
#113148 = ORIENTED_EDGE ( 'NONE', *, *, #33201, .T. ) ;
#113149 = VECTOR ( 'NONE', #23985, 1000.000000000000000 ) ;
#113151 = VERTEX_POINT ( 'NONE', #21120 ) ;
#113150 = VECTOR ( 'NONE', #86226, 1000.000000000000000 ) ;
#113152 = PLANE ( 'NONE',  #87357 ) ;
#113153 = EDGE_CURVE ( 'NONE', #63812, #37944, #2181, .T. ) ;
#113154 = EDGE_CURVE ( 'NONE', #96033, #11916, #143185, .T. ) ;
#113155 = FACE_OUTER_BOUND ( 'NONE', #85214, .T. ) ;
#113156 = VERTEX_POINT ( 'NONE', #76229 ) ;
#113157 = CARTESIAN_POINT ( 'NONE',  ( 21.29974487139158512, -27.71228299555221142, 4.000000000000000000 ) ) ;
#113158 = VECTOR ( 'NONE', #52714, 1000.000000000000000 ) ;
#113160 = ORIENTED_EDGE ( 'NONE', *, *, #122037, .T. ) ;
#113159 = VECTOR ( 'NONE', #95914, 1000.000000000000000 ) ;
#113161 = CARTESIAN_POINT ( 'NONE',  ( 22.49999999999984368, -1.695981523266237634, 4.571483868317931964 ) ) ;
#113162 = CARTESIAN_POINT ( 'NONE',  ( 28.65040314143521982, 7.934999999999989839, -2.126176841940961904 ) ) ;
#113163 = CARTESIAN_POINT ( 'NONE',  ( 2.254569808101886341, -6.871911579029512218, 3.967499999999996252 ) ) ;
#113164 = ORIENTED_EDGE ( 'NONE', *, *, #65820, .F. ) ;
#113165 = CARTESIAN_POINT ( 'NONE',  ( 109.1412635252314374, 4.472830434245837594, 4.472830434245841147 ) ) ;
#113166 = CARTESIAN_POINT ( 'NONE',  ( -9.299744871391588674, -27.71228299555212971, 4.000000000000000000 ) ) ;
#113167 = DIRECTION ( 'NONE',  ( 0.7071067811865487940, -0.7071067811865463515, 0.000000000000000000 ) ) ;
#113168 = ORIENTED_EDGE ( 'NONE', *, *, #76954, .F. ) ;
#113169 = CARTESIAN_POINT ( 'NONE',  ( -24.18398860626899705, 28.73617430169804265, 5.000000000000000000 ) ) ;
#113171 = ORIENTED_EDGE ( 'NONE', *, *, #58883, .T. ) ;
#113170 = LINE ( 'NONE', #78429, #125923 ) ;
#113172 = VECTOR ( 'NONE', #26214, 1000.000000000000114 ) ;
#113173 = FACE_OUTER_BOUND ( 'NONE', #94763, .T. ) ;
#113174 = DIRECTION ( 'NONE',  ( 0.3543493200069162685, -0.000000000000000000, -0.9351131265310288487 ) ) ;
#113175 = DIRECTION ( 'NONE',  ( -0.7071067811865486830, 0.7071067811865464625, 0.000000000000000000 ) ) ;
#113176 = FACE_OUTER_BOUND ( 'NONE', #38452, .T. ) ;
#113177 = DIRECTION ( 'NONE',  ( -1.000000000000000000, -0.000000000000000000, -0.000000000000000000 ) ) ;
#113178 = EDGE_CURVE ( 'NONE', #9024, #83531, #36, .T. ) ;
#113179 = ORIENTED_EDGE ( 'NONE', *, *, #77644, .F. ) ;
#113180 = CARTESIAN_POINT ( 'NONE',  ( -26.99999999999980815, 16.55218569542899587, 5.000000000000000000 ) ) ;
#113181 = VECTOR ( 'NONE', #96798, 999.9999999999998863 ) ;
#113182 = CARTESIAN_POINT ( 'NONE',  ( 2.510786437626908008, -27.52281430457053446, 5.000000000000000000 ) ) ;
#113183 = DIRECTION ( 'NONE',  ( 0.6830127018922181881, 0.6830127018922202975, -0.2588190451025214056 ) ) ;
#113184 = ORIENTED_EDGE ( 'NONE', *, *, #120577, .F. ) ;
#113185 = VECTOR ( 'NONE', #54807, 1000.000000000000000 ) ;
#113187 = AXIS2_PLACEMENT_3D ( 'NONE', #14077, #59765, #58377 ) ;
#113186 = LINE ( 'NONE', #13149, #49328 ) ;
#113188 = ORIENTED_EDGE ( 'NONE', *, *, #122873, .T. ) ;
#113189 = MECHANICAL_DESIGN_GEOMETRIC_PRESENTATION_REPRESENTATION (  '', ( #127064 ), #141030 ) ;
#113191 = VERTEX_POINT ( 'NONE', #11641 ) ;
#113190 = CARTESIAN_POINT ( 'NONE',  ( -27.18398860626900060, 28.73617430169806042, 5.000000000000000000 ) ) ;
#113192 = EDGE_LOOP ( 'NONE', ( #112163, #40613, #12000 ) ) ;
#113193 = CARTESIAN_POINT ( 'NONE',  ( 5.178098103386369111, 13.15750331121097716, -24.81904025722317897 ) ) ;
#113194 =( NAMED_UNIT ( * ) PLANE_ANGLE_UNIT ( ) SI_UNIT ( $, .RADIAN. ) );
#113195 = EDGE_LOOP ( 'NONE', ( #22426, #85584, #112611, #83703 ) ) ;
#113196 = VECTOR ( 'NONE', #16682, 1000.000000000000000 ) ;
#113197 = ADVANCED_FACE ( 'NONE', ( #46503 ), #87802, .T. ) ;
#113198 = CARTESIAN_POINT ( 'NONE',  ( 32.29289321881323360, -6.740707523384209310, 5.000000000000000000 ) ) ;
#113199 = EDGE_CURVE ( 'NONE', #78047, #50562, #78373, .T. ) ;
#113200 = DIRECTION ( 'NONE',  ( 0.7071067811865487940, 0.7071067811865463515, -0.000000000000000000 ) ) ;
#113201 = ORIENTED_EDGE ( 'NONE', *, *, #70637, .F. ) ;
#113202 = ADVANCED_FACE ( 'NONE', ( #54495 ), #29848, .T. ) ;
#113203 = CARTESIAN_POINT ( 'NONE',  ( -83.99451991528748351, 28.92564299267996830, 4.000000000000000000 ) ) ;
#113204 = DIRECTION ( 'NONE',  ( 0.7071067811865486830, -0.7071067811865464625, -0.000000000000000000 ) ) ;
#113205 = CARTESIAN_POINT ( 'NONE',  ( -23.00492477221180110, -5.240707523384232402, 12.38332538355501100 ) ) ;
#113206 = VECTOR ( 'NONE', #108172, 1000.000000000000000 ) ;
#113207 = DIRECTION ( 'NONE',  ( 0.6830127018922180770, -0.6830127018922204085, -0.2588190451025214056 ) ) ;
#113208 = FACE_OUTER_BOUND ( 'NONE', #46047, .T. ) ;
#113209 = DIRECTION ( 'NONE',  ( -0.000000000000000000, 0.3543493200069153248, 0.9351131265310292928 ) ) ;
#113211 = ADVANCED_FACE ( 'NONE', ( #142905 ), #55195, .F. ) ;
#113210 = PLANE ( 'NONE',  #133402 ) ;
#113213 = ADVANCED_FACE ( 'NONE', ( #110953 ), #123325, .F. ) ;
#113212 = VERTEX_POINT ( 'NONE', #79118 ) ;
#113214 = ORIENTED_EDGE ( 'NONE', *, *, #104328, .T. ) ;
#113215 = ORIENTED_EDGE ( 'NONE', *, *, #69240, .F. ) ;
#113216 = CARTESIAN_POINT ( 'NONE',  ( 121.4583333333333286, 3.974999999999997424, 6.884901960086288852 ) ) ;
#113217 = ORIENTED_EDGE ( 'NONE', *, *, #10697, .T. ) ;
#113218 = ORIENTED_EDGE ( 'NONE', *, *, #94378, .F. ) ;
#113219 = VERTEX_POINT ( 'NONE', #47908 ) ;
#113220 = CARTESIAN_POINT ( 'NONE',  ( 0.7210889554053107053, -7.059391798541635232, -2.151955493142619247 ) ) ;
#113221 = DIRECTION ( 'NONE',  ( 2.781805975412906507E-17, 0.3543493200069153248, 0.9351131265310292928 ) ) ;
#113222 = ORIENTED_EDGE ( 'NONE', *, *, #51762, .T. ) ;
#113223 = CARTESIAN_POINT ( 'NONE',  ( 18.70710678118640757, -18.74070752338409562, 5.000000000000000000 ) ) ;
#113224 = CARTESIAN_POINT ( 'NONE',  ( -25.39999999999996305, 0.000000000000000000, 0.000000000000000000 ) ) ;
#113225 = LINE ( 'NONE', #57460, #113512 ) ;
#113226 = EDGE_CURVE ( 'NONE', #54347, #76671, #26829, .T. ) ;
#113227 = CARTESIAN_POINT ( 'NONE',  ( 19.05000000000000071, 3.174999999999997158, 5.000000000000000000 ) ) ;
#113228 = CARTESIAN_POINT ( 'NONE',  ( 115.2087635252314470, -7.482591942790329030E-16, 6.110000000000001208 ) ) ;
#113229 = VERTEX_POINT ( 'NONE', #71078 ) ;
#113230 = EDGE_CURVE ( 'NONE', #87384, #28061, #2932, .T. ) ;
#113231 = LINE ( 'NONE', #58208, #122821 ) ;
#113232 = DIRECTION ( 'NONE',  ( 0.7071067811865487940, -0.7071067811865463515, 0.000000000000000000 ) ) ;
#113233 = DIRECTION ( 'NONE',  ( -0.000000000000000000, -0.3543493200069152693, 0.9351131265310292928 ) ) ;
#113234 = CARTESIAN_POINT ( 'NONE',  ( 5.719980320105927163, 0.7592924766157069794, 14.27032725228010612 ) ) ;
#113235 = LINE ( 'NONE', #3730, #79808 ) ;
#113236 = CARTESIAN_POINT ( 'NONE',  ( 3.398789304146613954, 4.202752102959690472E-16, 0.000000000000000000 ) ) ;
#113237 = CARTESIAN_POINT ( 'NONE',  ( 19.00193056682084247, -22.22500000000000142, 4.500000000000000888 ) ) ;
#113238 = CARTESIAN_POINT ( 'NONE',  ( 43.53752705046289151, -9.735942053221456900E-16, 7.949999999999998401 ) ) ;
#113239 = DIRECTION ( 'NONE',  ( 0.7071067811865487940, 0.7071067811865463515, 0.000000000000000000 ) ) ;
#113240 = DIRECTION ( 'NONE',  ( -0.7071067811865486830, 0.7071067811865464625, 0.000000000000000000 ) ) ;
#113241 = VERTEX_POINT ( 'NONE', #137758 ) ;
#113242 = ORIENTED_EDGE ( 'NONE', *, *, #136286, .F. ) ;
#113243 = CARTESIAN_POINT ( 'NONE',  ( 37.74999999999999289, -9.735942053221458872E-16, 7.950000000000000178 ) ) ;
#113244 = EDGE_CURVE ( 'NONE', #17447, #86210, #81969, .T. ) ;
#113245 = ORIENTED_EDGE ( 'NONE', *, *, #124168, .F. ) ;
#113246 = DIRECTION ( 'NONE',  ( -0.7071067811865486830, -0.7071067811865464625, -0.000000000000000000 ) ) ;
#113247 = ORIENTED_EDGE ( 'NONE', *, *, #31216, .F. ) ;
#113248 = EDGE_CURVE ( 'NONE', #133165, #60739, #82654, .T. ) ;
#113249 = CARTESIAN_POINT ( 'NONE',  ( 0.000000000000000000, 0.000000000000000000, 5.000000000000000000 ) ) ;
#113250 = DIRECTION ( 'NONE',  ( 0.7071067811865486830, -0.7071067811865464625, -0.000000000000000000 ) ) ;
#113251 = CARTESIAN_POINT ( 'NONE',  ( 34.70876352523143282, -7.482591942790329030E-16, 6.110000000000001208 ) ) ;
#113252 = ORIENTED_EDGE ( 'NONE', *, *, #49728, .T. ) ;
#113253 = LINE ( 'NONE', #58235, #117312 ) ;
#113254 = ORIENTED_EDGE ( 'NONE', *, *, #79391, .T. ) ;
#113255 = ADVANCED_FACE ( 'NONE', ( #113840 ), #92795, .F. ) ;
#113256 = CARTESIAN_POINT ( 'NONE',  ( 31.49999999999979039, 5.696342897626542445, -7.587980461218329253 ) ) ;
#113257 = VECTOR ( 'NONE', #62361, 1000.000000000000000 ) ;
#113258 = VECTOR ( 'NONE', #37263, 1000.000000000000000 ) ;
#113259 = STYLED_ITEM ( 'NONE', ( #59122 ), #62770 ) ;
#113260 = CARTESIAN_POINT ( 'NONE',  ( 1.171830600776462061, 3.759292476615678336, 4.000000000000000000 ) ) ;
#113261 = CARTESIAN_POINT ( 'NONE',  ( -60.18398860626900415, 28.73617430169829490, 5.000000000000000000 ) ) ;
#113262 = VECTOR ( 'NONE', #66454, 1000.000000000000227 ) ;
#113263 = CARTESIAN_POINT ( 'NONE',  ( 9.119999999999999218, 1.116877880822386018E-15, 10.00000000000000000 ) ) ;
#113264 = EDGE_LOOP ( 'NONE', ( #107599, #67343, #114566, #72347 ) ) ;
#113265 = CARTESIAN_POINT ( 'NONE',  ( 21.18398860626899349, 28.73617430169802134, 5.000000000000000000 ) ) ;
#113266 = ORIENTED_EDGE ( 'NONE', *, *, #12563, .T. ) ;
#113267 = CARTESIAN_POINT ( 'NONE',  ( -51.18398860626899705, 28.73617430169823095, 5.000000000000000000 ) ) ;
#113268 = DIRECTION ( 'NONE',  ( -1.000000000000000000, 0.000000000000000000, 0.000000000000000000 ) ) ;
#113269 = CARTESIAN_POINT ( 'NONE',  ( -42.18398860626899705, 28.73617430169816700, 5.000000000000000000 ) ) ;
#113270 = ADVANCED_FACE ( 'NONE', ( #37735 ), #27528, .F. ) ;
#113271 = EDGE_CURVE ( 'NONE', #36826, #134985, #115224, .T. ) ;
#113272 = LINE ( 'NONE', #24847, #37097 ) ;
#113273 = CARTESIAN_POINT ( 'NONE',  ( 12.00548008471251293, 28.92564299267929684, 4.000000000000000000 ) ) ;
#113274 = AXIS2_PLACEMENT_3D ( 'NONE', #73300, #40666, #16755 ) ;
#113275 = EDGE_CURVE ( 'NONE', #16581, #50105, #58081, .T. ) ;
#113276 = CARTESIAN_POINT ( 'NONE',  ( 8.926082202452091607, -22.22500000000000142, -11.61681428604210353 ) ) ;
#113277 = CARTESIAN_POINT ( 'NONE',  ( 58.09959685856477307, -6.109999999999997655, -1.637169565754160283 ) ) ;
#113278 = DIRECTION ( 'NONE',  ( 0.000000000000000000, -1.000000000000000000, 0.000000000000000000 ) ) ;
#113279 = CARTESIAN_POINT ( 'NONE',  ( 19.49999999999987921, 22.08746187583901843, 4.000000000000000000 ) ) ;
#113280 = EDGE_LOOP ( 'NONE', ( #67624, #99363, #76164, #105633 ) ) ;
#113281 = ORIENTED_EDGE ( 'NONE', *, *, #56461, .F. ) ;
#113282 = AXIS2_PLACEMENT_3D ( 'NONE', #43001, #87909, #32849 ) ;
#113283 = DIRECTION ( 'NONE',  ( -0.000000000000000000, 0.3543493200069153248, 0.9351131265310292928 ) ) ;
#113284 = ORIENTED_EDGE ( 'NONE', *, *, #84478, .T. ) ;
#113285 = AXIS2_PLACEMENT_3D ( 'NONE', #59777, #103943, #4590 ) ;
#113286 = FACE_OUTER_BOUND ( 'NONE', #142573, .T. ) ;
#113287 = ORIENTED_EDGE ( 'NONE', *, *, #68604, .T. ) ;
#113288 = CARTESIAN_POINT ( 'NONE',  ( -1.180000000000000604, 10.00000000000000178, 6.750000000000000888 ) ) ;
#113289 = VECTOR ( 'NONE', #107398, 1000.000000000000000 ) ;
#113290 = VECTOR ( 'NONE', #20680, 999.9999999999998863 ) ;
#113291 = VECTOR ( 'NONE', #74004, 1000.000000000000000 ) ;
#113292 = FACE_BOUND ( 'NONE', #124979, .T. ) ;
#113293 = CARTESIAN_POINT ( 'NONE',  ( -13.49999999999990052, -6.839392718269134974, -8.480912228396052299 ) ) ;
#113294 = DIRECTION ( 'NONE',  ( -0.7071067811865486830, 0.7071067811865464625, 0.000000000000000000 ) ) ;
#113295 = DIRECTION ( 'NONE',  ( 1.000000000000000000, 1.224606353822377258E-16, 0.000000000000000000 ) ) ;
#113297 = ORIENTED_EDGE ( 'NONE', *, *, #108613, .F. ) ;
#113296 = CARTESIAN_POINT ( 'NONE',  ( 2.816011393730999401, 28.73617430169785436, 5.000000000000000000 ) ) ;
#113298 = VECTOR ( 'NONE', #39638, 1000.000000000000114 ) ;
#113299 = ORIENTED_EDGE ( 'NONE', *, *, #62263, .T. ) ;
#113300 = AXIS2_PLACEMENT_3D ( 'NONE', #138872, #93204, #16327 ) ;
#113301 = LINE ( 'NONE', #3114, #63429 ) ;
#113302 = ORIENTED_EDGE ( 'NONE', *, *, #134853, .F. ) ;
#113303 = ORIENTED_EDGE ( 'NONE', *, *, #99454, .T. ) ;
#113304 = CARTESIAN_POINT ( 'NONE',  ( 68.89126352523143737, -4.472830434245838482, -4.472830434245838482 ) ) ;
#113305 = EDGE_LOOP ( 'NONE', ( #114448, #68976, #83749, #63076 ) ) ;
#113306 = PLANE ( 'NONE',  #64996 ) ;
#113307 = ADVANCED_FACE ( 'NONE', ( #81242 ), #71788, .F. ) ;
#113308 = EDGE_LOOP ( 'NONE', ( #39470, #95060, #15661, #75876, #64954 ) ) ;
#113309 = CARTESIAN_POINT ( 'NONE',  ( 22.17183060077632817, 21.75929247661549937, 4.000000000000000000 ) ) ;
#113310 = TOROIDAL_SURFACE ( 'NONE', #78672, 31.92999999999999972, 3.000000000000000000 ) ;
#113311 = CARTESIAN_POINT ( 'NONE',  ( 122.0416666666666714, -3.975000000000002753, 6.884901960086286188 ) ) ;
#113312 = PLANE ( 'NONE',  #47893 ) ;
#113313 =( NAMED_UNIT ( * ) PLANE_ANGLE_UNIT ( ) SI_UNIT ( $, .RADIAN. ) );
#113315 = CARTESIAN_POINT ( 'NONE',  ( -17.20666063542140378, 21.75929247661549937, 4.998822639870711626 ) ) ;
#113314 = CARTESIAN_POINT ( 'NONE',  ( 27.18398860626900060, 28.73617430169806042, 5.000000000000000000 ) ) ;
#113316 = LINE ( 'NONE', #24195, #93278 ) ;
#113317 = CARTESIAN_POINT ( 'NONE',  ( -10.49999999999992184, 21.05218569542895679, 5.000000000000000000 ) ) ;
#113318 = ORIENTED_EDGE ( 'NONE', *, *, #67785, .F. ) ;
#113319 = VERTEX_POINT ( 'NONE', #102281 ) ;
#113320 = DIRECTION ( 'NONE',  ( -0.000000000000000000, -0.000000000000000000, -1.000000000000000000 ) ) ;
#113321 = CARTESIAN_POINT ( 'NONE',  ( 20.29298673570680123, -21.74070752338406720, 4.999753212805221558 ) ) ;
#113322 = ORIENTED_EDGE ( 'NONE', *, *, #4790, .F. ) ;
#113323 = ORIENTED_EDGE ( 'NONE', *, *, #45365, .F. ) ;
#113324 = ORIENTED_EDGE ( 'NONE', *, *, #142804, .T. ) ;
#113325 = CARTESIAN_POINT ( 'NONE',  ( 11.67183060077638856, -9.740707523384186217, 4.000000000000000000 ) ) ;
#113326 = EDGE_CURVE ( 'NONE', #91987, #48040, #115959, .T. ) ;
#113327 = EDGE_CURVE ( 'NONE', #111735, #140719, #92075, .T. ) ;
#113328 = DIRECTION ( 'NONE',  ( 0.7071067811865487940, 0.7071067811865463515, 0.000000000000000000 ) ) ;
#113329 = ORIENTED_EDGE ( 'NONE', *, *, #30291, .T. ) ;
#113330 = FACE_OUTER_BOUND ( 'NONE', #5558, .T. ) ;
#113331 = CARTESIAN_POINT ( 'NONE',  ( 42.37086038379622721, 6.884901960086289741, -3.974999999999993427 ) ) ;
#113332 = CARTESIAN_POINT ( 'NONE',  ( -0.07876352523144723727, -9.717572351234235426E-16, -7.934999999999990727 ) ) ;
#113333 = CARTESIAN_POINT ( 'NONE',  ( 15.33107836643582900, 3.532353787238777798, -29.90988538521246909 ) ) ;
#113334 = ORIENTED_EDGE ( 'NONE', *, *, #40373, .T. ) ;
#113335 = ADVANCED_FACE ( 'NONE', ( #135608 ), #80524, .T. ) ;
#113336 = LINE ( 'NONE', #35838, #64275 ) ;
#113337 = CARTESIAN_POINT ( 'NONE',  ( -23.99999999999983302, -6.108550654416979420, -3.114665004255023462 ) ) ;
#113338 = DIRECTION ( 'NONE',  ( -0.7071067811865486830, 0.7071067811865464625, 0.000000000000000000 ) ) ;
#113340 = ORIENTED_EDGE ( 'NONE', *, *, #138240, .T. ) ;
#113339 = DIRECTION ( 'NONE',  ( 1.000000000000000000, 1.224606353822377258E-16, 0.000000000000000000 ) ) ;
#113341 = ORIENTED_EDGE ( 'NONE', *, *, #87182, .T. ) ;
#113342 = CARTESIAN_POINT ( 'NONE',  ( -26.99999999999980815, -0.4125381241607481431, 4.000000000000000000 ) ) ;
#113343 = LINE ( 'NONE', #14028, #40029 ) ;
#113344 = DIRECTION ( 'NONE',  ( -0.7071067811865486830, -0.7071067811865464625, 0.000000000000000000 ) ) ;
#113345 = EDGE_CURVE ( 'NONE', #107684, #118381, #36985, .T. ) ;
#113346 = ORIENTED_EDGE ( 'NONE', *, *, #5662, .F. ) ;
#113347 = SURFACE_STYLE_USAGE ( .BOTH. , #23497 ) ;
#113348 = DIRECTION ( 'NONE',  ( 0.000000000000000000, 0.000000000000000000, 1.000000000000000000 ) ) ;
#113349 = FILL_AREA_STYLE_COLOUR ( '', #129702 ) ;
#113350 = CARTESIAN_POINT ( 'NONE',  ( 20.29289321881332242, -12.74070752338415247, 5.000000000000000000 ) ) ;
#113351 = AXIS2_PLACEMENT_3D ( 'NONE', #37541, #39688, #83172 ) ;
#113352 = ORIENTED_EDGE ( 'NONE', *, *, #24055, .T. ) ;
#113354 = ADVANCED_FACE ( 'NONE', ( #26131 ), #70394, .F. ) ;
#113353 = AXIS2_PLACEMENT_3D ( 'NONE', #41308, #30454, #53639 ) ;
#113355 = VECTOR ( 'NONE', #11723, 1000.000000000000227 ) ;
#113356 = AXIS2_PLACEMENT_3D ( 'NONE', #64429, #139164, #20185 ) ;
#113357 = CARTESIAN_POINT ( 'NONE',  ( -32.99451991528749062, 28.92564299267960948, 4.000000000000000000 ) ) ;
#113358 = CARTESIAN_POINT ( 'NONE',  ( -23.99451991528749062, 28.92564299267954908, 4.000000000000000000 ) ) ;
#113359 = PLANE ( 'NONE',  #42388 ) ;
#113360 = AXIS2_PLACEMENT_3D ( 'NONE', #31500, #130105, #56145 ) ;
#113361 = CARTESIAN_POINT ( 'NONE',  ( -12.18398860626900060, 28.73617430169795739, 5.000000000000000000 ) ) ;
#113362 = CARTESIAN_POINT ( 'NONE',  ( -34.92500000000001137, -21.72500000000000142, 5.000000000000000000 ) ) ;
#113363 = ORIENTED_EDGE ( 'NONE', *, *, #1169, .F. ) ;
#113364 = EDGE_LOOP ( 'NONE', ( #59184, #109772, #80657, #104197 ) ) ;
#113365 = ADVANCED_FACE ( 'NONE', ( #28983 ), #73216, .T. ) ;
#113366 = DIRECTION ( 'NONE',  ( 0.000000000000000000, -1.000000000000000000, -5.559056632600921604E-15 ) ) ;
#113367 = LINE ( 'NONE', #24243, #93337 ) ;
#113368 = CARTESIAN_POINT ( 'NONE',  ( -34.75611968250421313, -3.187065745292602781, 4.955485411084894487 ) ) ;
#113369 = AXIS2_PLACEMENT_3D ( 'NONE', #27070, #73454, #6703 ) ;
#113370 = CARTESIAN_POINT ( 'NONE',  ( 4.499999999999968914, -4.796895815301017052, -3.611700055028670864 ) ) ;
#113371 = LINE ( 'NONE', #70644, #25095 ) ;
#113372 = PLANE ( 'NONE',  #74564 ) ;
#113373 = ORIENTED_EDGE ( 'NONE', *, *, #126342, .T. ) ;
#113374 = EDGE_CURVE ( 'NONE', #99040, #98806, #52153, .T. ) ;
#113375 = CARTESIAN_POINT ( 'NONE',  ( 26.51078643762690845, -27.52281430457036748, 5.000000000000000000 ) ) ;
#113376 = VECTOR ( 'NONE', #53122, 1000.000000000000000 ) ;
#113377 = AXIS2_PLACEMENT_3D ( 'NONE', #118287, #117558, #10242 ) ;
#113378 = FACE_OUTER_BOUND ( 'NONE', #83468, .T. ) ;
#113379 = CARTESIAN_POINT ( 'NONE',  ( 59.70376352523145158, 6.109999999999999432, 1.122388791418549108E-15 ) ) ;
#113380 = CARTESIAN_POINT ( 'NONE',  ( 183.4786297241425927, -52.14999999999998437, -41.05044666116291552 ) ) ;
#113381 = EDGE_CURVE ( 'NONE', #119254, #93631, #9313, .T. ) ;
#113382 = EDGE_CURVE ( 'NONE', #2974, #104604, #118085, .T. ) ;
#113383 = VECTOR ( 'NONE', #51234, 1000.000000000000000 ) ;
#113384 = LINE ( 'NONE', #93792, #11657 ) ;
#113385 = ORIENTED_EDGE ( 'NONE', *, *, #59533, .T. ) ;
#113386 = FACE_OUTER_BOUND ( 'NONE', #87656, .T. ) ;
#113387 = ORIENTED_EDGE ( 'NONE', *, *, #13323, .F. ) ;
#113388 = LINE ( 'NONE', #24262, #75591 ) ;
#113389 = VECTOR ( 'NONE', #85988, 1000.000000000000000 ) ;
#113390 = ADVANCED_FACE ( 'NONE', ( #127579 ), #141296, .F. ) ;
#113391 = VECTOR ( 'NONE', #117305, 1000.000000000000000 ) ;
#113392 = CARTESIAN_POINT ( 'NONE',  ( 7.139999999999992575, -35.14999999999999858, -40.00000000000000000 ) ) ;
#113393 = DIRECTION ( 'NONE',  ( -0.7071067811865486830, 0.7071067811865464625, 0.000000000000000000 ) ) ;
#113394 = PLANE ( 'NONE',  #25361 ) ;
#113395 = EDGE_CURVE ( 'NONE', #87783, #135817, #138461, .T. ) ;
#113396 = CARTESIAN_POINT ( 'NONE',  ( 17.21837311707493612, 21.74787736706806029, 4.999607392498049308 ) ) ;
#113397 = PLANE ( 'NONE',  #40752 ) ;
#113398 = VECTOR ( 'NONE', #66111, 1000.000000000000000 ) ;
#113399 = ORIENTED_EDGE ( 'NONE', *, *, #106068, .T. ) ;
#113400 = CIRCLE ( 'NONE', #118028, 0.5000000000000004441 ) ;
#113401 = EDGE_CURVE ( 'NONE', #33386, #63294, #4331, .T. ) ;
#113402 = VERTEX_POINT ( 'NONE', #31138 ) ;
#113403 = DIRECTION ( 'NONE',  ( 0.7071067811865486830, -0.7071067811865464625, -0.000000000000000000 ) ) ;
#113404 = CARTESIAN_POINT ( 'NONE',  ( 4.658131166821905644, 3.821174125832445049E-16, 0.000000000000000000 ) ) ;
#113405 = CIRCLE ( 'NONE', #131959, 5.999999999999998224 ) ;
#113406 = CARTESIAN_POINT ( 'NONE',  ( -1.499999999999984013, 12.43112307739206024, 4.000000000000000000 ) ) ;
#113407 = PLANE ( 'NONE',  #136029 ) ;
#113408 = CARTESIAN_POINT ( 'NONE',  ( 77.51669371712954160, 7.950000000000001066, -2.130196079827421318 ) ) ;
#113409 = CARTESIAN_POINT ( 'NONE',  ( 4.499999999999968914, -5.947814304570774091, 5.000000000000000000 ) ) ;
#113410 = LINE ( 'NONE', #2488, #4262 ) ;
#113411 = ORIENTED_EDGE ( 'NONE', *, *, #33473, .T. ) ;
#113412 = CARTESIAN_POINT ( 'NONE',  ( 76.39583333333332860, -2.130196079827427091, 7.949999999999999289 ) ) ;
#113413 = ADVANCED_FACE ( 'NONE', ( #106496 ), #128993, .T. ) ;
#113414 = DIRECTION ( 'NONE',  ( -0.000000000000000000, 0.000000000000000000, 1.000000000000000000 ) ) ;
#113415 = CARTESIAN_POINT ( 'NONE',  ( 35.99451991528749772, 28.92564299267963079, 4.000000000000000000 ) ) ;
#113416 = CARTESIAN_POINT ( 'NONE',  ( -0.4892135623730947680, -27.52281430457055578, 5.000000000000000000 ) ) ;
#113417 = VECTOR ( 'NONE', #102393, 1000.000000000000000 ) ;
#113418 = EDGE_LOOP ( 'NONE', ( #26960, #32036, #7038, #48383 ) ) ;
#113419 = EDGE_CURVE ( 'NONE', #22931, #129409, #75353, .T. ) ;
#113420 = DIRECTION ( 'NONE',  ( -0.6830127018922180770, -0.6830127018922204085, -0.2588190451025213501 ) ) ;
#113421 = CARTESIAN_POINT ( 'NONE',  ( -31.49999999999977263, 22.08746187583901843, 4.000000000000000000 ) ) ;
#113422 = CARTESIAN_POINT ( 'NONE',  ( 70.58376352523143282, -6.110000000000001208, -3.741295971395164515E-16 ) ) ;
#113423 = CARTESIAN_POINT ( 'NONE',  ( 6.707106781186501721, 8.259292476615629042, 5.000000000000000000 ) ) ;
#113424 = ORIENTED_EDGE ( 'NONE', *, *, #39229, .F. ) ;
#113425 = VERTEX_POINT ( 'NONE', #74645 ) ;
#113426 = VECTOR ( 'NONE', #25615, 1000.000000000000227 ) ;
#113427 = DIRECTION ( 'NONE',  ( -0.000000000000000000, -0.3543493200069152693, 0.9351131265310292928 ) ) ;
#113428 =( NAMED_UNIT ( * ) SI_UNIT ( $, .STERADIAN. ) SOLID_ANGLE_UNIT ( ) );
#113429 = DIRECTION ( 'NONE',  ( 0.6830127018922180770, -0.6830127018922204085, -0.2588190451025213501 ) ) ;
#113430 = DIRECTION ( 'NONE',  ( 0.7071067811865487940, 0.7071067811865463515, 0.000000000000000000 ) ) ;
#113431 = ORIENTED_EDGE ( 'NONE', *, *, #137442, .F. ) ;
#113432 = DIRECTION ( 'NONE',  ( 0.7071067811865487940, -0.7071067811865463515, 0.000000000000000000 ) ) ;
#113433 = FACE_OUTER_BOUND ( 'NONE', #115196, .T. ) ;
#113434 = DIRECTION ( 'NONE',  ( 0.7071067811865486830, -0.7071067811865464625, -0.000000000000000000 ) ) ;
#113435 = COLOUR_RGB ( '', 0.09019608, 0.27058824, 0.51372549) ;
#113436 = LINE ( 'NONE', #68550, #122464 ) ;
#113437 = CLOSED_SHELL ( 'NONE', ( #66228, #46689, #82437, #64958, #81930, #112081, #16114, #63034, #115316, #11702, #130635, #70028, #22614, #122273, #100016, #21254, #116793, #36322, #62770, #118359, #91558, #79080, #97639, #102640, #79637, #120916, #116870, #32375, #98966, #71398, #33147, #118172, #7398, #13691, #104071, #12196, #5117, #108314, #99140, #975, #4147, #43643, #23446, #86018, #65144, #61305, #47657, #139780, #20929, #134888, #23037, #33681, #137549, #80703, #15304, #34948, #111895, #47140, #90366, #73585, #41038, #70138, #81831, #31273, #124337, #96794, #83137, #44864, #89171, #117596, #939, #95871, #90943, #22381, #40939, #93057, #111891, #62206, #82181, #18383, #27925, #75511, #44362, #79516, #88505, #141443, #16334, #124980, #38134, #82293, #95688, #68458, #37829, #88424, #116311, #128132, #109467, #51969, #124881, #87420, #137587, #87823, #21720, #13350, #33428, #2933, #28818, #64289, #131194, #65185, #98714, #41693, #248, #27794, #8773, #120064, #57143, #6157, #41826, #34639, #113213, #65678, #33707, #113202, #111305, #49850, #41202, #116432, #77853, #25975, #12766, #63723, #90553, #39731, #131026, #96714, #120045, #62638, #69272 ) ) ;
#113438 = ORIENTED_EDGE ( 'NONE', *, *, #106727, .T. ) ;
#113439 = EDGE_CURVE ( 'NONE', #54392, #2047, #61635, .T. ) ;
#113440 = VERTEX_POINT ( 'NONE', #73911 ) ;
#113441 = CARTESIAN_POINT ( 'NONE',  ( 59.50043019189810423, -3.055000000000002380, 5.291415217122920289 ) ) ;
#113442 = EDGE_CURVE ( 'NONE', #118295, #16746, #128306, .T. ) ;
#113443 = ORIENTED_EDGE ( 'NONE', *, *, #45032, .F. ) ;
#113444 = CARTESIAN_POINT ( 'NONE',  ( 0.9950752277880503538, -5.240707523384228850, 12.38332538355495949 ) ) ;
#113445 = CARTESIAN_POINT ( 'NONE',  ( 3.000000000000000000, -43.14999999999999147, -31.92499999999998295 ) ) ;
#113446 = CARTESIAN_POINT ( 'NONE',  ( 111.3500270504628986, -5.819803920172573086, -5.819803920172573086 ) ) ;
#113447 = CARTESIAN_POINT ( 'NONE',  ( 54.52083333333332149, 7.949999999999998401, 2.130196079827431532 ) ) ;
#113448 = ORIENTED_EDGE ( 'NONE', *, *, #26944, .F. ) ;
#113449 = ORIENTED_EDGE ( 'NONE', *, *, #37689, .F. ) ;
#113450 = DIRECTION ( 'NONE',  ( 0.7071067811865487940, -0.7071067811865463515, 0.000000000000000000 ) ) ;
#113451 = CARTESIAN_POINT ( 'NONE',  ( -16.55061209249478082, 0.6983656428564303242, -33.57195050579999673 ) ) ;
#113453 = ORIENTED_EDGE ( 'NONE', *, *, #101338, .F. ) ;
#113452 = CIRCLE ( 'NONE', #46348, 2.055000000000001048 ) ;
#113454 = DIRECTION ( 'NONE',  ( -0.7071067811865487940, 0.7071067811865463515, -0.000000000000000000 ) ) ;
#113455 = ORIENTED_EDGE ( 'NONE', *, *, #67194, .F. ) ;
#113456 = CARTESIAN_POINT ( 'NONE',  ( 15.00548008471250228, 28.92564299267927552, 4.000000000000000000 ) ) ;
#113457 = PLANE ( 'NONE',  #139652 ) ;
#113458 = VECTOR ( 'NONE', #104972, 1000.000000000000000 ) ;
#113459 = AXIS2_PLACEMENT_3D ( 'NONE', #125527, #46583, #80600 ) ;
#113460 = MECHANICAL_DESIGN_GEOMETRIC_PRESENTATION_REPRESENTATION (  '', ( #53231 ), #48592 ) ;
#113461 = EDGE_LOOP ( 'NONE', ( #141481, #114436, #140920 ) ) ;
#113462 = TOROIDAL_SURFACE ( 'NONE', #32461, 14.46000000000000085, 3.000000000000000000 ) ;
#113463 = FACE_BOUND ( 'NONE', #70381, .T. ) ;
#113464 = DIRECTION ( 'NONE',  ( -1.000000000000000000, -1.224606353822377258E-16, -0.000000000000000000 ) ) ;
#113465 = CARTESIAN_POINT ( 'NONE',  ( 54.48921356237310221, -27.52281430457093236, 5.000000000000000000 ) ) ;
#113466 = LINE ( 'NONE', #58448, #113057 ) ;
#113467 = VECTOR ( 'NONE', #14975, 1000.000000000000000 ) ;
#113468 = DIRECTION ( 'NONE',  ( -0.7071067811865486830, -0.7071067811865464625, 0.000000000000000000 ) ) ;
#113469 = DIRECTION ( 'NONE',  ( 0.000000000000000000, 0.000000000000000000, 1.000000000000000000 ) ) ;
#113470 = CARTESIAN_POINT ( 'NONE',  ( -85.49107322549018306, -54.12360598635387987, 64.23745354946214547 ) ) ;
#113471 = ORIENTED_EDGE ( 'NONE', *, *, #98639, .F. ) ;
#113472 = ORIENTED_EDGE ( 'NONE', *, *, #126864, .T. ) ;
#113473 = CARTESIAN_POINT ( 'NONE',  ( 105.3495968585647944, 6.109999999999996767, 1.637169565754163836 ) ) ;
#113474 = ORIENTED_EDGE ( 'NONE', *, *, #124037, .T. ) ;
#113475 = CARTESIAN_POINT ( 'NONE',  ( 19.10416666666666785, -1.633150327867672447, -6.094999999999999751 ) ) ;
#113476 = VERTEX_POINT ( 'NONE', #139194 ) ;
#113477 = VECTOR ( 'NONE', #37673, 1000.000000000000000 ) ;
#113478 = DIRECTION ( 'NONE',  ( -0.7071067811865487940, 0.7071067811865463515, 0.000000000000000000 ) ) ;
#113479 = LINE ( 'NONE', #124377, #101050 ) ;
#113480 = DIRECTION ( 'NONE',  ( -0.6830127018922180770, -0.6830127018922204085, -0.2588190451025213501 ) ) ;
#113481 = ORIENTED_EDGE ( 'NONE', *, *, #59376, .T. ) ;
#113482 = DIRECTION ( 'NONE',  ( 0.7071067811865487940, 0.7071067811865463515, -0.000000000000000000 ) ) ;
#113483 = DIRECTION ( 'NONE',  ( -0.7071067811865487940, 0.7071067811865463515, 0.000000000000000000 ) ) ;
#113484 = LINE ( 'NONE', #91743, #13373 ) ;
#113485 = CARTESIAN_POINT ( 'NONE',  ( 35.99451991528749772, 28.92564299267963079, 4.000000000000000000 ) ) ;
#113486 = VECTOR ( 'NONE', #23553, 1000.000000000000000 ) ;
#113487 = PLANE ( 'NONE',  #41544 ) ;
#113488 = DIRECTION ( 'NONE',  ( 1.000000000000000000, 0.000000000000000000, 0.000000000000000000 ) ) ;
#113489 = ORIENTED_EDGE ( 'NONE', *, *, #64635, .T. ) ;
#113490 = VECTOR ( 'NONE', #60884, 1000.000000000000227 ) ;
#113491 = DIRECTION ( 'NONE',  ( -0.7071067811865486830, -0.7071067811865464625, -0.000000000000000000 ) ) ;
#113492 = CARTESIAN_POINT ( 'NONE',  ( -34.92500000000001137, -12.53194198458142061, -8.170704600677588303 ) ) ;
#113493 = EDGE_CURVE ( 'NONE', #129328, #34178, #63067, .T. ) ;
#113494 = VERTEX_POINT ( 'NONE', #119517 ) ;
#113495 = EDGE_LOOP ( 'NONE', ( #18265, #22509, #70156, #27666 ) ) ;
#113496 = EDGE_CURVE ( 'NONE', #129679, #105081, #20212, .T. ) ;
#113497 = EDGE_CURVE ( 'NONE', #22057, #92143, #51458, .T. ) ;
#113498 = CIRCLE ( 'NONE', #97336, 2.500000000000000888 ) ;
#113499 = ORIENTED_EDGE ( 'NONE', *, *, #64009, .T. ) ;
#113500 = CARTESIAN_POINT ( 'NONE',  ( 52.50043019189811133, -3.055000000000002380, 5.291415217122920289 ) ) ;
#113501 = ORIENTED_EDGE ( 'NONE', *, *, #68484, .T. ) ;
#113502 = ADVANCED_FACE ( 'NONE', ( #18796 ), #107241, .F. ) ;
#113503 = EDGE_CURVE ( 'NONE', #81462, #134437, #132606, .T. ) ;
#113504 = CIRCLE ( 'NONE', #51033, 2.055000000000001048 ) ;
#113505 = CARTESIAN_POINT ( 'NONE',  ( 2.233306282870438864, -6.094999999999989981, -1.633150327867689100 ) ) ;
#113506 = CARTESIAN_POINT ( 'NONE',  ( 87.93793019189809002, -6.110000000000001208, 1.637169565754158951 ) ) ;
#113507 = FACE_OUTER_BOUND ( 'NONE', #33792, .T. ) ;
#113508 = VERTEX_POINT ( 'NONE', #63767 ) ;
#113509 = EDGE_CURVE ( 'NONE', #751, #67859, #65204, .T. ) ;
#113510 = CARTESIAN_POINT ( 'NONE',  ( 11.87852683662845799, -20.24070752338407431, 7.412974875817763376 ) ) ;
#113511 = ORIENTED_EDGE ( 'NONE', *, *, #20578, .T. ) ;
#113512 = VECTOR ( 'NONE', #113954, 1000.000000000000000 ) ;
#113513 = DIRECTION ( 'NONE',  ( 3.115803279706882722E-16, -1.000000000000000000, 0.000000000000000000 ) ) ;
#113514 = ORIENTED_EDGE ( 'NONE', *, *, #92157, .F. ) ;
#113515 = CYLINDRICAL_SURFACE ( 'NONE', #53773, 6.094999999999989093 ) ;
#113516 = CARTESIAN_POINT ( 'NONE',  ( -8.671830600776399223, -21.74070752338405299, 4.000000000000000000 ) ) ;
#113517 = DIRECTION ( 'NONE',  ( -0.000000000000000000, 0.3543493200069153248, 0.9351131265310292928 ) ) ;
#113518 = EDGE_CURVE ( 'NONE', #98020, #136003, #87716, .T. ) ;
#113519 = ORIENTED_EDGE ( 'NONE', *, *, #81995, .F. ) ;
#113520 = CARTESIAN_POINT ( 'NONE',  ( -56.99451991528749062, 28.92564299267978001, 4.000000000000000000 ) ) ;
#113521 = ORIENTED_EDGE ( 'NONE', *, *, #99401, .T. ) ;
#113522 = ORIENTED_EDGE ( 'NONE', *, *, #10741, .F. ) ;
#113523 = VERTEX_POINT ( 'NONE', #134008 ) ;
#113524 = LINE ( 'NONE', #36680, #72609 ) ;
#113525 = CONICAL_SURFACE ( 'NONE', #34913, 2.500000000000000888, 0.9599310885968822538 ) ;
#113526 = LINE ( 'NONE', #27231, #118665 ) ;
#113527 = DIRECTION ( 'NONE',  ( -0.3543493200069163240, -0.000000000000000000, 0.9351131265310288487 ) ) ;
#113528 = DIRECTION ( 'NONE',  ( 0.6830127018922181881, 0.6830127018922202975, -0.2588190451025214056 ) ) ;
#113529 = PLANE ( 'NONE',  #32637 ) ;
#113530 = EDGE_LOOP ( 'NONE', ( #111642, #61289, #141404, #128556 ) ) ;
#113531 = EDGE_CURVE ( 'NONE', #119333, #24024, #34701, .T. ) ;
#113532 = CIRCLE ( 'NONE', #136718, 5.968999999999998529 ) ;
#113533 = CARTESIAN_POINT ( 'NONE',  ( 14.59122188827396549, 7.143407583703162089, 5.000000000000000000 ) ) ;
#113534 = CARTESIAN_POINT ( 'NONE',  ( 22.43706980810188867, 2.126176841940952134, -7.934999999999993392 ) ) ;
#113535 = DIRECTION ( 'NONE',  ( -0.000000000000000000, 0.000000000000000000, 1.000000000000000000 ) ) ;
#113536 = CARTESIAN_POINT ( 'NONE',  ( 1.499999999999990896, 9.431123077392093990, 4.000000000000000000 ) ) ;
#113537 = CARTESIAN_POINT ( 'NONE',  ( -23.99451991528749062, 28.92564299267954908, 4.000000000000000000 ) ) ;
#113538 = VERTEX_POINT ( 'NONE', #112261 ) ;
#113539 = ORIENTED_EDGE ( 'NONE', *, *, #106436, .F. ) ;
#113541 = ORIENTED_EDGE ( 'NONE', *, *, #127231, .F. ) ;
#113540 = ADVANCED_FACE ( 'NONE', ( #42736 ), #87639, .T. ) ;
#113542 = LINE ( 'NONE', #136021, #115748 ) ;
#113543 = CARTESIAN_POINT ( 'NONE',  ( -42.48921356237308800, -27.52281430457085065, 5.000000000000000000 ) ) ;
#113544 = CARTESIAN_POINT ( 'NONE',  ( -32.99451991528749062, 28.92564299267960948, 4.000000000000000000 ) ) ;
#113545 = VECTOR ( 'NONE', #104474, 999.9999999999998863 ) ;
#113546 = CARTESIAN_POINT ( 'NONE',  ( -9.792893218813386369, 15.75929247661555976, 5.000000000000000000 ) ) ;
#113547 = CARTESIAN_POINT ( 'NONE',  ( 10.32500000000000107, 8.432637487761466488, 4.375000000000001776 ) ) ;
#113549 = EDGE_CURVE ( 'NONE', #132281, #63434, #10067, .T. ) ;
#113548 = VECTOR ( 'NONE', #116535, 999.9999999999998863 ) ;
#113550 = AXIS2_PLACEMENT_3D ( 'NONE', #116315, #6793, #95270 ) ;
#113551 = CARTESIAN_POINT ( 'NONE',  ( 29.99999999999979394, -0.4125381241607516403, 4.000000000000000000 ) ) ;
#113552 = DIRECTION ( 'NONE',  ( 0.7071067811865486830, -0.7071067811865464625, -0.000000000000000000 ) ) ;
#113553 = DIRECTION ( 'NONE',  ( 0.7071067811865487940, 0.7071067811865463515, 0.000000000000000000 ) ) ;
#113554 = CARTESIAN_POINT ( 'NONE',  ( 16.75173015016484968, 4.202752102959690472E-16, 0.000000000000000000 ) ) ;
#113555 = ADVANCED_FACE ( 'NONE', ( #55030 ), #65924, .T. ) ;
#113556 = FACE_OUTER_BOUND ( 'NONE', #36642, .T. ) ;
#113557 = ORIENTED_EDGE ( 'NONE', *, *, #139235, .T. ) ;
#113558 = AXIS2_PLACEMENT_3D ( 'NONE', #32074, #76304, #108880 ) ;
#113559 = AXIS2_PLACEMENT_3D ( 'NONE', #39042, #29578, #49941 ) ;
#113561 = CARTESIAN_POINT ( 'NONE',  ( 16.67979525387081807, 0.3337821591035643465, -30.81818940114110461 ) ) ;
#113560 = VECTOR ( 'NONE', #107131, 1000.000000000000000 ) ;
#113562 = ORIENTED_EDGE ( 'NONE', *, *, #43585, .F. ) ;
#113563 = EDGE_CURVE ( 'NONE', #64622, #82404, #115505, .T. ) ;
#113564 = AXIS2_PLACEMENT_3D ( 'NONE', #63469, #96043, #51861 ) ;
#113565 = DIRECTION ( 'NONE',  ( -0.7071067811865486830, -0.7071067811865464625, 0.000000000000000000 ) ) ;
#113567 = VERTEX_POINT ( 'NONE', #11471 ) ;
#113566 = PLANE ( 'NONE',  #14001 ) ;
#113568 = FACE_OUTER_BOUND ( 'NONE', #11934, .T. ) ;
#113569 = CARTESIAN_POINT ( 'NONE',  ( 10.17183060077640100, -11.24070752338417201, 4.000000000000000000 ) ) ;
#113570 = VERTEX_POINT ( 'NONE', #100671 ) ;
#113571 = LINE ( 'NONE', #40846, #9027 ) ;
#113572 = VERTEX_POINT ( 'NONE', #76800 ) ;
#113573 = AXIS2_PLACEMENT_3D ( 'NONE', #130388, #75298, #63711 ) ;
#113574 = ORIENTED_EDGE ( 'NONE', *, *, #119837, .F. ) ;
#113575 = DIRECTION ( 'NONE',  ( -0.7071067811865487940, 0.7071067811865463515, -0.000000000000000000 ) ) ;
#113576 = CARTESIAN_POINT ( 'NONE',  ( 99.68336038379624142, -2.130196079827426203, 7.949999999999997513 ) ) ;
#113577 = DIRECTION ( 'NONE',  ( 0.000000000000000000, -1.000000000000000000, 0.000000000000000000 ) ) ;
#113578 = DIRECTION ( 'NONE',  ( -0.6830127018922180770, -0.6830127018922204085, -0.2588190451025213501 ) ) ;
#113579 = ORIENTED_EDGE ( 'NONE', *, *, #17910, .T. ) ;
#113580 = ADVANCED_FACE ( 'NONE', ( #10761 ), #86936, .F. ) ;
#113581 = DIRECTION ( 'NONE',  ( -0.3543493200069162685, -0.000000000000000000, -0.9351131265310288487 ) ) ;
#113582 = DIRECTION ( 'NONE',  ( 0.7071067811865487940, 0.7071067811865463515, 0.000000000000000000 ) ) ;
#113583 = DIRECTION ( 'NONE',  ( 0.7071067811865487940, -0.7071067811865463515, 0.000000000000000000 ) ) ;
#113584 = CARTESIAN_POINT ( 'NONE',  ( 24.64583333333333570, -1.633150327867689988, 6.094999999999989981 ) ) ;
#113586 = VECTOR ( 'NONE', #123032, 1000.000000000000000 ) ;
#113585 = DIRECTION ( 'NONE',  ( -0.3543493200069162685, -0.000000000000000000, -0.9351131265310288487 ) ) ;
#113587 = PLANE ( 'NONE',  #48954 ) ;
#113588 = FACE_OUTER_BOUND ( 'NONE', #12740, .T. ) ;
#113589 = ORIENTED_EDGE ( 'NONE', *, *, #128913, .T. ) ;
#113590 = AXIS2_PLACEMENT_3D ( 'NONE', #124153, #24838, #132927 ) ;
#113591 = CARTESIAN_POINT ( 'NONE',  ( 23.99999999999983302, -21.03360074219752462, 5.000000000000000000 ) ) ;
#113592 = ORIENTED_EDGE ( 'NONE', *, *, #139333, .F. ) ;
#113593 = ADVANCED_FACE ( 'NONE', ( #31832 ), #109389, .T. ) ;
#113594 = CARTESIAN_POINT ( 'NONE',  ( 98.58376352523144703, -6.110000000000001208, -3.741295971395164515E-16 ) ) ;
#113595 = AXIS2_PLACEMENT_3D ( 'NONE', #69785, #58929, #13190 ) ;
#113596 = DIRECTION ( 'NONE',  ( 0.7071067811865487940, -0.7071067811865463515, 0.000000000000000000 ) ) ;
#113597 = CARTESIAN_POINT ( 'NONE',  ( 39.48921356237310221, -27.52281430457082934, 5.000000000000000000 ) ) ;
#113598 = CARTESIAN_POINT ( 'NONE',  ( 0.7586007421979610310, 21.72500000000000853, 5.000000000000000000 ) ) ;
#113599 = DIRECTION ( 'NONE',  ( 1.000000000000000000, 0.000000000000000000, 0.000000000000000000 ) ) ;
#113600 = ORIENTED_EDGE ( 'NONE', *, *, #115263, .T. ) ;
#113601 = VECTOR ( 'NONE', #1041, 1000.000000000000227 ) ;
#113602 = LINE ( 'NONE', #47690, #23383 ) ;
#113603 = CARTESIAN_POINT ( 'NONE',  ( -23.99451991528749062, 28.92564299267954908, 4.000000000000000000 ) ) ;
#113604 = EDGE_CURVE ( 'NONE', #14564, #101438, #12207, .T. ) ;
#113605 = ORIENTED_EDGE ( 'NONE', *, *, #417, .T. ) ;
#113606 = CARTESIAN_POINT ( 'NONE',  ( -29.99999999999978328, -10.44781430457071991, 5.000000000000000000 ) ) ;
#113607 = VECTOR ( 'NONE', #24252, 999.9999999999998863 ) ;
#113608 = DIRECTION ( 'NONE',  ( 0.7071067811865486830, -0.7071067811865464625, -0.000000000000000000 ) ) ;
#113609 = B_SPLINE_CURVE_WITH_KNOTS ( 'NONE', 3,
 ( #112469, #136351, #91439, #1524 ),
 .UNSPECIFIED., .F., .F.,
 ( 4, 4 ),
 ( 0.003615568590623256025, 0.004164643302645746128 ),
 .UNSPECIFIED. ) ;
#113611 = EDGE_LOOP ( 'NONE', ( #41472, #95468, #12753, #69062 ) ) ;
#113610 = DIRECTION ( 'NONE',  ( 0.7071067811865487940, 0.7071067811865463515, 0.000000000000000000 ) ) ;
#113612 = CARTESIAN_POINT ( 'NONE',  ( -12.69999999999998153, 0.000000000000000000, 0.000000000000000000 ) ) ;
#113613 = DIRECTION ( 'NONE',  ( 0.000000000000000000, 0.000000000000000000, 1.000000000000000000 ) ) ;
#113614 = CYLINDRICAL_SURFACE ( 'NONE', #121092, 7.950000000000000178 ) ;
#113615 = DIRECTION ( 'NONE',  ( -0.7071067811865486830, -0.7071067811865464625, 0.000000000000000000 ) ) ;
#113616 = ORIENTED_EDGE ( 'NONE', *, *, #46140, .F. ) ;
#113617 = ORIENTED_EDGE ( 'NONE', *, *, #59372, .T. ) ;
#113618 = ORIENTED_EDGE ( 'NONE', *, *, #93006, .T. ) ;
#113619 = CARTESIAN_POINT ( 'NONE',  ( 86.47959685856477563, 6.109999999999999432, 1.637169565754164280 ) ) ;
#113620 = AXIS2_PLACEMENT_3D ( 'NONE', #52590, #62784, #43168 ) ;
#113621 = EDGE_LOOP ( 'NONE', ( #81798, #40088, #126349, #126667 ) ) ;
#113622 = DIRECTION ( 'NONE',  ( 1.000000000000000000, 1.224606353822377258E-16, 0.000000000000000000 ) ) ;
#113623 = DIRECTION ( 'NONE',  ( 0.000000000000000000, 0.000000000000000000, 1.000000000000000000 ) ) ;
#113624 =( GEOMETRIC_REPRESENTATION_CONTEXT ( 3 ) GLOBAL_UNCERTAINTY_ASSIGNED_CONTEXT ( ( #37647 ) ) GLOBAL_UNIT_ASSIGNED_CONTEXT ( ( #108752, #11584, #131989 ) ) REPRESENTATION_CONTEXT ( 'NONE', 'WORKASPACE' ) );
#113625 = LINE ( 'NONE', #75488, #27186 ) ;
#113626 = LINE ( 'NONE', #14317, #17939 ) ;
#113627 = ORIENTED_EDGE ( 'NONE', *, *, #33420, .F. ) ;
#113628 = DIRECTION ( 'NONE',  ( -0.000000000000000000, 0.000000000000000000, 1.000000000000000000 ) ) ;
#113630 = EDGE_CURVE ( 'NONE', #46380, #50635, #121673, .T. ) ;
#113629 = DIRECTION ( 'NONE',  ( -0.7071067811865486830, -0.7071067811865464625, 0.000000000000000000 ) ) ;
#113631 = DIRECTION ( 'NONE',  ( 0.7071067811865487940, 0.7071067811865463515, -0.000000000000000000 ) ) ;
#113632 = CARTESIAN_POINT ( 'NONE',  ( 75.01626352523142316, -4.472830434245839371, 4.472830434245839371 ) ) ;
#113633 = EDGE_CURVE ( 'NONE', #44164, #92497, #131869, .T. ) ;
#113634 = VERTEX_POINT ( 'NONE', #120224 ) ;
#113635 = CARTESIAN_POINT ( 'NONE',  ( 15.71462683630238111, 8.126010640810376273, 4.668119888204643075 ) ) ;
#113636 = DIRECTION ( 'NONE',  ( 0.7071067811865487940, 0.7071067811865463515, -0.000000000000000000 ) ) ;
#113637 = DIRECTION ( 'NONE',  ( 0.000000000000000000, -1.000000000000000000, 0.000000000000000000 ) ) ;
#113638 = MECHANICAL_DESIGN_GEOMETRIC_PRESENTATION_REPRESENTATION (  '', ( #95107 ), #139118 ) ;
#113639 = ORIENTED_EDGE ( 'NONE', *, *, #22089, .F. ) ;
#113640 = ORIENTED_EDGE ( 'NONE', *, *, #77160, .T. ) ;
#113641 = CARTESIAN_POINT ( 'NONE',  ( 3.872664058232598183, 3.061616997868383634E-16, -2.500000000000000444 ) ) ;
#113642 = ADVANCED_FACE ( 'NONE', ( #20938 ), #120970, .F. ) ;
#113643 = CARTESIAN_POINT ( 'NONE',  ( 11.20710678118647152, 9.759292476615614831, 5.000000000000000000 ) ) ;
#113644 = CARTESIAN_POINT ( 'NONE',  ( 20.65000000000000213, 9.500000000000000000, 0.000000000000000000 ) ) ;
#113645 = CIRCLE ( 'NONE', #16342, 2.500000000000000888 ) ;
#113646 = CARTESIAN_POINT ( 'NONE',  ( 30.29974487139158867, -27.71228299555227537, 4.000000000000000000 ) ) ;
#113647 = CARTESIAN_POINT ( 'NONE',  ( -10.49999999999992539, -20.56887692260760758, 4.000000000000000000 ) ) ;
#113648 = CARTESIAN_POINT ( 'NONE',  ( 63.48921356237309510, -27.52281430457099631, 5.000000000000000000 ) ) ;
#113649 = SURFACE_STYLE_USAGE ( .BOTH. , #123133 ) ;
#113650 = ORIENTED_EDGE ( 'NONE', *, *, #70559, .F. ) ;
#113651 =( BOUNDED_CURVE ( )  B_SPLINE_CURVE ( 3, ( #129909, #19005, #50936, #139398 ),
 .UNSPECIFIED., .F., .T. ) 
 B_SPLINE_CURVE_WITH_KNOTS ( ( 4, 4 ),
 ( 1.570796326794896558, 3.141592653589793116 ),
 .UNSPECIFIED. ) 
 CURVE ( )  GEOMETRIC_REPRESENTATION_ITEM ( )  RATIONAL_B_SPLINE_CURVE ( ( 1.000000000000000000, 0.8047378541243649375, 0.8047378541243649375, 1.000000000000000000 ) ) 
 REPRESENTATION_ITEM ( '' )  );
#113652 = ORIENTED_EDGE ( 'NONE', *, *, #143348, .T. ) ;
#113653 = CARTESIAN_POINT ( 'NONE',  ( 39.29974487139159578, -27.71228299555233576, 4.000000000000000000 ) ) ;
#113654 = ORIENTED_EDGE ( 'NONE', *, *, #15795, .F. ) ;
#113655 = EDGE_LOOP ( 'NONE', ( #67186, #69620, #24698, #139795 ) ) ;
#113656 = AXIS2_PLACEMENT_3D ( 'NONE', #126891, #72595, #4350 ) ;
#113657 = CIRCLE ( 'NONE', #51181, 2.500000000000000444 ) ;
#113658 = VECTOR ( 'NONE', #71965, 1000.000000000000000 ) ;
#113659 = CARTESIAN_POINT ( 'NONE',  ( 0.000000000000000000, 0.000000000000000000, 5.000000000000000000 ) ) ;
#113660 = ORIENTED_EDGE ( 'NONE', *, *, #30153, .T. ) ;
#113661 = FACE_OUTER_BOUND ( 'NONE', #142487, .T. ) ;
#113662 = LINE ( 'NONE', #102093, #93490 ) ;
#113663 = DIRECTION ( 'NONE',  ( -0.3543493200069162685, -0.000000000000000000, -0.9351131265310288487 ) ) ;
#113664 = LINE ( 'NONE', #25226, #129503 ) ;
#113665 = VECTOR ( 'NONE', #63994, 999.9999999999998863 ) ;
#113666 = VECTOR ( 'NONE', #107523, 1000.000000000000227 ) ;
#113667 = VECTOR ( 'NONE', #104466, 1000.000000000000000 ) ;
#113668 = CARTESIAN_POINT ( 'NONE',  ( 60.18398860626900415, 28.73617430169829490, 5.000000000000000000 ) ) ;
#113669 = ORIENTED_EDGE ( 'NONE', *, *, #128368, .T. ) ;
#113670 = VECTOR ( 'NONE', #62560, 999.9999999999998863 ) ;
#113671 = CARTESIAN_POINT ( 'NONE',  ( -23.70025512860841133, -27.71228299555189523, 4.000000000000000000 ) ) ;
#113672 = CARTESIAN_POINT ( 'NONE',  ( 20.99999999999985434, -4.447814304570781196, 5.000000000000000000 ) ) ;
#113673 = EDGE_LOOP ( 'NONE', ( #71544, #114886, #39545, #58142 ) ) ;
#113674 = LINE ( 'NONE', #121678, #45751 ) ;
#113675 = EDGE_LOOP ( 'NONE', ( #33199, #102360, #86089, #24801 ) ) ;
#113677 = ORIENTED_EDGE ( 'NONE', *, *, #27864, .F. ) ;
#113676 = EDGE_CURVE ( 'NONE', #23262, #105676, #110786, .T. ) ;
#113678 = DIRECTION ( 'NONE',  ( -0.7071067811865486830, -0.7071067811865464625, 0.000000000000000000 ) ) ;
#113679 = ORIENTED_EDGE ( 'NONE', *, *, #16404, .F. ) ;
#113680 = ORIENTED_EDGE ( 'NONE', *, *, #135005, .F. ) ;
#113681 = VECTOR ( 'NONE', #76563, 1000.000000000000000 ) ;
#113682 = DIRECTION ( 'NONE',  ( -1.000000000000000000, -1.224606353822377258E-16, -0.000000000000000000 ) ) ;
#113683 = ORIENTED_EDGE ( 'NONE', *, *, #99940, .T. ) ;
#113684 = ADVANCED_FACE ( 'NONE', ( #78208 ), #122390, .T. ) ;
#113685 = ADVANCED_FACE ( 'NONE', ( #125994 ), #112953, .F. ) ;
#113686 = DIRECTION ( 'NONE',  ( 0.7071067811865486830, -0.7071067811865464625, -0.000000000000000000 ) ) ;
#113688 = ADVANCED_FACE ( 'NONE', ( #126672 ), #68773, .F. ) ;
#113687 = PLANE ( 'NONE',  #142201 ) ;
#113689 = CARTESIAN_POINT ( 'NONE',  ( 115.3545968585647614, -1.637169565754161615, 6.110000000000000320 ) ) ;
#113690 = DIRECTION ( 'NONE',  ( -0.7071067811865486830, 0.7071067811865464625, 0.000000000000000000 ) ) ;
#113691 = VECTOR ( 'NONE', #68589, 1000.000000000000000 ) ;
#113692 = EDGE_CURVE ( 'NONE', #13774, #124390, #127937, .T. ) ;
#113693 = LINE ( 'NONE', #12936, #117640 ) ;
#113694 = DIRECTION ( 'NONE',  ( 0.6830127018922181881, 0.6830127018922202975, -0.2588190451025214056 ) ) ;
#113695 = VECTOR ( 'NONE', #117476, 1000.000000000000000 ) ;
#113696 = LINE ( 'NONE', #14388, #11615 ) ;
#113697 = EDGE_CURVE ( 'NONE', #20428, #114476, #81795, .T. ) ;
#113698 = DIRECTION ( 'NONE',  ( 0.000000000000000000, 0.000000000000000000, 1.000000000000000000 ) ) ;
#113699 = STYLED_ITEM ( 'NONE', ( #36467 ), #98629 ) ;
#113700 = CYLINDRICAL_SURFACE ( 'NONE', #68331, 4.000000000000000000 ) ;
#113701 = ADVANCED_FACE ( 'NONE', ( #3457 ), #36819, .T. ) ;
#113702 = ORIENTED_EDGE ( 'NONE', *, *, #87479, .F. ) ;
#113703 = AXIS2_PLACEMENT_3D ( 'NONE', #108236, #53935, #98130 ) ;
#113704 = LINE ( 'NONE', #134043, #36496 ) ;
#113705 = PLANE ( 'NONE',  #124067 ) ;
#113706 = EDGE_LOOP ( 'NONE', ( #104559, #86688, #119092 ) ) ;
#113707 = VECTOR ( 'NONE', #50579, 1000.000000000000227 ) ;
#113708 = EDGE_LOOP ( 'NONE', ( #60064, #41321, #29806, #98292 ) ) ;
#113709 = CARTESIAN_POINT ( 'NONE',  ( 27.32816939922334143, -21.74070752338406365, 4.000000000000000000 ) ) ;
#113710 = EDGE_LOOP ( 'NONE', ( #81255, #22478, #55413, #58391 ) ) ;
#113711 = CIRCLE ( 'NONE', #106762, 2.500000000000000444 ) ;
#113712 = PLANE ( 'NONE',  #69984 ) ;
#113713 = DIRECTION ( 'NONE',  ( 1.000000000000000000, 0.000000000000000000, 0.000000000000000000 ) ) ;
#113714 = EDGE_CURVE ( 'NONE', #82607, #33848, #47746, .T. ) ;
#113715 = VECTOR ( 'NONE', #52931, 1000.000000000000114 ) ;
#113716 = CARTESIAN_POINT ( 'NONE',  ( 6.499999999999999112, 7.960204194457794491E-16, 10.00000000000000000 ) ) ;
#113717 = DIRECTION ( 'NONE',  ( 0.7071067811865487940, 0.7071067811865463515, 0.000000000000000000 ) ) ;
#113718 = ORIENTED_EDGE ( 'NONE', *, *, #13265, .T. ) ;
#113719 = CARTESIAN_POINT ( 'NONE',  ( 9.748407645496676821, -2.499999999999998224, 0.000000000000000000 ) ) ;
#113720 = ORIENTED_EDGE ( 'NONE', *, *, #14577, .F. ) ;
#113721 = ADVANCED_FACE ( 'NONE', ( #114384 ), #115061, .F. ) ;
#113722 = CARTESIAN_POINT ( 'NONE',  ( -24.79289321881328334, 0.7592924766157104211, 5.000000000000000000 ) ) ;
#113723 = VECTOR ( 'NONE', #130978, 1000.000000000000000 ) ;
#113724 = CARTESIAN_POINT ( 'NONE',  ( 30.54623647476855552, -7.934999999999990727, 4.858786175617117713E-16 ) ) ;
#113725 = VERTEX_POINT ( 'NONE', #2006 ) ;
#113726 = CARTESIAN_POINT ( 'NONE',  ( -31.49999999999976552, 16.08746187583907528, 4.000000000000000000 ) ) ;
#113727 = DIRECTION ( 'NONE',  ( -0.7071067811865487940, 0.7071067811865463515, 0.000000000000000000 ) ) ;
#113728 = ORIENTED_EDGE ( 'NONE', *, *, #3860, .T. ) ;
#113729 = VERTEX_POINT ( 'NONE', #124553 ) ;
#113730 = VECTOR ( 'NONE', #57130, 999.9999999999998863 ) ;
#113731 = EDGE_LOOP ( 'NONE', ( #116992, #58552, #99749, #81482 ) ) ;
#113732 = LINE ( 'NONE', #12971, #38012 ) ;
#113733 = LINE ( 'NONE', #17270, #88134 ) ;
#113734 = DIRECTION ( 'NONE',  ( -0.3543493200069162685, -0.000000000000000000, -0.9351131265310288487 ) ) ;
#113735 = VECTOR ( 'NONE', #120124, 1000.000000000000000 ) ;
#113736 = CARTESIAN_POINT ( 'NONE',  ( -13.49999999999990763, 16.18958161055401490, -11.56426086740814441 ) ) ;
#113737 = ORIENTED_EDGE ( 'NONE', *, *, #33671, .F. ) ;
#113738 = LINE ( 'NONE', #71670, #78628 ) ;
#113739 = CARTESIAN_POINT ( 'NONE',  ( -23.99999999999982947, 20.70535890316559247, 1.956823837851970449 ) ) ;
#113740 = DIRECTION ( 'NONE',  ( 0.7071067811865487940, 0.7071067811865463515, 0.000000000000000000 ) ) ;
#113741 = CARTESIAN_POINT ( 'NONE',  ( 39.18398860626899705, 28.73617430169814568, 5.000000000000000000 ) ) ;
#113742 = EDGE_CURVE ( 'NONE', #77649, #14760, #25956, .T. ) ;
#113743 = EDGE_LOOP ( 'NONE', ( #67862, #112109, #114561, #89428 ) ) ;
#113744 = VECTOR ( 'NONE', #55096, 1000.000000000000000 ) ;
#113745 = CARTESIAN_POINT ( 'NONE',  ( -28.82816939922332367, -11.24070752338416845, 4.000000000000000000 ) ) ;
#113746 = EDGE_LOOP ( 'NONE', ( #134740, #21304, #111682 ) ) ;
#113747 = EDGE_CURVE ( 'NONE', #99063, #49422, #46321, .T. ) ;
#113749 = VERTEX_POINT ( 'NONE', #48414 ) ;
#113748 = CARTESIAN_POINT ( 'NONE',  ( -31.49999999999977973, -16.91253812416059077, 4.000000000000000000 ) ) ;
#113750 = ORIENTED_EDGE ( 'NONE', *, *, #14513, .F. ) ;
#113751 = DIRECTION ( 'NONE',  ( -0.3543493200069162685, -0.000000000000000000, -0.9351131265310288487 ) ) ;
#113752 = FACE_OUTER_BOUND ( 'NONE', #50532, .T. ) ;
#113754 = VERTEX_POINT ( 'NONE', #136847 ) ;
#113753 = VECTOR ( 'NONE', #140017, 1000.000000000000227 ) ;
#113755 = PRESENTATION_STYLE_ASSIGNMENT (( #47137 ) ) ;
#113756 = VERTEX_POINT ( 'NONE', #37559 ) ;
#113757 = EDGE_CURVE ( 'NONE', #132084, #49722, #125266, .T. ) ;
#113758 = CARTESIAN_POINT ( 'NONE',  ( 34.17183060077623225, -20.24070752338407786, 4.000000000000000000 ) ) ;
#113759 = LINE ( 'NONE', #46409, #16117 ) ;
#113760 = CARTESIAN_POINT ( 'NONE',  ( -0.7071067811865398012, 2.259292476615692546, 5.000000000000000000 ) ) ;
#113761 = CARTESIAN_POINT ( 'NONE',  ( -1.499999999999987566, -6.839392718269127869, -8.480912228396080721 ) ) ;
#113762 = CARTESIAN_POINT ( 'NONE',  ( 34.92499999999998295, 5.816654386410395894, 4.500000000000000888 ) ) ;
#113763 = EDGE_CURVE ( 'NONE', #32610, #71084, #134751, .T. ) ;
#113764 = DIRECTION ( 'NONE',  ( 0.000000000000000000, -1.000000000000000000, 0.000000000000000000 ) ) ;
#113765 = DIRECTION ( 'NONE',  ( 0.7071067811865487940, 0.7071067811865463515, -0.000000000000000000 ) ) ;
#113766 = DIRECTION ( 'NONE',  ( 0.000000000000000000, -1.000000000000000000, 0.000000000000000000 ) ) ;
#113767 = CARTESIAN_POINT ( 'NONE',  ( 21.99956980810188867, -3.967499999999998028, -6.871911579029511330 ) ) ;
#113768 = CARTESIAN_POINT ( 'NONE',  ( 12.00548008471251293, 28.92564299267929684, 4.000000000000000000 ) ) ;
#113769 = CARTESIAN_POINT ( 'NONE',  ( -16.01987774928538499, -17.24070752338410273, 20.23474786156465655 ) ) ;
#113770 = VECTOR ( 'NONE', #109270, 1000.000000000000000 ) ;
#113771 = FACE_OUTER_BOUND ( 'NONE', #30421, .T. ) ;
#113772 = LINE ( 'NONE', #26059, #110276 ) ;
#113773 = EDGE_LOOP ( 'NONE', ( #75076, #45798, #15314, #76740 ) ) ;
#113774 = ORIENTED_EDGE ( 'NONE', *, *, #85383, .T. ) ;
#113775 = PRESENTATION_LAYER_ASSIGNMENT (  '', '', ( #116148 ) ) ;
#113776 = CARTESIAN_POINT ( 'NONE',  ( 95.64583333333334281, 2.130196079827431976, -7.949999999999999289 ) ) ;
#113777 = AXIS2_PLACEMENT_3D ( 'NONE', #24330, #13423, #57704 ) ;
#113778 = ORIENTED_EDGE ( 'NONE', *, *, #26492, .T. ) ;
#113779 = ORIENTED_EDGE ( 'NONE', *, *, #134000, .T. ) ;
#113780 = FACE_BOUND ( 'NONE', #76772, .T. ) ;
#113781 = CARTESIAN_POINT ( 'NONE',  ( -30.18398860626900060, 28.73617430169808173, 5.000000000000000000 ) ) ;
#113782 = VECTOR ( 'NONE', #6519, 1000.000000000000227 ) ;
#113783 = VECTOR ( 'NONE', #122474, 999.9999999999998863 ) ;
#113784 = COLOUR_RGB ( '', 0.66274510, 0.83137255, 0.94901961) ;
#113785 = CARTESIAN_POINT ( 'NONE',  ( 14.25124240572947265, 9.301334755096696938, 1.951233148376585236 ) ) ;
#113786 = ORIENTED_EDGE ( 'NONE', *, *, #17750, .T. ) ;
#113787 = CARTESIAN_POINT ( 'NONE',  ( 2.816011393730999401, 28.73617430169785436, 5.000000000000000000 ) ) ;
#113788 = VECTOR ( 'NONE', #94278, 1000.000000000000227 ) ;
#113789 = CARTESIAN_POINT ( 'NONE',  ( -34.92500000000001137, 2.464645009310397761, -2.487937186831662206 ) ) ;
#113790 = CARTESIAN_POINT ( 'NONE',  ( -34.92500000000001137, 22.22500000000000142, 4.000000000000000000 ) ) ;
#113791 = CARTESIAN_POINT ( 'NONE',  ( 125.9517069660836484, 3.572642044305429643, -6.597326320955100520 ) ) ;
#113792 = EDGE_CURVE ( 'NONE', #24475, #109980, #122567, .T. ) ;
#113793 = EDGE_CURVE ( 'NONE', #45578, #23228, #123862, .T. ) ;
#113794 = PLANE ( 'NONE',  #142265 ) ;
#113795 = VECTOR ( 'NONE', #100266, 1000.000000000000114 ) ;
#113796 = DIRECTION ( 'NONE',  ( 0.000000000000000000, 0.000000000000000000, 1.000000000000000000 ) ) ;
#113797 = CARTESIAN_POINT ( 'NONE',  ( -39.48921356237310221, -27.52281430457082934, 5.000000000000000000 ) ) ;
#113798 = CARTESIAN_POINT ( 'NONE',  ( 26.99451991528749417, 28.92564299267956685, 4.000000000000000000 ) ) ;
#113799 = DIRECTION ( 'NONE',  ( -0.000000000000000000, -0.3543493200069152693, 0.9351131265310292928 ) ) ;
#113800 = DIRECTION ( 'NONE',  ( 0.6830127018922181881, 0.6830127018922202975, -0.2588190451025214056 ) ) ;
#113801 = EDGE_CURVE ( 'NONE', #28238, #56422, #113664, .T. ) ;
#113802 = ORIENTED_EDGE ( 'NONE', *, *, #18720, .T. ) ;
#113803 = EDGE_LOOP ( 'NONE', ( #29364, #57002, #42138, #90974 ) ) ;
#113804 = CARTESIAN_POINT ( 'NONE',  ( 106.6045968585647472, 1.637169565754164946, -6.109999999999999432 ) ) ;
#113805 = VERTEX_POINT ( 'NONE', #38264 ) ;
#113806 = VECTOR ( 'NONE', #36481, 1000.000000000000000 ) ;
#113807 = DIRECTION ( 'NONE',  ( 0.6830127018922181881, 0.6830127018922202975, -0.2588190451025214056 ) ) ;
#113808 = CARTESIAN_POINT ( 'NONE',  ( 174.7500000000000000, 7.919999999999947526, -21.52769999999994965 ) ) ;
#113809 = CARTESIAN_POINT ( 'NONE',  ( 8.277185695429338352, -21.72500000000000142, 5.000000000000000000 ) ) ;
#113810 = DIRECTION ( 'NONE',  ( 0.000000000000000000, -1.000000000000000000, 0.000000000000000000 ) ) ;
#113811 = VECTOR ( 'NONE', #60200, 1000.000000000000227 ) ;
#113812 = VECTOR ( 'NONE', #20740, 1000.000000000000000 ) ;
#113813 = CARTESIAN_POINT ( 'NONE',  ( 104.1829301918981088, -1.637169565754158951, -6.109999999999998543 ) ) ;
#113814 = EDGE_CURVE ( 'NONE', #109323, #96749, #14363, .T. ) ;
#113815 = VERTEX_POINT ( 'NONE', #136134 ) ;
#113816 = VERTEX_POINT ( 'NONE', #81067 ) ;
#113817 = DIRECTION ( 'NONE',  ( -0.3543493200069163240, 4.681814790819596721E-17, -0.9351131265310288487 ) ) ;
#113818 = AXIS2_PLACEMENT_3D ( 'NONE', #72455, #63699, #107859 ) ;
#113819 = ORIENTED_EDGE ( 'NONE', *, *, #109895, .T. ) ;
#113820 = ORIENTED_EDGE ( 'NONE', *, *, #134517, .T. ) ;
#113821 = VERTEX_POINT ( 'NONE', #19359 ) ;
#113822 = CARTESIAN_POINT ( 'NONE',  ( -34.92500000000001137, 21.72500000000000142, 5.000000000000000000 ) ) ;
#113823 = EDGE_CURVE ( 'NONE', #10224, #68931, #106303, .T. ) ;
#113824 = VECTOR ( 'NONE', #116348, 1000.000000000000000 ) ;
#113825 = VERTEX_POINT ( 'NONE', #16471 ) ;
#113826 = VERTEX_POINT ( 'NONE', #8433 ) ;
#113827 = DIRECTION ( 'NONE',  ( -1.000000000000000000, -1.224606353822377258E-16, -0.000000000000000000 ) ) ;
#113828 = ORIENTED_EDGE ( 'NONE', *, *, #47489, .T. ) ;
#113829 = EDGE_LOOP ( 'NONE', ( #91431, #119183, #64255, #83662, #101949, #120327 ) ) ;
#113830 = VECTOR ( 'NONE', #741, 1000.000000000000000 ) ;
#113831 = VECTOR ( 'NONE', #98071, 1000.000000000000227 ) ;
#113832 = CARTESIAN_POINT ( 'NONE',  ( 26.29289321881327623, -0.7407075233842718154, 5.000000000000000000 ) ) ;
#113833 = CARTESIAN_POINT ( 'NONE',  ( 17.29289321881333663, 20.25929247661551713, 5.000000000000000000 ) ) ;
#113834 = CARTESIAN_POINT ( 'NONE',  ( -51.48921356237309510, -27.52281430457091460, 5.000000000000000000 ) ) ;
#113835 = ORIENTED_EDGE ( 'NONE', *, *, #71000, .T. ) ;
#113836 = CARTESIAN_POINT ( 'NONE',  ( 0.000000000000000000, 0.000000000000000000, 5.000000000000000000 ) ) ;
#113837 = AXIS2_PLACEMENT_3D ( 'NONE', #107794, #62186, #7025 ) ;
#113838 = EDGE_CURVE ( 'NONE', #94040, #28957, #51996, .T. ) ;
#113839 = DIRECTION ( 'NONE',  ( -0.7071067811865486830, -0.7071067811865464625, -0.000000000000000000 ) ) ;
#113840 = FACE_OUTER_BOUND ( 'NONE', #31077, .T. ) ;
#113841 =( NAMED_UNIT ( * ) SI_UNIT ( $, .STERADIAN. ) SOLID_ANGLE_UNIT ( ) );
#113842 = FACE_BOUND ( 'NONE', #44504, .T. ) ;
#113843 = ORIENTED_EDGE ( 'NONE', *, *, #108113, .T. ) ;
#113844 = CARTESIAN_POINT ( 'NONE',  ( 63.95419371712955581, 6.884901960086283523, 3.975000000000002753 ) ) ;
#113845 = DIRECTION ( 'NONE',  ( 0.000000000000000000, 0.000000000000000000, 1.000000000000000000 ) ) ;
#113846 = FACE_OUTER_BOUND ( 'NONE', #42995, .T. ) ;
#113847 = EDGE_LOOP ( 'NONE', ( #128454, #115237, #142208, #123095, #82216 ) ) ;
#113848 = CARTESIAN_POINT ( 'NONE',  ( -48.18398860626899705, 28.73617430169820608, 5.000000000000000000 ) ) ;
#113849 = ORIENTED_EDGE ( 'NONE', *, *, #50672, .F. ) ;
#113850 = VERTEX_POINT ( 'NONE', #63612 ) ;
#113851 = VECTOR ( 'NONE', #38736, 1000.000000000000000 ) ;
#113852 = ORIENTED_EDGE ( 'NONE', *, *, #56801, .F. ) ;
#113853 = EDGE_CURVE ( 'NONE', #25222, #53667, #95478, .T. ) ;
#113854 = CARTESIAN_POINT ( 'NONE',  ( 38.26626352523145158, 4.472830434245838482, -4.472830434245837594 ) ) ;
#113855 = ORIENTED_EDGE ( 'NONE', *, *, #134132, .F. ) ;
#113856 = DIRECTION ( 'NONE',  ( -0.7071067811865487940, 0.7071067811865463515, 0.000000000000000000 ) ) ;
#113857 = EDGE_CURVE ( 'NONE', #26091, #89877, #52688, .T. ) ;
#113858 = EDGE_CURVE ( 'NONE', #51446, #93029, #107772, .T. ) ;
#113859 = CYLINDRICAL_SURFACE ( 'NONE', #87803, 3.999999999999989786 ) ;
#113860 = CARTESIAN_POINT ( 'NONE',  ( -9.005480084712511157, 28.92564299267931816, 4.000000000000000000 ) ) ;
#113861 = EDGE_LOOP ( 'NONE', ( #8093, #124256, #88282, #138201 ) ) ;
#113862 = EDGE_CURVE ( 'NONE', #71344, #68553, #128825, .T. ) ;
#113863 = CARTESIAN_POINT ( 'NONE',  ( -14.99999999999989342, -21.03360074219752462, 5.000000000000000000 ) ) ;
#113864 = VECTOR ( 'NONE', #105841, 1000.000000000000000 ) ;
#113865 = EDGE_CURVE ( 'NONE', #64706, #67772, #13690, .T. ) ;
#113866 = FILL_AREA_STYLE ('',( #82000 ) ) ;
#113867 = PRESENTATION_LAYER_ASSIGNMENT (  '', '', ( #56070 ) ) ;
#113868 = AXIS2_PLACEMENT_3D ( 'NONE', #127025, #84287, #114023 ) ;
#113869 = DIRECTION ( 'NONE',  ( 0.7071067811865487940, 0.7071067811865463515, 0.000000000000000000 ) ) ;
#113870 = LINE ( 'NONE', #122595, #69118 ) ;
#113871 = FACE_OUTER_BOUND ( 'NONE', #41868, .T. ) ;
#113872 = ADVANCED_FACE ( 'NONE', ( #18612 ), #130284, .F. ) ;
#113873 = ORIENTED_EDGE ( 'NONE', *, *, #28768, .T. ) ;
#113874 = ORIENTED_EDGE ( 'NONE', *, *, #2546, .T. ) ;
#113875 = AXIS2_PLACEMENT_3D ( 'NONE', #28755, #138943, #96808 ) ;
#113876 = ORIENTED_EDGE ( 'NONE', *, *, #140839, .T. ) ;
#113877 = AXIS2_PLACEMENT_3D ( 'NONE', #57640, #22797, #21423 ) ;
#113878 = EDGE_LOOP ( 'NONE', ( #97679, #84915, #14130, #19823 ) ) ;
#113879 = VECTOR ( 'NONE', #115735, 1000.000000000000000 ) ;
#113880 = CARTESIAN_POINT ( 'NONE',  ( 25.39999999999999858, -30.18000000000009564, -12.70000000000045404 ) ) ;
#113881 = ORIENTED_EDGE ( 'NONE', *, *, #8101, .T. ) ;
#113882 = ORIENTED_EDGE ( 'NONE', *, *, #79559, .T. ) ;
#113883 = DIRECTION ( 'NONE',  ( 0.7071067811865487940, 0.7071067811865463515, 0.000000000000000000 ) ) ;
#113884 = ADVANCED_FACE ( 'NONE', ( #51289 ), #5599, .F. ) ;
#113885 = EDGE_CURVE ( 'NONE', #106778, #113634, #141120, .T. ) ;
#113886 = DIRECTION ( 'NONE',  ( 0.7071067811865487940, 0.7071067811865463515, -0.000000000000000000 ) ) ;
#113887 = ORIENTED_EDGE ( 'NONE', *, *, #24278, .F. ) ;
#113888 = DIRECTION ( 'NONE',  ( 0.7071067811865486830, -0.7071067811865464625, -0.000000000000000000 ) ) ;
#113889 = ORIENTED_EDGE ( 'NONE', *, *, #41838, .T. ) ;
#113890 = EDGE_CURVE ( 'NONE', #16704, #106916, #85305, .T. ) ;
#113891 = DIRECTION ( 'NONE',  ( -1.000000000000000000, -1.224606353822377258E-16, -0.000000000000000000 ) ) ;
#113892 = CARTESIAN_POINT ( 'NONE',  ( -0.1839886062690032631, 28.73617430169787568, 5.000000000000000000 ) ) ;
#113893 = CARTESIAN_POINT ( 'NONE',  ( 2.400403141435218934, -7.934999999999989839, 2.126176841940957907 ) ) ;
#113894 = EDGE_LOOP ( 'NONE', ( #16838, #59001, #54725, #68564 ) ) ;
#113896 = LINE ( 'NONE', #90743, #63855 ) ;
#113895 = CARTESIAN_POINT ( 'NONE',  ( 112.0579301918981372, 6.110000000000001208, -1.637169565754156286 ) ) ;
#113897 = CARTESIAN_POINT ( 'NONE',  ( 57.48921356237308800, -27.52281430457095368, 5.000000000000000000 ) ) ;
#113898 = CARTESIAN_POINT ( 'NONE',  ( -9.299744871391588674, -27.71228299555212971, 4.000000000000000000 ) ) ;
#113899 = VERTEX_POINT ( 'NONE', #75199 ) ;
#113900 = FILL_AREA_STYLE ('',( #69718 ) ) ;
#113901 = ORIENTED_EDGE ( 'NONE', *, *, #135782, .F. ) ;
#113902 = CARTESIAN_POINT ( 'NONE',  ( 4.499999999999962697, 22.08746187583903975, 4.000000000000000000 ) ) ;
#113903 = CARTESIAN_POINT ( 'NONE',  ( 21.18398860626899349, 28.73617430169802134, 5.000000000000000000 ) ) ;
#113904 = LINE ( 'NONE', #71139, #38194 ) ;
#113905 = CARTESIAN_POINT ( 'NONE',  ( 20.99999999999985079, -19.22509904557634641, 1.855685503482227494 ) ) ;
#113906 = CARTESIAN_POINT ( 'NONE',  ( 183.7880820442461811, -48.99280962439294029, -39.49606053969851160 ) ) ;
#113907 = ORIENTED_EDGE ( 'NONE', *, *, #87878, .F. ) ;
#113908 = VECTOR ( 'NONE', #21512, 999.9999999999998863 ) ;
#113909 = CARTESIAN_POINT ( 'NONE',  ( 74.99451991528749772, 28.92564299267990435, 4.000000000000000000 ) ) ;
#113910 = VECTOR ( 'NONE', #135935, 1000.000000000000227 ) ;
#113911 = VECTOR ( 'NONE', #25265, 999.9999999999998863 ) ;
#113912 = FACE_OUTER_BOUND ( 'NONE', #34895, .T. ) ;
#113913 = LINE ( 'NONE', #127657, #39884 ) ;
#113914 = EDGE_CURVE ( 'NONE', #56087, #25521, #41109, .T. ) ;
#113915 = ORIENTED_EDGE ( 'NONE', *, *, #133066, .F. ) ;
#113916 = LINE ( 'NONE', #127659, #2579 ) ;
#113917 = VECTOR ( 'NONE', #104863, 1000.000000000000000 ) ;
#113918 = CARTESIAN_POINT ( 'NONE',  ( -12.00548008471251293, 28.92564299267929684, 4.000000000000000000 ) ) ;
#113919 = ORIENTED_EDGE ( 'NONE', *, *, #53288, .F. ) ;
#113921 = VERTEX_POINT ( 'NONE', #49868 ) ;
#113920 = CARTESIAN_POINT ( 'NONE',  ( -14.84387692260748182, -22.22499999999999787, 4.000000000000000000 ) ) ;
#113922 = EDGE_LOOP ( 'NONE', ( #125223, #99278, #30426, #104849 ) ) ;
#113923 = CARTESIAN_POINT ( 'NONE',  ( -10.01929040585510933, 11.35911882391357430, -26.07695017617128741 ) ) ;
#113924 = CARTESIAN_POINT ( 'NONE',  ( 0.000000000000000000, 0.000000000000000000, 5.000000000000000000 ) ) ;
#113925 = ORIENTED_EDGE ( 'NONE', *, *, #78870, .F. ) ;
#113926 = EDGE_CURVE ( 'NONE', #88472, #861, #73733, .T. ) ;
#113927 = DIRECTION ( 'NONE',  ( -0.000000000000000000, 0.3543493200069153248, 0.9351131265310292928 ) ) ;
#113928 = ORIENTED_EDGE ( 'NONE', *, *, #121229, .T. ) ;
#113929 = CARTESIAN_POINT ( 'NONE',  ( 2.999999999999999112, -43.14999999999999147, -34.92499999999998295 ) ) ;
#113930 = LINE ( 'NONE', #135696, #104501 ) ;
#113931 = EDGE_CURVE ( 'NONE', #108305, #88917, #106328, .T. ) ;
#113932 = CARTESIAN_POINT ( 'NONE',  ( -25.39999999999996305, 0.000000000000000000, 2.500000000000000000 ) ) ;
#113933 = VECTOR ( 'NONE', #16621, 999.9999999999998863 ) ;
#113934 = LINE ( 'NONE', #71172, #123457 ) ;
#113935 = CARTESIAN_POINT ( 'NONE',  ( 31.49999999999978684, -11.94781430457070392, 5.000000000000000000 ) ) ;
#113936 = VECTOR ( 'NONE', #81895, 1000.000000000000000 ) ;
#113937 = CARTESIAN_POINT ( 'NONE',  ( 11.99451991528749417, 28.92564299267946382, 4.000000000000000000 ) ) ;
#113938 = DIRECTION ( 'NONE',  ( -0.000000000000000000, 1.000000000000000000, -0.000000000000000000 ) ) ;
#113939 = CARTESIAN_POINT ( 'NONE',  ( -12.70710678118645198, -18.74070752338409562, 5.000000000000000000 ) ) ;
#113940 = ORIENTED_EDGE ( 'NONE', *, *, #50342, .F. ) ;
#113941 = EDGE_LOOP ( 'NONE', ( #105235, #69857, #134199, #45126 ) ) ;
#113942 = ORIENTED_EDGE ( 'NONE', *, *, #63758, .T. ) ;
#113943 = CARTESIAN_POINT ( 'NONE',  ( 116.0625000000000000, -5.819803920172572198, -5.819803920172573086 ) ) ;
#113944 = ORIENTED_EDGE ( 'NONE', *, *, #139180, .T. ) ;
#113945 = EDGE_LOOP ( 'NONE', ( #6092, #107575, #80365, #9513 ) ) ;
#113946 = EDGE_CURVE ( 'NONE', #132528, #86782, #124869, .T. ) ;
#113947 = ORIENTED_EDGE ( 'NONE', *, *, #38885, .F. ) ;
#113948 = VECTOR ( 'NONE', #104996, 1000.000000000000000 ) ;
#113949 = CARTESIAN_POINT ( 'NONE',  ( 0.4515083163331480853, -7.650011319436560875, 0.5189475094714633974 ) ) ;
#113950 = CARTESIAN_POINT ( 'NONE',  ( 5.068407645496677105, 9.139736423841732040E-16, 0.000000000000000000 ) ) ;
#113951 = ORIENTED_EDGE ( 'NONE', *, *, #20200, .F. ) ;
#113952 =( BOUNDED_CURVE ( )  B_SPLINE_CURVE ( 3, ( #94673, #130919, #117839, #51923 ),
 .UNSPECIFIED., .F., .T. ) 
 B_SPLINE_CURVE_WITH_KNOTS ( ( 4, 4 ),
 ( 5.005968288816722733, 5.074607125596334534 ),
 .UNSPECIFIED. ) 
 CURVE ( )  GEOMETRIC_REPRESENTATION_ITEM ( )  RATIONAL_B_SPLINE_CURVE ( ( 1.000000000000000000, 0.9996074310407765395, 0.9996074310407765395, 1.000000000000000000 ) ) 
 REPRESENTATION_ITEM ( '' )  );
#113953 = LINE ( 'NONE', #48011, #48531 ) ;
#113954 = DIRECTION ( 'NONE',  ( 0.7071067811865487940, 0.7071067811865463515, -0.000000000000000000 ) ) ;
#113955 = LINE ( 'NONE', #126265, #111360 ) ;
#113956 = CARTESIAN_POINT ( 'NONE',  ( 109.6670968585647756, -3.055000000000000160, -5.291415217122921177 ) ) ;
#113957 = ADVANCED_FACE ( 'NONE', ( #129528 ), #61478, .T. ) ;
#113958 = VERTEX_POINT ( 'NONE', #30227 ) ;
#113959 = EDGE_CURVE ( 'NONE', #126961, #66021, #17216, .T. ) ;
#113960 = CARTESIAN_POINT ( 'NONE',  ( -41.99451991528749062, 28.92564299267967343, 4.000000000000000000 ) ) ;
#113961 = CARTESIAN_POINT ( 'NONE',  ( 11.99999999999991651, -0.8619312979531862373, -5.102805207349797811 ) ) ;
#113963 = VECTOR ( 'NONE', #130545, 1000.000000000000000 ) ;
#113962 = DIRECTION ( 'NONE',  ( 0.7071067811865487940, 0.7071067811865463515, 0.000000000000000000 ) ) ;
#113964 = CARTESIAN_POINT ( 'NONE',  ( 0.7643236001482540676, 7.174902596057846083, 1.559348790086458436 ) ) ;
#113965 = FILL_AREA_STYLE_COLOUR ( '', #56818 ) ;
#113966 = LINE ( 'NONE', #126273, #44678 ) ;
#113967 = CARTESIAN_POINT ( 'NONE',  ( -31.49999999999977973, -2.173586137069170032, -4.605770156576181940 ) ) ;
#113968 = CARTESIAN_POINT ( 'NONE',  ( 49.07919371712955581, 3.975000000000002753, -6.884901960086283523 ) ) ;
#113969 = CARTESIAN_POINT ( 'NONE',  ( 24.18398860626899705, 28.73617430169804265, 5.000000000000000000 ) ) ;
#113970 = DIRECTION ( 'NONE',  ( -0.3543493200069162685, -0.000000000000000000, -0.9351131265310288487 ) ) ;
#113971 = ORIENTED_EDGE ( 'NONE', *, *, #93603, .F. ) ;
#113972 = ORIENTED_EDGE ( 'NONE', *, *, #125868, .T. ) ;
#113973 = CARTESIAN_POINT ( 'NONE',  ( 34.54166666666666430, -3.975000000000002753, 6.884901960086286188 ) ) ;
#113974 = ORIENTED_EDGE ( 'NONE', *, *, #31125, .T. ) ;
#113975 = ORIENTED_EDGE ( 'NONE', *, *, #110429, .F. ) ;
#113976 = DIRECTION ( 'NONE',  ( -0.7071067811865487940, 0.7071067811865463515, 0.000000000000000000 ) ) ;
#113977 = CARTESIAN_POINT ( 'NONE',  ( -26.99999999999979750, 17.58746187583906462, 4.000000000000000000 ) ) ;
#113978 = EDGE_LOOP ( 'NONE', ( #88762, #79638, #72168, #137829 ) ) ;
#113979 = VECTOR ( 'NONE', #107973, 1000.000000000000000 ) ;
#113980 = AXIS2_PLACEMENT_3D ( 'NONE', #67308, #80341, #111508 ) ;
#113981 = PLANE ( 'NONE',  #131196 ) ;
#113982 = CARTESIAN_POINT ( 'NONE',  ( -20.99999999999985079, -18.41253812416056945, 4.000000000000000000 ) ) ;
#113983 = AXIS2_PLACEMENT_3D ( 'NONE', #15597, #138151, #91772 ) ;
#113984 = CARTESIAN_POINT ( 'NONE',  ( -14.29298673570684919, -21.74070752338405299, 4.999753212805220670 ) ) ;
#113985 = STYLED_ITEM ( 'NONE', ( #32570 ), #16334 ) ;
#113986 = CARTESIAN_POINT ( 'NONE',  ( 32.95876352523143282, 0.000000000000000000, -6.110000000000001208 ) ) ;
#113987 = EDGE_CURVE ( 'NONE', #5793, #56807, #99038, .T. ) ;
#113988 = EDGE_LOOP ( 'NONE', ( #69161, #102111, #36635, #123282, #139061, #117645 ) ) ;
#113989 = EDGE_CURVE ( 'NONE', #14910, #33281, #100504, .T. ) ;
#113990 = CARTESIAN_POINT ( 'NONE',  ( 1.500000000000000000, 1.163414459189985682E-15, -9.500000000000001776 ) ) ;
#113991 = ORIENTED_EDGE ( 'NONE', *, *, #106117, .T. ) ;
#113992 = VECTOR ( 'NONE', #56794, 1000.000000000000000 ) ;
#113993 = AXIS2_PLACEMENT_3D ( 'NONE', #27833, #105382, #25687 ) ;
#113994 = DIRECTION ( 'NONE',  ( -0.000000000000000000, 1.000000000000000000, -0.000000000000000000 ) ) ;
#113995 = CARTESIAN_POINT ( 'NONE',  ( -54.18398860626899705, 28.73617430169825226, 5.000000000000000000 ) ) ;
#113996 = DIRECTION ( 'NONE',  ( -1.000000000000000000, 0.000000000000000000, 0.000000000000000000 ) ) ;
#113997 = CARTESIAN_POINT ( 'NONE',  ( 62.83333333333332149, -6.884901960086287964, 3.974999999999998312 ) ) ;
#113999 = EDGE_CURVE ( 'NONE', #95318, #10073, #53412, .T. ) ;
#113998 = ORIENTED_EDGE ( 'NONE', *, *, #127772, .F. ) ;
#114000 = ORIENTED_EDGE ( 'NONE', *, *, #123500, .F. ) ;
#114001 = CARTESIAN_POINT ( 'NONE',  ( 39.16252705046288440, 7.949999999999998401, 1.460391307983218338E-15 ) ) ;
#114002 = EDGE_CURVE ( 'NONE', #7775, #121162, #54173, .T. ) ;
#114003 = DIRECTION ( 'NONE',  ( -0.7071067811865486830, 0.7071067811865464625, 0.000000000000000000 ) ) ;
#114004 = DIRECTION ( 'NONE',  ( -0.000000000000000000, -0.3543493200069152693, 0.9351131265310292928 ) ) ;
#114005 = CARTESIAN_POINT ( 'NONE',  ( 54.16209685856478018, -5.291415217122919401, 3.054999999999997939 ) ) ;
#114006 = DIRECTION ( 'NONE',  ( 0.7071067811865487940, 0.7071067811865463515, -0.000000000000000000 ) ) ;
#114007 = CARTESIAN_POINT ( 'NONE',  ( 0.1839886062690032631, 28.73617430169787568, 5.000000000000000000 ) ) ;
#114008 = EDGE_LOOP ( 'NONE', ( #82294, #119221, #61973, #114452 ) ) ;
#114009 = ORIENTED_EDGE ( 'NONE', *, *, #52372, .F. ) ;
#114010 = DIRECTION ( 'NONE',  ( 0.6830127018922181881, 0.6830127018922202975, -0.2588190451025214056 ) ) ;
#114011 = EDGE_LOOP ( 'NONE', ( #103502, #74488, #90374, #143418, #129097 ) ) ;
#114012 = EDGE_CURVE ( 'NONE', #94430, #60173, #22889, .T. ) ;
#114013 = VECTOR ( 'NONE', #43805, 1000.000000000000000 ) ;
#114014 = CARTESIAN_POINT ( 'NONE',  ( 32.59678851739267458, 22.26999999999999957, -14.57149272626654302 ) ) ;
#114015 = UNCERTAINTY_MEASURE_WITH_UNIT (LENGTH_MEASURE( 1.000000000000000082E-05 ), #4844, 'distance_accuracy_value', 'NONE');
#114016 = ORIENTED_EDGE ( 'NONE', *, *, #27290, .T. ) ;
#114017 = CIRCLE ( 'NONE', #88578, 3.000000000000002665 ) ;
#114018 = CARTESIAN_POINT ( 'NONE',  ( -34.42500000000001137, 0.000000000000000000, 4.500000000000000888 ) ) ;
#114019 = AXIS2_PLACEMENT_3D ( 'NONE', #89046, #44103, #123092 ) ;
#114020 = FACE_OUTER_BOUND ( 'NONE', #82460, .T. ) ;
#114021 = FACE_BOUND ( 'NONE', #84405, .T. ) ;
#114022 = CARTESIAN_POINT ( 'NONE',  ( -12.69999999999998153, 0.000000000000000000, 0.000000000000000000 ) ) ;
#114023 = DIRECTION ( 'NONE',  ( -0.7071067811865486830, 0.7071067811865464625, 0.000000000000000000 ) ) ;
#114024 = PLANE ( 'NONE',  #1634 ) ;
#114026 = ORIENTED_EDGE ( 'NONE', *, *, #55361, .F. ) ;
#114025 = DIRECTION ( 'NONE',  ( 0.000000000000000000, 0.000000000000000000, -1.000000000000000000 ) ) ;
#114027 = DIRECTION ( 'NONE',  ( -1.000000000000000000, -1.224606353822377258E-16, -0.000000000000000000 ) ) ;
#114028 = VERTEX_POINT ( 'NONE', #86773 ) ;
#114030 = ORIENTED_EDGE ( 'NONE', *, *, #129132, .T. ) ;
#114029 = EDGE_CURVE ( 'NONE', #46180, #124509, #65768, .T. ) ;
#114031 = CARTESIAN_POINT ( 'NONE',  ( 64.95376352523145158, -6.109999999999998543, -3.741295971395162543E-16 ) ) ;
#114032 = VERTEX_POINT ( 'NONE', #22192 ) ;
#114033 = LINE ( 'NONE', #45953, #48742 ) ;
#114034 = ADVANCED_FACE ( 'NONE', ( #31672 ), #55576, .F. ) ;
#114035 = VECTOR ( 'NONE', #105430, 1000.000000000000000 ) ;
#114036 = VERTEX_POINT ( 'NONE', #75890 ) ;
#114037 = SURFACE_STYLE_USAGE ( .BOTH. , #82164 ) ;
#114038 = EDGE_CURVE ( 'NONE', #15743, #79053, #123291, .T. ) ;
#114039 = EDGE_CURVE ( 'NONE', #43696, #4583, #24187, .T. ) ;
#114040 = DIRECTION ( 'NONE',  ( 0.6830127018922181881, 0.6830127018922202975, -0.2588190451025214056 ) ) ;
#114041 = CARTESIAN_POINT ( 'NONE',  ( -6.640000000000001457, 12.19802518668052649, 4.711086268963014412 ) ) ;
#114042 = DIRECTION ( 'NONE',  ( 1.000000000000000000, 0.000000000000000000, 0.000000000000000000 ) ) ;
#114044 = CARTESIAN_POINT ( 'NONE',  ( -17.22995720542194675, 21.73644205237997440, 5.000000000000000888 ) ) ;
#114043 = LINE ( 'NONE', #74858, #6433 ) ;
#114045 = FACE_OUTER_BOUND ( 'NONE', #83715, .T. ) ;
#114046 = LINE ( 'NONE', #14736, #41657 ) ;
#114047 = ORIENTED_EDGE ( 'NONE', *, *, #101716, .T. ) ;
#114048 = ORIENTED_EDGE ( 'NONE', *, *, #9758, .F. ) ;
#114049 = CARTESIAN_POINT ( 'NONE',  ( 31.49999999999978684, 3.073033219394658122, -6.593910359670897670 ) ) ;
#114050 = DIRECTION ( 'NONE',  ( 0.7071067811865486830, -0.7071067811865464625, -0.000000000000000000 ) ) ;
#114051 = EDGE_LOOP ( 'NONE', ( #11305, #50953, #18331, #11744 ) ) ;
#114052 = ORIENTED_EDGE ( 'NONE', *, *, #132032, .F. ) ;
#114053 = EDGE_LOOP ( 'NONE', ( #59643, #108297, #119490, #101601 ) ) ;
#114054 = EDGE_CURVE ( 'NONE', #38978, #27213, #119357, .T. ) ;
#114055 = ADVANCED_FACE ( 'NONE', ( #12038 ), #87481, .F. ) ;
#114056 = CARTESIAN_POINT ( 'NONE',  ( -12.69999999999999929, -59.76999999999998892, 24.34531699603381938 ) ) ;
#114057 = AXIS2_PLACEMENT_3D ( 'NONE', #58763, #90637, #35569 ) ;
#114058 = ORIENTED_EDGE ( 'NONE', *, *, #12886, .T. ) ;
#114059 = DIRECTION ( 'NONE',  ( -0.7071067811865487940, 0.7071067811865463515, 0.000000000000000000 ) ) ;
#114060 = EDGE_CURVE ( 'NONE', #115520, #76434, #131697, .T. ) ;
#114061 = LINE ( 'NONE', #57571, #49337 ) ;
#114062 = CARTESIAN_POINT ( 'NONE',  ( 2.254569808101886341, -6.871911579029512218, 3.967499999999996252 ) ) ;
#114063 = CARTESIAN_POINT ( 'NONE',  ( 22.25000000000000000, 2.143131898507868051E-16, -1.749999999999999778 ) ) ;
#114064 = ORIENTED_EDGE ( 'NONE', *, *, #57741, .F. ) ;
#114065 = CARTESIAN_POINT ( 'NONE',  ( -34.42500000000001137, -22.22500000000000142, 5.000000000000000000 ) ) ;
#114066 = LINE ( 'NONE', #101762, #67463 ) ;
#114067 = FACE_OUTER_BOUND ( 'NONE', #13500, .T. ) ;
#114068 = EDGE_CURVE ( 'NONE', #42161, #63574, #76627, .T. ) ;
#114069 = AXIS2_PLACEMENT_3D ( 'NONE', #142971, #22588, #11718 ) ;
#114071 = ORIENTED_EDGE ( 'NONE', *, *, #46153, .F. ) ;
#114070 = CARTESIAN_POINT ( 'NONE',  ( -63.18398860626900415, 28.73617430169831621, 5.000000000000000000 ) ) ;
#114072 = VECTOR ( 'NONE', #122746, 1000.000000000000000 ) ;
#114073 = VERTEX_POINT ( 'NONE', #97617 ) ;
#114074 = LINE ( 'NONE', #127084, #84364 ) ;
#114075 = DIRECTION ( 'NONE',  ( -0.000000000000000000, 0.000000000000000000, 1.000000000000000000 ) ) ;
#114076 = VECTOR ( 'NONE', #14597, 1000.000000000000227 ) ;
#114077 = CARTESIAN_POINT ( 'NONE',  ( -3.343500094706353121, -22.22500000000000142, -6.967410892577142079 ) ) ;
#114079 = VERTEX_POINT ( 'NONE', #141879 ) ;
#114078 = VECTOR ( 'NONE', #40095, 1000.000000000000000 ) ;
#114080 =( NAMED_UNIT ( * ) SI_UNIT ( $, .STERADIAN. ) SOLID_ANGLE_UNIT ( ) );
#114081 = DIRECTION ( 'NONE',  ( -1.000000000000000000, -0.000000000000000000, -0.000000000000000000 ) ) ;
#114082 = LINE ( 'NONE', #103197, #44879 ) ;
#114083 = DIRECTION ( 'NONE',  ( -0.6830127018922181881, 0.6830127018922202975, -0.2588190451025214056 ) ) ;
#114084 = FACE_OUTER_BOUND ( 'NONE', #20782, .T. ) ;
#114085 = VECTOR ( 'NONE', #94096, 999.9999999999998863 ) ;
#114086 = ADVANCED_FACE ( 'NONE', ( #10599 ), #143274, .F. ) ;
#114087 = CIRCLE ( 'NONE', #93285, 2.055000000000001048 ) ;
#114088 = ORIENTED_EDGE ( 'NONE', *, *, #87402, .F. ) ;
#114089 =( GEOMETRIC_REPRESENTATION_CONTEXT ( 3 ) GLOBAL_UNCERTAINTY_ASSIGNED_CONTEXT ( ( #121404 ) ) GLOBAL_UNIT_ASSIGNED_CONTEXT ( ( #97784, #111515, #86208 ) ) REPRESENTATION_CONTEXT ( 'NONE', 'WORKASPACE' ) );
#114090 = LINE ( 'NONE', #3848, #67041 ) ;
#114091 = LINE ( 'NONE', #114773, #53924 ) ;
#114092 = CARTESIAN_POINT ( 'NONE',  ( 7.045806282870439752, 5.278424836066143655, -3.047499999999997655 ) ) ;
#114093 = DIRECTION ( 'NONE',  ( 0.3543493200069163240, 0.000000000000000000, -0.9351131265310288487 ) ) ;
#114094 = DIRECTION ( 'NONE',  ( -0.3543493200069162685, -0.000000000000000000, -0.9351131265310288487 ) ) ;
#114095 = ORIENTED_EDGE ( 'NONE', *, *, #78222, .F. ) ;
#114096 = EDGE_CURVE ( 'NONE', #99824, #13806, #33140, .T. ) ;
#114097 = EDGE_LOOP ( 'NONE', ( #113142, #64658, #95883, #112151 ) ) ;
#114098 = EDGE_CURVE ( 'NONE', #107625, #75066, #9304, .T. ) ;
#114099 = LINE ( 'NONE', #34400, #27128 ) ;
#114100 = DIRECTION ( 'NONE',  ( 1.000000000000000000, 0.000000000000000000, 0.000000000000000000 ) ) ;
#114101 = EDGE_CURVE ( 'NONE', #100573, #9707, #26502, .T. ) ;
#114102 = CARTESIAN_POINT ( 'NONE',  ( 8.582903141435219041, 3.967499999999992699, -6.871911579029513994 ) ) ;
#114103 = CARTESIAN_POINT ( 'NONE',  ( 65.85002705046288440, -5.819803920172573086, -5.819803920172573086 ) ) ;
#114104 = VECTOR ( 'NONE', #98932, 1000.000000000000000 ) ;
#114105 = LINE ( 'NONE', #116951, #41537 ) ;
#114106 = LINE ( 'NONE', #1726, #136256 ) ;
#114107 = DIRECTION ( 'NONE',  ( 0.7071067811865486830, -0.7071067811865464625, -0.000000000000000000 ) ) ;
#114108 = VERTEX_POINT ( 'NONE', #101916 ) ;
#114109 = LINE ( 'NONE', #103221, #11763 ) ;
#114110 = DIRECTION ( 'NONE',  ( -0.7071067811865486830, -0.7071067811865464625, 0.000000000000000000 ) ) ;
#114111 = CARTESIAN_POINT ( 'NONE',  ( -48.18398860626899705, 28.73617430169820608, 5.000000000000000000 ) ) ;
#114112 = CARTESIAN_POINT ( 'NONE',  ( 60.28709685856478728, 3.054999999999997939, 5.291415217122920289 ) ) ;
#114113 = AXIS2_PLACEMENT_3D ( 'NONE', #83964, #62191, #116555 ) ;
#114114 = CARTESIAN_POINT ( 'NONE',  ( 13.13598696172163116, 2.500000000000000444, 0.000000000000000000 ) ) ;
#114115 = CARTESIAN_POINT ( 'NONE',  ( -34.92500000000001137, 5.816654386410375466, 4.500000000000000888 ) ) ;
#114116 = AXIS2_PLACEMENT_3D ( 'NONE', #89477, #11900, #133713 ) ;
#114117 = ORIENTED_EDGE ( 'NONE', *, *, #96503, .F. ) ;
#114118 = LINE ( 'NONE', #14801, #62215 ) ;
#114119 = ORIENTED_EDGE ( 'NONE', *, *, #78242, .F. ) ;
#114120 = CARTESIAN_POINT ( 'NONE',  ( 25.49999999999982592, 3.431123077392145948, 4.000000000000000000 ) ) ;
#114121 = FACE_OUTER_BOUND ( 'NONE', #95622, .T. ) ;
#114122 = PLANE ( 'NONE',  #88232 ) ;
#114123 = CARTESIAN_POINT ( 'NONE',  ( 0.000000000000000000, 0.000000000000000000, 5.000000000000000000 ) ) ;
#114124 = CARTESIAN_POINT ( 'NONE',  ( -66.18398860626901126, 28.73617430169833753, 5.000000000000000000 ) ) ;
#114125 = DIRECTION ( 'NONE',  ( 0.000000000000000000, -1.000000000000000000, 0.000000000000000000 ) ) ;
#114126 = ORIENTED_EDGE ( 'NONE', *, *, #594, .F. ) ;
#114127 = ORIENTED_EDGE ( 'NONE', *, *, #70637, .T. ) ;
#114128 = CARTESIAN_POINT ( 'NONE',  ( -75.29974487139158157, -27.71228299555258445, 4.000000000000000000 ) ) ;
#114129 = LINE ( 'NONE', #92355, #5197 ) ;
#114130 = UNCERTAINTY_MEASURE_WITH_UNIT (LENGTH_MEASURE( 1.000000000000000082E-05 ), #53299, 'distance_accuracy_value', 'NONE');
#114131 = DIRECTION ( 'NONE',  ( 0.000000000000000000, -1.000000000000000000, 0.000000000000000000 ) ) ;
#114132 =( BOUNDED_CURVE ( )  B_SPLINE_CURVE ( 3, ( #103856, #136506, #124926, #82870 ),
 .UNSPECIFIED., .F., .T. ) 
 B_SPLINE_CURVE_WITH_KNOTS ( ( 4, 4 ),
 ( 0.06988172079111230894, 0.1872541115065302075 ),
 .UNSPECIFIED. ) 
 CURVE ( )  GEOMETRIC_REPRESENTATION_ITEM ( )  RATIONAL_B_SPLINE_CURVE ( ( 1.000000000000000000, 0.9988523062762910687, 0.9988523062762910687, 1.000000000000000000 ) ) 
 REPRESENTATION_ITEM ( '' )  );
#114133 = CARTESIAN_POINT ( 'NONE',  ( 21.72281430457044493, -21.72500000000000142, 5.000000000000000000 ) ) ;
#114134 = CARTESIAN_POINT ( 'NONE',  ( 75.91252705046288440, -7.949999999999998401, -4.867971026610728450E-16 ) ) ;
#114135 = CARTESIAN_POINT ( 'NONE',  ( 0.000000000000000000, 0.000000000000000000, -8.000000000000001776 ) ) ;
#114136 = ORIENTED_EDGE ( 'NONE', *, *, #124687, .T. ) ;
#114137 = CARTESIAN_POINT ( 'NONE',  ( 66.77083333333332860, -7.949999999999999289, -2.130196079827426203 ) ) ;
#114138 = CARTESIAN_POINT ( 'NONE',  ( 8.207106781186487510, -20.24070752338407431, 5.000000000000000000 ) ) ;
#114139 = LINE ( 'NONE', #14824, #106442 ) ;
#114141 = VECTOR ( 'NONE', #81417, 1000.000000000000000 ) ;
#114140 = CARTESIAN_POINT ( 'NONE',  ( 4.499999999999976019, 0.4497235411627491519, -5.599840258123530035 ) ) ;
#114142 = EDGE_CURVE ( 'NONE', #140579, #32809, #80891, .T. ) ;
#114143 = VECTOR ( 'NONE', #142339, 1000.000000000000000 ) ;
#114144 = ORIENTED_EDGE ( 'NONE', *, *, #75665, .T. ) ;
#114145 = DIRECTION ( 'NONE',  ( -0.6830127018922180770, -0.6830127018922204085, -0.2588190451025213501 ) ) ;
#114146 = CARTESIAN_POINT ( 'NONE',  ( 17.85999999999999943, -2.055000000000000160, 0.000000000000000000 ) ) ;
#114147 = CARTESIAN_POINT ( 'NONE',  ( 69.85459685856476142, -1.637169565754161615, 6.110000000000000320 ) ) ;
#114148 = DIRECTION ( 'NONE',  ( 1.000000000000000000, 0.000000000000000000, 0.000000000000000000 ) ) ;
#114149 = ORIENTED_EDGE ( 'NONE', *, *, #65628, .T. ) ;
#114150 = VERTEX_POINT ( 'NONE', #48981 ) ;
#114151 = VECTOR ( 'NONE', #81591, 999.9999999999998863 ) ;
#114152 = CARTESIAN_POINT ( 'NONE',  ( 27.81349135397621453, -15.74070752338412760, 8.904080028138874781 ) ) ;
#114153 = DIRECTION ( 'NONE',  ( -0.7071067811865486830, 0.7071067811865464625, 0.000000000000000000 ) ) ;
#114154 = CARTESIAN_POINT ( 'NONE',  ( 44.16666666666665719, 6.884901960086285300, 3.975000000000003642 ) ) ;
#114155 = EDGE_CURVE ( 'NONE', #28590, #126135, #4682, .T. ) ;
#114156 = CARTESIAN_POINT ( 'NONE',  ( 72.48921356237309510, -27.52281430457106026, 5.000000000000000000 ) ) ;
#114158 = ORIENTED_EDGE ( 'NONE', *, *, #129278, .T. ) ;
#114157 = DIRECTION ( 'NONE',  ( -0.000000000000000000, -0.3543493200069152693, 0.9351131265310292928 ) ) ;
#114159 = EDGE_CURVE ( 'NONE', #133751, #54071, #53847, .T. ) ;
#114160 = PLANE ( 'NONE',  #115539 ) ;
#114161 = CARTESIAN_POINT ( 'NONE',  ( -45.18398860626900415, 28.73617430169818832, 5.000000000000000000 ) ) ;
#114162 = AXIS2_PLACEMENT_3D ( 'NONE', #134694, #80313, #23769 ) ;
#114163 = CARTESIAN_POINT ( 'NONE',  ( 42.48921356237308800, -27.52281430457085065, 5.000000000000000000 ) ) ;
#114164 = CARTESIAN_POINT ( 'NONE',  ( 42.18398860626899705, 28.73617430169816700, 5.000000000000000000 ) ) ;
#114165 = ORIENTED_EDGE ( 'NONE', *, *, #23148, .F. ) ;
#114166 = ORIENTED_EDGE ( 'NONE', *, *, #87740, .T. ) ;
#114167 = EDGE_CURVE ( 'NONE', #57842, #129322, #25052, .T. ) ;
#114168 =( LENGTH_UNIT ( ) NAMED_UNIT ( * ) SI_UNIT ( .MILLI., .METRE. ) );
#114169 = LINE ( 'NONE', #14853, #90384 ) ;
#114170 = CARTESIAN_POINT ( 'NONE',  ( 19.10840764549667270, -2.500000000000000888, 0.000000000000000000 ) ) ;
#114171 = CARTESIAN_POINT ( 'NONE',  ( -14.99451991528749595, 28.92564299267948513, 4.000000000000000000 ) ) ;
#114172 = CARTESIAN_POINT ( 'NONE',  ( -5.994519915287488843, 28.92564299267942118, 4.000000000000000000 ) ) ;
#114173 = ORIENTED_EDGE ( 'NONE', *, *, #85351, .T. ) ;
#114174 = VERTEX_POINT ( 'NONE', #15572 ) ;
#114175 = CIRCLE ( 'NONE', #74884, 2.500000000000000444 ) ;
#114176 = LINE ( 'NONE', #135252, #33065 ) ;
#114177 = PLANE ( 'NONE',  #102319 ) ;
#114178 = ADVANCED_FACE ( 'NONE', ( #59853 ), #104020, .F. ) ;
#114179 = VECTOR ( 'NONE', #86959, 1000.000000000000227 ) ;
#114180 = ORIENTED_EDGE ( 'NONE', *, *, #265, .F. ) ;
#114181 = ORIENTED_EDGE ( 'NONE', *, *, #39044, .F. ) ;
#114182 = LINE ( 'NONE', #59142, #135947 ) ;
#114183 = FACE_OUTER_BOUND ( 'NONE', #143033, .T. ) ;
#114184 = VECTOR ( 'NONE', #103882, 1000.000000000000227 ) ;
#114185 =( GEOMETRIC_REPRESENTATION_CONTEXT ( 3 ) GLOBAL_UNCERTAINTY_ASSIGNED_CONTEXT ( ( #46024 ) ) GLOBAL_UNIT_ASSIGNED_CONTEXT ( ( #138273, #51274, #104174 ) ) REPRESENTATION_CONTEXT ( 'NONE', 'WORKASPACE' ) );
#114186 = ADVANCED_FACE ( 'NONE', ( #91745 ), #113487, .F. ) ;
#114187 = ORIENTED_EDGE ( 'NONE', *, *, #80662, .T. ) ;
#114188 = FACE_BOUND ( 'NONE', #127185, .T. ) ;
#114189 = DIRECTION ( 'NONE',  ( -0.000000000000000000, 0.000000000000000000, 1.000000000000000000 ) ) ;
#114190 = CARTESIAN_POINT ( 'NONE',  ( -11.81601139373100651, 28.73617430169779041, 5.000000000000000000 ) ) ;
#114191 = CARTESIAN_POINT ( 'NONE',  ( 68.99451991528748351, 28.92564299267986172, 4.000000000000000000 ) ) ;
#114192 = CARTESIAN_POINT ( 'NONE',  ( 28.00000000000002487, -52.14999999999999147, 34.92500000000003268 ) ) ;
#114193 = DIRECTION ( 'NONE',  ( 1.000000000000000000, 0.000000000000000000, 0.000000000000000000 ) ) ;
#114194 = DIRECTION ( 'NONE',  ( 0.000000000000000000, 0.000000000000000000, 1.000000000000000000 ) ) ;
#114195 = ORIENTED_EDGE ( 'NONE', *, *, #121931, .T. ) ;
#114196 = VECTOR ( 'NONE', #20308, 1000.000000000000000 ) ;
#114197 = VERTEX_POINT ( 'NONE', #112099 ) ;
#114198 = CARTESIAN_POINT ( 'NONE',  ( 98.20376352523145158, 6.109999999999998543, 1.122388791418548911E-15 ) ) ;
#114199 = VERTEX_POINT ( 'NONE', #80197 ) ;
#114200 = DIRECTION ( 'NONE',  ( 0.6830127018922181881, 0.6830127018922202975, -0.2588190451025214056 ) ) ;
#114201 = ADVANCED_FACE ( 'NONE', ( #102650 ), #12747, .F. ) ;
#114202 = DIRECTION ( 'NONE',  ( 0.7071067811865487940, 0.7071067811865463515, 0.000000000000000000 ) ) ;
#114203 = VECTOR ( 'NONE', #88776, 999.9999999999998863 ) ;
#114204 = LINE ( 'NONE', #12738, #6121 ) ;
#114205 = EDGE_CURVE ( 'NONE', #125931, #97996, #101195, .T. ) ;
#114206 = EDGE_CURVE ( 'NONE', #121707, #120720, #35269, .T. ) ;
#114207 = CARTESIAN_POINT ( 'NONE',  ( -56.99451991528749062, 28.92564299267978001, 4.000000000000000000 ) ) ;
#114208 = VERTEX_POINT ( 'NONE', #47584 ) ;
#114209 = DIRECTION ( 'NONE',  ( 0.7071067811865487940, 0.7071067811865463515, 0.000000000000000000 ) ) ;
#114210 = FACE_OUTER_BOUND ( 'NONE', #107548, .T. ) ;
#114211 = CIRCLE ( 'NONE', #81867, 5.968999999999998529 ) ;
#114212 = CARTESIAN_POINT ( 'NONE',  ( 25.40000000000001279, 7.747411163680002488, -1.763262371054023170 ) ) ;
#114214 = PLANE ( 'NONE',  #142311 ) ;
#114213 = LINE ( 'NONE', #46885, #59649 ) ;
#114215 = LINE ( 'NONE', #14895, #134185 ) ;
#114216 = CARTESIAN_POINT ( 'NONE',  ( -1.180000000000000382, 6.391994993740215847, 10.00000000000000000 ) ) ;
#114217 = ORIENTED_EDGE ( 'NONE', *, *, #13989, .F. ) ;
#114218 = EDGE_CURVE ( 'NONE', #95318, #22921, #68600, .T. ) ;
#114219 = CARTESIAN_POINT ( 'NONE',  ( 11.30673006690394189, -3.740707523384244837, 12.88036043432864908 ) ) ;
#114220 = DIRECTION ( 'NONE',  ( 0.7071067811865487940, 0.7071067811865463515, 0.000000000000000000 ) ) ;
#114221 = AXIS2_PLACEMENT_3D ( 'NONE', #69178, #47463, #45305 ) ;
#114222 = VERTEX_POINT ( 'NONE', #70052 ) ;
#114223 = ORIENTED_EDGE ( 'NONE', *, *, #94279, .T. ) ;
#114224 = EDGE_CURVE ( 'NONE', #113754, #130071, #114215, .T. ) ;
#114226 = ORIENTED_EDGE ( 'NONE', *, *, #140245, .T. ) ;
#114225 = ADVANCED_FACE ( 'NONE', ( #103319 ), #48248, .F. ) ;
#114227 = CARTESIAN_POINT ( 'NONE',  ( 48.12543019189810423, 5.291415217122919401, 3.055000000000002824 ) ) ;
#114228 = VERTEX_POINT ( 'NONE', #71442 ) ;
#114229 = VECTOR ( 'NONE', #105453, 999.9999999999998863 ) ;
#114230 = AXIS2_PLACEMENT_3D ( 'NONE', #70787, #93223, #59901 ) ;
#114231 = CARTESIAN_POINT ( 'NONE',  ( 9.962472949537104938, -7.464222240803106570E-16, -6.094999999999989981 ) ) ;
#114232 = AXIS2_PLACEMENT_3D ( 'NONE', #71738, #59449, #137706 ) ;
#114233 = CARTESIAN_POINT ( 'NONE',  ( -7.150129580834428289, 11.08364541797794800, -28.03538095272935848 ) ) ;
#114234 = ADVANCED_FACE ( 'NONE', ( #105461 ), #6126, .T. ) ;
#114235 = ORIENTED_EDGE ( 'NONE', *, *, #17898, .T. ) ;
#114236 = LINE ( 'NONE', #35288, #78054 ) ;
#114237 = ORIENTED_EDGE ( 'NONE', *, *, #55127, .T. ) ;
#114238 = DIRECTION ( 'NONE',  ( 0.7071067811865487940, 0.7071067811865463515, 0.000000000000000000 ) ) ;
#114239 = EDGE_CURVE ( 'NONE', #101225, #21579, #95315, .T. ) ;
#114241 = ORIENTED_EDGE ( 'NONE', *, *, #38903, .F. ) ;
#114240 = FACE_OUTER_BOUND ( 'NONE', #104792, .T. ) ;
#114242 = VERTEX_POINT ( 'NONE', #38808 ) ;
#114243 = LINE ( 'NONE', #105490, #12137 ) ;
#114244 = CARTESIAN_POINT ( 'NONE',  ( -22.49999999999984368, -17.91344420646044711, 1.358650452708411782 ) ) ;
#114245 = DIRECTION ( 'NONE',  ( -0.6830127018922180770, -0.6830127018922204085, -0.2588190451025213501 ) ) ;
#114246 =( BOUNDED_CURVE ( )  B_SPLINE_CURVE ( 3, ( #76392, #21286, #109715, #10386 ),
 .UNSPECIFIED., .F., .T. ) 
 B_SPLINE_CURVE_WITH_KNOTS ( ( 4, 4 ),
 ( 1.901594255663605182, 1.933014472006535422 ),
 .UNSPECIFIED. ) 
 CURVE ( )  GEOMETRIC_REPRESENTATION_ITEM ( )  RATIONAL_B_SPLINE_CURVE ( ( 1.000000000000000000, 0.9999177325257868620, 0.9999177325257868620, 1.000000000000000000 ) ) 
 REPRESENTATION_ITEM ( '' )  );
#114247 = VERTEX_POINT ( 'NONE', #96707 ) ;
#114248 = DIRECTION ( 'NONE',  ( -0.6830127018922181881, 0.6830127018922202975, -0.2588190451025214056 ) ) ;
#114249 = VERTEX_POINT ( 'NONE', #117058 ) ;
#114250 = VERTEX_POINT ( 'NONE', #139579 ) ;
#114251 = EDGE_LOOP ( 'NONE', ( #76940, #106345, #31262, #55714, #105037 ) ) ;
#114252 = ORIENTED_EDGE ( 'NONE', *, *, #6492, .F. ) ;
#114253 = CARTESIAN_POINT ( 'NONE',  ( -38.99451991528749062, 28.92564299267965211, 4.000000000000000000 ) ) ;
#114254 = CARTESIAN_POINT ( 'NONE',  ( -21.79289321881330466, 15.75929247661555976, 5.000000000000000000 ) ) ;
#114255 = LINE ( 'NONE', #136713, #23896 ) ;
#114256 = DIRECTION ( 'NONE',  ( -0.7071067811865486830, -0.7071067811865464625, 0.000000000000000000 ) ) ;
#114257 = CARTESIAN_POINT ( 'NONE',  ( -24.18398860626899705, 28.73617430169804265, 5.000000000000000000 ) ) ;
#114258 = VECTOR ( 'NONE', #7698, 1000.000000000000000 ) ;
#114259 = ORIENTED_EDGE ( 'NONE', *, *, #69358, .F. ) ;
#114260 = EDGE_CURVE ( 'NONE', #72669, #57481, #40263, .T. ) ;
#114261 = ADVANCED_FACE ( 'NONE', ( #8275 ), #7577, .F. ) ;
#114262 = EDGE_CURVE ( 'NONE', #50077, #60759, #5430, .T. ) ;
#114263 = CARTESIAN_POINT ( 'NONE',  ( 20.10373647476854941, 5.808823158059036373, 5.808823158059032821 ) ) ;
#114264 = CARTESIAN_POINT ( 'NONE',  ( -18.53421140649331633, 9.121673282332597665, 4.000000000000000000 ) ) ;
#114265 = CONICAL_SURFACE ( 'NONE', #17006, 2.500000000000000444, 0.9599310885968830309 ) ;
#114266 = CARTESIAN_POINT ( 'NONE',  ( 48.18398860626899705, 28.73617430169820608, 5.000000000000000000 ) ) ;
#114267 = LINE ( 'NONE', #126553, #104557 ) ;
#114268 = EDGE_LOOP ( 'NONE', ( #117137, #95437, #91650, #94063 ) ) ;
#114269 = VERTEX_POINT ( 'NONE', #84474 ) ;
#114270 = ORIENTED_EDGE ( 'NONE', *, *, #143065, .T. ) ;
#114271 = DIRECTION ( 'NONE',  ( -0.7071067811865487940, 0.7071067811865463515, -0.000000000000000000 ) ) ;
#114272 = CARTESIAN_POINT ( 'NONE',  ( 34.42499999999998295, 0.000000000000000000, 4.500000000000000888 ) ) ;
#114273 = UNCERTAINTY_MEASURE_WITH_UNIT (LENGTH_MEASURE( 1.000000000000000082E-05 ), #50834, 'distance_accuracy_value', 'NONE');
#114274 = CARTESIAN_POINT ( 'NONE',  ( -6.489213562373093325, -27.52281430457059841, 5.000000000000000000 ) ) ;
#114275 = CARTESIAN_POINT ( 'NONE',  ( -2.999999999999980016, 1.931123077392165488, 4.000000000000000000 ) ) ;
#114276 = ADVANCED_FACE ( 'NONE', ( #51121 ), #106899, .F. ) ;
#114277 = CARTESIAN_POINT ( 'NONE',  ( -5.999999999999963585, -2.904428200921325143, -6.989807076074931125 ) ) ;
#114278 = DIRECTION ( 'NONE',  ( 0.7071067811865486830, -0.7071067811865464625, -0.000000000000000000 ) ) ;
#114279 = AXIS2_PLACEMENT_3D ( 'NONE', #65025, #29499, #86044 ) ;
#114280 = DIRECTION ( 'NONE',  ( -0.000000000000000000, -0.3543493200069152693, 0.9351131265310292928 ) ) ;
#114281 = DIRECTION ( 'NONE',  ( -0.6830127018922181881, 0.6830127018922202975, -0.2588190451025214056 ) ) ;
#114282 = FACE_OUTER_BOUND ( 'NONE', #68628, .T. ) ;
#114283 = DIRECTION ( 'NONE',  ( 1.000000000000000000, 0.000000000000000000, 0.000000000000000000 ) ) ;
#114284 = CARTESIAN_POINT ( 'NONE',  ( 60.18398860626900415, 28.73617430169829490, 5.000000000000000000 ) ) ;
#114285 = EDGE_LOOP ( 'NONE', ( #43044, #85724, #110349, #139920 ) ) ;
#114286 = ORIENTED_EDGE ( 'NONE', *, *, #122197, .F. ) ;
#114287 = CARTESIAN_POINT ( 'NONE',  ( -17.20710678118642889, 9.759292476615625489, 5.000000000000000000 ) ) ;
#114289 = ORIENTED_EDGE ( 'NONE', *, *, #105418, .F. ) ;
#114288 = DIRECTION ( 'NONE',  ( -0.000000000000000000, -0.000000000000000000, 1.000000000000000000 ) ) ;
#114290 = PLANE ( 'NONE',  #23186 ) ;
#114291 = DIRECTION ( 'NONE',  ( 0.000000000000000000, 0.9976538855070753442, -0.06845965770171351383 ) ) ;
#114292 =( REPRESENTATION_RELATIONSHIP ('NONE','NONE', #69070, #9754 ) REPRESENTATION_RELATIONSHIP_WITH_TRANSFORMATION ( #19172 )SHAPE_REPRESENTATION_RELATIONSHIP( ) );
#114293 = ORIENTED_EDGE ( 'NONE', *, *, #10541, .F. ) ;
#114294 = LINE ( 'NONE', #124461, #108594 ) ;
#114295 = VERTEX_POINT ( 'NONE', #40947 ) ;
#114296 = FACE_OUTER_BOUND ( 'NONE', #62443, .T. ) ;
#114297 = ORIENTED_EDGE ( 'NONE', *, *, #19660, .F. ) ;
#114298 = COLOUR_RGB ( '', 0.09019608, 0.27058824, 0.51372549) ;
#114299 = CARTESIAN_POINT ( 'NONE',  ( 5.292986735706907808, -21.74070752338406365, 4.999753212805221558 ) ) ;
#114300 = CARTESIAN_POINT ( 'NONE',  ( 104.2041937171295700, -6.884901960086285300, -3.975000000000000089 ) ) ;
#114301 = CARTESIAN_POINT ( 'NONE',  ( -5.994519915287488843, 28.92564299267942118, 4.000000000000000000 ) ) ;
#114302 = AXIS2_PLACEMENT_3D ( 'NONE', #44996, #89170, #137681 ) ;
#114303 = LINE ( 'NONE', #70141, #46292 ) ;
#114304 = VERTEX_POINT ( 'NONE', #115593 ) ;
#114305 = CARTESIAN_POINT ( 'NONE',  ( -34.92500000000001137, -9.908632306349543839, -7.176634499130168265 ) ) ;
#114306 = FACE_OUTER_BOUND ( 'NONE', #124991, .T. ) ;
#114307 = FACE_OUTER_BOUND ( 'NONE', #33338, .T. ) ;
#114308 = CARTESIAN_POINT ( 'NONE',  ( 26.54166666666666785, 3.047499999999993214, -5.278424836066146320 ) ) ;
#114309 = DIRECTION ( 'NONE',  ( 0.000000000000000000, 1.000000000000000000, -0.000000000000000000 ) ) ;
#114310 = CARTESIAN_POINT ( 'NONE',  ( 24.48921356237309510, -27.52281430457072631, 5.000000000000000000 ) ) ;
#114311 = DIRECTION ( 'NONE',  ( 1.000000000000000000, 1.224606353822377258E-16, 0.000000000000000000 ) ) ;
#114312 = ORIENTED_EDGE ( 'NONE', *, *, #109382, .F. ) ;
#114313 = AXIS2_PLACEMENT_3D ( 'NONE', #66141, #129953, #30654 ) ;
#114314 = DIRECTION ( 'NONE',  ( -0.6830127018922181881, 0.6830127018922202975, -0.2588190451025214056 ) ) ;
#114315 = ORIENTED_EDGE ( 'NONE', *, *, #1573, .F. ) ;
#114316 = CARTESIAN_POINT ( 'NONE',  ( 91.14626352523144703, -4.472830434245840259, 4.472830434245839371 ) ) ;
#114317 = PLANE ( 'NONE',  #87157 ) ;
#114318 = SURFACE_SIDE_STYLE ('',( #95236 ) ) ;
#114319 = CARTESIAN_POINT ( 'NONE',  ( 34.45011844616453800, 19.51628081163730499, 5.000000000000001776 ) ) ;
#114320 = CARTESIAN_POINT ( 'NONE',  ( -31.49999999999976552, 4.087461875839202285, 4.000000000000000000 ) ) ;
#114321 = ORIENTED_EDGE ( 'NONE', *, *, #28317, .F. ) ;
#114322 = DIRECTION ( 'NONE',  ( -0.7071067811865486830, -0.7071067811865464625, 0.000000000000000000 ) ) ;
#114323 = VECTOR ( 'NONE', #132132, 1000.000000000000000 ) ;
#114324 = ADVANCED_FACE ( 'NONE', ( #138843 ), #85149, .F. ) ;
#114325 = CARTESIAN_POINT ( 'NONE',  ( 100.7500000000000000, -9.735942053221458872E-16, 7.950000000000000178 ) ) ;
#114326 = ORIENTED_EDGE ( 'NONE', *, *, #123562, .T. ) ;
#114327 = DIRECTION ( 'NONE',  ( -0.7071067811865486830, -0.7071067811865464625, 0.000000000000000000 ) ) ;
#114328 = ADVANCED_FACE ( 'NONE', ( #73580 ), #29337, .F. ) ;
#114329 = CARTESIAN_POINT ( 'NONE',  ( 3.250000000000000000, 0.000000000000000000, 0.000000000000000000 ) ) ;
#114331 = EDGE_LOOP ( 'NONE', ( #141477, #47825, #19452, #21674 ) ) ;
#114330 = CARTESIAN_POINT ( 'NONE',  ( 5.994519915287488843, 28.92564299267942118, 4.000000000000000000 ) ) ;
#114332 = LINE ( 'NONE', #15006, #8936 ) ;
#114333 = CARTESIAN_POINT ( 'NONE',  ( 12.48921356237309155, -27.52281430457064104, 5.000000000000000000 ) ) ;
#114334 = CARTESIAN_POINT ( 'NONE',  ( -25.49999999999981526, -5.947814304570765209, 5.000000000000000000 ) ) ;
#114335 = SURFACE_SIDE_STYLE ('',( #102041 ) ) ;
#114337 = EDGE_CURVE ( 'NONE', #111908, #65308, #111335, .T. ) ;
#114336 = VECTOR ( 'NONE', #127604, 1000.000000000000000 ) ;
#114339 = ORIENTED_EDGE ( 'NONE', *, *, #34840, .T. ) ;
#114338 = ADVANCED_FACE ( 'NONE', ( #138120 ), #127219, .F. ) ;
#114340 = ORIENTED_EDGE ( 'NONE', *, *, #77253, .F. ) ;
#114341 = VERTEX_POINT ( 'NONE', #72911 ) ;
#114342 = CARTESIAN_POINT ( 'NONE',  ( 82.39626352523143282, 4.472830434245840259, -4.472830434245839371 ) ) ;
#114343 = AXIS2_PLACEMENT_3D ( 'NONE', #99231, #42770, #22384 ) ;
#114344 = EDGE_LOOP ( 'NONE', ( #14940, #139396, #125101, #8991 ) ) ;
#114345 = EDGE_CURVE ( 'NONE', #14650, #1294, #111067, .T. ) ;
#114346 = DIRECTION ( 'NONE',  ( -1.000000000000000000, -0.000000000000000000, 0.000000000000000000 ) ) ;
#114347 = CARTESIAN_POINT ( 'NONE',  ( -29.67183060077626422, 14.25929247661557397, 4.000000000000000000 ) ) ;
#114348 = AXIS2_PLACEMENT_3D ( 'NONE', #4764, #16381, #104844 ) ;
#114349 = LINE ( 'NONE', #15019, #142997 ) ;
#114350 = CARTESIAN_POINT ( 'NONE',  ( 48.48921356237309510, -27.52281430457089328, 5.000000000000000000 ) ) ;
#114351 = EDGE_LOOP ( 'NONE', ( #18509, #12862, #84693, #64593 ) ) ;
#114352 = CARTESIAN_POINT ( 'NONE',  ( 14.19331503651554272, 6.646281381260698673, 4.665372575888455664 ) ) ;
#114353 = CARTESIAN_POINT ( 'NONE',  ( -42.48921356237308800, -27.52281430457085065, 5.000000000000000000 ) ) ;
#114354 = EDGE_CURVE ( 'NONE', #142044, #46122, #64858, .T. ) ;
#114355 = CARTESIAN_POINT ( 'NONE',  ( 77.49543019189810877, 5.291415217122916737, 3.055000000000001936 ) ) ;
#114356 = ORIENTED_EDGE ( 'NONE', *, *, #11523, .T. ) ;
#114357 = DIRECTION ( 'NONE',  ( -0.6830127018922181881, 0.6830127018922202975, -0.2588190451025214056 ) ) ;
#114358 = CARTESIAN_POINT ( 'NONE',  ( 34.64169371712954160, -2.130196079827424871, -7.949999999999998401 ) ) ;
#114359 = VECTOR ( 'NONE', #8147, 1000.000000000000000 ) ;
#114360 = DIRECTION ( 'NONE',  ( -0.7071067811865486830, -0.7071067811865464625, 0.000000000000000000 ) ) ;
#114361 = ADVANCED_FACE ( 'NONE', ( #131525 ), #143109, .F. ) ;
#114362 = ORIENTED_EDGE ( 'NONE', *, *, #72000, .F. ) ;
#114363 = ORIENTED_EDGE ( 'NONE', *, *, #70204, .T. ) ;
#114364 = LINE ( 'NONE', #63419, #16808 ) ;
#114365 = DIRECTION ( 'NONE',  ( -0.7071067811865486830, -0.7071067811865464625, 0.000000000000000000 ) ) ;
#114366 = CARTESIAN_POINT ( 'NONE',  ( 2.000000000000000000, 2.375000000000000000, 4.319999999999998508 ) ) ;
#114367 = ADVANCED_FACE ( 'NONE', ( #65594 ), #22716, .F. ) ;
#114368 = FACE_OUTER_BOUND ( 'NONE', #20203, .T. ) ;
#114369 = LINE ( 'NONE', #15040, #55775 ) ;
#114370 = FACE_OUTER_BOUND ( 'NONE', #78931, .T. ) ;
#114371 = CIRCLE ( 'NONE', #51890, 5.968999999999998529 ) ;
#114372 = ORIENTED_EDGE ( 'NONE', *, *, #59991, .T. ) ;
#114373 = EDGE_LOOP ( 'NONE', ( #115999, #60627, #31699, #74662 ) ) ;
#114374 = LINE ( 'NONE', #13611, #138334 ) ;
#114375 = ORIENTED_EDGE ( 'NONE', *, *, #40410, .T. ) ;
#114376 = ADVANCED_FACE ( 'NONE', ( #88018 ), #85867, .F. ) ;
#114377 = VECTOR ( 'NONE', #20048, 1000.000000000000000 ) ;
#114378 = EDGE_CURVE ( 'NONE', #101569, #108829, #41647, .T. ) ;
#114379 = DIRECTION ( 'NONE',  ( -0.7071067811865486830, -0.7071067811865464625, 0.000000000000000000 ) ) ;
#114380 = ORIENTED_EDGE ( 'NONE', *, *, #63346, .F. ) ;
#114381 = DIRECTION ( 'NONE',  ( -0.7071067811865486830, -0.7071067811865464625, 0.000000000000000000 ) ) ;
#114382 = LINE ( 'NONE', #37557, #121206 ) ;
#114383 = EDGE_CURVE ( 'NONE', #54251, #30424, #43802, .T. ) ;
#114384 = FACE_OUTER_BOUND ( 'NONE', #69910, .T. ) ;
#114385 = LINE ( 'NONE', #112263, #42119 ) ;
#114386 = ORIENTED_EDGE ( 'NONE', *, *, #12751, .F. ) ;
#114387 = ADVANCED_FACE ( 'NONE', ( #53992 ), #142415, .F. ) ;
#114388 = PLANE ( 'NONE',  #56508 ) ;
#114389 = CARTESIAN_POINT ( 'NONE',  ( -0.4892135623730947680, -27.52281430457055578, 5.000000000000000000 ) ) ;
#114390 = ORIENTED_EDGE ( 'NONE', *, *, #96960, .F. ) ;
#114391 = CARTESIAN_POINT ( 'NONE',  ( -32.29298673570672662, -21.74070752338405299, 4.999753212805210012 ) ) ;
#114392 = ORIENTED_EDGE ( 'NONE', *, *, #27781, .T. ) ;
#114393 = ORIENTED_EDGE ( 'NONE', *, *, #5371, .T. ) ;
#114394 = CARTESIAN_POINT ( 'NONE',  ( -33.32816939922329880, 5.259292476615662792, 4.000000000000000000 ) ) ;
#114395 = ORIENTED_EDGE ( 'NONE', *, *, #95104, .F. ) ;
#114396 = ORIENTED_EDGE ( 'NONE', *, *, #52381, .F. ) ;
#114397 = CARTESIAN_POINT ( 'NONE',  ( 2.924914550060625285, -9.629649721936179265E-32, 2.500000000000000444 ) ) ;
#114398 = AXIS2_PLACEMENT_3D ( 'NONE', #83032, #48985, #61326 ) ;
#114399 = ORIENTED_EDGE ( 'NONE', *, *, #121097, .T. ) ;
#114400 = CARTESIAN_POINT ( 'NONE',  ( 22.21321903303345024, 12.75929247661558641, 10.29404684609040643 ) ) ;
#114401 = VECTOR ( 'NONE', #35002, 1000.000000000000227 ) ;
#114402 = CARTESIAN_POINT ( 'NONE',  ( 50.53752705046289861, -9.735942053221456900E-16, 7.949999999999998401 ) ) ;
#114403 = CARTESIAN_POINT ( 'NONE',  ( 115.0629301918981042, 1.637169565754157174, 6.110000000000002984 ) ) ;
#114404 = FACE_OUTER_BOUND ( 'NONE', #57732, .T. ) ;
#114405 = EDGE_CURVE ( 'NONE', #94039, #81745, #30057, .T. ) ;
#114406 = CARTESIAN_POINT ( 'NONE',  ( -4.499999999999966249, -17.56887692260763245, 4.000000000000000000 ) ) ;
#114407 = DIRECTION ( 'NONE',  ( 0.7071067811865487940, 0.7071067811865463515, 0.000000000000000000 ) ) ;
#114408 = CARTESIAN_POINT ( 'NONE',  ( 5.700255128608413102, -27.71228299555201957, 4.000000000000000000 ) ) ;
#114409 = ADVANCED_FACE ( 'NONE', ( #111168 ), #141696, .F. ) ;
#114410 = LINE ( 'NONE', #24545, #102546 ) ;
#114411 = SURFACE_STYLE_USAGE ( .BOTH. , #70937 ) ;
#114412 = CARTESIAN_POINT ( 'NONE',  ( -12.69999999999998153, 0.000000000000000000, 0.000000000000000000 ) ) ;
#114413 = EDGE_LOOP ( 'NONE', ( #81381, #123728, #127453, #67701 ) ) ;
#114414 = DIRECTION ( 'NONE',  ( 0.000000000000000000, 0.000000000000000000, 1.000000000000000000 ) ) ;
#114416 = DIRECTION ( 'NONE',  ( 0.7071067811865486830, -0.7071067811865464625, -0.000000000000000000 ) ) ;
#114415 = AXIS2_PLACEMENT_3D ( 'NONE', #8491, #18675, #139800 ) ;
#114417 = CIRCLE ( 'NONE', #47421, 4.000000000000000000 ) ;
#114418 = ORIENTED_EDGE ( 'NONE', *, *, #132398, .T. ) ;
#114419 = EDGE_LOOP ( 'NONE', ( #44088, #135758, #107901, #61873 ) ) ;
#114420 = CARTESIAN_POINT ( 'NONE',  ( 2.125146193092330105, -14.24070752338413470, 9.401115078912654965 ) ) ;
#114421 = VERTEX_POINT ( 'NONE', #42398 ) ;
#114422 = CARTESIAN_POINT ( 'NONE',  ( 54.48921356237310221, -27.52281430457093236, 5.000000000000000000 ) ) ;
#114423 = DIRECTION ( 'NONE',  ( -0.000000000000000000, 0.3543493200069153248, 0.9351131265310292928 ) ) ;
#114424 = COLOUR_RGB ( '', 0.31764706, 0.68627451, 0.89019608) ;
#114425 = CARTESIAN_POINT ( 'NONE',  ( 34.42499999999998295, 5.977185695429338530, 5.000000000000000000 ) ) ;
#114426 = FACE_OUTER_BOUND ( 'NONE', #130828, .T. ) ;
#114427 = VERTEX_POINT ( 'NONE', #21336 ) ;
#114428 = ORIENTED_EDGE ( 'NONE', *, *, #139762, .F. ) ;
#114430 = VECTOR ( 'NONE', #52013, 1000.000000000000000 ) ;
#114429 = CARTESIAN_POINT ( 'NONE',  ( -27.32816939922333432, 8.259292476615641476, 4.000000000000000000 ) ) ;
#114431 = EDGE_CURVE ( 'NONE', #107568, #49762, #132270, .T. ) ;
#114432 = CARTESIAN_POINT ( 'NONE',  ( 27.33790314143521982, -6.871911579029513106, -3.967499999999993587 ) ) ;
#114433 = CARTESIAN_POINT ( 'NONE',  ( 10.03498081871643954, -8.432637487761464712, 4.375000000000000888 ) ) ;
#114434 = CARTESIAN_POINT ( 'NONE',  ( 14.25160702508294541, -9.301495327579425876, 1.950216952696393280 ) ) ;
#114435 = ORIENTED_EDGE ( 'NONE', *, *, #107412, .T. ) ;
#114436 = ORIENTED_EDGE ( 'NONE', *, *, #95997, .T. ) ;
#114437 = ORIENTED_EDGE ( 'NONE', *, *, #109264, .F. ) ;
#114438 = CARTESIAN_POINT ( 'NONE',  ( -22.49999999999984723, 18.05218569542898877, 5.000000000000000000 ) ) ;
#114439 = DIRECTION ( 'NONE',  ( 0.3543493200069162685, -0.000000000000000000, -0.9351131265310288487 ) ) ;
#114440 = LINE ( 'NONE', #102164, #142300 ) ;
#114441 = CYLINDRICAL_SURFACE ( 'NONE', #7908, 3.000000000000002665 ) ;
#114442 = ORIENTED_EDGE ( 'NONE', *, *, #25541, .T. ) ;
#114443 = CARTESIAN_POINT ( 'NONE',  ( -9.183988606268997046, 28.73617430169793607, 5.000000000000000000 ) ) ;
#114444 = DIRECTION ( 'NONE',  ( -0.000000000000000000, -0.3543493200069152693, 0.9351131265310292928 ) ) ;
#114445 = AXIS2_PLACEMENT_3D ( 'NONE', #1670, #122047, #25595 ) ;
#114446 = DIRECTION ( 'NONE',  ( -0.7071067811865487940, 0.7071067811865463515, 0.000000000000000000 ) ) ;
#114447 = CARTESIAN_POINT ( 'NONE',  ( 0.000000000000000000, 0.000000000000000000, 5.000000000000000000 ) ) ;
#114448 = ORIENTED_EDGE ( 'NONE', *, *, #30848, .T. ) ;
#114449 = CARTESIAN_POINT ( 'NONE',  ( 0.000000000000000000, 0.000000000000000000, 0.000000000000000000 ) ) ;
#114450 = ORIENTED_EDGE ( 'NONE', *, *, #22962, .T. ) ;
#114452 = ORIENTED_EDGE ( 'NONE', *, *, #120268, .F. ) ;
#114451 =( LENGTH_UNIT ( ) NAMED_UNIT ( * ) SI_UNIT ( .MILLI., .METRE. ) );
#114453 = ORIENTED_EDGE ( 'NONE', *, *, #118465, .F. ) ;
#114454 = FACE_OUTER_BOUND ( 'NONE', #120089, .T. ) ;
#114455 = CARTESIAN_POINT ( 'NONE',  ( 10.15640092694706453, 0.000000000000000000, 2.500000000000000444 ) ) ;
#114456 = VERTEX_POINT ( 'NONE', #86608 ) ;
#114457 = CARTESIAN_POINT ( 'NONE',  ( 128.1499999999997499, -49.14999999999999147, 40.92499999999998295 ) ) ;
#114458 = CARTESIAN_POINT ( 'NONE',  ( 11.70025512860841133, -27.71228299555198049, 4.000000000000000000 ) ) ;
#114459 = CARTESIAN_POINT ( 'NONE',  ( -3.183988606268992161, 28.73617430169789699, 5.000000000000000000 ) ) ;
#114460 = CARTESIAN_POINT ( 'NONE',  ( 32.43293019189810877, 1.637169565754156730, 6.110000000000001208 ) ) ;
#114461 = DIRECTION ( 'NONE',  ( 0.7071067811865487940, 0.7071067811865463515, 0.000000000000000000 ) ) ;
#114462 = CARTESIAN_POINT ( 'NONE',  ( 47.03752705046289151, -9.735942053221456900E-16, 7.949999999999998401 ) ) ;
#114463 = FACE_OUTER_BOUND ( 'NONE', #88515, .T. ) ;
#114464 = LINE ( 'NONE', #37657, #7789 ) ;
#114465 = CARTESIAN_POINT ( 'NONE',  ( -48.29974487139158867, -27.71228299555239971, 4.000000000000000000 ) ) ;
#114466 = CARTESIAN_POINT ( 'NONE',  ( 29.43706980810189222, 2.126176841940952134, -7.934999999999993392 ) ) ;
#114467 = LINE ( 'NONE', #112353, #104641 ) ;
#114468 = CARTESIAN_POINT ( 'NONE',  ( 22.49999999999984013, -1.592773361805351673, -6.492772025301281502 ) ) ;
#114469 = FACE_OUTER_BOUND ( 'NONE', #64264, .T. ) ;
#114470 = DIRECTION ( 'NONE',  ( -0.000000000000000000, -0.3543493200069152693, 0.9351131265310292928 ) ) ;
#114471 = ORIENTED_EDGE ( 'NONE', *, *, #123718, .F. ) ;
#114472 = VECTOR ( 'NONE', #85495, 1000.000000000000000 ) ;
#114473 = EDGE_LOOP ( 'NONE', ( #74651, #68593, #41664, #46214 ) ) ;
#114474 = CARTESIAN_POINT ( 'NONE',  ( 88.06249999999998579, -5.819803920172572198, -5.819803920172573086 ) ) ;
#114475 = ORIENTED_EDGE ( 'NONE', *, *, #15329, .F. ) ;
#114476 = VERTEX_POINT ( 'NONE', #19885 ) ;
#114477 = ADVANCED_FACE ( 'NONE', ( #66280 ), #32215, .F. ) ;
#114478 = CARTESIAN_POINT ( 'NONE',  ( 26.99999999999980105, -13.06887692260767331, 4.000000000000000000 ) ) ;
#114479 = CARTESIAN_POINT ( 'NONE',  ( 13.79752787990784668, 9.118485449599289083, -2.676246828001755507 ) ) ;
#114480 = VERTEX_POINT ( 'NONE', #64130 ) ;
#114481 = PLANE ( 'NONE',  #74090 ) ;
#114482 = CARTESIAN_POINT ( 'NONE',  ( -16.82816939922341248, -8.240707523384195099, 4.000000000000000000 ) ) ;
#114483 = LINE ( 'NONE', #15164, #53358 ) ;
#114484 = CARTESIAN_POINT ( 'NONE',  ( 126.7260406512308322, 5.298822016825037728, 4.147063925414387953 ) ) ;
#114485 = EDGE_CURVE ( 'NONE', #42223, #23228, #108296, .T. ) ;
#114486 = EDGE_CURVE ( 'NONE', #54110, #125050, #2299, .T. ) ;
#114487 = DIRECTION ( 'NONE',  ( -0.7071067811865487940, 0.7071067811865463515, -0.000000000000000000 ) ) ;
#114488 = FACE_OUTER_BOUND ( 'NONE', #141163, .T. ) ;
#114489 = PLANE ( 'NONE',  #125844 ) ;
#114490 = AXIS2_PLACEMENT_3D ( 'NONE', #143113, #111930, #12587 ) ;
#114491 = FACE_OUTER_BOUND ( 'NONE', #64656, .T. ) ;
#114492 = DIRECTION ( 'NONE',  ( 0.7071067811865486830, -0.7071067811865464625, -0.000000000000000000 ) ) ;
#114493 = DIRECTION ( 'NONE',  ( -1.000000000000000000, -0.000000000000000000, 0.000000000000000000 ) ) ;
#114494 = LINE ( 'NONE', #15173, #3579 ) ;
#114495 = CARTESIAN_POINT ( 'NONE',  ( 55.49226980201036952, -49.12413125935466240, 39.93743342457241141 ) ) ;
#114496 = EDGE_CURVE ( 'NONE', #9195, #41509, #88752, .T. ) ;
#114497 = ADVANCED_FACE ( 'NONE', ( #33662 ), #98872, .F. ) ;
#114498 = VECTOR ( 'NONE', #128423, 1000.000000000000000 ) ;
#114499 = ORIENTED_EDGE ( 'NONE', *, *, #16898, .T. ) ;
#114500 = ORIENTED_EDGE ( 'NONE', *, *, #35385, .F. ) ;
#114501 = CARTESIAN_POINT ( 'NONE',  ( 114.0420968585647898, 5.291415217122923842, -3.054999999999996163 ) ) ;
#114502 = EDGE_CURVE ( 'NONE', #19931, #15280, #136543, .T. ) ;
#114503 =( BOUNDED_CURVE ( )  B_SPLINE_CURVE ( 3, ( #67602, #123, #111793, #110328 ),
 .UNSPECIFIED., .F., .T. ) 
 B_SPLINE_CURVE_WITH_KNOTS ( ( 4, 4 ),
 ( 0.6873533248919956318, 0.6988790395524699939 ),
 .UNSPECIFIED. ) 
 CURVE ( )  GEOMETRIC_REPRESENTATION_ITEM ( )  RATIONAL_B_SPLINE_CURVE ( ( 1.000000000000000000, 0.9999889298557675943, 0.9999889298557675943, 1.000000000000000000 ) ) 
 REPRESENTATION_ITEM ( '' )  );
#114504 = ORIENTED_EDGE ( 'NONE', *, *, #63708, .T. ) ;
#114505 = VECTOR ( 'NONE', #142331, 1000.000000000000000 ) ;
#114506 = EDGE_CURVE ( 'NONE', #55578, #109227, #13998, .T. ) ;
#114507 = LINE ( 'NONE', #61600, #20074 ) ;
#114508 = EDGE_CURVE ( 'NONE', #31895, #11167, #26336, .T. ) ;
#114509 = DIRECTION ( 'NONE',  ( 0.7071067811865487940, 0.7071067811865463515, -0.000000000000000000 ) ) ;
#114510 = ORIENTED_EDGE ( 'NONE', *, *, #4630, .F. ) ;
#114511 = DIRECTION ( 'NONE',  ( 0.7071067811865487940, -0.7071067811865463515, 0.000000000000000000 ) ) ;
#114512 = CARTESIAN_POINT ( 'NONE',  ( -25.39999999999996305, 0.000000000000000000, 0.000000000000000000 ) ) ;
#114513 = ADVANCED_FACE ( 'NONE', ( #112624 ), #69139, .F. ) ;
#114514 = CARTESIAN_POINT ( 'NONE',  ( 108.7037635252314516, 6.109999999999998543, 1.122388791418548911E-15 ) ) ;
#114515 = AXIS2_PLACEMENT_3D ( 'NONE', #53294, #117119, #85930 ) ;
#114516 = VERTEX_POINT ( 'NONE', #134391 ) ;
#114517 = ORIENTED_EDGE ( 'NONE', *, *, #35661, .F. ) ;
#114518 = CARTESIAN_POINT ( 'NONE',  ( -4.499999999999957367, -4.912538124160707120, 4.000000000000000000 ) ) ;
#114519 = FACE_OUTER_BOUND ( 'NONE', #73029, .T. ) ;
#114520 = DIRECTION ( 'NONE',  ( -0.000000000000000000, 0.000000000000000000, 1.000000000000000000 ) ) ;
#114521 = EDGE_CURVE ( 'NONE', #31605, #72597, #58303, .T. ) ;
#114522 = EDGE_LOOP ( 'NONE', ( #126436, #78920, #125674, #44478 ) ) ;
#114523 = ORIENTED_EDGE ( 'NONE', *, *, #7270, .T. ) ;
#114524 = VERTEX_POINT ( 'NONE', #984 ) ;
#114525 = CARTESIAN_POINT ( 'NONE',  ( -69.18398860626899705, 28.73617430169835529, 5.000000000000000000 ) ) ;
#114526 = CARTESIAN_POINT ( 'NONE',  ( 0.2129031414352194063, 3.967499999999992699, -6.871911579029513994 ) ) ;
#114527 = EDGE_CURVE ( 'NONE', #87598, #96265, #111925, .T. ) ;
#114528 = COLOUR_RGB ( '', 0.40784314, 0.44705882, 0.49803922) ;
#114530 = MECHANICAL_DESIGN_GEOMETRIC_PRESENTATION_REPRESENTATION (  '', ( #47438 ), #24212 ) ;
#114529 =( LENGTH_UNIT ( ) NAMED_UNIT ( * ) SI_UNIT ( .MILLI., .METRE. ) );
#114531 = VECTOR ( 'NONE', #36872, 999.9999999999998863 ) ;
#114532 = CARTESIAN_POINT ( 'NONE',  ( 19.05000000000000071, 3.174999999999997158, 4.000000000000000000 ) ) ;
#114533 = EDGE_LOOP ( 'NONE', ( #106375, #32756, #61957 ) ) ;
#114535 = ORIENTED_EDGE ( 'NONE', *, *, #63406, .F. ) ;
#114534 = AXIS2_PLACEMENT_3D ( 'NONE', #1314, #70222, #12909 ) ;
#114536 = CARTESIAN_POINT ( 'NONE',  ( 2.816011393730999401, 28.73617430169785436, 5.000000000000000000 ) ) ;
#114537 = ORIENTED_EDGE ( 'NONE', *, *, #33496, .T. ) ;
#114538 = ORIENTED_EDGE ( 'NONE', *, *, #89328, .F. ) ;
#114539 = DIRECTION ( 'NONE',  ( -0.3543493200069162685, -0.000000000000000000, -0.9351131265310288487 ) ) ;
#114540 = EDGE_CURVE ( 'NONE', #29743, #9910, #56864, .T. ) ;
#114541 = CARTESIAN_POINT ( 'NONE',  ( -81.18398860626899705, 28.73617430169844056, 5.000000000000000000 ) ) ;
#114542 = ORIENTED_EDGE ( 'NONE', *, *, #105500, .T. ) ;
#114543 = DIRECTION ( 'NONE',  ( 0.6830127018922180770, -0.6830127018922204085, -0.2588190451025213501 ) ) ;
#114544 = EDGE_CURVE ( 'NONE', #30609, #82053, #35092, .T. ) ;
#114545 = FACE_OUTER_BOUND ( 'NONE', #28358, .T. ) ;
#114546 = DIRECTION ( 'NONE',  ( -0.7071067811865487940, 0.7071067811865463515, 0.000000000000000000 ) ) ;
#114547 = EDGE_CURVE ( 'NONE', #138330, #47703, #68446, .T. ) ;
#114548 = CARTESIAN_POINT ( 'NONE',  ( 21.29974487139158512, -27.71228299555221142, 4.000000000000000000 ) ) ;
#114549 = CARTESIAN_POINT ( 'NONE',  ( 48.29974487139158867, -27.71228299555239971, 4.000000000000000000 ) ) ;
#114550 = FACE_BOUND ( 'NONE', #120020, .T. ) ;
#114551 = ORIENTED_EDGE ( 'NONE', *, *, #39889, .F. ) ;
#114552 = DIRECTION ( 'NONE',  ( -1.000000000000000000, -1.224606353822377258E-16, -0.000000000000000000 ) ) ;
#114553 = CARTESIAN_POINT ( 'NONE',  ( -27.18398860626900060, 28.73617430169806042, 5.000000000000000000 ) ) ;
#114554 = DIRECTION ( 'NONE',  ( -0.7071067811865486830, -0.7071067811865464625, 0.000000000000000000 ) ) ;
#114555 = ORIENTED_EDGE ( 'NONE', *, *, #27205, .F. ) ;
#114556 = CARTESIAN_POINT ( 'NONE',  ( 4.585192374791373204, 22.22500000000000142, 19.97188885935846869 ) ) ;
#114557 = EDGE_LOOP ( 'NONE', ( #100249, #81715, #37902, #44724 ) ) ;
#114558 = ORIENTED_EDGE ( 'NONE', *, *, #41366, .T. ) ;
#114559 = ORIENTED_EDGE ( 'NONE', *, *, #27142, .F. ) ;
#114560 = CARTESIAN_POINT ( 'NONE',  ( 35.93293019189810877, 1.637169565754156508, 6.110000000000000320 ) ) ;
#114561 = ORIENTED_EDGE ( 'NONE', *, *, #42689, .F. ) ;
#114562 = LINE ( 'NONE', #15231, #15893 ) ;
#114563 = DIRECTION ( 'NONE',  ( -0.7071067811865486830, 0.7071067811865464625, 0.000000000000000000 ) ) ;
#114564 = DIRECTION ( 'NONE',  ( -0.7071067811865487940, 0.7071067811865463515, -0.000000000000000000 ) ) ;
#114565 = EDGE_CURVE ( 'NONE', #22070, #17208, #79333, .T. ) ;
#114566 = ORIENTED_EDGE ( 'NONE', *, *, #77569, .F. ) ;
#114567 = LINE ( 'NONE', #134945, #483 ) ;
#114568 = CARTESIAN_POINT ( 'NONE',  ( 34.49999999999975842, -7.535744391599426883, 4.994342998332164107 ) ) ;
#114569 = DIRECTION ( 'NONE',  ( 0.7071067811865487940, 0.7071067811865463515, 0.000000000000000000 ) ) ;
#114570 = LINE ( 'NONE', #5071, #141236 ) ;
#114572 = EDGE_CURVE ( 'NONE', #126032, #46388, #45268, .T. ) ;
#114571 = CARTESIAN_POINT ( 'NONE',  ( 0.000000000000000000, 0.000000000000000000, 5.000000000000000000 ) ) ;
#114573 = DIRECTION ( 'NONE',  ( 0.7071067811865486830, -0.7071067811865464625, -0.000000000000000000 ) ) ;
#114574 = VERTEX_POINT ( 'NONE', #113317 ) ;
#114575 = ORIENTED_EDGE ( 'NONE', *, *, #57272, .T. ) ;
#114576 = EDGE_LOOP ( 'NONE', ( #97003, #81855, #13269, #8591 ) ) ;
#114577 = VERTEX_POINT ( 'NONE', #1672 ) ;
#114578 = SURFACE_STYLE_FILL_AREA ( #26865 ) ;
#114579 = ORIENTED_EDGE ( 'NONE', *, *, #76128, .T. ) ;
#114580 = ORIENTED_EDGE ( 'NONE', *, *, #83682, .F. ) ;
#114581 = FACE_OUTER_BOUND ( 'NONE', #122761, .T. ) ;
#114582 = ADVANCED_FACE ( 'NONE', ( #133671 ), #34353, .T. ) ;
#114583 = DIRECTION ( 'NONE',  ( 0.7071067811865486830, -0.7071067811865464625, -0.000000000000000000 ) ) ;
#114584 = ORIENTED_EDGE ( 'NONE', *, *, #116326, .T. ) ;
#114585 = CARTESIAN_POINT ( 'NONE',  ( -12.69999999999998153, 0.000000000000000000, 0.000000000000000000 ) ) ;
#114586 = ORIENTED_EDGE ( 'NONE', *, *, #71671, .F. ) ;
#114587 = DIRECTION ( 'NONE',  ( -1.000000000000000000, -1.224606353822377258E-16, -0.000000000000000000 ) ) ;
#114588 = AXIS2_PLACEMENT_3D ( 'NONE', #84577, #116476, #38918 ) ;
#114589 = PLANE ( 'NONE',  #68230 ) ;
#114590 = SURFACE_SIDE_STYLE ('',( #105155 ) ) ;
#114591 = ORIENTED_EDGE ( 'NONE', *, *, #71247, .F. ) ;
#114593 = DIRECTION ( 'NONE',  ( 0.000000000000000000, -1.000000000000000000, 0.000000000000000000 ) ) ;
#114592 = CARTESIAN_POINT ( 'NONE',  ( 101.5579301918981088, 6.110000000000001208, -1.637169565754156286 ) ) ;
#114594 = VECTOR ( 'NONE', #112895, 1000.000000000000000 ) ;
#114595 = DIRECTION ( 'NONE',  ( 0.000000000000000000, -1.000000000000000000, 0.000000000000000000 ) ) ;
#114596 = ORIENTED_EDGE ( 'NONE', *, *, #38464, .T. ) ;
#114597 = ORIENTED_EDGE ( 'NONE', *, *, #106858, .T. ) ;
#114598 = CARTESIAN_POINT ( 'NONE',  ( 57.48921356237308800, -27.52281430457095368, 5.000000000000000000 ) ) ;
#114599 = ORIENTED_EDGE ( 'NONE', *, *, #116414, .T. ) ;
#114600 = CARTESIAN_POINT ( 'NONE',  ( -39.48921356237310221, -27.52281430457082934, 5.000000000000000000 ) ) ;
#114601 = CARTESIAN_POINT ( 'NONE',  ( 20.19999999999999929, 9.521314400968980422E-16, 0.000000000000000000 ) ) ;
#114602 = CARTESIAN_POINT ( 'NONE',  ( -12.69999999999998153, 0.000000000000000000, 2.500000000000000444 ) ) ;
#114603 = CARTESIAN_POINT ( 'NONE',  ( -32.99451991528749062, 28.92564299267960948, 4.000000000000000000 ) ) ;
#114605 = EDGE_CURVE ( 'NONE', #70432, #82515, #83266, .T. ) ;
#114604 = ORIENTED_EDGE ( 'NONE', *, *, #79035, .T. ) ;
#114606 = LINE ( 'NONE', #62406, #108458 ) ;
#114607 = ADVANCED_FACE ( 'NONE', ( #78576 ), #92276, .F. ) ;
#114608 = VECTOR ( 'NONE', #32648, 1000.000000000000000 ) ;
#114609 = VECTOR ( 'NONE', #52291, 1000.000000000000227 ) ;
#114610 = DIRECTION ( 'NONE',  ( -0.000000000000000000, -0.000000000000000000, 1.000000000000000000 ) ) ;
#114611 = LINE ( 'NONE', #126225, #7439 ) ;
#114612 = EDGE_LOOP ( 'NONE', ( #70152, #98708, #16876, #96264 ) ) ;
#114613 = DIRECTION ( 'NONE',  ( 0.000000000000000000, 1.000000000000000000, 0.000000000000000000 ) ) ;
#114614 = CARTESIAN_POINT ( 'NONE',  ( 19.82816939922337696, -17.24070752338412049, 4.000000000000000000 ) ) ;
#114615 = VERTEX_POINT ( 'NONE', #123533 ) ;
#114617 = ORIENTED_EDGE ( 'NONE', *, *, #2709, .F. ) ;
#114616 = DIRECTION ( 'NONE',  ( 0.7071067811865486830, 0.7071067811865463515, 0.000000000000000000 ) ) ;
#114618 = ADVANCED_FACE ( 'NONE', ( #37202 ), #24196, .F. ) ;
#114619 = VERTEX_POINT ( 'NONE', #80039 ) ;
#114620 = LINE ( 'NONE', #5122, #42643 ) ;
#114621 = PLANE ( 'NONE',  #131721 ) ;
#114622 = ORIENTED_EDGE ( 'NONE', *, *, #500, .F. ) ;
#114623 = DIRECTION ( 'NONE',  ( -0.7071067811865486830, -0.7071067811865464625, 0.000000000000000000 ) ) ;
#114624 = VECTOR ( 'NONE', #108580, 1000.000000000000000 ) ;
#114625 = CARTESIAN_POINT ( 'NONE',  ( -21.48921356237309155, -27.52281430457070499, 5.000000000000000000 ) ) ;
#114626 = VECTOR ( 'NONE', #85168, 1000.000000000000000 ) ;
#114627 = CIRCLE ( 'NONE', #133192, 2.500000000000000888 ) ;
#114628 = FACE_OUTER_BOUND ( 'NONE', #87759, .T. ) ;
#114629 = ORIENTED_EDGE ( 'NONE', *, *, #62325, .T. ) ;
#114630 = AXIS2_PLACEMENT_3D ( 'NONE', #125666, #67740, #70601 ) ;
#114631 = CARTESIAN_POINT ( 'NONE',  ( -5.563198967791673333, -12.74070752338415247, 9.898150129686387189 ) ) ;
#114632 = FACE_OUTER_BOUND ( 'NONE', #38320, .T. ) ;
#114633 = DIRECTION ( 'NONE',  ( -0.7071067811865487940, 0.7071067811865463515, 0.000000000000000000 ) ) ;
#114634 = DIRECTION ( 'NONE',  ( -0.000000000000000000, 0.000000000000000000, 1.000000000000000000 ) ) ;
#114635 = LINE ( 'NONE', #103745, #86437 ) ;
#114636 = CARTESIAN_POINT ( 'NONE',  ( 125.8183334000146374, -5.871789562033242760, 4.884347503592287865 ) ) ;
#114637 = CARTESIAN_POINT ( 'NONE',  ( 29.10002705046288085, 5.819803920172570422, 5.819803920172575751 ) ) ;
#114638 = DIRECTION ( 'NONE',  ( -0.6830127018922180770, -0.6830127018922204085, -0.2588190451025213501 ) ) ;
#114639 = ORIENTED_EDGE ( 'NONE', *, *, #6960, .T. ) ;
#114640 = VERTEX_POINT ( 'NONE', #124213 ) ;
#114641 = ORIENTED_EDGE ( 'NONE', *, *, #37987, .F. ) ;
#114642 = CARTESIAN_POINT ( 'NONE',  ( 121.7500000000000000, -9.735942053221458872E-16, 7.950000000000000178 ) ) ;
#114643 = ORIENTED_EDGE ( 'NONE', *, *, #89746, .F. ) ;
#114644 = ORIENTED_EDGE ( 'NONE', *, *, #91186, .T. ) ;
#114645 = ORIENTED_EDGE ( 'NONE', *, *, #1487, .T. ) ;
#114646 = CARTESIAN_POINT ( 'NONE',  ( -16.21498419724179740, -3.740707523384238176, 15.76143240460120154 ) ) ;
#114647 = CARTESIAN_POINT ( 'NONE',  ( -32.99999999999977263, 12.25461709320617842, -10.07315571508704544 ) ) ;
#114648 = ORIENTED_EDGE ( 'NONE', *, *, #103325, .F. ) ;
#114649 = DIRECTION ( 'NONE',  ( 1.000000000000000000, -0.000000000000000000, -0.000000000000000000 ) ) ;
#114650 = CARTESIAN_POINT ( 'NONE',  ( -11.99451991528749417, 28.92564299267946382, 4.000000000000000000 ) ) ;
#114651 = CARTESIAN_POINT ( 'NONE',  ( 8.811592354503320124, 9.902892378096218942E-16, 0.000000000000000000 ) ) ;
#114652 = CARTESIAN_POINT ( 'NONE',  ( 112.7295968585647756, -6.110000000000000320, -1.637169565754161393 ) ) ;
#114653 = VERTEX_POINT ( 'NONE', #124923 ) ;
#114654 = EDGE_CURVE ( 'NONE', #101750, #112039, #114046, .T. ) ;
#114655 = FACE_OUTER_BOUND ( 'NONE', #135845, .T. ) ;
#114656 = CARTESIAN_POINT ( 'NONE',  ( 105.5166937171295558, 7.950000000000000178, -2.130196079827421318 ) ) ;
#114657 = CARTESIAN_POINT ( 'NONE',  ( 10.35824297541133099, 15.75929247661555088, 19.34181609438697080 ) ) ;
#114658 = CARTESIAN_POINT ( 'NONE',  ( 83.49586038379622721, -3.974999999999998312, -6.884901960086286188 ) ) ;
#114659 = DIRECTION ( 'NONE',  ( 0.7071067811865487940, 0.7071067811865463515, 0.000000000000000000 ) ) ;
#114660 = LINE ( 'NONE', #69056, #95521 ) ;
#114661 = LINE ( 'NONE', #113967, #112947 ) ;
#114662 = CARTESIAN_POINT ( 'NONE',  ( 39.16252705046288440, 7.949999999999998401, 1.460391307983218338E-15 ) ) ;
#114663 = CARTESIAN_POINT ( 'NONE',  ( -28.49999999999980460, 13.56627193232212392, -10.57019076586074924 ) ) ;
#114664 = ADVANCED_FACE ( 'NONE', ( #128507 ), #29176, .F. ) ;
#114665 = CYLINDRICAL_SURFACE ( 'NONE', #27710, 1.000000000000000000 ) ;
#114666 = VERTEX_POINT ( 'NONE', #127053 ) ;
#114667 = ORIENTED_EDGE ( 'NONE', *, *, #64639, .F. ) ;
#114668 = CARTESIAN_POINT ( 'NONE',  ( 34.68749999999999289, -5.819803920172573086, 5.819803920172572198 ) ) ;
#114669 = EDGE_CURVE ( 'NONE', #45045, #116840, #16884, .T. ) ;
#114670 = EDGE_LOOP ( 'NONE', ( #72073, #62947, #118933, #98344 ) ) ;
#114671 = EDGE_LOOP ( 'NONE', ( #102368, #93495, #72874, #40908 ) ) ;
#114672 = DIRECTION ( 'NONE',  ( 0.7071067811865487940, -0.7071067811865463515, 0.000000000000000000 ) ) ;
#114673 = ADVANCED_FACE ( 'NONE', ( #60413 ), #29875, .F. ) ;
#114674 = PLANE ( 'NONE',  #68764 ) ;
#114675 = EDGE_LOOP ( 'NONE', ( #25057, #68297, #67350, #31184 ) ) ;
#114676 = EDGE_CURVE ( 'NONE', #118592, #67057, #103851, .T. ) ;
#114677 = CYLINDRICAL_SURFACE ( 'NONE', #41065, 7.950000000000000178 ) ;
#114678 = LINE ( 'NONE', #15346, #28421 ) ;
#114679 = CARTESIAN_POINT ( 'NONE',  ( 2.816011393730999401, 28.73617430169785436, 5.000000000000000000 ) ) ;
#114680 = CARTESIAN_POINT ( 'NONE',  ( 26.54209685856477563, 5.291415217122923842, -3.054999999999996163 ) ) ;
#114682 = EDGE_CURVE ( 'NONE', #46293, #84665, #82867, .T. ) ;
#114681 = ORIENTED_EDGE ( 'NONE', *, *, #112697, .T. ) ;
#114683 = DIRECTION ( 'NONE',  ( -0.7071067811865486830, -0.7071067811865464625, 0.000000000000000000 ) ) ;
#114684 = VERTEX_POINT ( 'NONE', #118309 ) ;
#114685 = FACE_OUTER_BOUND ( 'NONE', #136260, .T. ) ;
#114686 = LINE ( 'NONE', #137190, #117106 ) ;
#114687 = EDGE_CURVE ( 'NONE', #92319, #15951, #5961, .T. ) ;
#114688 = LINE ( 'NONE', #95083, #134423 ) ;
#114689 = ORIENTED_EDGE ( 'NONE', *, *, #114431, .T. ) ;
#114690 = ADVANCED_FACE ( 'NONE', ( #72746 ), #62541, .F. ) ;
#114691 = EDGE_LOOP ( 'NONE', ( #81306, #106428, #101278, #36881 ) ) ;
#114692 = DIRECTION ( 'NONE',  ( -0.6830127018922180770, -0.6830127018922204085, -0.2588190451025213501 ) ) ;
#114693 = CARTESIAN_POINT ( 'NONE',  ( 5.483345613589513334, 22.22500000000000142, 4.500000000000000888 ) ) ;
#114694 = DIRECTION ( 'NONE',  ( -0.6830127018922181881, 0.6830127018922202975, -0.2588190451025214056 ) ) ;
#114695 = ADVANCED_FACE ( 'NONE', ( #61834 ), #115429, .F. ) ;
#114696 = VECTOR ( 'NONE', #132202, 1000.000000000000000 ) ;
#114697 = CARTESIAN_POINT ( 'NONE',  ( 52.41209685856478018, 5.291415217122921177, -3.054999999999994831 ) ) ;
#114698 = VECTOR ( 'NONE', #138802, 1000.000000000000000 ) ;
#114699 = LINE ( 'NONE', #127005, #136841 ) ;
#114700 = CARTESIAN_POINT ( 'NONE',  ( -1.828169399223516400, 6.759292476615651246, 4.000000000000000000 ) ) ;
#114701 = ORIENTED_EDGE ( 'NONE', *, *, #24105, .T. ) ;
#114702 = ORIENTED_EDGE ( 'NONE', *, *, #136119, .T. ) ;
#114703 = CARTESIAN_POINT ( 'NONE',  ( -4.499999999999962697, 13.46639925780213076, 5.000000000000000000 ) ) ;
#114704 = EDGE_LOOP ( 'NONE', ( #22313, #68095, #104942, #134050 ) ) ;
#114705 = VECTOR ( 'NONE', #75813, 1000.000000000000000 ) ;
#114706 = CARTESIAN_POINT ( 'NONE',  ( 59.43336038379622011, 2.130196079827431532, -7.949999999999996625 ) ) ;
#114707 = ORIENTED_EDGE ( 'NONE', *, *, #30388, .F. ) ;
#114708 = LINE ( 'NONE', #6626, #122360 ) ;
#114709 = ADVANCED_FACE ( 'NONE', ( #106711 ), #105305, .F. ) ;
#114710 = CARTESIAN_POINT ( 'NONE',  ( -10.49999999999992539, 19.08746187583905751, 4.000000000000000000 ) ) ;
#114711 = FACE_BOUND ( 'NONE', #32342, .T. ) ;
#114712 = CARTESIAN_POINT ( 'NONE',  ( 45.18398860626900415, 28.73617430169818832, 5.000000000000000000 ) ) ;
#114713 = CARTESIAN_POINT ( 'NONE',  ( -11.15466569459995583, 22.22500000000000142, 14.00746825007390406 ) ) ;
#114714 = CARTESIAN_POINT ( 'NONE',  ( -1.180000000000000604, 10.00000000000000178, 6.750000000000000888 ) ) ;
#114715 = LINE ( 'NONE', #135785, #129120 ) ;
#114717 = VERTEX_POINT ( 'NONE', #50946 ) ;
#114716 = LINE ( 'NONE', #137935, #36587 ) ;
#114718 = DIRECTION ( 'NONE',  ( 0.7071067811865486830, -0.7071067811865464625, -0.000000000000000000 ) ) ;
#114719 = ADVANCED_FACE ( 'NONE', ( #138674 ), #113462, .T. ) ;
#114720 = AXIS2_PLACEMENT_3D ( 'NONE', #64246, #29453, #85258 ) ;
#114721 = ORIENTED_EDGE ( 'NONE', *, *, #78554, .T. ) ;
#114723 = ORIENTED_EDGE ( 'NONE', *, *, #91229, .T. ) ;
#114722 = VECTOR ( 'NONE', #82599, 1000.000000000000000 ) ;
#114724 = CARTESIAN_POINT ( 'NONE',  ( 64.37043019189810877, -3.055000000000001492, 5.291415217122917625 ) ) ;
#114725 = ORIENTED_EDGE ( 'NONE', *, *, #35653, .T. ) ;
#114726 = VECTOR ( 'NONE', #59359, 1000.000000000000000 ) ;
#114727 = LINE ( 'NONE', #80720, #113806 ) ;
#114728 = FACE_OUTER_BOUND ( 'NONE', #39659, .T. ) ;
#114729 = EDGE_CURVE ( 'NONE', #137509, #103304, #51661, .T. ) ;
#114730 = VERTEX_POINT ( 'NONE', #21153 ) ;
#114731 = CARTESIAN_POINT ( 'NONE',  ( -24.09843580608222169, 11.25929247661560240, 10.79108189686401431 ) ) ;
#114732 = VECTOR ( 'NONE', #117129, 1000.000000000000000 ) ;
#114733 = FACE_OUTER_BOUND ( 'NONE', #105111, .T. ) ;
#114734 = EDGE_CURVE ( 'NONE', #86215, #26526, #87841, .T. ) ;
#114735 = CARTESIAN_POINT ( 'NONE',  ( 101.1874999999999858, -5.819803920172573974, 5.819803920172573086 ) ) ;
#114736 = CARTESIAN_POINT ( 'NONE',  ( -25.88982677111770414, -22.22500000000000142, 4.785647885939355639 ) ) ;
#114737 = CARTESIAN_POINT ( 'NONE',  ( -0.4892135623730947680, -27.52281430457055578, 5.000000000000000000 ) ) ;
#114738 = CARTESIAN_POINT ( 'NONE',  ( -36.18398860626899705, 28.73617430169812437, 5.000000000000000000 ) ) ;
#114739 = EDGE_LOOP ( 'NONE', ( #97647, #81588, #113852, #76091, #131153 ) ) ;
#114740 = ORIENTED_EDGE ( 'NONE', *, *, #112108, .T. ) ;
#114741 = CARTESIAN_POINT ( 'NONE',  ( -17.99451991528748351, 28.92564299267950645, 4.000000000000000000 ) ) ;
#114742 = CARTESIAN_POINT ( 'NONE',  ( 48.18398860626899705, 28.73617430169820608, 5.000000000000000000 ) ) ;
#114743 = ORIENTED_EDGE ( 'NONE', *, *, #54752, .T. ) ;
#114744 = EDGE_LOOP ( 'NONE', ( #90036, #142060, #68876, #142877 ) ) ;
#114745 = VERTEX_POINT ( 'NONE', #64669 ) ;
#114746 = CARTESIAN_POINT ( 'NONE',  ( 30.31249999999999289, 5.819803920172571310, 5.819803920172576639 ) ) ;
#114747 = EDGE_LOOP ( 'NONE', ( #13665, #111177, #136316, #110480 ) ) ;
#114748 = CARTESIAN_POINT ( 'NONE',  ( 0.000000000000000000, 0.000000000000000000, 4.749999999999997335 ) ) ;
#114749 = CARTESIAN_POINT ( 'NONE',  ( 41.93336038379621300, 2.130196079827431532, -7.949999999999996625 ) ) ;
#114750 = CARTESIAN_POINT ( 'NONE',  ( 9.400403141435219823, -7.934999999999989839, 2.126176841940957907 ) ) ;
#114751 = CARTESIAN_POINT ( 'NONE',  ( 34.92499999999998295, -0.1833456135895417671, 4.500000000000000888 ) ) ;
#114752 = ORIENTED_EDGE ( 'NONE', *, *, #35708, .F. ) ;
#114753 = DIRECTION ( 'NONE',  ( 0.7071067811865486830, -0.7071067811865464625, -0.000000000000000000 ) ) ;
#114754 = CARTESIAN_POINT ( 'NONE',  ( 120.3916937171301953, 2.130196079819464128, 7.950000000004595613 ) ) ;
#114755 = DIRECTION ( 'NONE',  ( -0.000000000000000000, 0.3543493200069153248, 0.9351131265310292928 ) ) ;
#114757 = ORIENTED_EDGE ( 'NONE', *, *, #92244, .T. ) ;
#114756 = DIRECTION ( 'NONE',  ( -1.000000000000000000, -1.224606353822377258E-16, -0.000000000000000000 ) ) ;
#114758 = DIRECTION ( 'NONE',  ( 0.6830127018922181881, 0.6830127018922202975, -0.2588190451025214056 ) ) ;
#114759 = ORIENTED_EDGE ( 'NONE', *, *, #80746, .F. ) ;
#114760 = PLANE ( 'NONE',  #75047 ) ;
#114761 = LINE ( 'NONE', #104626, #26121 ) ;
#114762 = EDGE_CURVE ( 'NONE', #130905, #92017, #10265, .T. ) ;
#114763 = DIRECTION ( 'NONE',  ( 1.000000000000000000, 0.000000000000000000, 0.000000000000000000 ) ) ;
#114764 = EDGE_LOOP ( 'NONE', ( #23852, #11229, #49378, #110054 ) ) ;
#114765 = DIRECTION ( 'NONE',  ( 0.7071067811865487940, 0.7071067811865463515, -0.000000000000000000 ) ) ;
#114766 = FACE_OUTER_BOUND ( 'NONE', #34361, .T. ) ;
#114767 = ADVANCED_FACE ( 'NONE', ( #65411 ), #75550, .F. ) ;
#114768 = CARTESIAN_POINT ( 'NONE',  ( 2.915086768062360889, -12.74070752338415602, 18.74364270924355225 ) ) ;
#114769 = DIRECTION ( 'NONE',  ( -1.000000000000000000, -1.224606353822377258E-16, -0.000000000000000000 ) ) ;
#114770 = DIRECTION ( 'NONE',  ( -0.6830127018922181881, 0.6830127018922202975, -0.2588190451025214056 ) ) ;
#114771 = ORIENTED_EDGE ( 'NONE', *, *, #126459, .T. ) ;
#114772 = LINE ( 'NONE', #35858, #92464 ) ;
#114773 = CARTESIAN_POINT ( 'NONE',  ( 28.49999999999980460, -12.08601207473286543, -10.46905243149100961 ) ) ;
#114774 =( BOUNDED_CURVE ( )  B_SPLINE_CURVE ( 3, ( #76712, #102003, #46965, #111439 ),
 .UNSPECIFIED., .F., .T. ) 
 B_SPLINE_CURVE_WITH_KNOTS ( ( 4, 4 ),
 ( 1.901594255663603183, 1.933014472006576945 ),
 .UNSPECIFIED. ) 
 CURVE ( )  GEOMETRIC_REPRESENTATION_ITEM ( )  RATIONAL_B_SPLINE_CURVE ( ( 1.000000000000000000, 0.9999177325257866400, 0.9999177325257866400, 1.000000000000000000 ) ) 
 REPRESENTATION_ITEM ( '' )  );
#114775 = CARTESIAN_POINT ( 'NONE',  ( 17.11162361894747619, 9.759292476615614831, 17.35367589129208810 ) ) ;
#114776 = DIRECTION ( 'NONE',  ( 0.7071067811865486830, -0.7071067811865464625, -0.000000000000000000 ) ) ;
#114777 = CARTESIAN_POINT ( 'NONE',  ( 71.99451991528749772, 28.92564299267988304, 4.000000000000000000 ) ) ;
#114778 = ORIENTED_EDGE ( 'NONE', *, *, #121883, .F. ) ;
#114779 = EDGE_CURVE ( 'NONE', #132371, #110801, #54525, .T. ) ;
#114780 = VERTEX_POINT ( 'NONE', #74860 ) ;
#114781 = PLANE ( 'NONE',  #61101 ) ;
#114782 = PRODUCT_DEFINITION ( 'UNKNOWN', '', #121211, #128474 ) ;
#114783 = CARTESIAN_POINT ( 'NONE',  ( 9.020403141435219041, 7.934999999999989839, -2.126176841940961904 ) ) ;
#114784 = AXIS2_PLACEMENT_3D ( 'NONE', #15626, #71497, #77325 ) ;
#114785 = CARTESIAN_POINT ( 'NONE',  ( 64.53752705046289861, -9.735942053221456900E-16, 7.949999999999998401 ) ) ;
#114786 = LINE ( 'NONE', #48863, #143380 ) ;
#114787 = DIRECTION ( 'NONE',  ( -0.6830127018922180770, -0.6830127018922204085, -0.2588190451025213501 ) ) ;
#114788 = FACE_OUTER_BOUND ( 'NONE', #134313, .T. ) ;
#114789 = AXIS2_PLACEMENT_3D ( 'NONE', #128282, #116675, #127559 ) ;
#114790 = VERTEX_POINT ( 'NONE', #77002 ) ;
#114791 = PLANE ( 'NONE',  #51621 ) ;
#114792 = CARTESIAN_POINT ( 'NONE',  ( -69.18398860626899705, 28.73617430169835529, 5.000000000000000000 ) ) ;
#114793 = CARTESIAN_POINT ( 'NONE',  ( 49.64126352523145158, 4.472830434245837594, 4.472830434245841147 ) ) ;
#114794 = EDGE_CURVE ( 'NONE', #74021, #99505, #30630, .T. ) ;
#114795 = CARTESIAN_POINT ( 'NONE',  ( -0.7586007421979610310, 21.72500000000000853, 5.000000000000000000 ) ) ;
#114796 = ORIENTED_EDGE ( 'NONE', *, *, #51613, .F. ) ;
#114797 = CARTESIAN_POINT ( 'NONE',  ( -34.42500000000001137, -0.02281430457058350458, 5.000000000000000000 ) ) ;
#114798 = ORIENTED_EDGE ( 'NONE', *, *, #97011, .T. ) ;
#114799 = VECTOR ( 'NONE', #142326, 999.9999999999998863 ) ;
#114800 = DIRECTION ( 'NONE',  ( -0.000000000000000000, 0.9647414015272155474, -0.2631995976047525887 ) ) ;
#114801 = VERTEX_POINT ( 'NONE', #109589 ) ;
#114802 = DIRECTION ( 'NONE',  ( -0.000000000000000000, -0.3543493200069152693, 0.9351131265310292928 ) ) ;
#114803 = CARTESIAN_POINT ( 'NONE',  ( 5.999999999999960920, -15.41253812416059787, 4.000000000000000000 ) ) ;
#114804 = LINE ( 'NONE', #62613, #83587 ) ;
#114805 = DIRECTION ( 'NONE',  ( 0.7071067811865486830, -0.7071067811865464625, -0.000000000000000000 ) ) ;
#114806 = CARTESIAN_POINT ( 'NONE',  ( -34.75611968250420603, -16.29434930147576921, 4.955485411084901592 ) ) ;
#114807 = CARTESIAN_POINT ( 'NONE',  ( 10.93750000000000178, -4.461849672132299105, 4.461849672132299993 ) ) ;
#114808 = ORIENTED_EDGE ( 'NONE', *, *, #60928, .F. ) ;
#114809 = DIRECTION ( 'NONE',  ( -0.6830127018922181881, 0.6830127018922202975, -0.2588190451025214056 ) ) ;
#114810 = PLANE ( 'NONE',  #137187 ) ;
#114811 = FACE_OUTER_BOUND ( 'NONE', #16332, .T. ) ;
#114812 = VECTOR ( 'NONE', #53940, 1000.000000000000000 ) ;
#114813 = FACE_OUTER_BOUND ( 'NONE', #63107, .T. ) ;
#114814 = CARTESIAN_POINT ( 'NONE',  ( 67.45419371712955581, 6.884901960086283523, 3.975000000000002753 ) ) ;
#114816 = EDGE_CURVE ( 'NONE', #39099, #6138, #21866, .T. ) ;
#114815 = VECTOR ( 'NONE', #31440, 1000.000000000000000 ) ;
#114817 = CYLINDRICAL_SURFACE ( 'NONE', #113285, 7.950000000000000178 ) ;
#114818 = ORIENTED_EDGE ( 'NONE', *, *, #33697, .F. ) ;
#114819 = VERTEX_POINT ( 'NONE', #119036 ) ;
#114820 = CARTESIAN_POINT ( 'NONE',  ( 66.91666666666667140, -6.884901960086287076, -3.975000000000000977 ) ) ;
#114821 = DIRECTION ( 'NONE',  ( -1.734723475976806848E-16, 1.000000000000000000, 0.000000000000000000 ) ) ;
#114822 = EDGE_CURVE ( 'NONE', #143096, #143231, #86434, .T. ) ;
#114823 = VECTOR ( 'NONE', #133425, 1000.000000000000000 ) ;
#114824 = LINE ( 'NONE', #139508, #43896 ) ;
#114825 = LINE ( 'NONE', #14099, #86814 ) ;
#114826 = ADVANCED_FACE ( 'NONE', ( #63280 ), #8110, .T. ) ;
#114827 = VECTOR ( 'NONE', #3549, 1000.000000000000227 ) ;
#114828 = EDGE_LOOP ( 'NONE', ( #143156, #138472, #98520, #59859 ) ) ;
#114829 = EDGE_CURVE ( 'NONE', #125405, #25399, #142936, .T. ) ;
#114830 = EDGE_CURVE ( 'NONE', #33874, #92295, #96539, .T. ) ;
#114831 = DIRECTION ( 'NONE',  ( -1.000000000000000000, -1.224606353822377258E-16, -0.000000000000000000 ) ) ;
#114832 = CARTESIAN_POINT ( 'NONE',  ( 16.27785539607886633, -2.500000000000000444, 3.061616997868384127E-16 ) ) ;
#114833 = CARTESIAN_POINT ( 'NONE',  ( 60.37543019189810423, -5.291415217122920289, -3.055000000000001492 ) ) ;
#114834 = DIRECTION ( 'NONE',  ( 0.6830127018922181881, 0.6830127018922202975, -0.2588190451025214056 ) ) ;
#114835 = ORIENTED_EDGE ( 'NONE', *, *, #87128, .F. ) ;
#114836 = ORIENTED_EDGE ( 'NONE', *, *, #44948, .F. ) ;
#114837 = LINE ( 'NONE', #12158, #123356 ) ;
#114838 = DIRECTION ( 'NONE',  ( 0.7071067811865487940, 0.7071067811865463515, 0.000000000000000000 ) ) ;
#114839 = CARTESIAN_POINT ( 'NONE',  ( 18.51665438641032324, 22.22500000000000142, 4.500000000000000888 ) ) ;
#114840 = ADVANCED_FACE ( 'NONE', ( #110281 ), #98013, .T. ) ;
#114841 = LINE ( 'NONE', #15519, #81132 ) ;
#114842 = EDGE_CURVE ( 'NONE', #30447, #82994, #32772, .T. ) ;
#114843 = CARTESIAN_POINT ( 'NONE',  ( 26.29289321881327623, -6.740707523384216415, 5.000000000000000000 ) ) ;
#114845 = ORIENTED_EDGE ( 'NONE', *, *, #125134, .F. ) ;
#114844 = CARTESIAN_POINT ( 'NONE',  ( 85.29166666666667140, 3.975000000000003642, -6.884901960086285300 ) ) ;
#114846 = DIRECTION ( 'NONE',  ( 0.7071067811865486830, -0.7071067811865464625, -0.000000000000000000 ) ) ;
#114847 = LINE ( 'NONE', #96652, #114812 ) ;
#114848 = DIRECTION ( 'NONE',  ( 0.6830127018922180770, -0.6830127018922204085, -0.2588190451025213501 ) ) ;
#114849 = LINE ( 'NONE', #59807, #27565 ) ;
#114850 = EDGE_CURVE ( 'NONE', #45393, #54270, #108132, .T. ) ;
#114851 = VERTEX_POINT ( 'NONE', #141516 ) ;
#114852 = ORIENTED_EDGE ( 'NONE', *, *, #19114, .T. ) ;
#114853 = CARTESIAN_POINT ( 'NONE',  ( 33.48921356237309510, -27.52281430457078670, 5.000000000000000000 ) ) ;
#114854 = LINE ( 'NONE', #39489, #44143 ) ;
#114855 = CARTESIAN_POINT ( 'NONE',  ( 124.3291937171295700, -3.975000000000001865, 6.884901960086284411 ) ) ;
#114856 = CYLINDRICAL_SURFACE ( 'NONE', #50182, 1.000000000000000888 ) ;
#114857 = ORIENTED_EDGE ( 'NONE', *, *, #94202, .T. ) ;
#114859 = EDGE_CURVE ( 'NONE', #86507, #118884, #97295, .T. ) ;
#114858 = ORIENTED_EDGE ( 'NONE', *, *, #105798, .T. ) ;
#114860 = CIRCLE ( 'NONE', #17593, 9.000000000000001776 ) ;
#114861 = LINE ( 'NONE', #48943, #19038 ) ;
#114862 = CARTESIAN_POINT ( 'NONE',  ( 30.18398860626900060, 28.73617430169808173, 5.000000000000000000 ) ) ;
#114863 = ORIENTED_EDGE ( 'NONE', *, *, #86707, .T. ) ;
#114864 = CARTESIAN_POINT ( 'NONE',  ( -21.28001967989390764, 0.7592924766157173044, 14.27032725228004040 ) ) ;
#114865 = ORIENTED_EDGE ( 'NONE', *, *, #57801, .F. ) ;
#114866 = FACE_OUTER_BOUND ( 'NONE', #52448, .T. ) ;
#114867 = ADVANCED_FACE ( 'NONE', ( #31332 ), #119723, .F. ) ;
#114869 = AXIS2_PLACEMENT_3D ( 'NONE', #103567, #70302, #59408 ) ;
#114868 = DIRECTION ( 'NONE',  ( -0.7071067811865486830, -0.7071067811865464625, 0.000000000000000000 ) ) ;
#114870 = FACE_BOUND ( 'NONE', #3577, .T. ) ;
#114871 = DIRECTION ( 'NONE',  ( -0.7071067811865487940, 0.7071067811865463515, 0.000000000000000000 ) ) ;
#114872 = LINE ( 'NONE', #17708, #18868 ) ;
#114873 = DIRECTION ( 'NONE',  ( 0.7071067811865487940, 0.7071067811865463515, 0.000000000000000000 ) ) ;
#114874 = FACE_OUTER_BOUND ( 'NONE', #65441, .T. ) ;
#114876 = EDGE_CURVE ( 'NONE', #7339, #32128, #120425, .T. ) ;
#114875 = APPLICATION_PROTOCOL_DEFINITION ( 'draft international standard', 'automotive_design', 1998, #50377 ) ;
#114878 = ORIENTED_EDGE ( 'NONE', *, *, #115859, .F. ) ;
#114877 = AXIS2_PLACEMENT_3D ( 'NONE', #64844, #75718, #65590 ) ;
#114879 = ORIENTED_EDGE ( 'NONE', *, *, #18951, .F. ) ;
#114880 = CARTESIAN_POINT ( 'NONE',  ( 93.82876352523145158, 0.000000000000000000, -6.109999999999998543 ) ) ;
#114881 = ORIENTED_EDGE ( 'NONE', *, *, #9300, .T. ) ;
#114882 = CIRCLE ( 'NONE', #117175, 2.500000000000000888 ) ;
#114883 = CARTESIAN_POINT ( 'NONE',  ( -18.79333936457834753, 21.75929247661549937, 4.998822639870701856 ) ) ;
#114884 = CARTESIAN_POINT ( 'NONE',  ( -36.18398860626899705, 28.73617430169812437, 5.000000000000000000 ) ) ;
#114885 = CARTESIAN_POINT ( 'NONE',  ( -0.1839886062690032631, 28.73617430169787568, 5.000000000000000000 ) ) ;
#114886 = ORIENTED_EDGE ( 'NONE', *, *, #83980, .F. ) ;
#114887 = CARTESIAN_POINT ( 'NONE',  ( -6.328169399223480873, -18.74070752338408852, 4.000000000000000000 ) ) ;
#114888 = DIRECTION ( 'NONE',  ( -1.000000000000000000, -0.000000000000000000, -0.000000000000000000 ) ) ;
#114889 = MECHANICAL_DESIGN_GEOMETRIC_PRESENTATION_REPRESENTATION (  '', ( #29240 ), #112655 ) ;
#114890 = ADVANCED_FACE ( 'NONE', ( #93373 ), #137608, .F. ) ;
#114891 = LINE ( 'NONE', #38804, #108248 ) ;
#114893 = CARTESIAN_POINT ( 'NONE',  ( -11.99999999999991118, -6.412538124160689357, 4.000000000000000000 ) ) ;
#114892 = CARTESIAN_POINT ( 'NONE',  ( -33.29974487139158867, -27.71228299555229313, 4.000000000000000000 ) ) ;
#114894 = DIRECTION ( 'NONE',  ( -0.3543493200069162685, -0.000000000000000000, -0.9351131265310288487 ) ) ;
#114895 = CARTESIAN_POINT ( 'NONE',  ( -14.99999999999989875, 8.966399257802175171, 5.000000000000000000 ) ) ;
#114896 = ORIENTED_EDGE ( 'NONE', *, *, #39040, .T. ) ;
#114897 = DIRECTION ( 'NONE',  ( -0.7071067811865487940, 0.7071067811865463515, -0.000000000000000000 ) ) ;
#114898 = LINE ( 'NONE', #26507, #58150 ) ;
#114899 = ORIENTED_EDGE ( 'NONE', *, *, #95781, .T. ) ;
#114901 = ORIENTED_EDGE ( 'NONE', *, *, #140086, .F. ) ;
#114900 = AXIS2_PLACEMENT_3D ( 'NONE', #27321, #71572, #115732 ) ;
#114902 = EDGE_CURVE ( 'NONE', #106219, #12022, #38289, .T. ) ;
#114903 = VERTEX_POINT ( 'NONE', #808 ) ;
#114904 = CARTESIAN_POINT ( 'NONE',  ( 42.29209685856477563, -5.291415217122921177, 3.054999999999999272 ) ) ;
#114905 = ORIENTED_EDGE ( 'NONE', *, *, #95829, .T. ) ;
#114906 = VECTOR ( 'NONE', #112843, 1000.000000000000000 ) ;
#114907 = CARTESIAN_POINT ( 'NONE',  ( 13.89997294953710494, 4.461849672132297329, -4.461849672132302658 ) ) ;
#114908 = CARTESIAN_POINT ( 'NONE',  ( -15.02522766578277746, 7.701385942161060427, -28.15899997092440898 ) ) ;
#114909 = ORIENTED_EDGE ( 'NONE', *, *, #70080, .F. ) ;
#114910 = FACE_OUTER_BOUND ( 'NONE', #85548, .T. ) ;
#114911 = ORIENTED_EDGE ( 'NONE', *, *, #110419, .T. ) ;
#114912 = DIRECTION ( 'NONE',  ( 0.6830127018922180770, -0.6830127018922204085, -0.2588190451025213501 ) ) ;
#114913 = VECTOR ( 'NONE', #68694, 1000.000000000000000 ) ;
#114914 = DIRECTION ( 'NONE',  ( -0.7071067811865486830, -0.7071067811865464625, 0.000000000000000000 ) ) ;
#114916 = VERTEX_POINT ( 'NONE', #138311 ) ;
#114915 = LINE ( 'NONE', #46168, #35508 ) ;
#114917 = ORIENTED_EDGE ( 'NONE', *, *, #55217, .T. ) ;
#114918 = DIRECTION ( 'NONE',  ( -1.000000000000000000, -1.224606353822377258E-16, -0.000000000000000000 ) ) ;
#114919 = CARTESIAN_POINT ( 'NONE',  ( -34.92500000000001137, -12.03857301832753102, 17.98374865626354335 ) ) ;
#114920 = ORIENTED_EDGE ( 'NONE', *, *, #88611, .F. ) ;
#114921 = CARTESIAN_POINT ( 'NONE',  ( -25.82816939922335209, -5.240707523384228850, 4.000000000000000000 ) ) ;
#114922 = ORIENTED_EDGE ( 'NONE', *, *, #97188, .F. ) ;
#114924 = VERTEX_POINT ( 'NONE', #36156 ) ;
#114923 = EDGE_CURVE ( 'NONE', #62444, #139660, #82505, .T. ) ;
#114925 = ORIENTED_EDGE ( 'NONE', *, *, #116184, .F. ) ;
#114926 = ORIENTED_EDGE ( 'NONE', *, *, #124486, .T. ) ;
#114927 = DIRECTION ( 'NONE',  ( 0.3543493200069162685, -0.000000000000000000, -0.9351131265310288487 ) ) ;
#114928 = CARTESIAN_POINT ( 'NONE',  ( 23.99999999999982947, 20.70535890316563155, 1.956823837851859871 ) ) ;
#114929 = EDGE_CURVE ( 'NONE', #6269, #7326, #134401, .T. ) ;
#114930 = CARTESIAN_POINT ( 'NONE',  ( 27.99999999999999645, -49.14999999999999147, -53.92499999999967741 ) ) ;
#114931 = ADVANCED_FACE ( 'NONE', ( #27378 ), #6945, .T. ) ;
#114932 = FACE_OUTER_BOUND ( 'NONE', #105799, .T. ) ;
#114933 = VERTEX_POINT ( 'NONE', #58669 ) ;
#114934 = CARTESIAN_POINT ( 'NONE',  ( -25.59167451900982826, -0.7407075233842735917, 14.76736230305374775 ) ) ;
#114935 = CARTESIAN_POINT ( 'NONE',  ( 24.62456980810188867, -6.871911579029512218, 3.967499999999996252 ) ) ;
#114936 = CARTESIAN_POINT ( 'NONE',  ( 0.000000000000000000, 0.000000000000000000, 5.000000000000000000 ) ) ;
#114937 = AXIS2_PLACEMENT_3D ( 'NONE', #18095, #129749, #129032 ) ;
#114938 = CARTESIAN_POINT ( 'NONE',  ( 31.49999999999977973, -10.04351517176475106, -1.623559851933751075 ) ) ;
#114939 = ADVANCED_FACE ( 'NONE', ( #59353, #102840, #66809 ), #26692, .T. ) ;
#114940 = DIRECTION ( 'NONE',  ( 1.000000000000000000, 0.000000000000000000, 0.000000000000000000 ) ) ;
#114941 = EDGE_LOOP ( 'NONE', ( #109, #47425, #29017, #21723 ) ) ;
#114942 = ORIENTED_EDGE ( 'NONE', *, *, #99601, .T. ) ;
#114943 = ORIENTED_EDGE ( 'NONE', *, *, #20091, .T. ) ;
#114944 = CARTESIAN_POINT ( 'NONE',  ( 3.250000000000000000, 0.000000000000000000, 0.000000000000000000 ) ) ;
#114945 = DIRECTION ( 'NONE',  ( 0.7071067811865487940, 0.7071067811865463515, 0.000000000000000000 ) ) ;
#114946 = DIRECTION ( 'NONE',  ( 0.7071067811865486830, -0.7071067811865464625, -0.000000000000000000 ) ) ;
#114947 = AXIS2_PLACEMENT_3D ( 'NONE', #142869, #8728, #63206 ) ;
#114948 = CARTESIAN_POINT ( 'NONE',  ( 1.828169399223523284, 3.759292476615681888, 4.000000000000000000 ) ) ;
#114949 = DIRECTION ( 'NONE',  ( -0.000000000000000000, -0.3543493200069152693, 0.9351131265310292928 ) ) ;
#114950 = CARTESIAN_POINT ( 'NONE',  ( 70.93293019189810877, 1.637169565754156730, 6.110000000000001208 ) ) ;
#114951 = EDGE_CURVE ( 'NONE', #99187, #75880, #113696, .T. ) ;
#114952 = CARTESIAN_POINT ( 'NONE',  ( 12.19999999999999574, -21.76999999999999247, 0.000000000000000000 ) ) ;
#114953 = DIRECTION ( 'NONE',  ( -1.000000000000000000, -0.000000000000000000, -0.000000000000000000 ) ) ;
#114954 = CARTESIAN_POINT ( 'NONE',  ( -6.183988606268994381, 28.73617430169791476, 5.000000000000000000 ) ) ;
#114955 = LINE ( 'NONE', #47647, #62890 ) ;
#114956 = PLANE ( 'NONE',  #81233 ) ;
#114957 = AXIS2_PLACEMENT_3D ( 'NONE', #21780, #97917, #130557 ) ;
#114958 = ORIENTED_EDGE ( 'NONE', *, *, #24623, .T. ) ;
#114959 = CARTESIAN_POINT ( 'NONE',  ( 8.999999999999937828, -5.527737879153182377, -7.983877177622392907 ) ) ;
#114960 = EDGE_LOOP ( 'NONE', ( #3264, #91121, #136853, #45899 ) ) ;
#114961 = LINE ( 'NONE', #38179, #27502 ) ;
#114963 = VERTEX_POINT ( 'NONE', #125295 ) ;
#114962 = CARTESIAN_POINT ( 'NONE',  ( 34.92499999999998295, 22.22500000000000142, 4.500000000000000888 ) ) ;
#114964 = AXIS2_PLACEMENT_3D ( 'NONE', #23060, #52841, #98512 ) ;
#114965 = CARTESIAN_POINT ( 'NONE',  ( -24.18398860626899705, 28.73617430169804265, 5.000000000000000000 ) ) ;
#114966 = CARTESIAN_POINT ( 'NONE',  ( 24.70710678118637560, -3.740707523384243505, 5.000000000000000000 ) ) ;
#114967 = ORIENTED_EDGE ( 'NONE', *, *, #121273, .T. ) ;
#114968 = DIRECTION ( 'NONE',  ( -0.000000000000000000, 0.000000000000000000, 1.000000000000000000 ) ) ;
#114969 = ORIENTED_EDGE ( 'NONE', *, *, #2589, .F. ) ;
#114970 = CARTESIAN_POINT ( 'NONE',  ( 65.99451991528749772, 28.92564299267984396, 4.000000000000000000 ) ) ;
#114971 = ORIENTED_EDGE ( 'NONE', *, *, #16310, .T. ) ;
#114972 = PLANE ( 'NONE',  #103137 ) ;
#114973 = AXIS2_PLACEMENT_3D ( 'NONE', #59008, #3803, #127049 ) ;
#114974 = EDGE_CURVE ( 'NONE', #6620, #122713, #70248, .T. ) ;
#114975 = CARTESIAN_POINT ( 'NONE',  ( 102.1625270504628844, 7.949999999999998401, 1.460391307983218338E-15 ) ) ;
#114976 = DIRECTION ( 'NONE',  ( 0.6830127018922180770, -0.6830127018922204085, -0.2588190451025213501 ) ) ;
#114977 = EDGE_CURVE ( 'NONE', #1511, #37150, #60052, .T. ) ;
#114978 = CARTESIAN_POINT ( 'NONE',  ( -80.99451991528748351, 28.92564299267994699, 4.000000000000000000 ) ) ;
#114979 = ORIENTED_EDGE ( 'NONE', *, *, #126495, .F. ) ;
#114980 = VECTOR ( 'NONE', #35239, 1000.000000000000000 ) ;
#114981 = CARTESIAN_POINT ( 'NONE',  ( 34.75611968250419892, -18.18706574529242204, 4.955485411084882941 ) ) ;
#114983 = ADVANCED_FACE ( 'NONE', ( #92638 ), #37584, .F. ) ;
#114982 = CARTESIAN_POINT ( 'NONE',  ( -20.24139925780189841, 21.72500000000000853, 5.000000000000000000 ) ) ;
#114984 = DIRECTION ( 'NONE',  ( -0.7071067811865487940, 0.7071067811865463515, 0.000000000000000000 ) ) ;
#114985 = VECTOR ( 'NONE', #76348, 1000.000000000000227 ) ;
#114986 = CARTESIAN_POINT ( 'NONE',  ( 26.83333333333333570, 5.278424836066143655, -3.047499999999997655 ) ) ;
#114987 = FACE_OUTER_BOUND ( 'NONE', #106465, .T. ) ;
#114988 = LINE ( 'NONE', #47678, #63040 ) ;
#114989 = ORIENTED_EDGE ( 'NONE', *, *, #61392, .F. ) ;
#114990 = ADVANCED_FACE ( 'NONE', ( #29523 ), #129556, .F. ) ;
#114991 = EDGE_CURVE ( 'NONE', #70329, #29685, #74502, .T. ) ;
#114992 = DIRECTION ( 'NONE',  ( -0.000000000000000000, -0.3543493200069152693, 0.9351131265310292928 ) ) ;
#114993 = EDGE_LOOP ( 'NONE', ( #41938, #109046, #3694, #86448 ) ) ;
#114994 = CARTESIAN_POINT ( 'NONE',  ( 83.12543019189810423, 5.291415217122919401, 3.055000000000002824 ) ) ;
#114995 = DIRECTION ( 'NONE',  ( -0.7071067811865487940, 0.7071067811865463515, 0.000000000000000000 ) ) ;
#114996 = CARTESIAN_POINT ( 'NONE',  ( -14.99451991528749595, 28.92564299267948513, 4.000000000000000000 ) ) ;
#114997 = DIRECTION ( 'NONE',  ( 0.7071067811865486830, -0.7071067811865464625, -0.000000000000000000 ) ) ;
#114998 = ORIENTED_EDGE ( 'NONE', *, *, #132246, .F. ) ;
#114999 = LINE ( 'NONE', #15678, #134558 ) ;
#115000 = DIRECTION ( 'NONE',  ( -1.000000000000000000, -1.224606353822377258E-16, -0.000000000000000000 ) ) ;
#115001 = VECTOR ( 'NONE', #84091, 1000.000000000000227 ) ;
#115002 = ADVANCED_FACE ( 'NONE', ( #139028 ), #39734, .F. ) ;
#115003 = CARTESIAN_POINT ( 'NONE',  ( 117.4750270504628844, -5.819803920172573086, 5.819803920172573086 ) ) ;
#115004 = EDGE_CURVE ( 'NONE', #28808, #83728, #85331, .T. ) ;
#115005 = CARTESIAN_POINT ( 'NONE',  ( 3.183988606268992161, 28.73617430169789699, 5.000000000000000000 ) ) ;
#115007 = ORIENTED_EDGE ( 'NONE', *, *, #4280, .T. ) ;
#115006 = LINE ( 'NONE', #114330, #116884 ) ;
#115008 = CARTESIAN_POINT ( 'NONE',  ( 54.29974487139159578, -27.71228299555243879, 4.000000000000000000 ) ) ;
#115009 = CARTESIAN_POINT ( 'NONE',  ( -5.999999999999963585, 20.96639925780204905, 5.000000000000000000 ) ) ;
#115010 = CARTESIAN_POINT ( 'NONE',  ( 1.809685201411095568, -5.249926533735820300, 3.476758287636498412 ) ) ;
#115011 = AXIS2_PLACEMENT_3D ( 'NONE', #9485, #58618, #54478 ) ;
#115012 = CARTESIAN_POINT ( 'NONE',  ( -25.39999999999996305, 0.000000000000000000, 0.000000000000000000 ) ) ;
#115013 = VECTOR ( 'NONE', #98665, 1000.000000000000000 ) ;
#115014 = VERTEX_POINT ( 'NONE', #83961 ) ;
#115015 = ORIENTED_EDGE ( 'NONE', *, *, #88668, .F. ) ;
#115016 = ORIENTED_EDGE ( 'NONE', *, *, #63323, .F. ) ;
#115017 = AXIS2_PLACEMENT_3D ( 'NONE', #126606, #27297, #64773 ) ;
#115018 = CARTESIAN_POINT ( 'NONE',  ( 80.93793019189807580, -6.110000000000001208, 1.637169565754158951 ) ) ;
#115019 = ORIENTED_EDGE ( 'NONE', *, *, #28839, .F. ) ;
#115020 = EDGE_CURVE ( 'NONE', #22078, #112797, #72385, .T. ) ;
#115021 = FACE_OUTER_BOUND ( 'NONE', #126281, .T. ) ;
#115022 = CIRCLE ( 'NONE', #138248, 5.968999999999998529 ) ;
#115023 = LINE ( 'NONE', #58604, #142930 ) ;
#115025 = STYLED_ITEM ( 'NONE', ( #45200 ), #134888 ) ;
#115024 = CARTESIAN_POINT ( 'NONE',  ( 21.29974487139158512, -27.71228299555221142, 4.000000000000000000 ) ) ;
#115026 = DIRECTION ( 'NONE',  ( 0.7071067811865487940, 0.7071067811865463515, 0.000000000000000000 ) ) ;
#115027 = EDGE_LOOP ( 'NONE', ( #49495, #38114, #26110, #98218 ) ) ;
#115028 = EDGE_CURVE ( 'NONE', #103874, #84791, #8456, .T. ) ;
#115029 = CARTESIAN_POINT ( 'NONE',  ( 1.827855086967997700, 4.202752102959690472E-16, 0.000000000000000000 ) ) ;
#115030 = CARTESIAN_POINT ( 'NONE',  ( -17.99451991528748351, 28.92564299267950645, 4.000000000000000000 ) ) ;
#115031 = CARTESIAN_POINT ( 'NONE',  ( 79.68293019189812298, -1.637169565754158951, -6.109999999999998543 ) ) ;
#115032 = ORIENTED_EDGE ( 'NONE', *, *, #4276, .T. ) ;
#115033 = PLANE ( 'NONE',  #55892 ) ;
#115034 = LINE ( 'NONE', #104161, #107971 ) ;
#115035 = EDGE_CURVE ( 'NONE', #3179, #108745, #51310, .T. ) ;
#115036 = CARTESIAN_POINT ( 'NONE',  ( 8.700255128608413102, -27.71228299555199825, 4.000000000000000000 ) ) ;
#115037 = ORIENTED_EDGE ( 'NONE', *, *, #41847, .T. ) ;
#115038 = ORIENTED_EDGE ( 'NONE', *, *, #81689, .F. ) ;
#115039 = CARTESIAN_POINT ( 'NONE',  ( 24.70701326429286482, -21.74070752338406365, 4.999753212805220670 ) ) ;
#115040 = CARTESIAN_POINT ( 'NONE',  ( -21.18398860626899349, 28.73617430169802134, 5.000000000000000000 ) ) ;
#115041 = DIRECTION ( 'NONE',  ( 0.7071067811865486830, -0.7071067811865464625, -0.000000000000000000 ) ) ;
#115043 = ADVANCED_FACE ( 'NONE', ( #9168 ), #73081, .F. ) ;
#115042 = VECTOR ( 'NONE', #131361, 999.9999999999998863 ) ;
#115044 = SURFACE_STYLE_FILL_AREA ( #48395 ) ;
#115045 = DIRECTION ( 'NONE',  ( -0.5735764363510507113, 0.8191520442889885789, 1.003171929053520926E-16 ) ) ;
#115046 = CARTESIAN_POINT ( 'NONE',  ( -1.179999999999998384, -9.043340090917736163, 6.750000000000000888 ) ) ;
#115047 = ADVANCED_FACE ( 'NONE', ( #28121 ), #117234, .F. ) ;
#115048 = AXIS2_PLACEMENT_3D ( 'NONE', #37917, #14714, #58990 ) ;
#115049 = EDGE_LOOP ( 'NONE', ( #91171, #127951, #24890, #126796 ) ) ;
#115050 = ORIENTED_EDGE ( 'NONE', *, *, #118062, .F. ) ;
#115051 = DIRECTION ( 'NONE',  ( 0.7071067811865486830, -0.7071067811865464625, -0.000000000000000000 ) ) ;
#115052 = ORIENTED_EDGE ( 'NONE', *, *, #8183, .T. ) ;
#115053 = VECTOR ( 'NONE', #36777, 1000.000000000000000 ) ;
#115054 = ADVANCED_FACE ( 'NONE', ( #62188 ), #127419, .F. ) ;
#115055 = DIRECTION ( 'NONE',  ( 0.7071067811865487940, 0.7071067811865463515, 0.000000000000000000 ) ) ;
#115056 = EDGE_LOOP ( 'NONE', ( #62744, #6215, #48498, #142566, #41493 ) ) ;
#115057 = CARTESIAN_POINT ( 'NONE',  ( 69.49586038379622721, -3.974999999999998312, -6.884901960086286188 ) ) ;
#115058 = FACE_OUTER_BOUND ( 'NONE', #64732, .T. ) ;
#115059 = DIRECTION ( 'NONE',  ( 0.7071067811865487940, 0.7071067811865463515, 0.000000000000000000 ) ) ;
#115060 = VECTOR ( 'NONE', #140514, 1000.000000000000000 ) ;
#115061 = PLANE ( 'NONE',  #83170 ) ;
#115062 = CARTESIAN_POINT ( 'NONE',  ( 0.000000000000000000, 7.776507174585690191E-16, -6.349999999999997868 ) ) ;
#115063 = ORIENTED_EDGE ( 'NONE', *, *, #55046, .F. ) ;
#115064 = LINE ( 'NONE', #105625, #118848 ) ;
#115065 = CARTESIAN_POINT ( 'NONE',  ( -12.18398860626900060, 28.73617430169795739, 5.000000000000000000 ) ) ;
#115067 = ORIENTED_EDGE ( 'NONE', *, *, #62356, .F. ) ;
#115066 = VECTOR ( 'NONE', #138288, 1000.000000000000000 ) ;
#115068 = LINE ( 'NONE', #61484, #24999 ) ;
#115069 = VERTEX_POINT ( 'NONE', #107795 ) ;
#115070 = ORIENTED_EDGE ( 'NONE', *, *, #122230, .T. ) ;
#115071 = CARTESIAN_POINT ( 'NONE',  ( 0.000000000000000000, 0.000000000000000000, 5.000000000000000000 ) ) ;
#115072 = ORIENTED_EDGE ( 'NONE', *, *, #30115, .T. ) ;
#115073 = ORIENTED_EDGE ( 'NONE', *, *, #8865, .T. ) ;
#115074 = CARTESIAN_POINT ( 'NONE',  ( 74.81293019189809002, -1.637169565754159617, -6.110000000000001208 ) ) ;
#115075 = ORIENTED_EDGE ( 'NONE', *, *, #36012, .F. ) ;
#115076 = CARTESIAN_POINT ( 'NONE',  ( 23.93182425469048979, -0.2601698552150336075, 4.222180570310123393 ) ) ;
#115077 = CARTESIAN_POINT ( 'NONE',  ( -12.69999999999998153, 0.000000000000000000, 0.000000000000000000 ) ) ;
#115078 = VECTOR ( 'NONE', #3785, 1000.000000000000227 ) ;
#115079 = CARTESIAN_POINT ( 'NONE',  ( 106.7504301918981184, 3.055000000000002824, -5.291415217122919401 ) ) ;
#115080 = CARTESIAN_POINT ( 'NONE',  ( 0.000000000000000000, 0.000000000000000000, 5.000000000000000000 ) ) ;
#115081 = ADVANCED_FACE ( 'NONE', ( #84646 ), #140440, .F. ) ;
#115082 = LINE ( 'NONE', #135475, #43581 ) ;
#115083 = FACE_OUTER_BOUND ( 'NONE', #89091, .T. ) ;
#115084 = DIRECTION ( 'NONE',  ( -0.7071067811865486830, -0.7071067811865464625, 0.000000000000000000 ) ) ;
#115085 = CARTESIAN_POINT ( 'NONE',  ( -14.92733143757284786, -1.141545485034857643, 4.000000000000000000 ) ) ;
#115086 = PLANE ( 'NONE',  #58610 ) ;
#115087 = CARTESIAN_POINT ( 'NONE',  ( 11.93159235450332112, -2.500000000000000444, 3.061616997868384620E-16 ) ) ;
#115088 = PLANE ( 'NONE',  #123878 ) ;
#115089 = VERTEX_POINT ( 'NONE', #139764 ) ;
#115090 = CARTESIAN_POINT ( 'NONE',  ( -33.32816939922329880, -15.74070752338412404, 4.000000000000000000 ) ) ;
#115091 = DIRECTION ( 'NONE',  ( 0.000000000000000000, -1.000000000000000000, 0.000000000000000000 ) ) ;
#115092 = ORIENTED_EDGE ( 'NONE', *, *, #14618, .F. ) ;
#115093 = VERTEX_POINT ( 'NONE', #73762 ) ;
#115094 = DIRECTION ( 'NONE',  ( -0.7071067811865486830, -0.7071067811865464625, 0.000000000000000000 ) ) ;
#115095 = VERTEX_POINT ( 'NONE', #130308 ) ;
#115096 = CARTESIAN_POINT ( 'NONE',  ( -72.48921356237309510, -27.52281430457106026, 5.000000000000000000 ) ) ;
#115097 = EDGE_CURVE ( 'NONE', #90471, #29177, #6303, .T. ) ;
#115098 = CARTESIAN_POINT ( 'NONE',  ( 36.48921356237310221, -27.52281430457080802, 5.000000000000000000 ) ) ;
#115099 = CARTESIAN_POINT ( 'NONE',  ( -41.99451991528749062, 28.92564299267967343, 4.000000000000000000 ) ) ;
#115100 = EDGE_LOOP ( 'NONE', ( #86763, #97386, #41549, #48241 ) ) ;
#115101 = EDGE_CURVE ( 'NONE', #99617, #137268, #117939, .T. ) ;
#115102 = CARTESIAN_POINT ( 'NONE',  ( -19.82816939922338406, 9.759292476615620160, 4.000000000000000000 ) ) ;
#115103 = ORIENTED_EDGE ( 'NONE', *, *, #27944, .F. ) ;
#115104 = VECTOR ( 'NONE', #46105, 1000.000000000000000 ) ;
#115107 = EDGE_CURVE ( 'NONE', #12703, #816, #128847, .T. ) ;
#115106 = CARTESIAN_POINT ( 'NONE',  ( -57.18398860626899705, 28.73617430169827358, 5.000000000000000000 ) ) ;
#115105 = VECTOR ( 'NONE', #143087, 1000.000000000000000 ) ;
#115108 = MECHANICAL_DESIGN_GEOMETRIC_PRESENTATION_REPRESENTATION (  '', ( #133687 ), #29461 ) ;
#115109 = CARTESIAN_POINT ( 'NONE',  ( 25.15040314143521627, 7.934999999999989839, -2.126176841940961904 ) ) ;
#115110 = LINE ( 'NONE', #96220, #86375 ) ;
#115111 = DIRECTION ( 'NONE',  ( -0.000000000000000000, 0.3543493200069153248, 0.9351131265310292928 ) ) ;
#115112 = EDGE_CURVE ( 'NONE', #63799, #5098, #62917, .T. ) ;
#115113 = CARTESIAN_POINT ( 'NONE',  ( 13.61473099516978991, -9.049659518163096550, -2.897983823904738188 ) ) ;
#115114 = VERTEX_POINT ( 'NONE', #96200 ) ;
#115115 = ORIENTED_EDGE ( 'NONE', *, *, #59669, .T. ) ;
#115116 = VERTEX_POINT ( 'NONE', #41129 ) ;
#115117 = LINE ( 'NONE', #15788, #63485 ) ;
#115118 = CARTESIAN_POINT ( 'NONE',  ( 30.51665438641024153, 22.22500000000000142, 4.500000000000000888 ) ) ;
#115119 = AXIS2_PLACEMENT_3D ( 'NONE', #38932, #137544, #83153 ) ;
#115120 = CARTESIAN_POINT ( 'NONE',  ( -36.29974487139159578, -27.71228299555231445, 4.000000000000000000 ) ) ;
#115121 = DIRECTION ( 'NONE',  ( -0.6830127018922181881, 0.6830127018922202975, -0.2588190451025214056 ) ) ;
#115122 = LINE ( 'NONE', #26023, #129513 ) ;
#115123 = CARTESIAN_POINT ( 'NONE',  ( 17.61782366839360847, 8.969638207445433054, 4.000000000000000000 ) ) ;
#115124 = EDGE_CURVE ( 'NONE', #71084, #127668, #10622, .T. ) ;
#115125 = DIRECTION ( 'NONE',  ( -0.000000000000000000, 0.000000000000000000, 1.000000000000000000 ) ) ;
#115126 = CARTESIAN_POINT ( 'NONE',  ( 7.408407645496676963, -2.499999999999999556, 0.000000000000000000 ) ) ;
#115127 = PLANE ( 'NONE',  #76723 ) ;
#115128 = ORIENTED_EDGE ( 'NONE', *, *, #117739, .F. ) ;
#115129 = LINE ( 'NONE', #103557, #132039 ) ;
#115130 = EDGE_CURVE ( 'NONE', #112685, #86810, #86796, .T. ) ;
#115131 = DIRECTION ( 'NONE',  ( 0.000000000000000000, -1.000000000000000000, 0.000000000000000000 ) ) ;
#115132 = ORIENTED_EDGE ( 'NONE', *, *, #6698, .T. ) ;
#115133 = CARTESIAN_POINT ( 'NONE',  ( -3.183988606268992161, 28.73617430169789699, 5.000000000000000000 ) ) ;
#115135 = VERTEX_POINT ( 'NONE', #133857 ) ;
#115134 = CARTESIAN_POINT ( 'NONE',  ( 59.09089496824513787, -46.71325913967877597, -35.40428284070723208 ) ) ;
#115136 = ORIENTED_EDGE ( 'NONE', *, *, #46662, .F. ) ;
#115137 = DIRECTION ( 'NONE',  ( -0.000000000000000000, -0.3543493200069152693, 0.9351131265310292928 ) ) ;
#115138 = DIRECTION ( 'NONE',  ( -1.000000000000000000, -1.224606353822377258E-16, -0.000000000000000000 ) ) ;
#115140 = VECTOR ( 'NONE', #28680, 1000.000000000000000 ) ;
#115139 = DIRECTION ( 'NONE',  ( -0.000000000000000000, 0.3543493200069153248, 0.9351131265310291818 ) ) ;
#115141 = EDGE_CURVE ( 'NONE', #80852, #137944, #120080, .T. ) ;
#115142 = EDGE_LOOP ( 'NONE', ( #111544, #5461, #112739, #72935 ) ) ;
#115143 = ADVANCED_FACE ( 'NONE', ( #131720 ), #57043, .F. ) ;
#115144 = ORIENTED_EDGE ( 'NONE', *, *, #114060, .T. ) ;
#115145 = DIRECTION ( 'NONE',  ( -0.7071067811865486830, -0.7071067811865464625, 0.000000000000000000 ) ) ;
#115146 = CARTESIAN_POINT ( 'NONE',  ( 107.3124999999999858, 5.819803920172571310, 5.819803920172576639 ) ) ;
#115147 = CARTESIAN_POINT ( 'NONE',  ( 27.18293019189811588, -1.637169565754159173, -6.109999999999999432 ) ) ;
#115148 = DIRECTION ( 'NONE',  ( -0.7071067811865486830, 0.7071067811865464625, 0.000000000000000000 ) ) ;
#115149 = DIRECTION ( 'NONE',  ( -0.7071067811865486830, 0.7071067811865464625, 0.000000000000000000 ) ) ;
#115150 = CARTESIAN_POINT ( 'NONE',  ( -51.48921356237309510, -27.52281430457091460, 5.000000000000000000 ) ) ;
#115152 = EDGE_CURVE ( 'NONE', #51562, #15743, #78827, .T. ) ;
#115151 = CARTESIAN_POINT ( 'NONE',  ( 2.292893218813443657, 2.259292476615692546, 5.000000000000000000 ) ) ;
#115153 = FACE_OUTER_BOUND ( 'NONE', #102396, .T. ) ;
#115154 = CARTESIAN_POINT ( 'NONE',  ( 29.58290314143522082, 3.967499999999992699, -6.871911579029513994 ) ) ;
#115155 = CARTESIAN_POINT ( 'NONE',  ( 5.812069808101886892, 7.934999999999992504, 2.126176841940951689 ) ) ;
#115156 = DIRECTION ( 'NONE',  ( -0.7071067811865486830, -0.7071067811865464625, 0.000000000000000000 ) ) ;
#115157 = LINE ( 'NONE', #123954, #62831 ) ;
#115158 = DIRECTION ( 'NONE',  ( -1.000000000000000000, 0.000000000000000000, 0.000000000000000000 ) ) ;
#115159 = ORIENTED_EDGE ( 'NONE', *, *, #21262, .F. ) ;
#115160 =( BOUNDED_CURVE ( )  B_SPLINE_CURVE ( 3, ( #12818, #37465, #101993, #90398 ),
 .UNSPECIFIED., .F., .T. ) 
 B_SPLINE_CURVE_WITH_KNOTS ( ( 4, 4 ),
 ( 4.350170835173029715, 4.500739107949206286 ),
 .UNSPECIFIED. ) 
 CURVE ( )  GEOMETRIC_REPRESENTATION_ITEM ( )  RATIONAL_B_SPLINE_CURVE ( ( 1.000000000000000000, 0.9981116584018959736, 0.9981116584018959736, 1.000000000000000000 ) ) 
 REPRESENTATION_ITEM ( '' )  );
#115162 = ORIENTED_EDGE ( 'NONE', *, *, #10344, .F. ) ;
#115161 = ADVANCED_FACE ( 'NONE', ( #143297 ), #112119, .F. ) ;
#115163 = ADVANCED_FACE ( 'NONE', ( #121536 ), #34547, .F. ) ;
#115164 = CARTESIAN_POINT ( 'NONE',  ( 96.66666666666667140, 6.884901960086285300, 3.975000000000003642 ) ) ;
#115165 = VERTEX_POINT ( 'NONE', #21529 ) ;
#115166 = EDGE_LOOP ( 'NONE', ( #99774, #110376, #62609, #109963 ) ) ;
#115167 = CARTESIAN_POINT ( 'NONE',  ( 23.81663961620377279, -1.633150327867672447, -6.094999999999999751 ) ) ;
#115168 = DIRECTION ( 'NONE',  ( -0.000000000000000000, 0.3543493200069153248, 0.9351131265310292928 ) ) ;
#115169 = VERTEX_POINT ( 'NONE', #101214 ) ;
#115170 = FACE_OUTER_BOUND ( 'NONE', #97788, .T. ) ;
#115171 = EDGE_CURVE ( 'NONE', #20015, #98883, #131014, .T. ) ;
#115172 = FACE_OUTER_BOUND ( 'NONE', #99266, .T. ) ;
#115173 = LINE ( 'NONE', #137701, #27900 ) ;
#115174 = CARTESIAN_POINT ( 'NONE',  ( 126.3683832355216055, 7.029815251288743738, -0.9939000555549801774 ) ) ;
#115175 = ADVANCED_FACE ( 'NONE', ( #99055 ), #11316, .F. ) ;
#115176 = FACE_OUTER_BOUND ( 'NONE', #79999, .T. ) ;
#115177 = DIRECTION ( 'NONE',  ( 0.7071067811865486830, -0.7071067811865464625, -0.000000000000000000 ) ) ;
#115178 = CARTESIAN_POINT ( 'NONE',  ( 30.29974487139158867, -27.71228299555227537, 4.000000000000000000 ) ) ;
#115179 = DIRECTION ( 'NONE',  ( -0.000000000000000000, -0.3543493200069152693, 0.9351131265310292928 ) ) ;
#115180 = LINE ( 'NONE', #128948, #77636 ) ;
#115181 = CARTESIAN_POINT ( 'NONE',  ( 33.18398860626899705, 28.73617430169810305, 5.000000000000000000 ) ) ;
#115182 = CARTESIAN_POINT ( 'NONE',  ( 55.95337363913753848, -51.41954113333839871, 38.53170190052308186 ) ) ;
#115183 = VERTEX_POINT ( 'NONE', #44000 ) ;
#115184 = VERTEX_POINT ( 'NONE', #100525 ) ;
#115185 = CARTESIAN_POINT ( 'NONE',  ( 115.6462635252314328, -4.472830434245840259, 4.472830434245839371 ) ) ;
#115186 = AXIS2_PLACEMENT_3D ( 'NONE', #116359, #104766, #39536 ) ;
#115187 = ORIENTED_EDGE ( 'NONE', *, *, #32742, .T. ) ;
#115188 = EDGE_CURVE ( 'NONE', #130548, #9302, #55598, .T. ) ;
#115189 = LINE ( 'NONE', #125408, #126561 ) ;
#115190 = VERTEX_POINT ( 'NONE', #31690 ) ;
#115191 = EDGE_CURVE ( 'NONE', #111380, #108455, #75909, .T. ) ;
#115192 = DIRECTION ( 'NONE',  ( 0.7071067811865487940, 0.7071067811865463515, -0.000000000000000000 ) ) ;
#115193 = DIRECTION ( 'NONE',  ( -0.7071067811865486830, -0.7071067811865464625, 0.000000000000000000 ) ) ;
#115194 = VECTOR ( 'NONE', #106075, 1000.000000000000000 ) ;
#115195 = CARTESIAN_POINT ( 'NONE',  ( 100.3912635252314516, -4.472830434245839371, -4.472830434245839371 ) ) ;
#115196 = EDGE_LOOP ( 'NONE', ( #59998, #24387, #72569, #55129 ) ) ;
#115197 = VERTEX_POINT ( 'NONE', #89631 ) ;
#115198 = LINE ( 'NONE', #81210, #119439 ) ;
#115199 = FACE_OUTER_BOUND ( 'NONE', #21200, .T. ) ;
#115200 = DIRECTION ( 'NONE',  ( 0.3543493200069162685, -0.000000000000000000, -0.9351131265310288487 ) ) ;
#115201 = AXIS2_PLACEMENT_3D ( 'NONE', #45459, #88956, #66482 ) ;
#115202 = ORIENTED_EDGE ( 'NONE', *, *, #57438, .F. ) ;
#115203 = ORIENTED_EDGE ( 'NONE', *, *, #25504, .F. ) ;
#115204 = VECTOR ( 'NONE', #11280, 1000.000000000000227 ) ;
#115205 = ORIENTED_EDGE ( 'NONE', *, *, #69339, .F. ) ;
#115206 = CARTESIAN_POINT ( 'NONE',  ( -24.79593897580385331, 4.791522900035168675, 4.000000000000000000 ) ) ;
#115207 = CARTESIAN_POINT ( 'NONE',  ( 7.358736474768553748, 5.808823158059031044, -5.808823158059037262 ) ) ;
#115208 = CIRCLE ( 'NONE', #105915, 2.500000000000000888 ) ;
#115209 = VECTOR ( 'NONE', #71802, 1000.000000000000227 ) ;
#115210 = DIRECTION ( 'NONE',  ( 1.000000000000000000, 0.000000000000000000, 0.000000000000000000 ) ) ;
#115211 = EDGE_CURVE ( 'NONE', #141554, #121112, #122241, .T. ) ;
#115212 = DIRECTION ( 'NONE',  ( 0.000000000000000000, 1.000000000000000000, 0.000000000000000000 ) ) ;
#115213 = ORIENTED_EDGE ( 'NONE', *, *, #140376, .F. ) ;
#115214 = VERTEX_POINT ( 'NONE', #133166 ) ;
#115215 = CARTESIAN_POINT ( 'NONE',  ( -37.44665057663194574, 2.259292476615697876, 14.86850063742363126 ) ) ;
#115216 = ORIENTED_EDGE ( 'NONE', *, *, #52818, .F. ) ;
#115217 = VERTEX_POINT ( 'NONE', #109241 ) ;
#115218 = PLANE ( 'NONE',  #7715 ) ;
#115219 = DIRECTION ( 'NONE',  ( -0.7071067811865486830, -0.7071067811865464625, 0.000000000000000000 ) ) ;
#115220 = CARTESIAN_POINT ( 'NONE',  ( 63.18398860626900415, 28.73617430169831621, 5.000000000000000000 ) ) ;
#115221 = ORIENTED_EDGE ( 'NONE', *, *, #13048, .F. ) ;
#115222 = CARTESIAN_POINT ( 'NONE',  ( -7.828169399223476432, 21.75929247661548871, 4.000000000000000000 ) ) ;
#115223 = PLANE ( 'NONE',  #38647 ) ;
#115224 = LINE ( 'NONE', #47225, #64535 ) ;
#115225 = LINE ( 'NONE', #15909, #113811 ) ;
#115226 = DIRECTION ( 'NONE',  ( -0.7071067811865487940, 0.7071067811865463515, -0.000000000000000000 ) ) ;
#115227 = FACE_BOUND ( 'NONE', #105299, .T. ) ;
#115228 = ORIENTED_EDGE ( 'NONE', *, *, #85241, .F. ) ;
#115229 = CARTESIAN_POINT ( 'NONE',  ( 48.29974487139158867, -27.71228299555239971, 4.000000000000000000 ) ) ;
#115230 = FACE_OUTER_BOUND ( 'NONE', #4345, .T. ) ;
#115231 = LINE ( 'NONE', #39156, #88542 ) ;
#115232 = ORIENTED_EDGE ( 'NONE', *, *, #7755, .F. ) ;
#115233 = CARTESIAN_POINT ( 'NONE',  ( -25.49999999999982236, 12.05218569542904561, 5.000000000000000000 ) ) ;
#115234 = ORIENTED_EDGE ( 'NONE', *, *, #3583, .T. ) ;
#115235 = VECTOR ( 'NONE', #43611, 1000.000000000000000 ) ;
#115236 = ORIENTED_EDGE ( 'NONE', *, *, #90372, .T. ) ;
#115237 = ORIENTED_EDGE ( 'NONE', *, *, #95218, .T. ) ;
#115238 = CARTESIAN_POINT ( 'NONE',  ( 37.82876352523144448, 0.000000000000000000, -6.109999999999998543 ) ) ;
#115239 = VERTEX_POINT ( 'NONE', #22911 ) ;
#115240 = CARTESIAN_POINT ( 'NONE',  ( 57.48921356237308800, -27.52281430457095368, 5.000000000000000000 ) ) ;
#115241 = PLANE ( 'NONE',  #108669 ) ;
#115242 = CARTESIAN_POINT ( 'NONE',  ( 14.29320749275917635, 20.25929247661551358, 20.83292124670811418 ) ) ;
#115243 = VERTEX_POINT ( 'NONE', #67177 ) ;
#115244 = CARTESIAN_POINT ( 'NONE',  ( 19.93618820137057668, -0.2700000000508058218, 500000.0000000000582 ) ) ;
#115245 = LINE ( 'NONE', #4314, #70078 ) ;
#115246 = MECHANICAL_DESIGN_GEOMETRIC_PRESENTATION_REPRESENTATION (  '', ( #75983 ), #66774 ) ;
#115247 = DIRECTION ( 'NONE',  ( 0.000000000000000000, -1.000000000000000000, 0.000000000000000000 ) ) ;
#115248 = DIRECTION ( 'NONE',  ( 0.7071067811865487940, 0.7071067811865463515, 0.000000000000000000 ) ) ;
#115249 = DIRECTION ( 'NONE',  ( -0.7071067811865486830, -0.7071067811865464625, -0.000000000000000000 ) ) ;
#115250 = CARTESIAN_POINT ( 'NONE',  ( 32.99999999999975842, 14.58746187583910192, 4.000000000000000000 ) ) ;
#115251 = ORIENTED_EDGE ( 'NONE', *, *, #124687, .F. ) ;
#115252 = EDGE_CURVE ( 'NONE', #68516, #19275, #83594, .T. ) ;
#115253 = ORIENTED_EDGE ( 'NONE', *, *, #121467, .F. ) ;
#115254 = EDGE_LOOP ( 'NONE', ( #109068, #98864, #76854, #86731 ) ) ;
#115255 = ORIENTED_EDGE ( 'NONE', *, *, #70389, .F. ) ;
#115256 = CARTESIAN_POINT ( 'NONE',  ( 151.4000000000000057, -16.48000000000005016, 34.92499999999998295 ) ) ;
#115257 = ORIENTED_EDGE ( 'NONE', *, *, #61589, .T. ) ;
#115259 = VERTEX_POINT ( 'NONE', #111368 ) ;
#115258 = EDGE_CURVE ( 'NONE', #43279, #112772, #21054, .T. ) ;
#115260 = DIRECTION ( 'NONE',  ( 0.7071067811865487940, 0.7071067811865463515, 0.000000000000000000 ) ) ;
#115261 = DIRECTION ( 'NONE',  ( 0.7071067811865487940, -0.7071067811865463515, 0.000000000000000000 ) ) ;
#115262 = EDGE_CURVE ( 'NONE', #124292, #2262, #12059, .T. ) ;
#115263 = EDGE_CURVE ( 'NONE', #33303, #80619, #112807, .T. ) ;
#115264 = CARTESIAN_POINT ( 'NONE',  ( 26.99999999999981526, -6.108550654416935011, -3.114665004254905334 ) ) ;
#115265 = ORIENTED_EDGE ( 'NONE', *, *, #52470, .T. ) ;
#115266 = DIRECTION ( 'NONE',  ( 0.7071067811865487940, -0.7071067811865463515, 0.000000000000000000 ) ) ;
#115267 = VERTEX_POINT ( 'NONE', #70073 ) ;
#115269 = EDGE_CURVE ( 'NONE', #47748, #36255, #2601, .T. ) ;
#115268 = LINE ( 'NONE', #95700, #60618 ) ;
#115270 = ADVANCED_FACE ( 'NONE', ( #4702 ), #48999, .F. ) ;
#115271 = LINE ( 'NONE', #37780, #63567 ) ;
#115272 =( NAMED_UNIT ( * ) PLANE_ANGLE_UNIT ( ) SI_UNIT ( $, .RADIAN. ) );
#115273 = ORIENTED_EDGE ( 'NONE', *, *, #40711, .T. ) ;
#115275 = CARTESIAN_POINT ( 'NONE',  ( 1.499999999999987566, 12.05218569542904561, 5.000000000000000000 ) ) ;
#115274 = CARTESIAN_POINT ( 'NONE',  ( 104.1829301918981088, -1.637169565754159173, -6.109999999999999432 ) ) ;
#115276 = STYLED_ITEM ( 'NONE', ( #111165 ), #93406 ) ;
#115277 = EDGE_CURVE ( 'NONE', #79589, #24205, #58496, .T. ) ;
#115278 = DIRECTION ( 'NONE',  ( -0.7071067811865486830, -0.7071067811865464625, -0.000000000000000000 ) ) ;
#115279 = CARTESIAN_POINT ( 'NONE',  ( -29.99999999999979039, 12.25461709320618553, -10.07315571508704188 ) ) ;
#115280 = ORIENTED_EDGE ( 'NONE', *, *, #85715, .F. ) ;
#115281 = EDGE_LOOP ( 'NONE', ( #117372, #117204, #112130, #80110 ) ) ;
#115282 = DIRECTION ( 'NONE',  ( -0.000000000000000000, -0.3543493200069152693, 0.9351131265310292928 ) ) ;
#115283 = ORIENTED_EDGE ( 'NONE', *, *, #15473, .T. ) ;
#115284 = FACE_OUTER_BOUND ( 'NONE', #123767, .T. ) ;
#115285 = DIRECTION ( 'NONE',  ( 0.6830127018922180770, -0.6830127018922204085, -0.2588190451025213501 ) ) ;
#115286 = DIRECTION ( 'NONE',  ( 0.000000000000000000, 0.000000000000000000, -1.000000000000000000 ) ) ;
#115287 = DIRECTION ( 'NONE',  ( -1.000000000000000000, -1.224606353822377258E-16, -0.000000000000000000 ) ) ;
#115288 = EDGE_LOOP ( 'NONE', ( #77745, #58405, #62380, #85798 ) ) ;
#115289 = DIRECTION ( 'NONE',  ( 0.000000000000000000, 1.000000000000000000, -0.000000000000000000 ) ) ;
#115290 = EDGE_CURVE ( 'NONE', #51730, #16952, #48265, .T. ) ;
#115291 = PLANE ( 'NONE',  #81212 ) ;
#115292 = DIRECTION ( 'NONE',  ( -0.000000000000000000, -0.3543493200069152693, 0.9351131265310292928 ) ) ;
#115293 = EDGE_LOOP ( 'NONE', ( #25563, #61304, #3739, #14891 ) ) ;
#115294 = FACE_OUTER_BOUND ( 'NONE', #113530, .T. ) ;
#115295 = CARTESIAN_POINT ( 'NONE',  ( -13.78678096696632061, 12.75929247661558996, 10.29404684609032117 ) ) ;
#115296 = ORIENTED_EDGE ( 'NONE', *, *, #48536, .T. ) ;
#115297 = AXIS2_PLACEMENT_3D ( 'NONE', #64829, #109011, #79313 ) ;
#115299 = ORIENTED_EDGE ( 'NONE', *, *, #100267, .T. ) ;
#115298 = DIRECTION ( 'NONE',  ( -1.000000000000000000, -1.224606353822377258E-16, -0.000000000000000000 ) ) ;
#115300 = EDGE_LOOP ( 'NONE', ( #52729, #112398, #38771, #19367 ) ) ;
#115301 = CARTESIAN_POINT ( 'NONE',  ( -14.86926710130653717, 7.855190979727734835, -28.08282898950776385 ) ) ;
#115302 = FILL_AREA_STYLE ('',( #5842 ) ) ;
#115303 = EDGE_CURVE ( 'NONE', #97211, #52188, #101938, .T. ) ;
#115304 = AXIS2_PLACEMENT_3D ( 'NONE', #49541, #50944, #138672 ) ;
#115305 = VERTEX_POINT ( 'NONE', #81645 ) ;
#115306 = PLANE ( 'NONE',  #14113 ) ;
#115307 = AXIS2_PLACEMENT_3D ( 'NONE', #104202, #69494, #113678 ) ;
#115308 = LINE ( 'NONE', #39975, #77506 ) ;
#115309 = FILL_AREA_STYLE_COLOUR ( '', #18245 ) ;
#115310 =( BOUNDED_CURVE ( )  B_SPLINE_CURVE ( 3, ( #74206, #82247, #116274, #27113 ),
 .UNSPECIFIED., .F., .T. ) 
 B_SPLINE_CURVE_WITH_KNOTS ( ( 4, 4 ),
 ( 2.779374508378135378, 4.199602562396837158 ),
 .UNSPECIFIED. ) 
 CURVE ( )  GEOMETRIC_REPRESENTATION_ITEM ( )  RATIONAL_B_SPLINE_CURVE ( ( 1.000000000000000000, 0.8388583629366632710, 0.8388583629366632710, 1.000000000000000000 ) ) 
 REPRESENTATION_ITEM ( '' )  );
#115311 = ORIENTED_EDGE ( 'NONE', *, *, #65018, .F. ) ;
#115312 = CARTESIAN_POINT ( 'NONE',  ( -18.32816939922339827, -21.74070752338405654, 4.000000000000000000 ) ) ;
#115313 = CARTESIAN_POINT ( 'NONE',  ( -39.18398860626899705, 28.73617430169814568, 5.000000000000000000 ) ) ;
#115314 = CARTESIAN_POINT ( 'NONE',  ( -30.29974487139158867, -27.71228299555227537, 4.000000000000000000 ) ) ;
#115315 = CARTESIAN_POINT ( 'NONE',  ( -5.994519915287488843, 28.92564299267942118, 4.000000000000000000 ) ) ;
#115316 = ADVANCED_FACE ( 'NONE', ( #27216 ), #38125, .F. ) ;
#115318 = VECTOR ( 'NONE', #17614, 1000.000000000000000 ) ;
#115317 = CARTESIAN_POINT ( 'NONE',  ( 0.2569208697893814453, 4.202752102959690472E-16, 0.000000000000000000 ) ) ;
#115319 = CARTESIAN_POINT ( 'NONE',  ( 26.62809147121574327, 6.350000000000004974, -1.701477371937626826 ) ) ;
#115320 = CARTESIAN_POINT ( 'NONE',  ( -27.29974487139158512, -27.71228299555225405, 4.000000000000000000 ) ) ;
#115321 = DIRECTION ( 'NONE',  ( 0.000000000000000000, 1.000000000000000000, 6.938893903907228378E-15 ) ) ;
#115322 = EDGE_LOOP ( 'NONE', ( #83891, #117606, #15896, #134935 ) ) ;
#115323 = ORIENTED_EDGE ( 'NONE', *, *, #104175, .F. ) ;
#115324 = ORIENTED_EDGE ( 'NONE', *, *, #110757, .T. ) ;
#115325 = ADVANCED_FACE ( 'NONE', ( #82347 ), #125110, .F. ) ;
#115326 = CARTESIAN_POINT ( 'NONE',  ( 118.6874999999999858, -5.819803920172573086, 5.819803920172572198 ) ) ;
#115327 = EDGE_LOOP ( 'NONE', ( #84545, #193, #110553, #51606 ) ) ;
#115328 = VERTEX_POINT ( 'NONE', #3312 ) ;
#115329 = ADVANCED_FACE ( 'NONE', ( #103340 ), #3989, .F. ) ;
#115330 = ORIENTED_EDGE ( 'NONE', *, *, #90738, .T. ) ;
#115331 = CARTESIAN_POINT ( 'NONE',  ( -12.32816939922344979, -3.740707523384244837, 4.000000000000000000 ) ) ;
#115332 = VECTOR ( 'NONE', #55494, 1000.000000000000000 ) ;
#115333 = DIRECTION ( 'NONE',  ( 0.6830127018922181881, 0.6830127018922202975, -0.2588190451025214056 ) ) ;
#115334 = VERTEX_POINT ( 'NONE', #90343 ) ;
#115335 = PLANE ( 'NONE',  #117919 ) ;
#115337 = ADVANCED_FACE ( 'NONE', ( #126529 ), #79531, .F. ) ;
#115336 = AXIS2_PLACEMENT_3D ( 'NONE', #101793, #46015, #70642 ) ;
#115338 = DIRECTION ( 'NONE',  ( 0.000000000000000000, 0.000000000000000000, 1.000000000000000000 ) ) ;
#115339 = LINE ( 'NONE', #117498, #72100 ) ;
#115340 = CARTESIAN_POINT ( 'NONE',  ( 108.3545968585647472, -1.637169565754161615, 6.110000000000000320 ) ) ;
#115341 = EDGE_LOOP ( 'NONE', ( #82296, #18250, #113720, #92813 ) ) ;
#115342 = CARTESIAN_POINT ( 'NONE',  ( -13.41477511890566454, 6.314159094412498341, -31.22869265677382344 ) ) ;
#115343 = FACE_OUTER_BOUND ( 'NONE', #8384, .T. ) ;
#115344 = LINE ( 'NONE', #36408, #52011 ) ;
#115345 = CARTESIAN_POINT ( 'NONE',  ( 83.20419371712955581, -6.884901960086285300, -3.975000000000000089 ) ) ;
#115346 = CARTESIAN_POINT ( 'NONE',  ( -20.99451991528748707, 28.92564299267952777, 4.000000000000000000 ) ) ;
#115348 = ADVANCED_FACE ( 'NONE', ( #25796 ), #104788, .T. ) ;
#115347 =( BOUNDED_CURVE ( )  B_SPLINE_CURVE ( 3, ( #100389, #35872, #56906, #1727 ),
 .UNSPECIFIED., .F., .F. ) 
 B_SPLINE_CURVE_WITH_KNOTS ( ( 4, 4 ),
 ( 0.8834430019029047010, 0.8929338002999916979 ),
 .UNSPECIFIED. ) 
 CURVE ( )  GEOMETRIC_REPRESENTATION_ITEM ( )  RATIONAL_B_SPLINE_CURVE ( ( 1.000000000000000000, 0.9999924937429014449, 0.9999924937429014449, 1.000000000000000000 ) ) 
 REPRESENTATION_ITEM ( '' )  );
#115349 = CARTESIAN_POINT ( 'NONE',  ( 17.48334561358943162, 22.22500000000000142, 4.500000000000000888 ) ) ;
#115350 = FACE_OUTER_BOUND ( 'NONE', #113192, .T. ) ;
#115351 = CARTESIAN_POINT ( 'NONE',  ( 37.55836038379622011, -7.949999999999997513, -2.130196079827425759 ) ) ;
#115352 = DIRECTION ( 'NONE',  ( -1.000000000000000000, -1.224606353822377258E-16, -0.000000000000000000 ) ) ;
#115353 = DIRECTION ( 'NONE',  ( -0.6830127018922180770, -0.6830127018922204085, -0.2588190451025213501 ) ) ;
#115354 = ORIENTED_EDGE ( 'NONE', *, *, #141056, .T. ) ;
#115355 = VERTEX_POINT ( 'NONE', #116383 ) ;
#115356 = CARTESIAN_POINT ( 'NONE',  ( 37.16666666666666430, 6.884901960086285300, 3.975000000000003642 ) ) ;
#115357 = ORIENTED_EDGE ( 'NONE', *, *, #138994, .T. ) ;
#115358 = ORIENTED_EDGE ( 'NONE', *, *, #6976, .F. ) ;
#115359 = EDGE_CURVE ( 'NONE', #52699, #44719, #49731, .T. ) ;
#115360 = DIRECTION ( 'NONE',  ( -0.7071067811865486830, 0.7071067811865463515, 0.000000000000000000 ) ) ;
#115361 = DIRECTION ( 'NONE',  ( -0.6830127018922180770, -0.6830127018922204085, -0.2588190451025213501 ) ) ;
#115362 = ORIENTED_EDGE ( 'NONE', *, *, #34512, .T. ) ;
#115363 = VECTOR ( 'NONE', #57930, 1000.000000000000000 ) ;
#115364 = CARTESIAN_POINT ( 'NONE',  ( -34.92500000000001137, -22.22500000000000142, 4.000000000000000000 ) ) ;
#115366 = STYLED_ITEM ( 'NONE', ( #65472 ), #38349 ) ;
#115365 = DIRECTION ( 'NONE',  ( -0.7071067811865487940, 0.7071067811865463515, 0.000000000000000000 ) ) ;
#115367 = DIRECTION ( 'NONE',  ( -0.7071067811865487940, 0.7071067811865463515, 0.000000000000000000 ) ) ;
#115368 = CARTESIAN_POINT ( 'NONE',  ( 26.10459685856476852, 1.637169565754164946, -6.109999999999999432 ) ) ;
#115369 = ORIENTED_EDGE ( 'NONE', *, *, #85716, .T. ) ;
#115370 = DIRECTION ( 'NONE',  ( -0.6830127018922180770, -0.6830127018922204085, -0.2588190451025213501 ) ) ;
#115371 = ORIENTED_EDGE ( 'NONE', *, *, #40855, .T. ) ;
#115372 = LINE ( 'NONE', #50880, #138792 ) ;
#115373 = DIRECTION ( 'NONE',  ( 0.7071067811865486830, -0.7071067811865464625, -0.000000000000000000 ) ) ;
#115374 = DIRECTION ( 'NONE',  ( -0.000000000000000000, -0.000000000000000000, -1.000000000000000000 ) ) ;
#115375 = DIRECTION ( 'NONE',  ( 0.000000000000000000, 0.000000000000000000, 1.000000000000000000 ) ) ;
#115376 = ORIENTED_EDGE ( 'NONE', *, *, #135957, .T. ) ;
#115377 = ADVANCED_FACE ( 'NONE', ( #62740 ), #28682, .T. ) ;
#115378 = VERTEX_POINT ( 'NONE', #85167 ) ;
#115379 = LINE ( 'NONE', #50893, #142048 ) ;
#115380 = DIRECTION ( 'NONE',  ( 0.7071067811865487940, -0.7071067811865463515, 0.000000000000000000 ) ) ;
#115381 = DIRECTION ( 'NONE',  ( -1.000000000000000000, -1.224606353822377258E-16, -0.000000000000000000 ) ) ;
#115382 = ADVANCED_FACE ( 'NONE', ( #119222 ), #7598, .F. ) ;
#115383 = CARTESIAN_POINT ( 'NONE',  ( 53.14126352523144448, 4.472830434245836706, 4.472830434245840259 ) ) ;
#115384 = ORIENTED_EDGE ( 'NONE', *, *, #143042, .F. ) ;
#115385 = CARTESIAN_POINT ( 'NONE',  ( 0.000000000000000000, 0.000000000000000000, 5.000000000000000000 ) ) ;
#115386 = CARTESIAN_POINT ( 'NONE',  ( -11.99999999999992006, 10.93112307739207267, 4.000000000000000000 ) ) ;
#115387 = EDGE_LOOP ( 'NONE', ( #134878, #53315, #37664, #17738, #50157 ) ) ;
#115388 = ORIENTED_EDGE ( 'NONE', *, *, #4273, .F. ) ;
#115389 = CARTESIAN_POINT ( 'NONE',  ( 30.32816939922331656, -0.7407075233842805861, 4.000000000000000000 ) ) ;
#115390 = ORIENTED_EDGE ( 'NONE', *, *, #47549, .F. ) ;
#115391 = EDGE_CURVE ( 'NONE', #85257, #125144, #95334, .T. ) ;
#115392 = EDGE_CURVE ( 'NONE', #9454, #16274, #130127, .T. ) ;
#115393 = VECTOR ( 'NONE', #5107, 999.9999999999998863 ) ;
#115394 = CARTESIAN_POINT ( 'NONE',  ( 21.18398860626899349, 28.73617430169802134, 5.000000000000000000 ) ) ;
#115395 = ORIENTED_EDGE ( 'NONE', *, *, #115986, .F. ) ;
#115396 = DIRECTION ( 'NONE',  ( -0.000000000000000000, 0.3543493200069153248, 0.9351131265310292928 ) ) ;
#115397 = LINE ( 'NONE', #16088, #47889 ) ;
#115398 = AXIS2_PLACEMENT_3D ( 'NONE', #62886, #19356, #142578 ) ;
#115399 = VECTOR ( 'NONE', #77396, 1000.000000000000000 ) ;
#115400 = VECTOR ( 'NONE', #90687, 1000.000000000000227 ) ;
#115401 = DIRECTION ( 'NONE',  ( 1.000000000000000000, 0.000000000000000000, 0.000000000000000000 ) ) ;
#115402 = PRESENTATION_LAYER_ASSIGNMENT (  '', '', ( #103822 ) ) ;
#115403 = FACE_BOUND ( 'NONE', #118866, .T. ) ;
#115404 = EDGE_CURVE ( 'NONE', #42067, #121003, #105485, .T. ) ;
#115405 = LINE ( 'NONE', #124900, #112833 ) ;
#115406 = DIRECTION ( 'NONE',  ( 0.3543493200069162685, -0.000000000000000000, -0.9351131265310288487 ) ) ;
#115407 = FACE_OUTER_BOUND ( 'NONE', #22393, .T. ) ;
#115408 = EDGE_LOOP ( 'NONE', ( #60921, #80246, #102428, #102159 ) ) ;
#115409 = CARTESIAN_POINT ( 'NONE',  ( 18.48921356237309510, -27.52281430457068367, 5.000000000000000000 ) ) ;
#115411 = VERTEX_POINT ( 'NONE', #72926 ) ;
#115410 = DIRECTION ( 'NONE',  ( -0.000000000000000000, 1.000000000000000000, 2.921639538487157626E-15 ) ) ;
#115412 = VECTOR ( 'NONE', #115249, 1000.000000000000000 ) ;
#115413 = VECTOR ( 'NONE', #140155, 999.9999999999998863 ) ;
#115414 = DIRECTION ( 'NONE',  ( 0.000000000000000000, 0.000000000000000000, 1.000000000000000000 ) ) ;
#115415 = VERTEX_POINT ( 'NONE', #106920 ) ;
#115416 = VERTEX_POINT ( 'NONE', #93907 ) ;
#115417 = CARTESIAN_POINT ( 'NONE',  ( 62.18293019189812298, -1.637169565754158951, -6.109999999999998543 ) ) ;
#115418 = ORIENTED_EDGE ( 'NONE', *, *, #110427, .F. ) ;
#115419 = DIRECTION ( 'NONE',  ( -0.7071067811865486830, 0.7071067811865464625, 0.000000000000000000 ) ) ;
#115420 = DIRECTION ( 'NONE',  ( 0.3543493200069162685, -0.000000000000000000, -0.9351131265310288487 ) ) ;
#115421 = ORIENTED_EDGE ( 'NONE', *, *, #62820, .F. ) ;
#115422 = CARTESIAN_POINT ( 'NONE',  ( -34.92500000000001137, 19.51246187583930336, 4.000000000000000000 ) ) ;
#115423 = AXIS2_PLACEMENT_3D ( 'NONE', #104278, #26041, #48497 ) ;
#115424 = CIRCLE ( 'NONE', #50699, 3.378199999999997871 ) ;
#115425 = DIRECTION ( 'NONE',  ( -0.6830127018922181881, 0.6830127018922202975, -0.2588190451025214056 ) ) ;
#115426 = CARTESIAN_POINT ( 'NONE',  ( 101.9166666666666714, -6.884901960086287076, -3.975000000000000977 ) ) ;
#115427 = PLANE ( 'NONE',  #131510 ) ;
#115428 = DIRECTION ( 'NONE',  ( -0.000000000000000000, 0.3543493200069153248, 0.9351131265310292928 ) ) ;
#115429 = PLANE ( 'NONE',  #78717 ) ;
#115430 = ORIENTED_EDGE ( 'NONE', *, *, #61365, .F. ) ;
#115431 = AXIS2_PLACEMENT_3D ( 'NONE', #45157, #135013, #866 ) ;
#115432 = ORIENTED_EDGE ( 'NONE', *, *, #69537, .F. ) ;
#115433 = DIRECTION ( 'NONE',  ( 0.6830127018922180770, -0.6830127018922204085, -0.2588190451025213501 ) ) ;
#115434 = DIRECTION ( 'NONE',  ( 0.000000000000000000, 0.000000000000000000, -1.000000000000000000 ) ) ;
#115435 = ORIENTED_EDGE ( 'NONE', *, *, #139142, .F. ) ;
#115436 = VECTOR ( 'NONE', #54930, 1000.000000000000000 ) ;
#115437 = EDGE_LOOP ( 'NONE', ( #41197, #20688, #106403, #12736 ) ) ;
#115438 = CIRCLE ( 'NONE', #18273, 2.500000000000000888 ) ;
#115439 = ORIENTED_EDGE ( 'NONE', *, *, #48082, .F. ) ;
#115440 = FACE_OUTER_BOUND ( 'NONE', #86882, .T. ) ;
#115441 = EDGE_CURVE ( 'NONE', #37944, #55809, #18458, .T. ) ;
#115442 = DIRECTION ( 'NONE',  ( -0.000000000000000000, -0.000000000000000000, 1.000000000000000000 ) ) ;
#115443 = ORIENTED_EDGE ( 'NONE', *, *, #72717, .T. ) ;
#115444 = AXIS2_PLACEMENT_3D ( 'NONE', #17302, #61564, #105713 ) ;
#115445 = DIRECTION ( 'NONE',  ( -0.000000000000000000, 0.3543493200069153248, 0.9351131265310292928 ) ) ;
#115447 = ADVANCED_FACE ( 'NONE', ( #117076 ), #140282, .F. ) ;
#115446 = SURFACE_STYLE_USAGE ( .BOTH. , #47437 ) ;
#115448 = EDGE_CURVE ( 'NONE', #137834, #96838, #107636, .T. ) ;
#115449 = CARTESIAN_POINT ( 'NONE',  ( 7.212903141435218934, 3.967499999999992699, -6.871911579029513994 ) ) ;
#115450 = CARTESIAN_POINT ( 'NONE',  ( 9.299744871391588674, -27.71228299555212971, 4.000000000000000000 ) ) ;
#115451 = EDGE_CURVE ( 'NONE', #3406, #89682, #94610, .T. ) ;
#115452 = VERTEX_POINT ( 'NONE', #17753 ) ;
#115453 = PLANE ( 'NONE',  #43468 ) ;
#115454 = ADVANCED_FACE ( 'NONE', ( #40970 ), #38829, .F. ) ;
#115455 = LINE ( 'NONE', #105327, #141526 ) ;
#115456 = CARTESIAN_POINT ( 'NONE',  ( -23.99451991528749062, 28.92564299267954908, 4.000000000000000000 ) ) ;
#115457 = VECTOR ( 'NONE', #46009, 1000.000000000000000 ) ;
#115459 = ORIENTED_EDGE ( 'NONE', *, *, #36877, .F. ) ;
#115458 = CARTESIAN_POINT ( 'NONE',  ( -16.82816939922340893, -14.24070752338413826, 4.000000000000000000 ) ) ;
#115460 = ORIENTED_EDGE ( 'NONE', *, *, #62620, .T. ) ;
#115461 = EDGE_CURVE ( 'NONE', #56410, #19080, #8460, .T. ) ;
#115462 = FACE_OUTER_BOUND ( 'NONE', #79561, .T. ) ;
#115463 = DIRECTION ( 'NONE',  ( 0.7071067811865486830, -0.7071067811865464625, -0.000000000000000000 ) ) ;
#115464 = CARTESIAN_POINT ( 'NONE',  ( -9.707106781186478628, 14.25929247661557753, 5.000000000000000000 ) ) ;
#115465 = VERTEX_POINT ( 'NONE', #62028 ) ;
#115466 = EDGE_CURVE ( 'NONE', #66246, #44911, #127999, .T. ) ;
#115467 = CARTESIAN_POINT ( 'NONE',  ( 27.27825451568556048, 8.259292476615630818, 11.78515199841156935 ) ) ;
#115468 = FACE_OUTER_BOUND ( 'NONE', #125099, .T. ) ;
#115469 = PLANE ( 'NONE',  #76834 ) ;
#115470 = ORIENTED_EDGE ( 'NONE', *, *, #68395, .F. ) ;
#115471 = DIRECTION ( 'NONE',  ( 0.7071067811865486830, -0.7071067811865464625, -0.000000000000000000 ) ) ;
#115472 = DIRECTION ( 'NONE',  ( -0.000000000000000000, 0.3543493200069153248, 0.9351131265310292928 ) ) ;
#115473 = CYLINDRICAL_SURFACE ( 'NONE', #141836, 2.500000000000000000 ) ;
#115474 = EDGE_CURVE ( 'NONE', #7430, #115805, #139601, .T. ) ;
#115475 = LINE ( 'NONE', #116940, #63453 ) ;
#115476 = CARTESIAN_POINT ( 'NONE',  ( 29.14818355038126896, 17.25929247661554200, 8.802941693769270159 ) ) ;
#115477 = ORIENTED_EDGE ( 'NONE', *, *, #92811, .F. ) ;
#115478 = ORIENTED_EDGE ( 'NONE', *, *, #124511, .T. ) ;
#115479 = PLANE ( 'NONE',  #130604 ) ;
#115480 = CARTESIAN_POINT ( 'NONE',  ( 5.292893218813423672, -18.74070752338408852, 5.000000000000000000 ) ) ;
#115481 = EDGE_CURVE ( 'NONE', #118031, #11132, #110475, .T. ) ;
#115482 = CARTESIAN_POINT ( 'NONE',  ( 0.8537364747685528554, -5.808823158059035485, -5.808823158059033709 ) ) ;
#115483 = LINE ( 'NONE', #142298, #52845 ) ;
#115484 = CARTESIAN_POINT ( 'NONE',  ( -15.18398860626900237, 28.73617430169797871, 5.000000000000000000 ) ) ;
#115485 = LINE ( 'NONE', #19067, #18142 ) ;
#115486 = DIRECTION ( 'NONE',  ( 0.000000000000000000, 1.000000000000000000, 0.000000000000000000 ) ) ;
#115487 = ORIENTED_EDGE ( 'NONE', *, *, #4892, .F. ) ;
#115488 = CARTESIAN_POINT ( 'NONE',  ( -4.591674519009967703, -0.7407075233842735917, 14.76736230305379571 ) ) ;
#115489 = CARTESIAN_POINT ( 'NONE',  ( 26.99999999999980815, -2.904428200921286951, -6.989807076075007508 ) ) ;
#115490 = FACE_OUTER_BOUND ( 'NONE', #21093, .T. ) ;
#115491 = CARTESIAN_POINT ( 'NONE',  ( 44.97459685856478018, 1.637169565754164280, -6.109999999999997655 ) ) ;
#115492 = CARTESIAN_POINT ( 'NONE',  ( -54.18398860626899705, 28.73617430169825226, 5.000000000000000000 ) ) ;
#115493 = EDGE_LOOP ( 'NONE', ( #74654, #29815, #116918, #21018 ) ) ;
#115494 = VERTEX_POINT ( 'NONE', #55421 ) ;
#115495 = ADVANCED_FACE ( 'NONE', ( #43825 ), #118212, .T. ) ;
#115496 = ORIENTED_EDGE ( 'NONE', *, *, #128450, .F. ) ;
#115497 = MECHANICAL_DESIGN_GEOMETRIC_PRESENTATION_REPRESENTATION (  '', ( #101672 ), #124861 ) ;
#115498 = CARTESIAN_POINT ( 'NONE',  ( 2.700255128608413990, -27.71228299555204089, 4.000000000000000000 ) ) ;
#115499 = CIRCLE ( 'NONE', #136338, 2.055000000000001048 ) ;
#115500 = AXIS2_PLACEMENT_3D ( 'NONE', #23994, #124726, #100132 ) ;
#115501 = AXIS2_PLACEMENT_3D ( 'NONE', #46088, #24305, #80147 ) ;
#115502 = EDGE_CURVE ( 'NONE', #27206, #141564, #67006, .T. ) ;
#115503 = FILL_AREA_STYLE_COLOUR ( '', #73888 ) ;
#115504 = DIRECTION ( 'NONE',  ( -0.7071067811865486830, -0.7071067811865464625, 0.000000000000000000 ) ) ;
#115505 = CIRCLE ( 'NONE', #80801, 6.349999999999999645 ) ;
#115506 = CARTESIAN_POINT ( 'NONE',  ( 24.18398860626899705, 28.73617430169804265, 5.000000000000000000 ) ) ;
#115507 = CARTESIAN_POINT ( 'NONE',  ( 51.29974487139158867, -27.71228299555242103, 4.000000000000000000 ) ) ;
#115508 = FACE_OUTER_BOUND ( 'NONE', #20321, .T. ) ;
#115509 = EDGE_LOOP ( 'NONE', ( #25239, #103012, #11368 ) ) ;
#115510 = LINE ( 'NONE', #126420, #30194 ) ;
#115511 = DIRECTION ( 'NONE',  ( 0.7071067811865486830, -0.7071067811865464625, -0.000000000000000000 ) ) ;
#115512 = UNCERTAINTY_MEASURE_WITH_UNIT (LENGTH_MEASURE( 1.000000000000000082E-05 ), #87579, 'distance_accuracy_value', 'NONE');
#115513 = VECTOR ( 'NONE', #66008, 1000.000000000000114 ) ;
#115514 = LINE ( 'NONE', #51750, #111005 ) ;
#115515 = LINE ( 'NONE', #37294, #70582 ) ;
#115516 = ADVANCED_FACE ( 'NONE', ( #88774 ), #89459, .F. ) ;
#115517 = DIRECTION ( 'NONE',  ( 0.7071067811865487940, -0.7071067811865463515, 0.000000000000000000 ) ) ;
#115518 = CARTESIAN_POINT ( 'NONE',  ( 63.22502705046289151, 5.819803920172573086, -5.819803920172572198 ) ) ;
#115519 = FACE_OUTER_BOUND ( 'NONE', #133791, .T. ) ;
#115520 = VERTEX_POINT ( 'NONE', #119914 ) ;
#115521 = VERTEX_POINT ( 'NONE', #66304 ) ;
#115522 = CARTESIAN_POINT ( 'NONE',  ( 60.64583333333333570, 2.130196079827431976, -7.949999999999999289 ) ) ;
#115523 = CARTESIAN_POINT ( 'NONE',  ( -19.49999999999986855, 22.01701374228154151, 2.453858888625676471 ) ) ;
#115524 = EDGE_CURVE ( 'NONE', #100863, #53824, #64156, .T. ) ;
#115525 = DIRECTION ( 'NONE',  ( 1.000000000000000000, 0.000000000000000000, 0.000000000000000000 ) ) ;
#115526 = CARTESIAN_POINT ( 'NONE',  ( -3.005480084712505828, 28.92564299267936079, 4.000000000000000000 ) ) ;
#115527 = VECTOR ( 'NONE', #136933, 1000.000000000000227 ) ;
#115528 = VECTOR ( 'NONE', #111209, 1000.000000000000000 ) ;
#115529 = ORIENTED_EDGE ( 'NONE', *, *, #47900, .F. ) ;
#115530 = CARTESIAN_POINT ( 'NONE',  ( 127.1072581378824253, -3.174999999999999378, -5.499261314031185677 ) ) ;
#115531 = VECTOR ( 'NONE', #102409, 1000.000000000000227 ) ;
#115532 = EDGE_CURVE ( 'NONE', #142336, #133793, #22738, .T. ) ;
#115533 = CARTESIAN_POINT ( 'NONE',  ( 0.7070132642930391231, -21.74070752338405654, 4.999753212805213565 ) ) ;
#115534 = CARTESIAN_POINT ( 'NONE',  ( 59.64626352523142572, -4.472830434245840259, 4.472830434245839371 ) ) ;
#115535 = LINE ( 'NONE', #14832, #36693 ) ;
#115536 = VERTEX_POINT ( 'NONE', #11880 ) ;
#115537 = ORIENTED_EDGE ( 'NONE', *, *, #107223, .T. ) ;
#115538 = LINE ( 'NONE', #16230, #97881 ) ;
#115539 = AXIS2_PLACEMENT_3D ( 'NONE', #103273, #3923, #77985 ) ;
#115540 = VECTOR ( 'NONE', #143183, 1000.000000000000000 ) ;
#115541 = PLANE ( 'NONE',  #22206 ) ;
#115542 = VECTOR ( 'NONE', #141391, 1000.000000000000000 ) ;
#115543 = DIRECTION ( 'NONE',  ( 0.000000000000000000, 5.075120898959323014E-15, 1.000000000000000000 ) ) ;
#115544 = EDGE_CURVE ( 'NONE', #37768, #92198, #8988, .T. ) ;
#115545 = DIRECTION ( 'NONE',  ( -0.3543493200069162685, -0.000000000000000000, -0.9351131265310288487 ) ) ;
#115547 = ORIENTED_EDGE ( 'NONE', *, *, #141793, .T. ) ;
#115546 = DIRECTION ( 'NONE',  ( -0.7071067811865486830, 0.7071067811865464625, 0.000000000000000000 ) ) ;
#115548 = LINE ( 'NONE', #138065, #131736 ) ;
#115549 = DIRECTION ( 'NONE',  ( 0.000000000000000000, -1.000000000000000000, 0.000000000000000000 ) ) ;
#115550 = CARTESIAN_POINT ( 'NONE',  ( 39.18398860626899705, 28.73617430169814568, 5.000000000000000000 ) ) ;
#115551 = AXIS2_PLACEMENT_3D ( 'NONE', #57820, #101290, #113583 ) ;
#115552 = LINE ( 'NONE', #106847, #138743 ) ;
#115553 = CIRCLE ( 'NONE', #113300, 2.055000000000000604 ) ;
#115554 = ORIENTED_EDGE ( 'NONE', *, *, #5362, .T. ) ;
#115555 = ORIENTED_EDGE ( 'NONE', *, *, #79753, .F. ) ;
#115556 = DIRECTION ( 'NONE',  ( -0.000000000000000000, 0.000000000000000000, 1.000000000000000000 ) ) ;
#115557 = LINE ( 'NONE', #48937, #132117 ) ;
#115558 = LINE ( 'NONE', #114171, #70992 ) ;
#115559 = DIRECTION ( 'NONE',  ( 1.000000000000000000, 0.000000000000000000, 0.000000000000000000 ) ) ;
#115560 = ORIENTED_EDGE ( 'NONE', *, *, #61538, .T. ) ;
#115561 = ORIENTED_EDGE ( 'NONE', *, *, #93272, .F. ) ;
#115562 = DIRECTION ( 'NONE',  ( -0.6830127018922180770, -0.6830127018922204085, -0.2588190451025213501 ) ) ;
#115563 = FILL_AREA_STYLE ('',( #126468 ) ) ;
#115564 = ORIENTED_EDGE ( 'NONE', *, *, #63981, .T. ) ;
#115565 = VERTEX_POINT ( 'NONE', #108317 ) ;
#115566 = EDGE_CURVE ( 'NONE', #138000, #141315, #133003, .T. ) ;
#115567 = DIRECTION ( 'NONE',  ( -0.7071067811865486830, -0.7071067811865464625, 0.000000000000000000 ) ) ;
#115568 = ORIENTED_EDGE ( 'NONE', *, *, #75675, .F. ) ;
#115569 = DIRECTION ( 'NONE',  ( -1.000000000000000000, 0.000000000000000000, -0.000000000000000000 ) ) ;
#115570 = CARTESIAN_POINT ( 'NONE',  ( 0.000000000000000000, 0.000000000000000000, 5.000000000000000000 ) ) ;
#115571 = FACE_BOUND ( 'NONE', #61351, .T. ) ;
#115572 = EDGE_CURVE ( 'NONE', #102891, #73062, #10455, .T. ) ;
#115573 = CARTESIAN_POINT ( 'NONE',  ( -62.99451991528749772, 28.92564299267982264, 4.000000000000000000 ) ) ;
#115574 = PLANE ( 'NONE',  #4966 ) ;
#115575 = DIRECTION ( 'NONE',  ( 1.000000000000000000, 0.000000000000000000, 0.000000000000000000 ) ) ;
#115576 = CARTESIAN_POINT ( 'NONE',  ( 2.999999999999999112, 0.000000000000000000, 0.000000000000000000 ) ) ;
#115577 = CARTESIAN_POINT ( 'NONE',  ( 152.4000000000000057, 7.919999999999947526, 19.12499999999998224 ) ) ;
#115578 = APPLICATION_PROTOCOL_DEFINITION ( 'draft international standard', 'automotive_design', 1998, #127200 ) ;
#115579 = ORIENTED_EDGE ( 'NONE', *, *, #42361, .T. ) ;
#115580 = ORIENTED_EDGE ( 'NONE', *, *, #130264, .F. ) ;
#115581 = CARTESIAN_POINT ( 'NONE',  ( 93.68293019189812298, -1.637169565754158951, -6.109999999999998543 ) ) ;
#115582 = EDGE_LOOP ( 'NONE', ( #94102, #2111, #62172, #35982 ) ) ;
#115583 = CARTESIAN_POINT ( 'NONE',  ( 0.000000000000000000, 0.000000000000000000, 5.000000000000000000 ) ) ;
#115584 = LINE ( 'NONE', #37372, #125429 ) ;
#115585 = DIRECTION ( 'NONE',  ( 0.000000000000000000, -1.000000000000000000, 0.000000000000000000 ) ) ;
#115586 = ORIENTED_EDGE ( 'NONE', *, *, #87824, .T. ) ;
#115587 = CARTESIAN_POINT ( 'NONE',  ( 24.29974487139158867, -27.71228299555223273, 4.000000000000000000 ) ) ;
#115588 = LINE ( 'NONE', #128663, #43115 ) ;
#115589 = DIRECTION ( 'NONE',  ( 0.6830127018922180770, -0.6830127018922204085, -0.2588190451025213501 ) ) ;
#115591 = FACE_OUTER_BOUND ( 'NONE', #79131, .T. ) ;
#115590 = DIRECTION ( 'NONE',  ( -0.000000000000000000, -0.000000000000000000, 1.000000000000000000 ) ) ;
#115592 =( LENGTH_UNIT ( ) NAMED_UNIT ( * ) SI_UNIT ( .MILLI., .METRE. ) );
#115593 = CARTESIAN_POINT ( 'NONE',  ( -6.792893218813407685, -8.240707523384200428, 5.000000000000000000 ) ) ;
#115594 = AXIS2_PLACEMENT_3D ( 'NONE', #104914, #5582, #62143 ) ;
#115595 = STYLED_ITEM ( 'NONE', ( #54357 ), #70138 ) ;
#115596 = CIRCLE ( 'NONE', #99475, 9.000000000000001776 ) ;
#115597 = DIRECTION ( 'NONE',  ( 0.7071067811865486830, -0.7071067811865464625, -0.000000000000000000 ) ) ;
#115598 = VECTOR ( 'NONE', #24143, 1000.000000000000000 ) ;
#115599 = VERTEX_POINT ( 'NONE', #76470 ) ;
#115600 = CARTESIAN_POINT ( 'NONE',  ( 17.99451991528748351, 28.92564299267950645, 4.000000000000000000 ) ) ;
#115601 =( BOUNDED_CURVE ( )  B_SPLINE_CURVE ( 3, ( #113762, #45688, #34792, #112347 ),
 .UNSPECIFIED., .F., .T. ) 
 B_SPLINE_CURVE_WITH_KNOTS ( ( 4, 4 ),
 ( 5.920967161967928050, 7.341195215986584088 ),
 .UNSPECIFIED. ) 
 CURVE ( )  GEOMETRIC_REPRESENTATION_ITEM ( )  RATIONAL_B_SPLINE_CURVE ( ( 1.000000000000000000, 0.8388583629366732630, 0.8388583629366732630, 1.000000000000000000 ) ) 
 REPRESENTATION_ITEM ( '' )  );
#115602 = CARTESIAN_POINT ( 'NONE',  ( -17.99999999999986855, 17.96639925780207747, 5.000000000000000000 ) ) ;
#115603 = ADVANCED_FACE ( 'NONE', ( #98209 ), #21355, .F. ) ;
#115604 = AXIS2_PLACEMENT_3D ( 'NONE', #83939, #139742, #40420 ) ;
#115605 = VERTEX_POINT ( 'NONE', #97465 ) ;
#115606 = ORIENTED_EDGE ( 'NONE', *, *, #11458, .F. ) ;
#115607 = ORIENTED_EDGE ( 'NONE', *, *, #88700, .T. ) ;
#115608 = CARTESIAN_POINT ( 'NONE',  ( 46.52126352523142572, -4.472830434245838482, -4.472830434245840259 ) ) ;
#115609 = ORIENTED_EDGE ( 'NONE', *, *, #49910, .T. ) ;
#115610 = AXIS2_PLACEMENT_3D ( 'NONE', #44065, #14275, #67241 ) ;
#115611 = EDGE_CURVE ( 'NONE', #68485, #91029, #97411, .T. ) ;
#115612 = AXIS2_PLACEMENT_3D ( 'NONE', #7441, #129230, #37978 ) ;
#115613 = CARTESIAN_POINT ( 'NONE',  ( 18.56663961620376924, 1.633150327867695095, 6.094999999999988205 ) ) ;
#115614 = CARTESIAN_POINT ( 'NONE',  ( -15.70492293426981334, 6.989513400225817463, -28.49959148306838230 ) ) ;
#115615 = EDGE_CURVE ( 'NONE', #41257, #119805, #88041, .T. ) ;
#115616 = ORIENTED_EDGE ( 'NONE', *, *, #35861, .T. ) ;
#115617 = ADVANCED_FACE ( 'NONE', ( #98894 ), #16478, .T. ) ;
#115618 = DIRECTION ( 'NONE',  ( 0.3543493200069162685, -0.000000000000000000, -0.9351131265310288487 ) ) ;
#115620 = VERTEX_POINT ( 'NONE', #137263 ) ;
#115619 = EDGE_CURVE ( 'NONE', #58958, #124820, #68659, .T. ) ;
#115621 =( NAMED_UNIT ( * ) SI_UNIT ( $, .STERADIAN. ) SOLID_ANGLE_UNIT ( ) );
#115622 = VECTOR ( 'NONE', #118766, 1000.000000000000000 ) ;
#115623 = CARTESIAN_POINT ( 'NONE',  ( 34.75611968250419892, -3.187065745292582797, 4.955485411084882053 ) ) ;
#115625 = ORIENTED_EDGE ( 'NONE', *, *, #106814, .F. ) ;
#115624 = CARTESIAN_POINT ( 'NONE',  ( 28.99806943317882002, -22.22500000000000142, 4.500000000000000888 ) ) ;
#115626 = ORIENTED_EDGE ( 'NONE', *, *, #6500, .T. ) ;
#115627 = EDGE_CURVE ( 'NONE', #114036, #103815, #4521, .T. ) ;
#115628 = CARTESIAN_POINT ( 'NONE',  ( 27.32816939922334853, 14.25929247661557397, 4.000000000000000000 ) ) ;
#115629 = DIRECTION ( 'NONE',  ( 0.000000000000000000, 0.000000000000000000, 1.000000000000000000 ) ) ;
#115630 = VERTEX_POINT ( 'NONE', #56881 ) ;
#115631 = VECTOR ( 'NONE', #70852, 999.9999999999998863 ) ;
#115632 = DIRECTION ( 'NONE',  ( -0.000000000000000000, -0.3543493200069152693, 0.9351131265310292928 ) ) ;
#115633 = ORIENTED_EDGE ( 'NONE', *, *, #86765, .F. ) ;
#115634 = EDGE_LOOP ( 'NONE', ( #56553, #142093, #91399, #93059 ) ) ;
#115635 = ORIENTED_EDGE ( 'NONE', *, *, #114902, .T. ) ;
#115636 = EDGE_CURVE ( 'NONE', #110801, #141891, #37224, .T. ) ;
#115637 = VERTEX_POINT ( 'NONE', #48832 ) ;
#115638 = LINE ( 'NONE', #94623, #68059 ) ;
#115639 = VECTOR ( 'NONE', #5210, 1000.000000000000000 ) ;
#115640 = VECTOR ( 'NONE', #77075, 1000.000000000000000 ) ;
#115641 = FACE_OUTER_BOUND ( 'NONE', #136427, .T. ) ;
#115642 = AXIS2_PLACEMENT_3D ( 'NONE', #126084, #7837, #94135 ) ;
#115643 = EDGE_CURVE ( 'NONE', #17453, #73565, #125677, .T. ) ;
#115644 = CARTESIAN_POINT ( 'NONE',  ( 181.1500000000000057, -43.14999999999999147, 34.92499999999998295 ) ) ;
#115645 = CARTESIAN_POINT ( 'NONE',  ( 26.67183060077627488, -9.740707523384191546, 4.000000000000000000 ) ) ;
#115646 = ADVANCED_FACE ( 'NONE', ( #37959 ), #67755, .F. ) ;
#115647 = AXIS2_PLACEMENT_3D ( 'NONE', #44367, #133496, #34183 ) ;
#115648 = CARTESIAN_POINT ( 'NONE',  ( 66.77083333333331439, -7.949999999999998401, -2.130196079827426203 ) ) ;
#115649 = ORIENTED_EDGE ( 'NONE', *, *, #79867, .F. ) ;
#115650 = AXIS2_PLACEMENT_3D ( 'NONE', #93108, #106083, #115525 ) ;
#115651 = DIRECTION ( 'NONE',  ( 0.7071067811865487940, 0.7071067811865463515, -0.000000000000000000 ) ) ;
#115652 = EDGE_CURVE ( 'NONE', #136003, #64283, #134608, .T. ) ;
#115653 = CARTESIAN_POINT ( 'NONE',  ( 30.45790314143522437, 6.871911579029515771, 3.967499999999989146 ) ) ;
#115654 = DIRECTION ( 'NONE',  ( -0.7071067811865486830, -0.7071067811865464625, -0.000000000000000000 ) ) ;
#115655 = CARTESIAN_POINT ( 'NONE',  ( -5.277185695429377432, -21.72500000000000853, 5.000000000000000000 ) ) ;
#115656 = VERTEX_POINT ( 'NONE', #102504 ) ;
#115657 = EDGE_LOOP ( 'NONE', ( #136757, #138675, #110933, #8570, #115362 ) ) ;
#115658 = ORIENTED_EDGE ( 'NONE', *, *, #116569, .F. ) ;
#115659 = DIRECTION ( 'NONE',  ( -0.6830127018922180770, -0.6830127018922204085, -0.2588190451025213501 ) ) ;
#115660 = LINE ( 'NONE', #80949, #18652 ) ;
#115661 = EDGE_CURVE ( 'NONE', #57451, #31683, #24219, .T. ) ;
#115662 = CARTESIAN_POINT ( 'NONE',  ( -14.48334561358944761, 22.22500000000000142, 4.500000000000000888 ) ) ;
#115663 = DIRECTION ( 'NONE',  ( 0.6830127018922181881, 0.6830127018922202975, -0.2588190451025214056 ) ) ;
#115664 = DIRECTION ( 'NONE',  ( -0.6830127018922181881, 0.6830127018922202975, -0.2588190451025214056 ) ) ;
#115665 = CARTESIAN_POINT ( 'NONE',  ( 75.89126352523143737, -4.472830434245839371, -4.472830434245839371 ) ) ;
#115666 = CARTESIAN_POINT ( 'NONE',  ( 81.35416666666667140, -2.130196079827501698, -7.949999999999956657 ) ) ;
#115667 = CARTESIAN_POINT ( 'NONE',  ( 74.99451991528749772, 28.92564299267990435, 4.000000000000000000 ) ) ;
#115668 = LINE ( 'NONE', #5499, #41464 ) ;
#115669 = CARTESIAN_POINT ( 'NONE',  ( 72.18398860626899705, 28.73617430169837661, 5.000000000000000000 ) ) ;
#115670 = DIRECTION ( 'NONE',  ( 1.000000000000000000, 0.000000000000000000, 0.000000000000000000 ) ) ;
#115671 = EDGE_CURVE ( 'NONE', #91273, #30305, #25622, .T. ) ;
#115672 = ORIENTED_EDGE ( 'NONE', *, *, #137421, .T. ) ;
#115673 = CIRCLE ( 'NONE', #53203, 2.500000000000000444 ) ;
#115674 = CARTESIAN_POINT ( 'NONE',  ( -10.17183060077640810, -17.24070752338411694, 4.000000000000000000 ) ) ;
#115675 = VERTEX_POINT ( 'NONE', #26357 ) ;
#115676 = LINE ( 'NONE', #60678, #69145 ) ;
#115678 = VERTEX_POINT ( 'NONE', #90915 ) ;
#115677 = DIRECTION ( 'NONE',  ( -0.7071067811865486830, -0.7071067811865464625, 0.000000000000000000 ) ) ;
#115679 = LINE ( 'NONE', #114965, #136621 ) ;
#115680 = DIRECTION ( 'NONE',  ( 0.7071067811865486830, -0.7071067811865464625, -0.000000000000000000 ) ) ;
#115681 = ORIENTED_EDGE ( 'NONE', *, *, #132277, .T. ) ;
#115682 = DIRECTION ( 'NONE',  ( 0.000000000000000000, -1.000000000000000000, 0.000000000000000000 ) ) ;
#115683 = ORIENTED_EDGE ( 'NONE', *, *, #101611, .T. ) ;
#115684 = DIRECTION ( 'NONE',  ( -0.7071067811865486830, -0.7071067811865464625, -0.000000000000000000 ) ) ;
#115685 = ORIENTED_EDGE ( 'NONE', *, *, #23055, .F. ) ;
#115686 = CARTESIAN_POINT ( 'NONE',  ( 31.49999999999978684, 18.43112307739199451, 4.000000000000000000 ) ) ;
#115687 = EDGE_CURVE ( 'NONE', #51279, #65170, #114066, .T. ) ;
#115688 = CARTESIAN_POINT ( 'NONE',  ( 96.32919371712955581, -3.975000000000001865, 6.884901960086284411 ) ) ;
#115689 = CARTESIAN_POINT ( 'NONE',  ( 72.31250000000001421, 5.819803920172571310, 5.819803920172576639 ) ) ;
#115690 = DIRECTION ( 'NONE',  ( 0.7071067811865486830, -0.7071067811865464625, -0.000000000000000000 ) ) ;
#115691 = ORIENTED_EDGE ( 'NONE', *, *, #10811, .F. ) ;
#115692 = CARTESIAN_POINT ( 'NONE',  ( -57.29974487139158157, -27.71228299555246011, 4.000000000000000000 ) ) ;
#115693 = ADVANCED_FACE ( 'NONE', ( #90167 ), #47445, .F. ) ;
#115694 = DIRECTION ( 'NONE',  ( -0.7071067811865486830, -0.7071067811865464625, 0.000000000000000000 ) ) ;
#115695 = CARTESIAN_POINT ( 'NONE',  ( 19.68750000000000000, 4.461849672132297329, -4.461849672132302658 ) ) ;
#115696 = DIRECTION ( 'NONE',  ( -0.000000000000000000, -0.3543493200069152693, 0.9351131265310292928 ) ) ;
#115697 = ORIENTED_EDGE ( 'NONE', *, *, #83627, .T. ) ;
#115698 = CARTESIAN_POINT ( 'NONE',  ( 20.99999999999985079, -0.2811185226894094558, -5.995736974527563490 ) ) ;
#115699 = ORIENTED_EDGE ( 'NONE', *, *, #41213, .T. ) ;
#115700 = VECTOR ( 'NONE', #114256, 1000.000000000000000 ) ;
#115701 = EDGE_CURVE ( 'NONE', #71447, #20610, #142730, .T. ) ;
#115702 = CARTESIAN_POINT ( 'NONE',  ( 88.08376352523144703, -6.110000000000001208, -3.741295971395164515E-16 ) ) ;
#115703 = CARTESIAN_POINT ( 'NONE',  ( -51.18398860626899705, 28.73617430169823095, 5.000000000000000000 ) ) ;
#115704 = VECTOR ( 'NONE', #134341, 1000.000000000000227 ) ;
#115705 = DIRECTION ( 'NONE',  ( -0.7071067811865487940, 0.7071067811865463515, -0.000000000000000000 ) ) ;
#115706 = CARTESIAN_POINT ( 'NONE',  ( -14.51078643762690490, -27.52281430457045275, 5.000000000000000000 ) ) ;
#115707 = ORIENTED_EDGE ( 'NONE', *, *, #41124, .T. ) ;
#115708 = AXIS2_PLACEMENT_3D ( 'NONE', #84321, #96549, #41485 ) ;
#115709 = VECTOR ( 'NONE', #50106, 1000.000000000000227 ) ;
#115710 = CARTESIAN_POINT ( 'NONE',  ( 25.39999999999999858, 1.399999999999987699, -20.40202195861970580 ) ) ;
#115711 = VECTOR ( 'NONE', #18431, 1000.000000000000000 ) ;
#115712 = DIRECTION ( 'NONE',  ( -0.000000000000000000, 0.3543493200069153248, 0.9351131265310292928 ) ) ;
#115713 = CARTESIAN_POINT ( 'NONE',  ( 117.7666937171295416, -7.949999999999998401, 2.130196079827423983 ) ) ;
#115714 = EDGE_CURVE ( 'NONE', #139082, #7243, #60526, .T. ) ;
#115715 = CARTESIAN_POINT ( 'NONE',  ( 12.69999999999999574, 0.000000000000000000, -40.00000000000000000 ) ) ;
#115717 = ORIENTED_EDGE ( 'NONE', *, *, #21201, .F. ) ;
#115716 = CARTESIAN_POINT ( 'NONE',  ( 20.99065804761471199, 4.584330080086930965E-16, 0.000000000000000000 ) ) ;
#115718 = DIRECTION ( 'NONE',  ( -1.000000000000000000, -1.224606353822377258E-16, -0.000000000000000000 ) ) ;
#115719 = DIRECTION ( 'NONE',  ( -0.7071067811865486830, -0.7071067811865464625, -0.000000000000000000 ) ) ;
#115720 = AXIS2_PLACEMENT_3D ( 'NONE', #80279, #114976, #138931 ) ;
#115721 = CARTESIAN_POINT ( 'NONE',  ( 7.939999999999994174, -60.26999999999998892, -10.00000000000000178 ) ) ;
#115722 = ORIENTED_EDGE ( 'NONE', *, *, #12870, .T. ) ;
#115723 = ORIENTED_EDGE ( 'NONE', *, *, #12202, .F. ) ;
#115724 = ORIENTED_EDGE ( 'NONE', *, *, #91262, .T. ) ;
#115725 = CARTESIAN_POINT ( 'NONE',  ( 70.29209685856477563, -5.291415217122921177, 3.054999999999999272 ) ) ;
#115726 = ORIENTED_EDGE ( 'NONE', *, *, #66978, .T. ) ;
#115727 = FACE_OUTER_BOUND ( 'NONE', #50686, .T. ) ;
#115728 = LINE ( 'NONE', #81759, #115053 ) ;
#115729 = VECTOR ( 'NONE', #67629, 999.9999999999998863 ) ;
#115730 = VECTOR ( 'NONE', #46988, 1000.000000000000227 ) ;
#115731 = LINE ( 'NONE', #6248, #15561 ) ;
#115732 = DIRECTION ( 'NONE',  ( 0.000000000000000000, -1.000000000000000000, 0.000000000000000000 ) ) ;
#115733 = ORIENTED_EDGE ( 'NONE', *, *, #120357, .F. ) ;
#115734 = DIRECTION ( 'NONE',  ( 0.6830127018922180770, -0.6830127018922204085, -0.2588190451025213501 ) ) ;
#115735 = DIRECTION ( 'NONE',  ( 0.7071067811865486830, -0.7071067811865464625, -0.000000000000000000 ) ) ;
#115736 = VECTOR ( 'NONE', #74416, 1000.000000000000000 ) ;
#115737 = ORIENTED_EDGE ( 'NONE', *, *, #119908, .F. ) ;
#115738 = EDGE_CURVE ( 'NONE', #55801, #100675, #38659, .T. ) ;
#115739 = LINE ( 'NONE', #60741, #7299 ) ;
#115740 = VECTOR ( 'NONE', #124293, 1000.000000000000000 ) ;
#115741 = DIRECTION ( 'NONE',  ( 0.7071067811865487940, -0.7071067811865463515, 0.000000000000000000 ) ) ;
#115742 = DIRECTION ( 'NONE',  ( -0.000000000000000000, 0.000000000000000000, 1.000000000000000000 ) ) ;
#115743 = VECTOR ( 'NONE', #5708, 1000.000000000000000 ) ;
#115744 = ORIENTED_EDGE ( 'NONE', *, *, #136641, .T. ) ;
#115745 = VERTEX_POINT ( 'NONE', #5980 ) ;
#115746 = EDGE_CURVE ( 'NONE', #9950, #83013, #93751, .T. ) ;
#115747 = CARTESIAN_POINT ( 'NONE',  ( 64.72916666666667140, 7.950000000000001954, -2.130196079827421762 ) ) ;
#115748 = VECTOR ( 'NONE', #114271, 999.9999999999998863 ) ;
#115749 = EDGE_CURVE ( 'NONE', #20953, #134952, #140797, .T. ) ;
#115750 = DIRECTION ( 'NONE',  ( -0.3543493200069162685, -0.000000000000000000, -0.9351131265310288487 ) ) ;
#115751 = FACE_OUTER_BOUND ( 'NONE', #14336, .T. ) ;
#115752 = DIRECTION ( 'NONE',  ( -0.000000000000000000, 0.3543493200069153248, 0.9351131265310292928 ) ) ;
#115753 = CARTESIAN_POINT ( 'NONE',  ( -8.999999999999937828, -3.485240976185084882, -4.108735105802418630 ) ) ;
#115754 = AXIS2_PLACEMENT_3D ( 'NONE', #64595, #75481, #41403 ) ;
#115755 = PLANE ( 'NONE',  #55034 ) ;
#115756 = DIRECTION ( 'NONE',  ( 0.7071067811865487940, 0.7071067811865463515, 0.000000000000000000 ) ) ;
#115757 = VERTEX_POINT ( 'NONE', #50965 ) ;
#115758 = ORIENTED_EDGE ( 'NONE', *, *, #62200, .F. ) ;
#115759 = EDGE_LOOP ( 'NONE', ( #75379, #53959, #69927, #132273 ) ) ;
#115760 = ORIENTED_EDGE ( 'NONE', *, *, #38715, .F. ) ;
#115761 = AXIS2_PLACEMENT_3D ( 'NONE', #13185, #124831, #48012 ) ;
#115762 = EDGE_CURVE ( 'NONE', #120761, #55777, #27054, .T. ) ;
#115763 = CARTESIAN_POINT ( 'NONE',  ( -14.18650864602352080, -15.74070752338411694, 8.904080028138976033 ) ) ;
#115764 =( NAMED_UNIT ( * ) PLANE_ANGLE_UNIT ( ) SI_UNIT ( $, .RADIAN. ) );
#115765 = ORIENTED_EDGE ( 'NONE', *, *, #136290, .F. ) ;
#115766 = CARTESIAN_POINT ( 'NONE',  ( -45.29974487139158867, -27.71228299555237840, 4.000000000000000000 ) ) ;
#115767 = CARTESIAN_POINT ( 'NONE',  ( 5.843876922607536883, -22.22500000000000497, 4.000000000000000000 ) ) ;
#115768 = DIRECTION ( 'NONE',  ( -0.7071067811865487940, 0.7071067811865463515, -0.000000000000000000 ) ) ;
#115769 = DIRECTION ( 'NONE',  ( -0.000000000000000000, 0.000000000000000000, 1.000000000000000000 ) ) ;
#115770 = VECTOR ( 'NONE', #7591, 999.9999999999998863 ) ;
#115771 = DIRECTION ( 'NONE',  ( 0.7071067811865486830, -0.7071067811865464625, -0.000000000000000000 ) ) ;
#115772 = ORIENTED_EDGE ( 'NONE', *, *, #112530, .F. ) ;
#115773 = DIRECTION ( 'NONE',  ( 1.000000000000000000, 0.000000000000000000, 0.000000000000000000 ) ) ;
#115774 = CARTESIAN_POINT ( 'NONE',  ( 0.2917770898304763993, -15.74070752338411694, 19.73771281079097761 ) ) ;
#115775 = EDGE_LOOP ( 'NONE', ( #61993, #36510, #56919, #136230 ) ) ;
#115776 = ORIENTED_EDGE ( 'NONE', *, *, #135797, .F. ) ;
#115777 = ORIENTED_EDGE ( 'NONE', *, *, #37822, .F. ) ;
#115778 = DIRECTION ( 'NONE',  ( 0.6830127018922181881, 0.6830127018922202975, -0.2588190451025214056 ) ) ;
#115779 = VERTEX_POINT ( 'NONE', #128530 ) ;
#115780 = ORIENTED_EDGE ( 'NONE', *, *, #64035, .F. ) ;
#115781 = CARTESIAN_POINT ( 'NONE',  ( 70.43793019189810423, -6.110000000000001208, 1.637169565754158951 ) ) ;
#115783 = VERTEX_POINT ( 'NONE', #117601 ) ;
#115782 = VECTOR ( 'NONE', #35171, 999.9999999999998863 ) ;
#115784 = VECTOR ( 'NONE', #2991, 1000.000000000000000 ) ;
#115785 =( BOUNDED_CURVE ( )  B_SPLINE_CURVE ( 3, ( #64199, #139647, #107679, #117819 ),
 .UNSPECIFIED., .F., .F. ) 
 B_SPLINE_CURVE_WITH_KNOTS ( ( 4, 4 ),
 ( 0.2663372438543387677, 1.570796326794899667 ),
 .UNSPECIFIED. ) 
 CURVE ( )  GEOMETRIC_REPRESENTATION_ITEM ( )  RATIONAL_B_SPLINE_CURVE ( ( 1.000000000000000000, 0.8631550219135049051, 0.8631550219135049051, 1.000000000000000000 ) ) 
 REPRESENTATION_ITEM ( '' )  );
#115786 = DIRECTION ( 'NONE',  ( -0.7071067811865486830, -0.7071067811865464625, 0.000000000000000000 ) ) ;
#115787 = EDGE_CURVE ( 'NONE', #3513, #62344, #137978, .T. ) ;
#115788 = CARTESIAN_POINT ( 'NONE',  ( 24.48921356237309510, -27.52281430457072631, 5.000000000000000000 ) ) ;
#115789 = CARTESIAN_POINT ( 'NONE',  ( 106.1670968585647756, -3.055000000000000160, -5.291415217122921177 ) ) ;
#115790 = PLANE ( 'NONE',  #5480 ) ;
#115791 = EDGE_CURVE ( 'NONE', #39763, #128366, #5279, .T. ) ;
#115792 = PLANE ( 'NONE',  #27748 ) ;
#115794 = CARTESIAN_POINT ( 'NONE',  ( -51.48921356237309510, -27.52281430457091460, 5.000000000000000000 ) ) ;
#115793 = CARTESIAN_POINT ( 'NONE',  ( -16.49999999999988276, -13.91253812416061386, 4.000000000000000000 ) ) ;
#115795 = CARTESIAN_POINT ( 'NONE',  ( -12.75860074219786711, 21.72500000000000142, 5.000000000000000000 ) ) ;
#115796 = VECTOR ( 'NONE', #84685, 1000.000000000000000 ) ;
#115797 = DIRECTION ( 'NONE',  ( -1.000000000000000000, -0.000000000000000000, -0.000000000000000000 ) ) ;
#115798 = EDGE_CURVE ( 'NONE', #134215, #122079, #29194, .T. ) ;
#115799 = ADVANCED_FACE ( 'NONE', ( #41496 ), #95879, .F. ) ;
#115800 = DIRECTION ( 'NONE',  ( -0.7071067811865487940, 0.7071067811865463515, -0.000000000000000000 ) ) ;
#115801 = VECTOR ( 'NONE', #7915, 1000.000000000000000 ) ;
#115803 = ORIENTED_EDGE ( 'NONE', *, *, #143162, .F. ) ;
#115802 = VECTOR ( 'NONE', #110412, 1000.000000000000227 ) ;
#115804 = VERTEX_POINT ( 'NONE', #72767 ) ;
#115805 = VERTEX_POINT ( 'NONE', #126364 ) ;
#115806 = CARTESIAN_POINT ( 'NONE',  ( 114.8500270504628702, -5.819803920172573086, -5.819803920172573086 ) ) ;
#115807 = AXIS2_PLACEMENT_3D ( 'NONE', #39396, #72051, #70628 ) ;
#115808 = VECTOR ( 'NONE', #36725, 1000.000000000000000 ) ;
#115809 = VERTEX_POINT ( 'NONE', #6686 ) ;
#115810 = TOROIDAL_SURFACE ( 'NONE', #78822, 9.000000000000001776, 3.000000000000000000 ) ;
#115811 = STYLED_ITEM ( 'NONE', ( #77805 ), #141893 ) ;
#115812 = VECTOR ( 'NONE', #55222, 1000.000000000000000 ) ;
#115813 = PLANE ( 'NONE',  #32925 ) ;
#115814 = CARTESIAN_POINT ( 'NONE',  ( 114.4583333333333286, 3.974999999999997424, 6.884901960086288852 ) ) ;
#115815 = EDGE_CURVE ( 'NONE', #142125, #37121, #115455, .T. ) ;
#115816 = CARTESIAN_POINT ( 'NONE',  ( -27.48921356237309155, -27.52281430457074762, 5.000000000000000000 ) ) ;
#115817 = ADVANCED_FACE ( 'NONE', ( #16144 ), #60438, .F. ) ;
#115818 = LINE ( 'NONE', #124594, #90391 ) ;
#115819 = ORIENTED_EDGE ( 'NONE', *, *, #81730, .T. ) ;
#115820 = CARTESIAN_POINT ( 'NONE',  ( 51.29974487139158867, -27.71228299555242103, 4.000000000000000000 ) ) ;
#115822 = ORIENTED_EDGE ( 'NONE', *, *, #55548, .F. ) ;
#115821 = VECTOR ( 'NONE', #112370, 1000.000000000000000 ) ;
#115823 = EDGE_CURVE ( 'NONE', #32796, #16078, #61175, .T. ) ;
#115824 = CARTESIAN_POINT ( 'NONE',  ( 26.46290314143521982, -3.967499999999994476, 6.871911579029513106 ) ) ;
#115825 = LINE ( 'NONE', #60818, #81733 ) ;
#115826 = DIRECTION ( 'NONE',  ( -0.6830127018922181881, 0.6830127018922202975, -0.2588190451025214056 ) ) ;
#115827 = FACE_OUTER_BOUND ( 'NONE', #20285, .T. ) ;
#115828 = VERTEX_POINT ( 'NONE', #73437 ) ;
#115829 = EDGE_LOOP ( 'NONE', ( #39967, #108590, #115733, #34757 ) ) ;
#115830 = ORIENTED_EDGE ( 'NONE', *, *, #121336, .F. ) ;
#115832 = VECTOR ( 'NONE', #3559, 999.9999999999998863 ) ;
#115831 = CARTESIAN_POINT ( 'NONE',  ( -38.99451991528749062, 28.92564299267965211, 4.000000000000000000 ) ) ;
#115833 = LINE ( 'NONE', #83250, #139043 ) ;
#115834 = EDGE_CURVE ( 'NONE', #128651, #56450, #140128, .T. ) ;
#115835 = CARTESIAN_POINT ( 'NONE',  ( 28.00000000000002487, -49.14999999999999147, 59.92500000000006111 ) ) ;
#115836 = FACE_OUTER_BOUND ( 'NONE', #72356, .T. ) ;
#115837 = LINE ( 'NONE', #77737, #6854 ) ;
#115838 = DIRECTION ( 'NONE',  ( 0.7071067811865486830, -0.7071067811865464625, -0.000000000000000000 ) ) ;
#115839 = VECTOR ( 'NONE', #37888, 1000.000000000000000 ) ;
#115840 = VECTOR ( 'NONE', #50224, 1000.000000000000227 ) ;
#115841 = DIRECTION ( 'NONE',  ( 0.7071067811865487940, -0.7071067811865463515, 0.000000000000000000 ) ) ;
#115842 = FACE_OUTER_BOUND ( 'NONE', #135387, .T. ) ;
#115843 = PLANE ( 'NONE',  #74329 ) ;
#115844 = CIRCLE ( 'NONE', #2436, 2.055000000000000604 ) ;
#115845 = ORIENTED_EDGE ( 'NONE', *, *, #40735, .F. ) ;
#115846 = LINE ( 'NONE', #15802, #27910 ) ;
#115847 = ADVANCED_FACE ( 'NONE', ( #82889 ), #138699, .T. ) ;
#115849 = VECTOR ( 'NONE', #88816, 1000.000000000000000 ) ;
#115848 = DIRECTION ( 'NONE',  ( 0.000000000000000000, 0.000000000000000000, 1.000000000000000000 ) ) ;
#115850 = ORIENTED_EDGE ( 'NONE', *, *, #96517, .T. ) ;
#115851 = CARTESIAN_POINT ( 'NONE',  ( 0.4892135623730947680, -27.52281430457055578, 5.000000000000000000 ) ) ;
#115853 = ORIENTED_EDGE ( 'NONE', *, *, #67032, .F. ) ;
#115852 = DIRECTION ( 'NONE',  ( -0.000000000000000000, 0.000000000000000000, 1.000000000000000000 ) ) ;
#115854 = ORIENTED_EDGE ( 'NONE', *, *, #63774, .F. ) ;
#115855 = TOROIDAL_SURFACE ( 'NONE', #78876, 25.00000000000002487, 3.000000000000000000 ) ;
#115856 = DIRECTION ( 'NONE',  ( -0.7071067811865487940, 0.7071067811865463515, 0.000000000000000000 ) ) ;
#115857 = EDGE_CURVE ( 'NONE', #4377, #139589, #27770, .T. ) ;
#115859 = EDGE_CURVE ( 'NONE', #89571, #21371, #39385, .T. ) ;
#115858 = DIRECTION ( 'NONE',  ( 0.6830127018922181881, 0.6830127018922202975, -0.2588190451025214056 ) ) ;
#115860 = ORIENTED_EDGE ( 'NONE', *, *, #48765, .T. ) ;
#115861 = LINE ( 'NONE', #114457, #122999 ) ;
#115862 = UNCERTAINTY_MEASURE_WITH_UNIT (LENGTH_MEASURE( 1.000000000000000082E-05 ), #13359, 'distance_accuracy_value', 'NONE');
#115863 = VERTEX_POINT ( 'NONE', #28507 ) ;
#115864 = CARTESIAN_POINT ( 'NONE',  ( -42.18398860626899705, 28.73617430169816700, 5.000000000000000000 ) ) ;
#115865 = LINE ( 'NONE', #16565, #36951 ) ;
#115866 = EDGE_CURVE ( 'NONE', #34536, #112793, #116921, .T. ) ;
#115867 = CARTESIAN_POINT ( 'NONE',  ( 120.9750270504629128, -5.819803920172572198, 5.819803920172572198 ) ) ;
#115868 = DIRECTION ( 'NONE',  ( 0.6830127018922181881, 0.6830127018922202975, -0.2588190451025214056 ) ) ;
#115869 = AXIS2_PLACEMENT_3D ( 'NONE', #114954, #15635, #59922 ) ;
#115870 = CARTESIAN_POINT ( 'NONE',  ( 57.18398860626899705, 28.73617430169827358, 5.000000000000000000 ) ) ;
#115871 = CARTESIAN_POINT ( 'NONE',  ( 20.51159235450331764, 2.500000000000001776, 0.000000000000000000 ) ) ;
#115872 = LINE ( 'NONE', #50648, #70377 ) ;
#115873 = FACE_OUTER_BOUND ( 'NONE', #74491, .T. ) ;
#115875 = VECTOR ( 'NONE', #40002, 1000.000000000000227 ) ;
#115874 = CARTESIAN_POINT ( 'NONE',  ( 34.54123647476855297, 0.000000000000000000, 7.934999999999990727 ) ) ;
#115876 = CARTESIAN_POINT ( 'NONE',  ( 8.582903141435219041, 3.967499999999992699, -6.871911579029513994 ) ) ;
#115877 = CARTESIAN_POINT ( 'NONE',  ( -36.29974487139159578, -27.71228299555231445, 4.000000000000000000 ) ) ;
#115878 = FACE_OUTER_BOUND ( 'NONE', #81569, .T. ) ;
#115879 = CARTESIAN_POINT ( 'NONE',  ( 0.000000000000000000, -4.600000000000013856, 20.40202195861967382 ) ) ;
#115880 = ORIENTED_EDGE ( 'NONE', *, *, #4492, .F. ) ;
#115881 = ORIENTED_EDGE ( 'NONE', *, *, #44872, .T. ) ;
#115882 = CARTESIAN_POINT ( 'NONE',  ( 79.60416666666664298, 2.130196079827422206, 7.950000000000001954 ) ) ;
#115884 = ORIENTED_EDGE ( 'NONE', *, *, #115671, .T. ) ;
#115883 = CARTESIAN_POINT ( 'NONE',  ( 25.40000000000000213, 4.219727177090330628, 4.866784818621353814 ) ) ;
#115885 = ORIENTED_EDGE ( 'NONE', *, *, #27161, .F. ) ;
#115886 = DIRECTION ( 'NONE',  ( 0.7071067811865486830, -0.7071067811865464625, -0.000000000000000000 ) ) ;
#115887 = DIRECTION ( 'NONE',  ( -0.3543493200069162685, -0.000000000000000000, -0.9351131265310288487 ) ) ;
#115888 = AXIS2_PLACEMENT_3D ( 'NONE', #114585, #26873, #15254 ) ;
#115889 = CARTESIAN_POINT ( 'NONE',  ( -19.82816939922339472, -11.24070752338416490, 4.000000000000000000 ) ) ;
#115890 = EDGE_LOOP ( 'NONE', ( #120325, #5728, #91120, #66235 ) ) ;
#115891 = CARTESIAN_POINT ( 'NONE',  ( -39.29974487139159578, -27.71228299555233576, 4.000000000000000000 ) ) ;
#115892 = CARTESIAN_POINT ( 'NONE',  ( 15.05159235450332034, 3.061616997868380183E-16, -2.500000000000001332 ) ) ;
#115893 = CARTESIAN_POINT ( 'NONE',  ( -27.79289321881325847, -14.24070752338414003, 5.000000000000000000 ) ) ;
#115894 = CARTESIAN_POINT ( 'NONE',  ( 21.29974487139158512, -27.71228299555221142, 4.000000000000000000 ) ) ;
#115895 = CARTESIAN_POINT ( 'NONE',  ( 11.27718569542934191, -21.72500000000000853, 5.000000000000000000 ) ) ;
#115896 = CYLINDRICAL_SURFACE ( 'NONE', #95975, 5.968999999999998529 ) ;
#115897 = FILL_AREA_STYLE_COLOUR ( '', #94312 ) ;
#115898 = CARTESIAN_POINT ( 'NONE',  ( -53.99451991528749062, 28.92564299267975869, 4.000000000000000000 ) ) ;
#115899 = VECTOR ( 'NONE', #56044, 1000.000000000000000 ) ;
#115900 = CARTESIAN_POINT ( 'NONE',  ( -48.18398860626899705, 28.73617430169820608, 5.000000000000000000 ) ) ;
#115901 = LINE ( 'NONE', #83320, #29354 ) ;
#115902 = VECTOR ( 'NONE', #41325, 1000.000000000000227 ) ;
#115903 = FACE_OUTER_BOUND ( 'NONE', #55505, .T. ) ;
#115904 = CARTESIAN_POINT ( 'NONE',  ( 25.39999999999999858, -14.29000000000013593, -12.70000000000045404 ) ) ;
#115905 = ORIENTED_EDGE ( 'NONE', *, *, #95606, .F. ) ;
#115906 = ORIENTED_EDGE ( 'NONE', *, *, #132031, .T. ) ;
#115907 = CARTESIAN_POINT ( 'NONE',  ( 113.4587635252314470, 0.000000000000000000, -6.110000000000001208 ) ) ;
#115908 = ORIENTED_EDGE ( 'NONE', *, *, #71713, .F. ) ;
#115909 = EDGE_CURVE ( 'NONE', #71117, #112837, #139165, .T. ) ;
#115910 = LINE ( 'NONE', #39103, #75685 ) ;
#115911 = DIRECTION ( 'NONE',  ( -0.7071067811865486830, -0.7071067811865464625, 0.000000000000000000 ) ) ;
#115912 = ORIENTED_EDGE ( 'NONE', *, *, #85351, .F. ) ;
#115913 = VECTOR ( 'NONE', #128046, 1000.000000000000000 ) ;
#115914 = DIRECTION ( 'NONE',  ( -1.000000000000000000, -0.000000000000000000, -0.000000000000000000 ) ) ;
#115915 = VECTOR ( 'NONE', #117217, 1000.000000000000227 ) ;
#115916 = VECTOR ( 'NONE', #60006, 1000.000000000000000 ) ;
#115917 = CARTESIAN_POINT ( 'NONE',  ( 105.0579301918981230, 6.110000000000000320, -1.637169565754156064 ) ) ;
#115918 = ORIENTED_EDGE ( 'NONE', *, *, #34532, .T. ) ;
#115919 = DIRECTION ( 'NONE',  ( 0.7071067811865487940, 0.7071067811865463515, 0.000000000000000000 ) ) ;
#115920 = ORIENTED_EDGE ( 'NONE', *, *, #99685, .F. ) ;
#115921 = DIRECTION ( 'NONE',  ( -1.000000000000000000, 3.640042140494138811E-14, 0.000000000000000000 ) ) ;
#115922 = VECTOR ( 'NONE', #12447, 1000.000000000000000 ) ;
#115923 = CIRCLE ( 'NONE', #53449, 5.968999999999998529 ) ;
#115924 = DIRECTION ( 'NONE',  ( 0.000000000000000000, 0.000000000000000000, -1.000000000000000000 ) ) ;
#115925 = AXIS2_PLACEMENT_3D ( 'NONE', #111988, #133039, #77927 ) ;
#115926 = COLOUR_RGB ( '', 0.72549020, 0.75294118, 0.79215686) ;
#115927 = CARTESIAN_POINT ( 'NONE',  ( -33.48921356237309510, -27.52281430457078670, 5.000000000000000000 ) ) ;
#115928 = DIRECTION ( 'NONE',  ( 0.000000000000000000, -1.000000000000000000, 0.000000000000000000 ) ) ;
#115929 = VECTOR ( 'NONE', #6860, 1000.000000000000000 ) ;
#115930 = VERTEX_POINT ( 'NONE', #19748 ) ;
#115931 = ORIENTED_EDGE ( 'NONE', *, *, #9175, .F. ) ;
#115932 = EDGE_CURVE ( 'NONE', #46130, #40296, #44397, .T. ) ;
#115933 = ORIENTED_EDGE ( 'NONE', *, *, #14861, .F. ) ;
#115934 = DIRECTION ( 'NONE',  ( 0.000000000000000000, -1.000000000000000000, 0.000000000000000000 ) ) ;
#115935 = ADVANCED_FACE ( 'NONE', ( #129950 ), #55248, .F. ) ;
#115936 = PLANE ( 'NONE',  #114789 ) ;
#115937 = CARTESIAN_POINT ( 'NONE',  ( 10.42123647476855375, -9.717572351234235426E-16, -7.934999999999990727 ) ) ;
#115938 = AXIS2_PLACEMENT_3D ( 'NONE', #119307, #108402, #73684 ) ;
#115939 = FACE_OUTER_BOUND ( 'NONE', #58572, .T. ) ;
#115940 = SURFACE_STYLE_FILL_AREA ( #59480 ) ;
#115941 = EDGE_LOOP ( 'NONE', ( #139875, #103080, #18917, #51369 ) ) ;
#115943 = VERTEX_POINT ( 'NONE', #74882 ) ;
#115942 = EDGE_CURVE ( 'NONE', #39257, #47204, #88602, .T. ) ;
#115944 = AXIS2_PLACEMENT_3D ( 'NONE', #123318, #23982, #68246 ) ;
#115945 = CARTESIAN_POINT ( 'NONE',  ( -39.18398860626899705, 28.73617430169814568, 5.000000000000000000 ) ) ;
#115946 = VERTEX_POINT ( 'NONE', #33519 ) ;
#115947 = ORIENTED_EDGE ( 'NONE', *, *, #95007, .F. ) ;
#115948 = VECTOR ( 'NONE', #102709, 999.9999999999998863 ) ;
#115949 = CARTESIAN_POINT ( 'NONE',  ( 112.3495968585647802, 6.109999999999996767, 1.637169565754163836 ) ) ;
#115950 = EDGE_CURVE ( 'NONE', #120720, #91343, #100182, .T. ) ;
#115951 = AXIS2_PLACEMENT_3D ( 'NONE', #43078, #65567, #56112 ) ;
#115952 = VECTOR ( 'NONE', #192, 1000.000000000000000 ) ;
#115953 = CARTESIAN_POINT ( 'NONE',  ( -12.70710678118645909, 17.25929247661554200, 5.000000000000000000 ) ) ;
#115954 = LINE ( 'NONE', #18048, #109667 ) ;
#115955 = EDGE_LOOP ( 'NONE', ( #16484, #118998, #2737, #49126 ) ) ;
#115956 = CARTESIAN_POINT ( 'NONE',  ( 2.292986735706931345, -21.74070752338405654, 4.999753212805221558 ) ) ;
#115957 = VECTOR ( 'NONE', #12051, 1000.000000000000000 ) ;
#115958 = CARTESIAN_POINT ( 'NONE',  ( 26.29298673570676215, -21.74070752338406365, 4.999753212805220670 ) ) ;
#115959 = LINE ( 'NONE', #16663, #32149 ) ;
#115960 = EDGE_CURVE ( 'NONE', #1441, #58822, #65434, .T. ) ;
#115961 = VECTOR ( 'NONE', #1570, 1000.000000000000000 ) ;
#115962 = DIRECTION ( 'NONE',  ( 0.000000000000000000, -1.000000000000000000, 0.000000000000000000 ) ) ;
#115963 = EDGE_LOOP ( 'NONE', ( #81024, #40224, #129351, #101023 ) ) ;
#115964 = FACE_BOUND ( 'NONE', #59128, .T. ) ;
#115965 = ORIENTED_EDGE ( 'NONE', *, *, #90285, .F. ) ;
#115966 = LINE ( 'NONE', #16670, #48083 ) ;
#115967 = CARTESIAN_POINT ( 'NONE',  ( 1.369266385878517678, 0.000000000000000000, -4.607329295533711289 ) ) ;
#115968 = PRESENTATION_LAYER_ASSIGNMENT (  '', '', ( #32606 ) ) ;
#115969 = ORIENTED_EDGE ( 'NONE', *, *, #104200, .F. ) ;
#115970 = LINE ( 'NONE', #13796, #45846 ) ;
#115971 = EDGE_LOOP ( 'NONE', ( #77652, #125956, #106876, #66592 ) ) ;
#115972 = ORIENTED_EDGE ( 'NONE', *, *, #95185, .T. ) ;
#115973 = EDGE_CURVE ( 'NONE', #101734, #111455, #108866, .T. ) ;
#115974 = EDGE_LOOP ( 'NONE', ( #18495, #15721, #55251, #40683 ) ) ;
#115975 = CARTESIAN_POINT ( 'NONE',  ( 42.49543019189810877, 5.291415217122916737, 3.055000000000001936 ) ) ;
#115976 = ORIENTED_EDGE ( 'NONE', *, *, #72932, .F. ) ;
#115977 = CONICAL_SURFACE ( 'NONE', #53510, 2.500000000000000444, 0.9599310885968830309 ) ;
#115978 = CARTESIAN_POINT ( 'NONE',  ( 18.79333936457835108, 21.75929247661549937, 4.998822639870708073 ) ) ;
#115979 = DIRECTION ( 'NONE',  ( -1.000000000000000000, -1.224606353822377258E-16, -0.000000000000000000 ) ) ;
#115980 = DIRECTION ( 'NONE',  ( -0.7071067811865486830, -0.7071067811865464625, 0.000000000000000000 ) ) ;
#115981 = EDGE_CURVE ( 'NONE', #88273, #133448, #99428, .T. ) ;
#115982 = LINE ( 'NONE', #80549, #56121 ) ;
#115983 = AXIS2_PLACEMENT_3D ( 'NONE', #136076, #46995, #114322 ) ;
#115984 = VECTOR ( 'NONE', #66512, 1000.000000000000227 ) ;
#115985 = FACE_OUTER_BOUND ( 'NONE', #25380, .T. ) ;
#115986 = EDGE_CURVE ( 'NONE', #98221, #98945, #119057, .T. ) ;
#115987 = EDGE_CURVE ( 'NONE', #118822, #28861, #108152, .T. ) ;
#115988 = DIRECTION ( 'NONE',  ( 0.7071067811865487940, 0.7071067811865463515, 0.000000000000000000 ) ) ;
#115989 = DIRECTION ( 'NONE',  ( -0.6830127018922181881, 0.6830127018922202975, -0.2588190451025214056 ) ) ;
#115990 = DIRECTION ( 'NONE',  ( 0.7071067811865486830, -0.7071067811865464625, -0.000000000000000000 ) ) ;
#115991 = LINE ( 'NONE', #70427, #72634 ) ;
#115992 = VECTOR ( 'NONE', #65048, 1000.000000000000114 ) ;
#115993 = ORIENTED_EDGE ( 'NONE', *, *, #100100, .T. ) ;
#115994 = EDGE_LOOP ( 'NONE', ( #100916, #74185, #75204, #90390 ) ) ;
#115995 = ORIENTED_EDGE ( 'NONE', *, *, #111228, .T. ) ;
#115996 = AXIS2_PLACEMENT_3D ( 'NONE', #14408, #3496, #47789 ) ;
#115997 = EDGE_LOOP ( 'NONE', ( #124283, #75457, #95758, #14448 ) ) ;
#115998 = FACE_OUTER_BOUND ( 'NONE', #129982, .T. ) ;
#115999 = ORIENTED_EDGE ( 'NONE', *, *, #109562, .F. ) ;
#116000 = ADVANCED_FACE ( 'NONE', ( #8817 ), #54548, .F. ) ;
#116001 = VERTEX_POINT ( 'NONE', #98725 ) ;
#116002 = CYLINDRICAL_SURFACE ( 'NONE', #123146, 0.5000000000000004441 ) ;
#116003 = DIRECTION ( 'NONE',  ( -0.000000000000000000, -0.000000000000000000, 1.000000000000000000 ) ) ;
#116004 = ADVANCED_FACE ( 'NONE', ( #42957 ), #53075, .F. ) ;
#116005 = EDGE_CURVE ( 'NONE', #49326, #140411, #22568, .T. ) ;
#116006 = CARTESIAN_POINT ( 'NONE',  ( 19.36246187583889977, 22.22499999999999432, 4.000000000000000000 ) ) ;
#116007 = ORIENTED_EDGE ( 'NONE', *, *, #116236, .T. ) ;
#116008 = FACE_OUTER_BOUND ( 'NONE', #101510, .T. ) ;
#116009 = AXIS2_PLACEMENT_3D ( 'NONE', #113227, #69781, #25505 ) ;
#116010 = EDGE_LOOP ( 'NONE', ( #138175, #39744, #69678, #118470, #14725 ) ) ;
#116011 = DIRECTION ( 'NONE',  ( -0.7071067811865486830, -0.7071067811865464625, 0.000000000000000000 ) ) ;
#116012 = CARTESIAN_POINT ( 'NONE',  ( 34.49999999999975131, 9.054329344830847504, 4.994342998332164107 ) ) ;
#116013 = CARTESIAN_POINT ( 'NONE',  ( -1.099596858564781066, -7.934999999999989839, 2.126176841940957907 ) ) ;
#116014 = ORIENTED_EDGE ( 'NONE', *, *, #120968, .T. ) ;
#116016 = DIRECTION ( 'NONE',  ( 0.3543493200069162685, -0.000000000000000000, -0.9351131265310288487 ) ) ;
#116015 = CARTESIAN_POINT ( 'NONE',  ( 104.6204301918981230, 3.055000000000002380, -5.291415217122917625 ) ) ;
#116017 = EDGE_CURVE ( 'NONE', #115415, #110261, #11696, .T. ) ;
#116018 = PLANE ( 'NONE',  #339 ) ;
#116019 = DIRECTION ( 'NONE',  ( 0.7071067811865487940, 0.7071067811865463515, -0.000000000000000000 ) ) ;
#116020 = EDGE_LOOP ( 'NONE', ( #91686, #121682, #62548, #125528, #1308 ) ) ;
#116021 = ORIENTED_EDGE ( 'NONE', *, *, #54144, .T. ) ;
#116022 = PLANE ( 'NONE',  #28766 ) ;
#116023 = EDGE_LOOP ( 'NONE', ( #104608, #78476, #5175, #21431 ) ) ;
#116024 = DIRECTION ( 'NONE',  ( -1.000000000000000000, 1.451651444332056451E-15, 0.000000000000000000 ) ) ;
#116025 = LINE ( 'NONE', #83435, #32433 ) ;
#116026 = PLANE ( 'NONE',  #142299 ) ;
#116028 = ADVANCED_FACE ( 'NONE', ( #86456 ), #87153, .F. ) ;
#116027 = AXIS2_PLACEMENT_3D ( 'NONE', #141357, #10818, #88429 ) ;
#116029 = FACE_OUTER_BOUND ( 'NONE', #100679, .T. ) ;
#116030 = CARTESIAN_POINT ( 'NONE',  ( 183.3316408629057150, -49.14999999999996305, -41.64500000000001734 ) ) ;
#116032 = ORIENTED_EDGE ( 'NONE', *, *, #132967, .T. ) ;
#116031 =( BOUNDED_CURVE ( )  B_SPLINE_CURVE ( 3, ( #139678, #71545, #62102, #106261 ),
 .UNSPECIFIED., .F., .F. ) 
 B_SPLINE_CURVE_WITH_KNOTS ( ( 4, 4 ),
 ( 1.739935637444958161, 1.766022064991929152 ),
 .UNSPECIFIED. ) 
 CURVE ( )  GEOMETRIC_REPRESENTATION_ITEM ( )  RATIONAL_B_SPLINE_CURVE ( ( 1.000000000000000000, 0.9999432923287778774, 0.9999432923287778774, 1.000000000000000000 ) ) 
 REPRESENTATION_ITEM ( '' )  );
#116033 = CIRCLE ( 'NONE', #97509, 6.499999999999999112 ) ;
#116034 = FACE_OUTER_BOUND ( 'NONE', #70713, .T. ) ;
#116035 = VECTOR ( 'NONE', #53207, 1000.000000000000227 ) ;
#116036 = LINE ( 'NONE', #38502, #48810 ) ;
#116037 = DIRECTION ( 'NONE',  ( -0.000000000000000000, -0.3543493200069152693, 0.9351131265310292928 ) ) ;
#116038 = EDGE_LOOP ( 'NONE', ( #140871, #39371, #78950, #59964 ) ) ;
#116039 = FACE_OUTER_BOUND ( 'NONE', #39677, .T. ) ;
#116040 = AXIS2_PLACEMENT_3D ( 'NONE', #110153, #55819, #94112 ) ;
#116041 = AXIS2_PLACEMENT_3D ( 'NONE', #143184, #109122, #87389 ) ;
#116042 = VECTOR ( 'NONE', #8678, 1000.000000000000000 ) ;
#116043 = VECTOR ( 'NONE', #124520, 1000.000000000000000 ) ;
#116044 = CARTESIAN_POINT ( 'NONE',  ( 0.005480084712502889671, 28.92564299267938210, 4.000000000000000000 ) ) ;
#116046 = VERTEX_POINT ( 'NONE', #119746 ) ;
#116045 = VECTOR ( 'NONE', #76292, 1000.000000000000227 ) ;
#116048 = EDGE_LOOP ( 'NONE', ( #93019, #106750, #39309, #57051, #102179 ) ) ;
#116047 = CARTESIAN_POINT ( 'NONE',  ( 0.000000000000000000, -49.85820393249936444, -34.92499999999998295 ) ) ;
#116049 = ORIENTED_EDGE ( 'NONE', *, *, #43035, .F. ) ;
#116050 = DIRECTION ( 'NONE',  ( 0.7071067811865486830, -0.7071067811865464625, -0.000000000000000000 ) ) ;
#116051 = AXIS2_PLACEMENT_3D ( 'NONE', #45374, #66389, #33773 ) ;
#116052 = CARTESIAN_POINT ( 'NONE',  ( -34.92500000000001137, -19.19990548397260000, 4.759050581649338696 ) ) ;
#116053 = ORIENTED_EDGE ( 'NONE', *, *, #89951, .T. ) ;
#116054 = LINE ( 'NONE', #26216, #72013 ) ;
#116055 = UNCERTAINTY_MEASURE_WITH_UNIT (LENGTH_MEASURE( 1.000000000000000082E-05 ), #44317, 'distance_accuracy_value', 'NONE');
#116056 = EDGE_CURVE ( 'NONE', #38115, #751, #66138, .T. ) ;
#116057 = CARTESIAN_POINT ( 'NONE',  ( 27.48921356237309155, -27.52281430457074762, 5.000000000000000000 ) ) ;
#116058 = EDGE_CURVE ( 'NONE', #25180, #99905, #120448, .T. ) ;
#116059 =( LENGTH_UNIT ( ) NAMED_UNIT ( * ) SI_UNIT ( .MILLI., .METRE. ) );
#116060 = ORIENTED_EDGE ( 'NONE', *, *, #133450, .T. ) ;
#116061 = AXIS2_PLACEMENT_3D ( 'NONE', #101902, #118479, #27185 ) ;
#116062 = DIRECTION ( 'NONE',  ( 1.000000000000000000, 1.224606353822377258E-16, 0.000000000000000000 ) ) ;
#116063 = LINE ( 'NONE', #18147, #69783 ) ;
#116064 = CARTESIAN_POINT ( 'NONE',  ( -47.99451991528749062, 28.92564299267971251, 4.000000000000000000 ) ) ;
#116065 = CARTESIAN_POINT ( 'NONE',  ( 2.333333333333333481, 5.278424836066143655, -3.047499999999997655 ) ) ;
#116066 =( LENGTH_UNIT ( ) NAMED_UNIT ( * ) SI_UNIT ( .MILLI., .METRE. ) );
#116067 = DIRECTION ( 'NONE',  ( -1.000000000000000000, -1.224606353822377258E-16, -0.000000000000000000 ) ) ;
#116068 = CARTESIAN_POINT ( 'NONE',  ( -9.328169399223463998, -3.740707523384244837, 4.000000000000000000 ) ) ;
#116069 = FACE_OUTER_BOUND ( 'NONE', #10931, .T. ) ;
#116070 = DIRECTION ( 'NONE',  ( 0.6830127018922181881, 0.6830127018922202975, -0.2588190451025214056 ) ) ;
#116071 = ORIENTED_EDGE ( 'NONE', *, *, #79276, .F. ) ;
#116072 = VECTOR ( 'NONE', #31139, 1000.000000000000000 ) ;
#116073 = ORIENTED_EDGE ( 'NONE', *, *, #76462, .T. ) ;
#116074 = ORIENTED_EDGE ( 'NONE', *, *, #124626, .F. ) ;
#116075 = CARTESIAN_POINT ( 'NONE',  ( 116.7916666666666714, 3.975000000000003642, -6.884901960086285300 ) ) ;
#116076 = VECTOR ( 'NONE', #128109, 1000.000000000000000 ) ;
#116077 = VERTEX_POINT ( 'NONE', #89297 ) ;
#116078 = ORIENTED_EDGE ( 'NONE', *, *, #115791, .T. ) ;
#116079 = VERTEX_POINT ( 'NONE', #58868 ) ;
#116080 = FACE_OUTER_BOUND ( 'NONE', #97732, .T. ) ;
#116081 = LINE ( 'NONE', #106607, #94842 ) ;
#116082 = VERTEX_POINT ( 'NONE', #134971 ) ;
#116083 = PLANE ( 'NONE',  #9145 ) ;
#116084 = CARTESIAN_POINT ( 'NONE',  ( 1.961882696559495765, 22.22500000000000142, 18.97781875781104333 ) ) ;
#116085 = DIRECTION ( 'NONE',  ( -0.7071067811865486830, -0.7071067811865464625, 0.000000000000000000 ) ) ;
#116086 = DIRECTION ( 'NONE',  ( 0.000000000000000000, 0.000000000000000000, 1.000000000000000000 ) ) ;
#116087 = CARTESIAN_POINT ( 'NONE',  ( 116.0837635252314470, -6.110000000000001208, -3.741295971395164515E-16 ) ) ;
#116088 = VECTOR ( 'NONE', #51202, 1000.000000000000000 ) ;
#116089 = ORIENTED_EDGE ( 'NONE', *, *, #48883, .T. ) ;
#116090 = CARTESIAN_POINT ( 'NONE',  ( -16.15228161756845893, 1.822542437158885642, -33.22373175091470188 ) ) ;
#116091 = DIRECTION ( 'NONE',  ( -0.000000000000000000, -0.3543493200069152693, 0.9351131265310292928 ) ) ;
#116092 = LINE ( 'NONE', #71196, #45113 ) ;
#116093 = DIRECTION ( 'NONE',  ( -0.000000000000000000, 0.3543493200069153248, 0.9351131265310292928 ) ) ;
#116094 = DIRECTION ( 'NONE',  ( -1.000000000000000000, -0.000000000000000000, -0.000000000000000000 ) ) ;
#116095 = LINE ( 'NONE', #128425, #35345 ) ;
#116096 = CARTESIAN_POINT ( 'NONE',  ( 33.47502705046289151, -5.819803920172572198, 5.819803920172572198 ) ) ;
#116097 = CARTESIAN_POINT ( 'NONE',  ( 27.29974487139158512, -27.71228299555225405, 4.000000000000000000 ) ) ;
#116098 = PLANE ( 'NONE',  #60018 ) ;
#116099 = EDGE_LOOP ( 'NONE', ( #127594, #58290, #125504, #133105 ) ) ;
#116100 = EDGE_LOOP ( 'NONE', ( #40072, #95762, #25233, #55559 ) ) ;
#116101 = CARTESIAN_POINT ( 'NONE',  ( 32.93749999999999289, 5.819803920172573974, -5.819803920172572198 ) ) ;
#116102 = EDGE_LOOP ( 'NONE', ( #120407, #140694, #95237, #124046, #127785 ) ) ;
#116103 = CARTESIAN_POINT ( 'NONE',  ( -17.51078643762690845, -27.52281430457043143, 5.000000000000000000 ) ) ;
#116104 = ADVANCED_FACE ( 'NONE', ( #123378 ), #103702, .F. ) ;
#116105 = ADVANCED_FACE ( 'NONE', ( #25444 ), #45119, .T. ) ;
#116106 = VECTOR ( 'NONE', #70534, 1000.000000000000000 ) ;
#116107 = CARTESIAN_POINT ( 'NONE',  ( -26.99999999999981526, -18.41253812416056945, 4.000000000000000000 ) ) ;
#116108 = VERTEX_POINT ( 'NONE', #35670 ) ;
#116109 = VECTOR ( 'NONE', #8847, 1000.000000000000000 ) ;
#116110 = CARTESIAN_POINT ( 'NONE',  ( 34.49999999999975842, -19.53574439159931231, 4.994342998332164107 ) ) ;
#116111 = SURFACE_SIDE_STYLE ('',( #61767 ) ) ;
#116112 = DIRECTION ( 'NONE',  ( 0.000000000000000000, 0.000000000000000000, 1.000000000000000000 ) ) ;
#116113 = CARTESIAN_POINT ( 'NONE',  ( 184.1500000000000057, -57.15000000000008384, -34.92499999999998295 ) ) ;
#116114 = CARTESIAN_POINT ( 'NONE',  ( 30.04209685856476497, 5.291415217122923842, -3.054999999999996163 ) ) ;
#116115 = ORIENTED_EDGE ( 'NONE', *, *, #59276, .T. ) ;
#116116 = AXIS2_PLACEMENT_3D ( 'NONE', #13647, #134775, #3481 ) ;
#116117 = DIRECTION ( 'NONE',  ( -0.7071067811865486830, -0.7071067811865464625, 0.000000000000000000 ) ) ;
#116118 = ORIENTED_EDGE ( 'NONE', *, *, #34550, .F. ) ;
#116119 = CIRCLE ( 'NONE', #90689, 2.552699999999928693 ) ;
#116120 = FACE_OUTER_BOUND ( 'NONE', #41141, .T. ) ;
#116121 = CARTESIAN_POINT ( 'NONE',  ( -23.52663903635771092, -5.240707523384225297, 16.25846745537490179 ) ) ;
#116122 = LINE ( 'NONE', #97956, #72241 ) ;
#116123 = EDGE_CURVE ( 'NONE', #106215, #79257, #62796, .T. ) ;
#116124 = CARTESIAN_POINT ( 'NONE',  ( 62.39583333333332149, -2.130196079827427091, 7.949999999999998401 ) ) ;
#116125 = EDGE_LOOP ( 'NONE', ( #110627, #1358, #135427, #14969, #91574 ) ) ;
#116126 = CARTESIAN_POINT ( 'NONE',  ( 53.66709685856477563, -3.055000000000000160, -5.291415217122921177 ) ) ;
#116127 = EDGE_CURVE ( 'NONE', #88880, #49293, #2620, .T. ) ;
#116128 = EDGE_CURVE ( 'NONE', #80339, #84583, #90744, .T. ) ;
#116129 = ORIENTED_EDGE ( 'NONE', *, *, #70450, .F. ) ;
#116130 = CARTESIAN_POINT ( 'NONE',  ( 0.000000000000000000, 0.000000000000000000, 5.000000000000000000 ) ) ;
#116131 = DIRECTION ( 'NONE',  ( -0.7071067811865486830, 0.7071067811865464625, 0.000000000000000000 ) ) ;
#116132 = CARTESIAN_POINT ( 'NONE',  ( 11.56505274454301357, 2.500000000000000444, 0.000000000000000000 ) ) ;
#116133 = DIRECTION ( 'NONE',  ( -0.7071067811865486830, -0.7071067811865464625, 0.000000000000000000 ) ) ;
#116134 = AXIS2_PLACEMENT_3D ( 'NONE', #101846, #134494, #57662 ) ;
#116135 = EDGE_CURVE ( 'NONE', #1016, #98487, #92128, .T. ) ;
#116136 = ADVANCED_FACE ( 'NONE', ( #34932 ), #125501, .F. ) ;
#116137 = CARTESIAN_POINT ( 'NONE',  ( 46.43293019189811588, 1.637169565754156508, 6.110000000000000320 ) ) ;
#116138 = ORIENTED_EDGE ( 'NONE', *, *, #70760, .T. ) ;
#116139 = CARTESIAN_POINT ( 'NONE',  ( -9.792893218813388145, 3.759292476615671230, 5.000000000000000000 ) ) ;
#116140 = EDGE_CURVE ( 'NONE', #105421, #136452, #122623, .T. ) ;
#116141 = DIRECTION ( 'NONE',  ( 0.000000000000000000, -1.000000000000000000, 0.000000000000000000 ) ) ;
#116142 = VERTEX_POINT ( 'NONE', #57401 ) ;
#116143 = ORIENTED_EDGE ( 'NONE', *, *, #15901, .F. ) ;
#116144 = LINE ( 'NONE', #82136, #30758 ) ;
#116145 = VECTOR ( 'NONE', #49761, 1000.000000000000000 ) ;
#116146 = AXIS2_PLACEMENT_3D ( 'NONE', #135654, #102329, #47270 ) ;
#116147 = VERTEX_POINT ( 'NONE', #67574 ) ;
#116148 = STYLED_ITEM ( 'NONE', ( #32964 ), #117596 ) ;
#116149 = EDGE_CURVE ( 'NONE', #128263, #118475, #47277, .T. ) ;
#116150 = CIRCLE ( 'NONE', #86152, 2.500000000000000444 ) ;
#116151 = DIRECTION ( 'NONE',  ( -0.7071067811865486830, 0.7071067811865464625, 0.000000000000000000 ) ) ;
#116152 = VERTEX_POINT ( 'NONE', #1531 ) ;
#116153 = DIRECTION ( 'NONE',  ( -1.000000000000000000, -0.000000000000000000, 0.000000000000000000 ) ) ;
#116154 = EDGE_CURVE ( 'NONE', #104818, #139610, #2243, .T. ) ;
#116155 = VECTOR ( 'NONE', #107680, 1000.000000000000000 ) ;
#116156 = VECTOR ( 'NONE', #107863, 1000.000000000000000 ) ;
#116157 = AXIS2_PLACEMENT_3D ( 'NONE', #19277, #20690, #62088 ) ;
#116158 = CIRCLE ( 'NONE', #120804, 2.500000000000000888 ) ;
#116159 = EDGE_CURVE ( 'NONE', #46535, #98731, #134237, .T. ) ;
#116160 = VECTOR ( 'NONE', #94929, 999.9999999999998863 ) ;
#116161 = CARTESIAN_POINT ( 'NONE',  ( 14.99999999999989875, 13.55218569542902429, 5.000000000000000000 ) ) ;
#116162 = FACE_BOUND ( 'NONE', #15972, .T. ) ;
#116163 = CARTESIAN_POINT ( 'NONE',  ( -8.510786437626906675, -27.52281430457049183, 5.000000000000000000 ) ) ;
#116164 = DIRECTION ( 'NONE',  ( 0.7071067811865487940, 0.7071067811865463515, 0.000000000000000000 ) ) ;
#116165 = DIRECTION ( 'NONE',  ( -0.7071067811865486830, -0.7071067811865464625, 0.000000000000000000 ) ) ;
#116166 = ORIENTED_EDGE ( 'NONE', *, *, #53385, .T. ) ;
#116168 = DIRECTION ( 'NONE',  ( 0.000000000000000000, 0.000000000000000000, -1.000000000000000000 ) ) ;
#116167 = MECHANICAL_DESIGN_GEOMETRIC_PRESENTATION_REPRESENTATION (  '', ( #28219 ), #34853 ) ;
#116170 = ORIENTED_EDGE ( 'NONE', *, *, #80035, .F. ) ;
#116169 = CARTESIAN_POINT ( 'NONE',  ( 0.000000000000000000, -21.72500000000000142, 4.500000000000000888 ) ) ;
#116172 = ORIENTED_EDGE ( 'NONE', *, *, #93148, .T. ) ;
#116171 = EDGE_CURVE ( 'NONE', #61213, #3140, #141286, .T. ) ;
#116173 = DIRECTION ( 'NONE',  ( -0.6830127018922181881, 0.6830127018922202975, -0.2588190451025214056 ) ) ;
#116174 = VERTEX_POINT ( 'NONE', #3668 ) ;
#116175 = VERTEX_POINT ( 'NONE', #13130 ) ;
#116176 = CARTESIAN_POINT ( 'NONE',  ( 67.14126352523145158, 4.472830434245835818, 4.472830434245840259 ) ) ;
#116177 = VERTEX_POINT ( 'NONE', #91450 ) ;
#116178 = CARTESIAN_POINT ( 'NONE',  ( -29.99451991528749417, 28.92564299267958816, 4.000000000000000000 ) ) ;
#116179 = CARTESIAN_POINT ( 'NONE',  ( -30.48921356237309510, -27.52281430457076894, 5.000000000000000000 ) ) ;
#116180 = ADVANCED_FACE ( 'NONE', ( #101581 ), #46555, .F. ) ;
#116181 = EDGE_LOOP ( 'NONE', ( #70353, #97634, #101077, #117966 ) ) ;
#116182 = LINE ( 'NONE', #61150, #137010 ) ;
#116183 = CIRCLE ( 'NONE', #134743, 2.500000000000000444 ) ;
#116184 = EDGE_CURVE ( 'NONE', #79885, #114073, #135663, .T. ) ;
#116185 = VECTOR ( 'NONE', #21303, 1000.000000000000227 ) ;
#116186 = CARTESIAN_POINT ( 'NONE',  ( 11.99999999999992006, -22.06887692260758982, 4.000000000000000000 ) ) ;
#116187 = CARTESIAN_POINT ( 'NONE',  ( 0.000000000000000000, 0.000000000000000000, 5.000000000000000000 ) ) ;
#116188 = DIRECTION ( 'NONE',  ( -0.7071067811865486830, -0.7071067811865464625, 0.000000000000000000 ) ) ;
#116189 = ADVANCED_FACE ( 'NONE', ( #124773 ), #68988, .F. ) ;
#116190 = VECTOR ( 'NONE', #84824, 1000.000000000000000 ) ;
#116191 = CARTESIAN_POINT ( 'NONE',  ( 15.89583333333333393, 1.633150327867687324, -6.094999999999991758 ) ) ;
#116192 = DIRECTION ( 'NONE',  ( -0.6830127018922181881, 0.6830127018922202975, -0.2588190451025214056 ) ) ;
#116193 = EDGE_LOOP ( 'NONE', ( #97184, #81931, #137314, #98312, #56002 ) ) ;
#116194 = ORIENTED_EDGE ( 'NONE', *, *, #60106, .F. ) ;
#116195 = VECTOR ( 'NONE', #28027, 999.9999999999998863 ) ;
#116196 = CARTESIAN_POINT ( 'NONE',  ( 33.32816939922329880, 2.259292476615694323, 4.000000000000000000 ) ) ;
#116197 = CARTESIAN_POINT ( 'NONE',  ( -19.05000000000000071, 3.174999999999997158, 4.000000000000000000 ) ) ;
#116198 = EDGE_LOOP ( 'NONE', ( #11575, #59793, #96397, #125336, #25525 ) ) ;
#116199 = EDGE_CURVE ( 'NONE', #34958, #110351, #17431, .T. ) ;
#116200 = ORIENTED_EDGE ( 'NONE', *, *, #10689, .T. ) ;
#116201 = ORIENTED_EDGE ( 'NONE', *, *, #118976, .T. ) ;
#116202 = DIRECTION ( 'NONE',  ( 0.7071067811865487940, -0.7071067811865463515, 0.000000000000000000 ) ) ;
#116203 =( REPRESENTATION_RELATIONSHIP ('NONE','NONE', #69070, #54265 ) REPRESENTATION_RELATIONSHIP_WITH_TRANSFORMATION ( #80714 )SHAPE_REPRESENTATION_RELATIONSHIP( ) );
#116204 = CARTESIAN_POINT ( 'NONE',  ( 30.45833333333332504, 3.974999999999997424, 6.884901960086288852 ) ) ;
#116205 = ORIENTED_EDGE ( 'NONE', *, *, #36277, .F. ) ;
#116206 = CARTESIAN_POINT ( 'NONE',  ( -8.994519915287490619, 28.92564299267944250, 4.000000000000000000 ) ) ;
#116207 = VECTOR ( 'NONE', #69865, 1000.000000000000227 ) ;
#116208 = CARTESIAN_POINT ( 'NONE',  ( 30.18398860626900060, 28.73617430169808173, 5.000000000000000000 ) ) ;
#116209 = CARTESIAN_POINT ( 'NONE',  ( 12.17123647476855375, 0.000000000000000000, 7.934999999999990727 ) ) ;
#116210 = FACE_OUTER_BOUND ( 'NONE', #64818, .T. ) ;
#116211 = ORIENTED_EDGE ( 'NONE', *, *, #8038, .T. ) ;
#116212 = EDGE_CURVE ( 'NONE', #62156, #136091, #60259, .T. ) ;
#116213 = DIRECTION ( 'NONE',  ( 0.7071067811865486830, -0.7071067811865464625, -0.000000000000000000 ) ) ;
#116214 = AXIS2_PLACEMENT_3D ( 'NONE', #15022, #113628, #81031 ) ;
#116215 = LINE ( 'NONE', #125678, #59126 ) ;
#116217 = ORIENTED_EDGE ( 'NONE', *, *, #117092, .F. ) ;
#116216 = DIRECTION ( 'NONE',  ( -1.000000000000000000, -1.224606353822377258E-16, -0.000000000000000000 ) ) ;
#116219 = VECTOR ( 'NONE', #110702, 1000.000000000000114 ) ;
#116218 = DIRECTION ( 'NONE',  ( -0.000000000000000000, -0.3543493200069152693, 0.9351131265310292928 ) ) ;
#116220 = ORIENTED_EDGE ( 'NONE', *, *, #5979, .F. ) ;
#116221 = CARTESIAN_POINT ( 'NONE',  ( 23.32000000000000028, 9.521314400968980422E-16, 0.000000000000000000 ) ) ;
#116222 = EDGE_CURVE ( 'NONE', #28440, #24958, #63120, .T. ) ;
#116223 = DIRECTION ( 'NONE',  ( 0.000000000000000000, 0.000000000000000000, -1.000000000000000000 ) ) ;
#116224 = CARTESIAN_POINT ( 'NONE',  ( -12.19999999999999929, -59.76999999999998892, -40.00000000000000000 ) ) ;
#116225 = ORIENTED_EDGE ( 'NONE', *, *, #71235, .F. ) ;
#116226 = CARTESIAN_POINT ( 'NONE',  ( 32.99999999999976552, 10.55218569542905982, 5.000000000000000000 ) ) ;
#116227 = CARTESIAN_POINT ( 'NONE',  ( 21.18398860626899349, 28.73617430169802134, 5.000000000000000000 ) ) ;
#116228 = PLANE ( 'NONE',  #25890 ) ;
#116229 = AXIS2_PLACEMENT_3D ( 'NONE', #79189, #87880, #69005 ) ;
#116230 = ORIENTED_EDGE ( 'NONE', *, *, #8288, .F. ) ;
#116231 = DIRECTION ( 'NONE',  ( -0.000000000000000000, -0.3543493200069152693, 0.9351131265310292928 ) ) ;
#116232 = DIRECTION ( 'NONE',  ( -0.7071067811865487940, 0.7071067811865463515, 0.000000000000000000 ) ) ;
#116233 = LINE ( 'NONE', #61194, #79356 ) ;
#116234 = DIRECTION ( 'NONE',  ( 0.000000000000000000, 1.000000000000000000, 0.000000000000000000 ) ) ;
#116235 = ORIENTED_EDGE ( 'NONE', *, *, #17418, .T. ) ;
#116236 = EDGE_CURVE ( 'NONE', #63701, #107149, #6507, .T. ) ;
#116237 = ORIENTED_EDGE ( 'NONE', *, *, #37126, .F. ) ;
#116238 = AXIS2_PLACEMENT_3D ( 'NONE', #31418, #114309, #93273 ) ;
#116239 = CARTESIAN_POINT ( 'NONE',  ( -23.91685193227054640, 21.75929247661549581, 7.311836541447997107 ) ) ;
#116240 = SURFACE_SIDE_STYLE ('',( #72066 ) ) ;
#116241 = CARTESIAN_POINT ( 'NONE',  ( 3.478736474768552078, -5.808823158059033709, 5.808823158059035485 ) ) ;
#116242 = LINE ( 'NONE', #27084, #36621 ) ;
#116243 = EDGE_CURVE ( 'NONE', #82235, #112523, #92848, .T. ) ;
#116244 = DIRECTION ( 'NONE',  ( -0.000000000000000000, 0.000000000000000000, 1.000000000000000000 ) ) ;
#116245 = DIRECTION ( 'NONE',  ( -0.3543493200069162685, -0.000000000000000000, -0.9351131265310288487 ) ) ;
#116246 = CARTESIAN_POINT ( 'NONE',  ( 7.499999999999949374, 15.05218569542901896, 5.000000000000000000 ) ) ;
#116247 = ORIENTED_EDGE ( 'NONE', *, *, #38294, .T. ) ;
#116248 = FACE_OUTER_BOUND ( 'NONE', #3033, .T. ) ;
#116249 = CARTESIAN_POINT ( 'NONE',  ( 63.18398860626900415, 28.73617430169831621, 5.000000000000000000 ) ) ;
#116250 = DIRECTION ( 'NONE',  ( 0.7071067811865487940, 0.7071067811865463515, 0.000000000000000000 ) ) ;
#116251 = VECTOR ( 'NONE', #79375, 1000.000000000000000 ) ;
#116252 = VECTOR ( 'NONE', #124532, 1000.000000000000000 ) ;
#116253 = CARTESIAN_POINT ( 'NONE',  ( 0.000000000000000000, 0.000000000000000000, 5.000000000000000000 ) ) ;
#116254 = CARTESIAN_POINT ( 'NONE',  ( 42.78709685856478728, 3.054999999999997939, 5.291415217122920289 ) ) ;
#116255 = CARTESIAN_POINT ( 'NONE',  ( 183.3316408629057435, -52.14999999999999147, -41.64500000000001023 ) ) ;
#116256 = TOROIDAL_SURFACE ( 'NONE', #56071, 9.000000000000001776, 3.000000000000000000 ) ;
#116257 = ADVANCED_FACE ( 'NONE', ( #137814 ), #116018, .F. ) ;
#116258 = ORIENTED_EDGE ( 'NONE', *, *, #39956, .T. ) ;
#116259 = CARTESIAN_POINT ( 'NONE',  ( 0.005480084712502889671, 28.92564299267938210, 4.000000000000000000 ) ) ;
#116260 = EDGE_LOOP ( 'NONE', ( #22477, #141038, #117500, #119496 ) ) ;
#116261 = ORIENTED_EDGE ( 'NONE', *, *, #108913, .T. ) ;
#116262 = AXIS2_PLACEMENT_3D ( 'NONE', #103259, #114145, #23569 ) ;
#116263 = AXIS2_PLACEMENT_3D ( 'NONE', #118396, #74204, #64041 ) ;
#116264 = LINE ( 'NONE', #115498, #1455 ) ;
#116265 = CARTESIAN_POINT ( 'NONE',  ( -17.48334561358942807, 22.22500000000000142, 4.500000000000000888 ) ) ;
#116266 = LINE ( 'NONE', #6735, #120581 ) ;
#116267 = FACE_OUTER_BOUND ( 'NONE', #124692, .T. ) ;
#116268 = EDGE_CURVE ( 'NONE', #83399, #37537, #50787, .T. ) ;
#116269 = PLANE ( 'NONE',  #4724 ) ;
#116270 = DIRECTION ( 'NONE',  ( -0.7071067811865486830, 0.7071067811865464625, 0.000000000000000000 ) ) ;
#116271 = ORIENTED_EDGE ( 'NONE', *, *, #23773, .F. ) ;
#116272 = CARTESIAN_POINT ( 'NONE',  ( 12.18398860626900060, 28.73617430169795739, 5.000000000000000000 ) ) ;
#116273 = CARTESIAN_POINT ( 'NONE',  ( -45.18398860626900415, 28.73617430169818832, 5.000000000000000000 ) ) ;
#116274 = CARTESIAN_POINT ( 'NONE',  ( -34.75611968250421313, -15.18706574529247000, 4.955485411084893599 ) ) ;
#116275 = DIRECTION ( 'NONE',  ( -0.6830127018922181881, 0.6830127018922202975, -0.2588190451025214056 ) ) ;
#116276 = CARTESIAN_POINT ( 'NONE',  ( 34.49999999999975842, 6.054329344830883031, 4.994342998332162331 ) ) ;
#116277 = CARTESIAN_POINT ( 'NONE',  ( 67.89169371712955581, 2.130196079827421762, 7.950000000000001066 ) ) ;
#116278 = DIRECTION ( 'NONE',  ( 0.6830127018922181881, 0.6830127018922202975, -0.2588190451025214056 ) ) ;
#116279 = VERTEX_POINT ( 'NONE', #51516 ) ;
#116280 = ORIENTED_EDGE ( 'NONE', *, *, #45221, .F. ) ;
#116281 = CARTESIAN_POINT ( 'NONE',  ( 68.81250000000000000, 5.819803920172571310, 5.819803920172575751 ) ) ;
#116282 = DIRECTION ( 'NONE',  ( 0.000000000000000000, -1.000000000000000000, -2.312964634635742661E-15 ) ) ;
#116283 = DIRECTION ( 'NONE',  ( 0.7071067811865486830, -0.7071067811865464625, -0.000000000000000000 ) ) ;
#116284 = ORIENTED_EDGE ( 'NONE', *, *, #615, .T. ) ;
#116285 = VECTOR ( 'NONE', #42041, 1000.000000000000227 ) ;
#116286 = LINE ( 'NONE', #137346, #37534 ) ;
#116287 = DIRECTION ( 'NONE',  ( -0.7071067811865487940, 0.7071067811865463515, 0.000000000000000000 ) ) ;
#116288 = CARTESIAN_POINT ( 'NONE',  ( 53.66709685856477563, -3.055000000000000160, -5.291415217122921177 ) ) ;
#116289 = AXIS2_PLACEMENT_3D ( 'NONE', #70093, #124418, #48284 ) ;
#116290 = EDGE_CURVE ( 'NONE', #61826, #75931, #40638, .T. ) ;
#116291 = LINE ( 'NONE', #8892, #124375 ) ;
#116292 = ORIENTED_EDGE ( 'NONE', *, *, #128350, .T. ) ;
#116293 = ORIENTED_EDGE ( 'NONE', *, *, #138786, .T. ) ;
#116294 = VECTOR ( 'NONE', #45724, 1000.000000000000114 ) ;
#116295 = PLANE ( 'NONE',  #130285 ) ;
#116296 = SURFACE_STYLE_USAGE ( .BOTH. , #73523 ) ;
#116297 = LINE ( 'NONE', #59797, #85961 ) ;
#116298 = DIRECTION ( 'NONE',  ( 0.000000000000000000, -1.000000000000000000, 0.000000000000000000 ) ) ;
#116299 = LINE ( 'NONE', #84414, #139187 ) ;
#116300 = EDGE_CURVE ( 'NONE', #8017, #79690, #48651, .T. ) ;
#116301 = EDGE_CURVE ( 'NONE', #44113, #60323, #83469, .T. ) ;
#116303 = ORIENTED_EDGE ( 'NONE', *, *, #134173, .F. ) ;
#116302 = CARTESIAN_POINT ( 'NONE',  ( 100.2666937171295700, -7.949999999999998401, 2.130196079827423983 ) ) ;
#116304 = CARTESIAN_POINT ( 'NONE',  ( 22.49999999999985434, 16.18958161055405043, -11.56426086740806269 ) ) ;
#116305 = PLANE ( 'NONE',  #87010 ) ;
#116306 = CARTESIAN_POINT ( 'NONE',  ( 20.51159235450331764, 9.902892378096218942E-16, 0.000000000000000000 ) ) ;
#116307 =( GEOMETRIC_REPRESENTATION_CONTEXT ( 3 ) GLOBAL_UNCERTAINTY_ASSIGNED_CONTEXT ( ( #68168 ) ) GLOBAL_UNIT_ASSIGNED_CONTEXT ( ( #118302, #108123, #31324 ) ) REPRESENTATION_CONTEXT ( 'NONE', 'WORKASPACE' ) );
#116308 = CARTESIAN_POINT ( 'NONE',  ( 24.18398860626899705, 28.73617430169804265, 5.000000000000000000 ) ) ;
#116310 = ORIENTED_EDGE ( 'NONE', *, *, #25966, .T. ) ;
#116309 = EDGE_CURVE ( 'NONE', #87414, #95968, #84163, .T. ) ;
#116311 = ADVANCED_FACE ( 'NONE', ( #29034 ), #102086, .T. ) ;
#116312 = VERTEX_POINT ( 'NONE', #120279 ) ;
#116313 = ADVANCED_FACE ( 'NONE', ( #31888 ), #52891, .F. ) ;
#116314 = FILL_AREA_STYLE ('',( #72143 ) ) ;
#116315 = CARTESIAN_POINT ( 'NONE',  ( 8.510786437626906675, -27.52281430457049183, 5.000000000000000000 ) ) ;
#116316 = ADVANCED_FACE ( 'NONE', ( #20995 ), #109443, .F. ) ;
#116317 = VECTOR ( 'NONE', #101873, 1000.000000000000000 ) ;
#116318 = CARTESIAN_POINT ( 'NONE',  ( 110.1833603837962130, -2.130196079827426203, 7.949999999999996625 ) ) ;
#116319 = CARTESIAN_POINT ( 'NONE',  ( 72.55836038379622721, -7.949999999999996625, -2.130196079827426203 ) ) ;
#116320 = VERTEX_POINT ( 'NONE', #65258 ) ;
#116321 = VERTEX_POINT ( 'NONE', #74706 ) ;
#116322 = VECTOR ( 'NONE', #93269, 1000.000000000000000 ) ;
#116323 = EDGE_CURVE ( 'NONE', #126742, #137862, #110138, .T. ) ;
#116324 = CARTESIAN_POINT ( 'NONE',  ( 63.48921356237309510, -27.52281430457099631, 5.000000000000000000 ) ) ;
#116325 = EDGE_LOOP ( 'NONE', ( #108647, #124619, #34418, #118310 ) ) ;
#116326 = EDGE_CURVE ( 'NONE', #71721, #51167, #10817, .T. ) ;
#116327 = ORIENTED_EDGE ( 'NONE', *, *, #117266, .T. ) ;
#116328 = DIRECTION ( 'NONE',  ( 1.000000000000000000, 0.000000000000000000, 0.000000000000000000 ) ) ;
#116329 = VERTEX_POINT ( 'NONE', #98563 ) ;
#116330 = CARTESIAN_POINT ( 'NONE',  ( 61.76669371712955581, -7.949999999999998401, 2.130196079827423983 ) ) ;
#116331 = DIRECTION ( 'NONE',  ( 0.7071067811865487940, 0.7071067811865463515, -0.000000000000000000 ) ) ;
#116332 = VECTOR ( 'NONE', #130786, 1000.000000000000000 ) ;
#116333 = ADVANCED_FACE ( 'NONE', ( #142789 ), #43481, .F. ) ;
#116334 = FACE_BOUND ( 'NONE', #137423, .T. ) ;
#116335 = SURFACE_STYLE_USAGE ( .BOTH. , #127946 ) ;
#116336 = DIRECTION ( 'NONE',  ( 0.7071067811865487940, 0.7071067811865463515, 0.000000000000000000 ) ) ;
#116337 = AXIS2_PLACEMENT_3D ( 'NONE', #38553, #63197, #63888 ) ;
#116339 = VERTEX_POINT ( 'NONE', #75404 ) ;
#116338 = DIRECTION ( 'NONE',  ( 0.7071067811865487940, 0.7071067811865463515, -0.000000000000000000 ) ) ;
#116340 = EDGE_CURVE ( 'NONE', #94995, #39996, #119577, .T. ) ;
#116341 = CARTESIAN_POINT ( 'NONE',  ( 17.20710678118642889, -17.24070752338410983, 5.000000000000000000 ) ) ;
#116342 = APPLICATION_PROTOCOL_DEFINITION ( 'draft international standard', 'automotive_design', 1998, #106872 ) ;
#116343 = ORIENTED_EDGE ( 'NONE', *, *, #77073, .F. ) ;
#116344 = ORIENTED_EDGE ( 'NONE', *, *, #9925, .T. ) ;
#116345 = CARTESIAN_POINT ( 'NONE',  ( 98.64126352523145158, 4.472830434245835818, 4.472830434245840259 ) ) ;
#116346 = EDGE_LOOP ( 'NONE', ( #81874, #97660, #134472, #107917 ) ) ;
#116347 = CARTESIAN_POINT ( 'NONE',  ( 20.20666063542138247, 21.75929247661549581, 4.998822639870702744 ) ) ;
#116348 = DIRECTION ( 'NONE',  ( 0.7071067811865486830, -0.7071067811865464625, -0.000000000000000000 ) ) ;
#116349 = VECTOR ( 'NONE', #28175, 1000.000000000000000 ) ;
#116350 = AXIS2_PLACEMENT_3D ( 'NONE', #99445, #10999, #119765 ) ;
#116351 = AXIS2_PLACEMENT_3D ( 'NONE', #74264, #92591, #137559 ) ;
#116352 = VECTOR ( 'NONE', #11889, 1000.000000000000000 ) ;
#116353 = CIRCLE ( 'NONE', #76966, 2.500000000000000888 ) ;
#116354 = LINE ( 'NONE', #49702, #72586 ) ;
#116356 = ORIENTED_EDGE ( 'NONE', *, *, #122510, .T. ) ;
#116355 = ADVANCED_FACE ( 'NONE', ( #32620 ), #7966, .T. ) ;
#116357 = CARTESIAN_POINT ( 'NONE',  ( -12.69999999999998153, 3.061616997868383634E-16, -2.500000000000000444 ) ) ;
#116358 = CARTESIAN_POINT ( 'NONE',  ( 8.816011393731004731, 28.73617430169781173, 5.000000000000000000 ) ) ;
#116359 = CARTESIAN_POINT ( 'NONE',  ( 2.510786437626908008, -27.52281430457053446, 5.000000000000000000 ) ) ;
#116361 = CARTESIAN_POINT ( 'NONE',  ( -7.499999999999947597, -15.29013452822855257, 0.3645803511610184455 ) ) ;
#116360 = DIRECTION ( 'NONE',  ( 0.000000000000000000, -1.000000000000000000, 0.000000000000000000 ) ) ;
#116362 = EDGE_CURVE ( 'NONE', #100660, #97392, #52207, .T. ) ;
#116363 = CARTESIAN_POINT ( 'NONE',  ( -13.08100000000000307, 3.174999999999997158, 1.444000000000000394 ) ) ;
#116364 = DIRECTION ( 'NONE',  ( 0.6830127018922181881, 0.6830127018922202975, -0.2588190451025214056 ) ) ;
#116365 = CIRCLE ( 'NONE', #53888, 2.500000000000000888 ) ;
#116366 = VECTOR ( 'NONE', #120909, 1000.000000000000000 ) ;
#116367 = LINE ( 'NONE', #37384, #33025 ) ;
#116368 = ORIENTED_EDGE ( 'NONE', *, *, #95013, .F. ) ;
#116369 = DIRECTION ( 'NONE',  ( -0.000000000000000000, -0.3543493200069152693, 0.9351131265310292928 ) ) ;
#116370 = EDGE_CURVE ( 'NONE', #141239, #132990, #95252, .T. ) ;
#116371 = CARTESIAN_POINT ( 'NONE',  ( -26.99999999999980460, 11.58746187583912324, 4.000000000000000000 ) ) ;
#116372 = EDGE_LOOP ( 'NONE', ( #78564, #142638, #105611, #141714 ) ) ;
#116373 = EDGE_LOOP ( 'NONE', ( #49334, #67549, #21892 ) ) ;
#116374 = VERTEX_POINT ( 'NONE', #85528 ) ;
#116375 = CARTESIAN_POINT ( 'NONE',  ( 47.39626352523143282, 4.472830434245840259, -4.472830434245838482 ) ) ;
#116376 = ORIENTED_EDGE ( 'NONE', *, *, #67747, .T. ) ;
#116377 = VECTOR ( 'NONE', #94482, 1000.000000000000000 ) ;
#116378 = CARTESIAN_POINT ( 'NONE',  ( 17.39997294953710849, 4.461849672132297329, -4.461849672132302658 ) ) ;
#116379 = ORIENTED_EDGE ( 'NONE', *, *, #90380, .F. ) ;
#116380 = EDGE_CURVE ( 'NONE', #2022, #31707, #129764, .T. ) ;
#116381 = LINE ( 'NONE', #84489, #43379 ) ;
#116382 = ORIENTED_EDGE ( 'NONE', *, *, #64691, .T. ) ;
#116383 = CARTESIAN_POINT ( 'NONE',  ( -0.3281693992235228396, 17.25929247661554200, 4.000000000000000000 ) ) ;
#116384 = CARTESIAN_POINT ( 'NONE',  ( -30.18398860626900060, 28.73617430169808173, 5.000000000000000000 ) ) ;
#116386 = ORIENTED_EDGE ( 'NONE', *, *, #136352, .T. ) ;
#116385 = CARTESIAN_POINT ( 'NONE',  ( -45.18398860626900415, 28.73617430169818832, 5.000000000000000000 ) ) ;
#116387 = ORIENTED_EDGE ( 'NONE', *, *, #135745, .F. ) ;
#116388 = CARTESIAN_POINT ( 'NONE',  ( 10.49999999999993605, 10.08746187583913922, 4.000000000000000000 ) ) ;
#116389 = VECTOR ( 'NONE', #106527, 999.9999999999998863 ) ;
#116390 = PLANE ( 'NONE',  #25351 ) ;
#116391 = ORIENTED_EDGE ( 'NONE', *, *, #85453, .T. ) ;
#116392 = LINE ( 'NONE', #51147, #45832 ) ;
#116393 = EDGE_LOOP ( 'NONE', ( #84335, #36967, #78759, #140609 ) ) ;
#116394 = PRODUCT_DEFINITION_SHAPE ( 'NONE', 'NONE',  #143572 ) ;
#116395 = ORIENTED_EDGE ( 'NONE', *, *, #52486, .T. ) ;
#116396 = EDGE_CURVE ( 'NONE', #488, #38295, #19576, .T. ) ;
#116397 = VECTOR ( 'NONE', #75766, 1000.000000000000000 ) ;
#116398 = ORIENTED_EDGE ( 'NONE', *, *, #30537, .T. ) ;
#116399 = ORIENTED_EDGE ( 'NONE', *, *, #82483, .T. ) ;
#116400 = DIRECTION ( 'NONE',  ( 0.7071067811865487940, 0.7071067811865463515, -0.000000000000000000 ) ) ;
#116401 = AXIS2_PLACEMENT_3D ( 'NONE', #38742, #129295, #140201 ) ;
#116402 = AXIS2_PLACEMENT_3D ( 'NONE', #4085, #82435, #92562 ) ;
#116403 = CARTESIAN_POINT ( 'NONE',  ( -31.49999999999977973, 0.4311230773921780335, 4.000000000000000000 ) ) ;
#116404 = CARTESIAN_POINT ( 'NONE',  ( -32.29289321881322650, 17.25929247661554200, 5.000000000000000000 ) ) ;
#116405 = EDGE_CURVE ( 'NONE', #9952, #13889, #51269, .T. ) ;
#116406 = LINE ( 'NONE', #138164, #90279 ) ;
#116407 = ORIENTED_EDGE ( 'NONE', *, *, #107653, .T. ) ;
#116409 = EDGE_CURVE ( 'NONE', #18530, #99520, #63595, .T. ) ;
#116408 = CARTESIAN_POINT ( 'NONE',  ( 1.171830600776462061, -2.240707523384260824, 4.000000000000000000 ) ) ;
#116410 = VERTEX_POINT ( 'NONE', #6986 ) ;
#116411 = LINE ( 'NONE', #139626, #95703 ) ;
#116412 = AXIS2_PLACEMENT_3D ( 'NONE', #44985, #46403, #79756 ) ;
#116413 = CARTESIAN_POINT ( 'NONE',  ( 33.66623647476855297, 7.934999999999990727, -1.457635852685135314E-15 ) ) ;
#116414 = EDGE_CURVE ( 'NONE', #95607, #54775, #96157, .T. ) ;
#116415 = CARTESIAN_POINT ( 'NONE',  ( 8.207106781186491062, 6.759292476615645917, 5.000000000000000000 ) ) ;
#116416 = LINE ( 'NONE', #127276, #129402 ) ;
#116417 = CARTESIAN_POINT ( 'NONE',  ( 15.52000000000000135, 9.521314400968980422E-16, 0.000000000000000000 ) ) ;
#116418 = ORIENTED_EDGE ( 'NONE', *, *, #118996, .F. ) ;
#116419 = VERTEX_POINT ( 'NONE', #107754 ) ;
#116420 = VECTOR ( 'NONE', #58258, 999.9999999999998863 ) ;
#116421 = ORIENTED_EDGE ( 'NONE', *, *, #5312, .F. ) ;
#116422 = CARTESIAN_POINT ( 'NONE',  ( 0.000000000000000000, 0.000000000000000000, 5.000000000000000000 ) ) ;
#116423 = LINE ( 'NONE', #126559, #85945 ) ;
#116424 = FACE_OUTER_BOUND ( 'NONE', #114960, .T. ) ;
#116425 = AXIS2_PLACEMENT_3D ( 'NONE', #26777, #39088, #49284 ) ;
#116426 = LINE ( 'NONE', #17112, #19627 ) ;
#116427 = CARTESIAN_POINT ( 'NONE',  ( -8.673617379884035472E-16, -49.85820393249935023, -34.92499999999999005 ) ) ;
#116428 = CARTESIAN_POINT ( 'NONE',  ( 73.12043019189812298, 3.055000000000002380, -5.291415217122917625 ) ) ;
#116429 = EDGE_CURVE ( 'NONE', #139700, #64622, #23543, .T. ) ;
#116430 = LINE ( 'NONE', #38169, #94962 ) ;
#116431 = CARTESIAN_POINT ( 'NONE',  ( 1.499999999999991784, -16.91253812416058722, 4.000000000000000000 ) ) ;
#116432 = ADVANCED_FACE ( 'NONE', ( #128805 ), #11940, .T. ) ;
#116433 = DIRECTION ( 'NONE',  ( -0.7071067811865487940, 0.7071067811865463515, 0.000000000000000000 ) ) ;
#116434 = CARTESIAN_POINT ( 'NONE',  ( -30.18398860626900060, 28.73617430169808173, 5.000000000000000000 ) ) ;
#116435 = CARTESIAN_POINT ( 'NONE',  ( 34.49999999999975131, 13.08746187583911436, 4.000000000000000000 ) ) ;
#116436 = EDGE_LOOP ( 'NONE', ( #87960, #7195, #59975, #37211 ) ) ;
#116437 = VECTOR ( 'NONE', #119493, 999.9999999999998863 ) ;
#116438 = DIRECTION ( 'NONE',  ( -0.000000000000000000, 0.3543493200069153248, 0.9351131265310292928 ) ) ;
#116439 = ORIENTED_EDGE ( 'NONE', *, *, #48244, .F. ) ;
#116440 = LINE ( 'NONE', #41018, #2124 ) ;
#116442 = ORIENTED_EDGE ( 'NONE', *, *, #73214, .T. ) ;
#116441 = CARTESIAN_POINT ( 'NONE',  ( 11.67183060077639212, 11.25929247661560240, 4.000000000000000000 ) ) ;
#116443 = EDGE_CURVE ( 'NONE', #27577, #74390, #82465, .T. ) ;
#116444 = DIRECTION ( 'NONE',  ( 0.7071067811865487940, -0.7071067811865463515, 0.000000000000000000 ) ) ;
#116445 = CARTESIAN_POINT ( 'NONE',  ( 24.39999999999999858, 1.126161369193132478, 16.41140641659140798 ) ) ;
#116446 = ORIENTED_EDGE ( 'NONE', *, *, #123469, .T. ) ;
#116448 = ORIENTED_EDGE ( 'NONE', *, *, #124711, .T. ) ;
#116447 = AXIS2_PLACEMENT_3D ( 'NONE', #78882, #135408, #81015 ) ;
#116449 = CARTESIAN_POINT ( 'NONE',  ( 9.707106781186476852, -12.74070752338415247, 5.000000000000000000 ) ) ;
#116450 = DIRECTION ( 'NONE',  ( 0.7071067811865487940, 0.7071067811865463515, -0.000000000000000000 ) ) ;
#116451 = CARTESIAN_POINT ( 'NONE',  ( 97.78752705046289861, 0.000000000000000000, -7.949999999999998401 ) ) ;
#116452 = LINE ( 'NONE', #3374, #113467 ) ;
#116453 = EDGE_LOOP ( 'NONE', ( #47556, #1352, #32489, #55597, #131731, #100339 ) ) ;
#116454 = LINE ( 'NONE', #17145, #35323 ) ;
#116455 = DIRECTION ( 'NONE',  ( -0.7071067811865486830, -0.7071067811865464625, 0.000000000000000000 ) ) ;
#116456 = CARTESIAN_POINT ( 'NONE',  ( 21.72916666666667140, -6.094999999999989093, 1.633150327867691765 ) ) ;
#116457 = CARTESIAN_POINT ( 'NONE',  ( 34.82816939922328459, 9.759292476615618384, 4.000000000000000000 ) ) ;
#116458 = VECTOR ( 'NONE', #108711, 1000.000000000000000 ) ;
#116459 = LINE ( 'NONE', #73673, #60676 ) ;
#116460 = ORIENTED_EDGE ( 'NONE', *, *, #17645, .T. ) ;
#116461 = VECTOR ( 'NONE', #59557, 1000.000000000000000 ) ;
#116462 = VECTOR ( 'NONE', #35813, 1000.000000000000227 ) ;
#116463 = CARTESIAN_POINT ( 'NONE',  ( 47.03752705046289151, -9.735942053221456900E-16, 7.949999999999998401 ) ) ;
#116464 = VERTEX_POINT ( 'NONE', #49853 ) ;
#116465 = CARTESIAN_POINT ( 'NONE',  ( 82.10459685856476142, 1.637169565754164946, -6.109999999999999432 ) ) ;
#116466 = CARTESIAN_POINT ( 'NONE',  ( -14.51078643762690490, -27.52281430457045275, 5.000000000000000000 ) ) ;
#116467 = EDGE_CURVE ( 'NONE', #50272, #103277, #95463, .T. ) ;
#116469 = LINE ( 'NONE', #6227, #127980 ) ;
#116468 = AXIS2_PLACEMENT_3D ( 'NONE', #3087, #80674, #48048 ) ;
#116470 = AXIS2_PLACEMENT_3D ( 'NONE', #46865, #68582, #125072 ) ;
#116471 = CARTESIAN_POINT ( 'NONE',  ( 5.816011393731002066, 28.73617430169783304, 5.000000000000000000 ) ) ;
#116472 = VERTEX_POINT ( 'NONE', #107055 ) ;
#116473 = CARTESIAN_POINT ( 'NONE',  ( 11.99999999999992006, 20.96639925780204905, 5.000000000000000000 ) ) ;
#116474 = CARTESIAN_POINT ( 'NONE',  ( -34.92500000000001137, -22.22500000000000142, 4.000000000000000000 ) ) ;
#116475 = CARTESIAN_POINT ( 'NONE',  ( -42.18398860626899705, 28.73617430169816700, 5.000000000000000000 ) ) ;
#116477 = EDGE_LOOP ( 'NONE', ( #18883, #134153, #63478, #48701 ) ) ;
#116476 = DIRECTION ( 'NONE',  ( -0.6830127018922180770, -0.6830127018922204085, -0.2588190451025213501 ) ) ;
#116478 = DIRECTION ( 'NONE',  ( 1.000000000000000000, 0.000000000000000000, 0.000000000000000000 ) ) ;
#116479 = CARTESIAN_POINT ( 'NONE',  ( -34.92500000000001137, 2.718490437204206689, 4.759050581649335143 ) ) ;
#116480 = FILL_AREA_STYLE_COLOUR ( '', #54083 ) ;
#116481 = LINE ( 'NONE', #28774, #40064 ) ;
#116482 = EDGE_LOOP ( 'NONE', ( #130307, #36431, #115016 ) ) ;
#116483 = ORIENTED_EDGE ( 'NONE', *, *, #69567, .F. ) ;
#116484 = EDGE_CURVE ( 'NONE', #48744, #41026, #71591, .T. ) ;
#116485 = CARTESIAN_POINT ( 'NONE',  ( 71.02126352523144703, -4.472830434245839371, -4.472830434245840259 ) ) ;
#116486 = AXIS2_PLACEMENT_3D ( 'NONE', #131418, #33557, #99462 ) ;
#116487 = ORIENTED_EDGE ( 'NONE', *, *, #88666, .F. ) ;
#116488 = EDGE_CURVE ( 'NONE', #72213, #77576, #29482, .T. ) ;
#116489 = FACE_OUTER_BOUND ( 'NONE', #25952, .T. ) ;
#116490 = EDGE_CURVE ( 'NONE', #15277, #57196, #98290, .T. ) ;
#116491 = FACE_OUTER_BOUND ( 'NONE', #104403, .T. ) ;
#116492 = CARTESIAN_POINT ( 'NONE',  ( -54.18398860626899705, 28.73617430169825226, 5.000000000000000000 ) ) ;
#116493 = VERTEX_POINT ( 'NONE', #83923 ) ;
#116494 = EDGE_CURVE ( 'NONE', #88587, #52361, #128118, .T. ) ;
#116495 = LINE ( 'NONE', #6252, #109379 ) ;
#116496 = CARTESIAN_POINT ( 'NONE',  ( -1.499999999999987566, 9.052185695429084689, 5.000000000000000000 ) ) ;
#116497 = CIRCLE ( 'NONE', #54021, 3.000000000000000000 ) ;
#116498 = ORIENTED_EDGE ( 'NONE', *, *, #110385, .F. ) ;
#116499 = VECTOR ( 'NONE', #33689, 999.9999999999998863 ) ;
#116500 = EDGE_CURVE ( 'NONE', #126231, #104004, #62145, .T. ) ;
#116501 = CARTESIAN_POINT ( 'NONE',  ( -0.1839886062690032631, 28.73617430169787568, 5.000000000000000000 ) ) ;
#116502 = CARTESIAN_POINT ( 'NONE',  ( -25.49999999999982236, -19.53360074219753884, 5.000000000000000000 ) ) ;
#116503 = DIRECTION ( 'NONE',  ( 0.7071067811865487940, 0.7071067811865463515, -0.000000000000000000 ) ) ;
#116504 =( BOUNDED_CURVE ( )  B_SPLINE_CURVE ( 2, ( #10188, #65332, #98626, #142858, #12332, #20339, #42143, #87764, #9449, #45022, #53729, #142168, #32690 ),
 .UNSPECIFIED., .F., .F. ) 
 B_SPLINE_CURVE_WITH_KNOTS ( ( 3, 2, 2, 2, 2, 2, 3 ),
 ( 0.6500000000000001332, 0.6583333333333334370, 0.6666666666666667407, 0.6750000000000001554, 0.6833333333333334592, 0.6916666666666667629, 0.7000000000000000666 ),
 .UNSPECIFIED. ) 
 CURVE ( )  GEOMETRIC_REPRESENTATION_ITEM ( )  RATIONAL_B_SPLINE_CURVE ( ( 0.9999999999999995559, 0.9659258262890687563, 1.000000000000000000, 0.9659258262890683122, 1.000000000000000000, 0.9659258262890683122, 1.000000000000000000, 0.9659258262890683122, 1.000000000000000000, 0.9659258262890683122, 1.000000000000000000, 0.9659258262890678681, 1.000000000000000444 ) ) 
 REPRESENTATION_ITEM ( '' )  );
#116505 = ORIENTED_EDGE ( 'NONE', *, *, #134051, .T. ) ;
#116507 = ORIENTED_EDGE ( 'NONE', *, *, #59968, .T. ) ;
#116506 = VECTOR ( 'NONE', #57769, 1000.000000000000000 ) ;
#116508 = EDGE_CURVE ( 'NONE', #26469, #1535, #139198, .T. ) ;
#116509 = EDGE_CURVE ( 'NONE', #48269, #41471, #37737, .T. ) ;
#116510 = LINE ( 'NONE', #17197, #29228 ) ;
#116511 = FACE_OUTER_BOUND ( 'NONE', #54915, .T. ) ;
#116512 = CARTESIAN_POINT ( 'NONE',  ( 25.40000000000000213, -6.224491245752634683, -3.516874333047554479 ) ) ;
#116513 = CARTESIAN_POINT ( 'NONE',  ( -17.70025512860841488, -27.71228299555193786, 4.000000000000000000 ) ) ;
#116514 = EDGE_CURVE ( 'NONE', #39920, #88187, #127584, .T. ) ;
#116515 = VECTOR ( 'NONE', #96866, 999.9999999999998863 ) ;
#116516 = FACE_OUTER_BOUND ( 'NONE', #127617, .T. ) ;
#116517 = ORIENTED_EDGE ( 'NONE', *, *, #102975, .F. ) ;
#116518 = VECTOR ( 'NONE', #60648, 999.9999999999998863 ) ;
#116519 = VERTEX_POINT ( 'NONE', #62346 ) ;
#116520 = ORIENTED_EDGE ( 'NONE', *, *, #111540, .F. ) ;
#116521 = VERTEX_POINT ( 'NONE', #73219 ) ;
#116522 = AXIS2_PLACEMENT_3D ( 'NONE', #23502, #69172, #89474 ) ;
#116523 = FILL_AREA_STYLE ('',( #105615 ) ) ;
#116524 = CYLINDRICAL_SURFACE ( 'NONE', #89109, 17.45000000000002061 ) ;
#116525 = EDGE_LOOP ( 'NONE', ( #97287, #4300, #47591, #79891 ) ) ;
#116526 = CARTESIAN_POINT ( 'NONE',  ( -2.510786437626908008, -27.52281430457053446, 5.000000000000000000 ) ) ;
#116527 = DIRECTION ( 'NONE',  ( -0.000000000000000000, 0.3543493200069153248, 0.9351131265310292928 ) ) ;
#116528 = CARTESIAN_POINT ( 'NONE',  ( 34.49999999999975842, -7.535744391599426883, 4.994342998332164107 ) ) ;
#116529 = EDGE_CURVE ( 'NONE', #77399, #140629, #28843, .T. ) ;
#116530 = DIRECTION ( 'NONE',  ( -0.000000000000000000, 0.3543493200069153248, 0.9351131265310292928 ) ) ;
#116531 = AXIS2_PLACEMENT_3D ( 'NONE', #47560, #15544, #125797 ) ;
#116532 = DIRECTION ( 'NONE',  ( -0.7071067811865487940, 0.7071067811865463515, 0.000000000000000000 ) ) ;
#116533 = EDGE_LOOP ( 'NONE', ( #61797, #123907, #100576, #127625 ) ) ;
#116534 = CARTESIAN_POINT ( 'NONE',  ( -21.79333936457831911, 21.75929247661549226, 4.998822639870701856 ) ) ;
#116535 = DIRECTION ( 'NONE',  ( 0.7071067811865487940, 0.7071067811865463515, 0.000000000000000000 ) ) ;
#116536 = ORIENTED_EDGE ( 'NONE', *, *, #130455, .T. ) ;
#116537 = DIRECTION ( 'NONE',  ( 0.6830127018922181881, 0.6830127018922202975, -0.2588190451025214056 ) ) ;
#116538 = EDGE_LOOP ( 'NONE', ( #87675, #1698, #3857, #98524 ) ) ;
#116539 = VERTEX_POINT ( 'NONE', #103650 ) ;
#116540 = DIRECTION ( 'NONE',  ( 0.000000000000000000, 0.000000000000000000, -1.000000000000000000 ) ) ;
#116541 = EDGE_LOOP ( 'NONE', ( #135711, #85088, #32371, #37572, #1007 ) ) ;
#116542 = ORIENTED_EDGE ( 'NONE', *, *, #85247, .F. ) ;
#116543 = AXIS2_PLACEMENT_3D ( 'NONE', #112042, #2519, #44679 ) ;
#116544 = CARTESIAN_POINT ( 'NONE',  ( 72.77126352523144703, 4.472830434245838482, 4.472830434245842035 ) ) ;
#116545 = VERTEX_POINT ( 'NONE', #70399 ) ;
#116546 = EDGE_CURVE ( 'NONE', #42161, #98060, #5769, .T. ) ;
#116547 = CARTESIAN_POINT ( 'NONE',  ( -31.49999999999977973, -14.56887692260766087, 4.000000000000000000 ) ) ;
#116548 = VECTOR ( 'NONE', #22909, 999.9999999999998863 ) ;
#116549 = CARTESIAN_POINT ( 'NONE',  ( -69.18398860626899705, 28.73617430169835529, 5.000000000000000000 ) ) ;
#116550 = CARTESIAN_POINT ( 'NONE',  ( 111.7087635252314470, -7.482591942790329030E-16, 6.110000000000001208 ) ) ;
#116551 = CARTESIAN_POINT ( 'NONE',  ( -39.48921356237310221, -27.52281430457082934, 5.000000000000000000 ) ) ;
#116552 = EDGE_CURVE ( 'NONE', #113440, #20682, #18057, .T. ) ;
#116553 = DIRECTION ( 'NONE',  ( 0.6830127018922180770, -0.6830127018922204085, -0.2588190451025213501 ) ) ;
#116554 = CARTESIAN_POINT ( 'NONE',  ( -24.48921356237309510, -27.52281430457072631, 5.000000000000000000 ) ) ;
#116555 = DIRECTION ( 'NONE',  ( -0.7071067811865486830, -0.7071067811865464625, 0.000000000000000000 ) ) ;
#116556 = VECTOR ( 'NONE', #129737, 999.9999999999998863 ) ;
#116557 = CARTESIAN_POINT ( 'NONE',  ( 35.22502705046288440, 5.819803920172573974, -5.819803920172573086 ) ) ;
#116558 = CARTESIAN_POINT ( 'NONE',  ( 78.53752705046289861, -9.735942053221456900E-16, 7.949999999999998401 ) ) ;
#116559 = VERTEX_POINT ( 'NONE', #104382 ) ;
#116560 = ADVANCED_FACE ( 'NONE', ( #136305 ), #7187, .F. ) ;
#116561 = ORIENTED_EDGE ( 'NONE', *, *, #128984, .T. ) ;
#116562 = VERTEX_POINT ( 'NONE', #84112 ) ;
#116563 = VECTOR ( 'NONE', #84765, 999.9999999999998863 ) ;
#116564 = PLANE ( 'NONE',  #25564 ) ;
#116565 = FACE_OUTER_BOUND ( 'NONE', #133773, .T. ) ;
#116566 = ORIENTED_EDGE ( 'NONE', *, *, #37440, .F. ) ;
#116567 = LINE ( 'NONE', #105662, #46920 ) ;
#116568 = DIRECTION ( 'NONE',  ( -0.3543493200069162685, -0.000000000000000000, -0.9351131265310288487 ) ) ;
#116569 = EDGE_CURVE ( 'NONE', #112632, #59289, #138466, .T. ) ;
#116570 = DIRECTION ( 'NONE',  ( -0.000000000000000000, 0.000000000000000000, 1.000000000000000000 ) ) ;
#116571 = LINE ( 'NONE', #83235, #50982 ) ;
#116572 = ORIENTED_EDGE ( 'NONE', *, *, #102741, .F. ) ;
#116573 = CARTESIAN_POINT ( 'NONE',  ( 0.2099742459736120836, -51.66308182546811167, 38.35990878063377352 ) ) ;
#116574 = EDGE_LOOP ( 'NONE', ( #108032, #30131, #57330 ) ) ;
#116575 = STYLED_ITEM ( 'NONE', ( #110972 ), #42351 ) ;
#116576 = VECTOR ( 'NONE', #121767, 1000.000000000000227 ) ;
#116577 = CARTESIAN_POINT ( 'NONE',  ( 6.103736474768551190, 5.808823158059036373, 5.808823158059032821 ) ) ;
#116578 = CARTESIAN_POINT ( 'NONE',  ( -21.48921356237309155, -27.52281430457070499, 5.000000000000000000 ) ) ;
#116579 = LINE ( 'NONE', #17263, #27354 ) ;
#116580 = CARTESIAN_POINT ( 'NONE',  ( 10.90898527456939426, -8.448166216745459423, 4.345408460216290791 ) ) ;
#116581 = ORIENTED_EDGE ( 'NONE', *, *, #120662, .F. ) ;
#116582 = ORIENTED_EDGE ( 'NONE', *, *, #89621, .F. ) ;
#116583 = ORIENTED_EDGE ( 'NONE', *, *, #99922, .F. ) ;
#116584 = CARTESIAN_POINT ( 'NONE',  ( -14.29289321881335972, 11.25929247661560240, 5.000000000000000000 ) ) ;
#116585 = CARTESIAN_POINT ( 'NONE',  ( 0.000000000000000000, 0.000000000000000000, 5.000000000000000000 ) ) ;
#116586 = LINE ( 'NONE', #32267, #128434 ) ;
#116587 = FACE_OUTER_BOUND ( 'NONE', #134159, .T. ) ;
#116588 = VECTOR ( 'NONE', #126367, 1000.000000000000000 ) ;
#116589 = PLANE ( 'NONE',  #4240 ) ;
#116590 = DIRECTION ( 'NONE',  ( 0.7071067811865487940, 0.7071067811865463515, -0.000000000000000000 ) ) ;
#116591 = DIRECTION ( 'NONE',  ( 0.7071067811865486830, -0.7071067811865464625, -0.000000000000000000 ) ) ;
#116592 = EDGE_CURVE ( 'NONE', #127118, #43460, #28278, .T. ) ;
#116593 = TOROIDAL_SURFACE ( 'NONE', #70392, 8.000000000000001776, 1.500000000000000000 ) ;
#116594 = DIRECTION ( 'NONE',  ( -0.7071067811865486830, 0.7071067811865464625, 0.000000000000000000 ) ) ;
#116595 = LINE ( 'NONE', #62959, #21112 ) ;
#116596 = ORIENTED_EDGE ( 'NONE', *, *, #118571, .T. ) ;
#116597 = LINE ( 'NONE', #17280, #81125 ) ;
#116598 = LINE ( 'NONE', #17281, #105429 ) ;
#116599 = ORIENTED_EDGE ( 'NONE', *, *, #50552, .F. ) ;
#116600 = AXIS2_PLACEMENT_3D ( 'NONE', #6706, #49587, #38678 ) ;
#116601 = PLANE ( 'NONE',  #8937 ) ;
#116602 = EDGE_CURVE ( 'NONE', #90399, #119015, #72539, .T. ) ;
#116604 = EDGE_LOOP ( 'NONE', ( #29395, #86103, #22177 ) ) ;
#116603 = LINE ( 'NONE', #17964, #23313 ) ;
#116605 = EDGE_CURVE ( 'NONE', #113212, #117294, #26133, .T. ) ;
#116606 = DIRECTION ( 'NONE',  ( -0.7071067811865487940, 0.7071067811865463515, 0.000000000000000000 ) ) ;
#116607 = CARTESIAN_POINT ( 'NONE',  ( 104.9791666666666714, -7.950000000000000178, 2.130196079827424427 ) ) ;
#116608 = ORIENTED_EDGE ( 'NONE', *, *, #36836, .F. ) ;
#116609 = PLANE ( 'NONE',  #97521 ) ;
#116610 = ORIENTED_EDGE ( 'NONE', *, *, #55680, .F. ) ;
#116611 = VECTOR ( 'NONE', #96701, 1000.000000000000114 ) ;
#116612 = LINE ( 'NONE', #126754, #73056 ) ;
#116613 = CARTESIAN_POINT ( 'NONE',  ( 124.9125270504628986, -7.949999999999998401, -4.867971026610728450E-16 ) ) ;
#116615 = AXIS2_PLACEMENT_3D ( 'NONE', #126704, #2049, #103520 ) ;
#116614 = DIRECTION ( 'NONE',  ( -0.6830127018922180770, -0.6830127018922204085, -0.2588190451025213501 ) ) ;
#116616 = CARTESIAN_POINT ( 'NONE',  ( 34.75611968250419892, 17.81293425470720848, 4.955485411084877612 ) ) ;
#116617 = DIRECTION ( 'NONE',  ( 0.7071067811865487940, 0.7071067811865463515, 0.000000000000000000 ) ) ;
#116618 = DIRECTION ( 'NONE',  ( 0.6830127018922180770, -0.6830127018922204085, -0.2588190451025213501 ) ) ;
#116619 = CARTESIAN_POINT ( 'NONE',  ( 41.99451991528749062, 28.92564299267967343, 4.000000000000000000 ) ) ;
#116620 = CARTESIAN_POINT ( 'NONE',  ( 34.24956980810188156, 3.967499999999998916, 6.871911579029510442 ) ) ;
#116621 = CARTESIAN_POINT ( 'NONE',  ( 11.79123647476855297, -9.717572351234235426E-16, -7.934999999999990727 ) ) ;
#116622 = AXIS2_PLACEMENT_3D ( 'NONE', #112658, #55434, #80765 ) ;
#116623 = DIRECTION ( 'NONE',  ( -0.3543493200069162685, -0.000000000000000000, -0.9351131265310288487 ) ) ;
#116624 = PLANE ( 'NONE',  #109157 ) ;
#116625 = CARTESIAN_POINT ( 'NONE',  ( -25.39999999999996305, 0.000000000000000000, 0.000000000000000000 ) ) ;
#116626 = ORIENTED_EDGE ( 'NONE', *, *, #9908, .F. ) ;
#116627 = EDGE_CURVE ( 'NONE', #22742, #50481, #108878, .T. ) ;
#116628 = ORIENTED_EDGE ( 'NONE', *, *, #115687, .T. ) ;
#116629 = CARTESIAN_POINT ( 'NONE',  ( 80.91666666666667140, -6.884901960086287076, -3.975000000000000977 ) ) ;
#116630 = CARTESIAN_POINT ( 'NONE',  ( 31.49999999999977973, -4.796895815300992183, -3.611700055028608247 ) ) ;
#116631 = EDGE_LOOP ( 'NONE', ( #6691, #25272, #136189, #72706, #84165 ) ) ;
#116632 = CARTESIAN_POINT ( 'NONE',  ( 20.29289321881331531, -3.740707523384241728, 5.000000000000000000 ) ) ;
#116633 = CARTESIAN_POINT ( 'NONE',  ( 23.67080628287044064, -3.047499999999997211, -5.278424836066143655 ) ) ;
#116634 = CARTESIAN_POINT ( 'NONE',  ( 29.82919371712955581, -3.975000000000001865, 6.884901960086284411 ) ) ;
#116635 = VERTEX_POINT ( 'NONE', #116701 ) ;
#116636 = DIRECTION ( 'NONE',  ( 0.3543493200069162685, -0.000000000000000000, -0.9351131265310288487 ) ) ;
#116637 = CARTESIAN_POINT ( 'NONE',  ( 50.99451991528749062, 28.92564299267973738, 4.000000000000000000 ) ) ;
#116638 = CARTESIAN_POINT ( 'NONE',  ( -26.81601139373100651, 28.73617430169768738, 5.000000000000000000 ) ) ;
#116639 = DIRECTION ( 'NONE',  ( -0.6830127018922181881, 0.6830127018922202975, -0.2588190451025214056 ) ) ;
#116640 = LINE ( 'NONE', #126110, #137343 ) ;
#116641 = DIRECTION ( 'NONE',  ( -0.000000000000000000, 0.3543493200069153248, 0.9351131265310292928 ) ) ;
#116642 = CARTESIAN_POINT ( 'NONE',  ( -33.48921356237309510, -27.52281430457078670, 5.000000000000000000 ) ) ;
#116643 = FACE_OUTER_BOUND ( 'NONE', #91765, .T. ) ;
#116644 = FACE_OUTER_BOUND ( 'NONE', #142107, .T. ) ;
#116645 = DIRECTION ( 'NONE',  ( 1.000000000000000000, 0.000000000000000000, 0.000000000000000000 ) ) ;
#116646 = CARTESIAN_POINT ( 'NONE',  ( 57.17148983091625780, -47.44491123045354897, 36.62621018406385787 ) ) ;
#116647 = EDGE_LOOP ( 'NONE', ( #137109, #44139, #52848, #82141 ) ) ;
#116648 = EDGE_LOOP ( 'NONE', ( #75600, #142624, #35383, #138447 ) ) ;
#116649 = EDGE_CURVE ( 'NONE', #57318, #115599, #137761, .T. ) ;
#116650 = CARTESIAN_POINT ( 'NONE',  ( 101.5004301918981042, -3.055000000000002380, 5.291415217122920289 ) ) ;
#116651 = ORIENTED_EDGE ( 'NONE', *, *, #61710, .T. ) ;
#116652 = EDGE_CURVE ( 'NONE', #37230, #137445, #39151, .T. ) ;
#116653 = DIRECTION ( 'NONE',  ( -0.3543493200069163240, 0.000000000000000000, 0.9351131265310288487 ) ) ;
#116654 = LINE ( 'NONE', #17341, #61992 ) ;
#116655 = VERTEX_POINT ( 'NONE', #81972 ) ;
#116656 = EDGE_CURVE ( 'NONE', #129709, #56655, #71080, .T. ) ;
#116657 = EDGE_CURVE ( 'NONE', #70306, #36106, #102946, .T. ) ;
#116658 = CARTESIAN_POINT ( 'NONE',  ( -20.93988928955967310, -9.740707523384180888, 10.89222023123385874 ) ) ;
#116660 = AXIS2_PLACEMENT_3D ( 'NONE', #105619, #93349, #92611 ) ;
#116659 = PLANE ( 'NONE',  #48921 ) ;
#116661 = CARTESIAN_POINT ( 'NONE',  ( 101.7037635252314374, 6.109999999999998543, 1.122388791418548911E-15 ) ) ;
#116662 = ORIENTED_EDGE ( 'NONE', *, *, #109610, .T. ) ;
#116663 = CARTESIAN_POINT ( 'NONE',  ( 18.32266436734346726, -2.055000000000000160, 2.789133085058097101E-16 ) ) ;
#116664 = EDGE_LOOP ( 'NONE', ( #21210, #113449, #121555, #95816 ) ) ;
#116665 = LINE ( 'NONE', #17350, #123944 ) ;
#116666 = LINE ( 'NONE', #60915, #79336 ) ;
#116667 = CARTESIAN_POINT ( 'NONE',  ( 17.81601139373099940, 28.73617430169775133, 5.000000000000000000 ) ) ;
#116668 = CARTESIAN_POINT ( 'NONE',  ( 2.671830600776460063, 20.25929247661551713, 4.000000000000000000 ) ) ;
#116669 = ORIENTED_EDGE ( 'NONE', *, *, #108935, .F. ) ;
#116670 = ORIENTED_EDGE ( 'NONE', *, *, #111996, .F. ) ;
#116671 = EDGE_CURVE ( 'NONE', #99825, #83817, #15911, .T. ) ;
#116672 = ORIENTED_EDGE ( 'NONE', *, *, #15290, .F. ) ;
#116673 = LINE ( 'NONE', #94196, #130134 ) ;
#116674 = EDGE_CURVE ( 'NONE', #25493, #52416, #16361, .T. ) ;
#116675 = DIRECTION ( 'NONE',  ( -0.6830127018922181881, 0.6830127018922202975, -0.2588190451025214056 ) ) ;
#116676 = CARTESIAN_POINT ( 'NONE',  ( 9.400403141435219823, -7.934999999999988951, 2.126176841940957907 ) ) ;
#116677 = VECTOR ( 'NONE', #85873, 1000.000000000000227 ) ;
#116678 = DIRECTION ( 'NONE',  ( -0.000000000000000000, -0.3543493200069152693, 0.9351131265310292928 ) ) ;
#116679 = EDGE_CURVE ( 'NONE', #51279, #86186, #40587, .T. ) ;
#116680 = PRESENTATION_STYLE_ASSIGNMENT (( #128287 ) ) ;
#116681 = VECTOR ( 'NONE', #13909, 999.9999999999998863 ) ;
#116682 = ORIENTED_EDGE ( 'NONE', *, *, #128443, .F. ) ;
#116683 = ORIENTED_EDGE ( 'NONE', *, *, #25732, .F. ) ;
#116684 = DIRECTION ( 'NONE',  ( 0.7071067811865487940, 0.7071067811865463515, -0.000000000000000000 ) ) ;
#116685 = ORIENTED_EDGE ( 'NONE', *, *, #142409, .F. ) ;
#116686 = ORIENTED_EDGE ( 'NONE', *, *, #127973, .F. ) ;
#116687 = EDGE_CURVE ( 'NONE', #104716, #44009, #64957, .T. ) ;
#116688 = CARTESIAN_POINT ( 'NONE',  ( 108.7037635252314516, 6.109999999999998543, 1.122388791418548911E-15 ) ) ;
#116689 = CARTESIAN_POINT ( 'NONE',  ( -26.99999999999980815, -16.02097659208073566, -11.96015758381202154 ) ) ;
#116690 = DIRECTION ( 'NONE',  ( 0.7071067811865487940, 0.7071067811865463515, -0.000000000000000000 ) ) ;
#116691 = ORIENTED_EDGE ( 'NONE', *, *, #13560, .T. ) ;
#116692 = AXIS2_PLACEMENT_3D ( 'NONE', #37620, #70965, #25285 ) ;
#116693 = CARTESIAN_POINT ( 'NONE',  ( 48.48921356237309510, -27.52281430457089328, 5.000000000000000000 ) ) ;
#116694 = CIRCLE ( 'NONE', #77319, 2.500000000000000888 ) ;
#116695 = CARTESIAN_POINT ( 'NONE',  ( 14.99999999999990230, 14.96639925780210767, 5.000000000000000000 ) ) ;
#116696 = EDGE_CURVE ( 'NONE', #21017, #11525, #9321, .T. ) ;
#116697 = CARTESIAN_POINT ( 'NONE',  ( 24.29974487139158867, -27.71228299555223273, 4.000000000000000000 ) ) ;
#116698 = CARTESIAN_POINT ( 'NONE',  ( -29.99999999999979394, 10.93112307739207623, 4.000000000000000000 ) ) ;
#116699 = ORIENTED_EDGE ( 'NONE', *, *, #19765, .T. ) ;
#116700 = AXIS2_PLACEMENT_3D ( 'NONE', #129238, #65459, #121219 ) ;
#116701 = CARTESIAN_POINT ( 'NONE',  ( 26.99999999999980815, -12.03360074219761700, 5.000000000000000000 ) ) ;
#116702 = DIRECTION ( 'NONE',  ( -1.000000000000000000, -1.224606353822377258E-16, -0.000000000000000000 ) ) ;
#116704 = ORIENTED_EDGE ( 'NONE', *, *, #54819, .F. ) ;
#116703 = AXIS2_PLACEMENT_3D ( 'NONE', #9563, #141544, #96561 ) ;
#116705 = PLANE ( 'NONE',  #110544 ) ;
#116706 = PLANE ( 'NONE',  #59706 ) ;
#116707 = CYLINDRICAL_SURFACE ( 'NONE', #28304, 3.999999999999989786 ) ;
#116708 = VERTEX_POINT ( 'NONE', #32565 ) ;
#116709 = EDGE_CURVE ( 'NONE', #104180, #34779, #118837, .T. ) ;
#116710 = LINE ( 'NONE', #128320, #119978 ) ;
#116711 = VERTEX_POINT ( 'NONE', #65208 ) ;
#116712 = EDGE_CURVE ( 'NONE', #5308, #25358, #139909, .T. ) ;
#116713 = EDGE_LOOP ( 'NONE', ( #26234, #33996, #48425, #131048, #28011, #76338 ) ) ;
#116714 = ORIENTED_EDGE ( 'NONE', *, *, #39170, .F. ) ;
#116715 = EDGE_CURVE ( 'NONE', #130843, #41370, #54340, .T. ) ;
#116716 = CARTESIAN_POINT ( 'NONE',  ( 32.72459685856478018, -1.637169565754160949, 6.109999999999997655 ) ) ;
#116718 = ORIENTED_EDGE ( 'NONE', *, *, #8938, .F. ) ;
#116717 = CIRCLE ( 'NONE', #14881, 0.5000000000000004441 ) ;
#116719 = DIRECTION ( 'NONE',  ( 0.7071067811865487940, 0.7071067811865463515, 0.000000000000000000 ) ) ;
#116720 = LINE ( 'NONE', #117402, #63462 ) ;
#116721 = LINE ( 'NONE', #26848, #18333 ) ;
#116722 = DIRECTION ( 'NONE',  ( 0.7071067811865487940, 0.7071067811865463515, 0.000000000000000000 ) ) ;
#116723 = DIRECTION ( 'NONE',  ( 0.7071067811865486830, -0.7071067811865464625, -0.000000000000000000 ) ) ;
#116724 = LINE ( 'NONE', #17402, #134946 ) ;
#116725 = CIRCLE ( 'NONE', #40391, 2.055000000000001048 ) ;
#116726 = FILL_AREA_STYLE ('',( #60973 ) ) ;
#116727 = CARTESIAN_POINT ( 'NONE',  ( 6.628407645496676714, 3.061616997868380183E-16, -2.500000000000001332 ) ) ;
#116728 = CARTESIAN_POINT ( 'NONE',  ( -35.99451991528749772, 28.92564299267963079, 4.000000000000000000 ) ) ;
#116729 = EDGE_CURVE ( 'NONE', #55828, #110463, #43431, .T. ) ;
#116730 = VERTEX_POINT ( 'NONE', #141304 ) ;
#116731 = ORIENTED_EDGE ( 'NONE', *, *, #64806, .T. ) ;
#116733 = ORIENTED_EDGE ( 'NONE', *, *, #79210, .T. ) ;
#116732 = AXIS2_PLACEMENT_3D ( 'NONE', #81858, #135504, #70962 ) ;
#116734 = ORIENTED_EDGE ( 'NONE', *, *, #2699, .F. ) ;
#116735 = DIRECTION ( 'NONE',  ( -0.7071067811865486830, 0.7071067811865464625, 0.000000000000000000 ) ) ;
#116736 = ORIENTED_EDGE ( 'NONE', *, *, #57932, .T. ) ;
#116737 = ORIENTED_EDGE ( 'NONE', *, *, #43906, .T. ) ;
#116738 = DIRECTION ( 'NONE',  ( 0.6830127018922180770, -0.6830127018922204085, -0.2588190451025213501 ) ) ;
#116739 = CARTESIAN_POINT ( 'NONE',  ( -3.183988606268992161, 28.73617430169789699, 5.000000000000000000 ) ) ;
#116740 = ORIENTED_EDGE ( 'NONE', *, *, #54102, .T. ) ;
#116741 = LINE ( 'NONE', #118137, #30228 ) ;
#116742 = ORIENTED_EDGE ( 'NONE', *, *, #142344, .T. ) ;
#116743 = CARTESIAN_POINT ( 'NONE',  ( -29.99999999999979039, -18.03360074219754949, 5.000000000000000000 ) ) ;
#116744 = LINE ( 'NONE', #92122, #86725 ) ;
#116745 = CARTESIAN_POINT ( 'NONE',  ( 8.525403141435219823, 2.126176841940962348, 7.934999999999989839 ) ) ;
#116746 = ORIENTED_EDGE ( 'NONE', *, *, #72179, .T. ) ;
#116748 = CARTESIAN_POINT ( 'NONE',  ( -8.207106781186485733, -2.240707523384259492, 5.000000000000000000 ) ) ;
#116747 = CARTESIAN_POINT ( 'NONE',  ( 101.4120968585647802, 5.291415217122922066, -3.054999999999995275 ) ) ;
#116749 = FACE_OUTER_BOUND ( 'NONE', #123805, .T. ) ;
#116750 = VERTEX_POINT ( 'NONE', #20945 ) ;
#116751 = ORIENTED_EDGE ( 'NONE', *, *, #112105, .F. ) ;
#116752 =( LENGTH_UNIT ( ) NAMED_UNIT ( * ) SI_UNIT ( .MILLI., .METRE. ) );
#116753 = VERTEX_POINT ( 'NONE', #109393 ) ;
#116754 = FILL_AREA_STYLE_COLOUR ( '', #27789 ) ;
#116755 = DIRECTION ( 'NONE',  ( 0.7071067811865486830, -0.7071067811865464625, -0.000000000000000000 ) ) ;
#116756 = DIRECTION ( 'NONE',  ( 0.6830127018922181881, 0.6830127018922202975, -0.2588190451025214056 ) ) ;
#116757 = CARTESIAN_POINT ( 'NONE',  ( 180.6665599231034207, -49.11775834062181190, -40.20665288735654030 ) ) ;
#116759 = VERTEX_POINT ( 'NONE', #20217 ) ;
#116758 = VECTOR ( 'NONE', #21140, 1000.000000000000000 ) ;
#116760 = LINE ( 'NONE', #61700, #46031 ) ;
#116761 = EDGE_CURVE ( 'NONE', #14518, #39863, #128996, .T. ) ;
#116762 = CARTESIAN_POINT ( 'NONE',  ( -17.29289321881333308, 11.25929247661560240, 5.000000000000000000 ) ) ;
#116763 = CARTESIAN_POINT ( 'NONE',  ( 12.49289321881344605, -60.26999999999998892, 25.00000000000000000 ) ) ;
#116764 = ORIENTED_EDGE ( 'NONE', *, *, #75688, .F. ) ;
#116765 = FACE_OUTER_BOUND ( 'NONE', #49745, .T. ) ;
#116766 = DIRECTION ( 'NONE',  ( -0.6830127018922181881, 0.6830127018922202975, -0.2588190451025214056 ) ) ;
#116767 = ORIENTED_EDGE ( 'NONE', *, *, #94025, .T. ) ;
#116768 = EDGE_CURVE ( 'NONE', #22223, #108166, #30414, .T. ) ;
#116770 = ORIENTED_EDGE ( 'NONE', *, *, #112719, .T. ) ;
#116769 = CARTESIAN_POINT ( 'NONE',  ( 0.01254890717040265530, -50.57777258831010414, -35.91905586107258586 ) ) ;
#116772 = VERTEX_POINT ( 'NONE', #52157 ) ;
#116771 = EDGE_CURVE ( 'NONE', #141085, #74995, #18801, .T. ) ;
#116773 = CARTESIAN_POINT ( 'NONE',  ( -3.684382248798170334, 13.44380610198669324, -24.60099495244268653 ) ) ;
#116774 = CARTESIAN_POINT ( 'NONE',  ( -51.18398860626899705, 28.73617430169823095, 5.000000000000000000 ) ) ;
#116775 = AXIS2_PLACEMENT_3D ( 'NONE', #120430, #121176, #65416 ) ;
#116776 = ORIENTED_EDGE ( 'NONE', *, *, #31396, .F. ) ;
#116777 = DIRECTION ( 'NONE',  ( -0.7071067811865486830, -0.7071067811865464625, -0.000000000000000000 ) ) ;
#116778 = VECTOR ( 'NONE', #115177, 1000.000000000000000 ) ;
#116779 = SURFACE_STYLE_USAGE ( .BOTH. , #83456 ) ;
#116780 = VERTEX_POINT ( 'NONE', #96336 ) ;
#116781 = EDGE_CURVE ( 'NONE', #8977, #116077, #74649, .T. ) ;
#116782 = FACE_OUTER_BOUND ( 'NONE', #132271, .T. ) ;
#116784 = FACE_OUTER_BOUND ( 'NONE', #50629, .T. ) ;
#116783 = VECTOR ( 'NONE', #27114, 1000.000000000000227 ) ;
#116785 = CARTESIAN_POINT ( 'NONE',  ( 18.99507522778794666, -5.240707523384225297, 12.38332538355491508 ) ) ;
#116786 = DIRECTION ( 'NONE',  ( 0.6830127018922180770, -0.6830127018922204085, -0.2588190451025213501 ) ) ;
#116787 = CARTESIAN_POINT ( 'NONE',  ( 21.48921356237309155, -27.52281430457070499, 5.000000000000000000 ) ) ;
#116788 = CARTESIAN_POINT ( 'NONE',  ( 27.48921356237309155, -27.52281430457074762, 5.000000000000000000 ) ) ;
#116789 = LINE ( 'NONE', #37832, #76168 ) ;
#116790 = LINE ( 'NONE', #118929, #81243 ) ;
#116791 = CARTESIAN_POINT ( 'NONE',  ( 7.499999999999958256, 4.087461875839200509, 4.000000000000000000 ) ) ;
#116792 = ORIENTED_EDGE ( 'NONE', *, *, #123890, .F. ) ;
#116793 = ADVANCED_FACE ( 'NONE', ( #129707 ), #19526, .F. ) ;
#116794 = VERTEX_POINT ( 'NONE', #113672 ) ;
#116795 = VERTEX_POINT ( 'NONE', #99953 ) ;
#116796 = CARTESIAN_POINT ( 'NONE',  ( 113.0000000000000000, 0.000000000000000000, -7.950000000000000178 ) ) ;
#116797 = ORIENTED_EDGE ( 'NONE', *, *, #26794, .F. ) ;
#116798 = VECTOR ( 'NONE', #2074, 1000.000000000000000 ) ;
#116799 = ORIENTED_EDGE ( 'NONE', *, *, #140971, .F. ) ;
#116800 = ORIENTED_EDGE ( 'NONE', *, *, #119030, .F. ) ;
#116801 = DIRECTION ( 'NONE',  ( 0.000000000000000000, 0.000000000000000000, 1.000000000000000000 ) ) ;
#116802 = CARTESIAN_POINT ( 'NONE',  ( 20.29289321881331887, 17.25929247661554911, 5.000000000000000000 ) ) ;
#116803 = ADVANCED_FACE ( 'NONE', ( #25232 ), #69488, .T. ) ;
#116804 = VERTEX_POINT ( 'NONE', #123151 ) ;
#116805 = DIRECTION ( 'NONE',  ( 0.000000000000000000, 1.000000000000000000, -0.000000000000000000 ) ) ;
#116806 = CARTESIAN_POINT ( 'NONE',  ( -14.81601139373099585, 28.73617430169776910, 5.000000000000000000 ) ) ;
#116807 = CARTESIAN_POINT ( 'NONE',  ( 7.326124847093153925, 4.202752102959690472E-16, 0.000000000000000000 ) ) ;
#116808 = FACE_OUTER_BOUND ( 'NONE', #40763, .T. ) ;
#116809 = CARTESIAN_POINT ( 'NONE',  ( 101.6462635252314186, -4.472830434245840259, 4.472830434245839371 ) ) ;
#116810 = VERTEX_POINT ( 'NONE', #110791 ) ;
#116811 = FACE_OUTER_BOUND ( 'NONE', #2194, .T. ) ;
#116812 = CARTESIAN_POINT ( 'NONE',  ( 33.29177708983026918, -15.74070752338412049, 19.73771281079105222 ) ) ;
#116813 = PLANE ( 'NONE',  #77494 ) ;
#116814 = CARTESIAN_POINT ( 'NONE',  ( -28.49999999999980105, -2.173586137069166924, -4.605770156576174834 ) ) ;
#116815 =( LENGTH_UNIT ( ) NAMED_UNIT ( * ) SI_UNIT ( .MILLI., .METRE. ) );
#116816 = CARTESIAN_POINT ( 'NONE',  ( 29.99999999999999645, 2.375000000000000000, 4.319999999999998508 ) ) ;
#116817 = DIRECTION ( 'NONE',  ( -0.3543493200069162685, -0.000000000000000000, -0.9351131265310288487 ) ) ;
#116818 = AXIS2_PLACEMENT_3D ( 'NONE', #131714, #143292, #109235 ) ;
#116819 = CARTESIAN_POINT ( 'NONE',  ( 37.99586038379622011, -3.974999999999998312, -6.884901960086286188 ) ) ;
#116820 = CARTESIAN_POINT ( 'NONE',  ( -15.48921356237309510, -27.52281430457066236, 5.000000000000000000 ) ) ;
#116821 = VECTOR ( 'NONE', #40124, 1000.000000000000227 ) ;
#116822 = DIRECTION ( 'NONE',  ( 0.7071067811865487940, 0.7071067811865463515, 0.000000000000000000 ) ) ;
#116823 = ORIENTED_EDGE ( 'NONE', *, *, #34314, .F. ) ;
#116824 = VERTEX_POINT ( 'NONE', #34705 ) ;
#116825 = VECTOR ( 'NONE', #142111, 1000.000000000000000 ) ;
#116826 = CARTESIAN_POINT ( 'NONE',  ( 28.12499999999999645, -7.950000000000000178, -4.867971026610729436E-16 ) ) ;
#116827 = ORIENTED_EDGE ( 'NONE', *, *, #65769, .T. ) ;
#116828 = PRESENTATION_LAYER_ASSIGNMENT (  '', '', ( #10322 ) ) ;
#116829 = CARTESIAN_POINT ( 'NONE',  ( -17.81601139373099940, 28.73617430169775133, 5.000000000000000000 ) ) ;
#116830 = EDGE_CURVE ( 'NONE', #65419, #91252, #80366, .T. ) ;
#116831 = FACE_OUTER_BOUND ( 'NONE', #92834, .T. ) ;
#116832 = DIRECTION ( 'NONE',  ( -0.3543493200069163240, -0.000000000000000000, -0.9351131265310288487 ) ) ;
#116834 = EDGE_CURVE ( 'NONE', #62799, #24662, #66619, .T. ) ;
#116833 = CARTESIAN_POINT ( 'NONE',  ( -19.05000000000000071, 3.174999999999997158, 0.000000000000000000 ) ) ;
#116835 = EDGE_CURVE ( 'NONE', #25909, #92341, #129813, .T. ) ;
#116836 = CARTESIAN_POINT ( 'NONE',  ( 19.05000000000000071, 3.174999999999997158, 1.444000000000000394 ) ) ;
#116837 = CARTESIAN_POINT ( 'NONE',  ( 30.91709685856476497, 3.054999999999998828, 5.291415217122922066 ) ) ;
#116838 = ORIENTED_EDGE ( 'NONE', *, *, #620, .T. ) ;
#116839 = DIRECTION ( 'NONE',  ( 1.000000000000000000, 0.000000000000000000, 0.000000000000000000 ) ) ;
#116840 = VERTEX_POINT ( 'NONE', #124557 ) ;
#116841 = DIRECTION ( 'NONE',  ( 0.000000000000000000, -1.000000000000000000, 0.000000000000000000 ) ) ;
#116842 = EDGE_CURVE ( 'NONE', #60629, #47758, #57194, .T. ) ;
#116843 = DIRECTION ( 'NONE',  ( 0.000000000000000000, -2.242629915582283412E-16, 1.000000000000000000 ) ) ;
#116844 = DIRECTION ( 'NONE',  ( 0.7071067811865486830, -0.7071067811865464625, -0.000000000000000000 ) ) ;
#116845 = CARTESIAN_POINT ( 'NONE',  ( 63.27083333333332860, -7.949999999999998401, -2.130196079827426203 ) ) ;
#116846 = ORIENTED_EDGE ( 'NONE', *, *, #140884, .T. ) ;
#116848 = EDGE_CURVE ( 'NONE', #73530, #109556, #12918, .T. ) ;
#116847 = CARTESIAN_POINT ( 'NONE',  ( 56.87543019189809712, -5.291415217122920289, -3.055000000000001492 ) ) ;
#116849 = ORIENTED_EDGE ( 'NONE', *, *, #54815, .F. ) ;
#116850 = FACE_OUTER_BOUND ( 'NONE', #45841, .T. ) ;
#116851 = EDGE_CURVE ( 'NONE', #123173, #46980, #143440, .T. ) ;
#116852 = CARTESIAN_POINT ( 'NONE',  ( -7.637538124160930586, 22.22500000000000142, 4.000000000000000000 ) ) ;
#116853 = CARTESIAN_POINT ( 'NONE',  ( 19.05000000000000071, 3.174999999999997158, 5.000000000000000000 ) ) ;
#116854 = DIRECTION ( 'NONE',  ( -0.7071067811865487940, 0.7071067811865463515, -0.000000000000000000 ) ) ;
#116855 = EDGE_CURVE ( 'NONE', #133448, #98744, #2013, .T. ) ;
#116856 = ADVANCED_FACE ( 'NONE', ( #11474 ), #44157, .F. ) ;
#116857 = CARTESIAN_POINT ( 'NONE',  ( 45.84959685856478018, 6.109999999999996767, 1.637169565754163836 ) ) ;
#116858 = ORIENTED_EDGE ( 'NONE', *, *, #54228, .F. ) ;
#116859 = LINE ( 'NONE', #17536, #55855 ) ;
#116860 = CYLINDRICAL_SURFACE ( 'NONE', #87223, 0.5000000000000000000 ) ;
#116861 = EDGE_LOOP ( 'NONE', ( #46269, #25910, #135113 ) ) ;
#116862 = VERTEX_POINT ( 'NONE', #24522 ) ;
#116863 = PLANE ( 'NONE',  #137231 ) ;
#116864 = EDGE_CURVE ( 'NONE', #36373, #107048, #132618, .T. ) ;
#116865 = ORIENTED_EDGE ( 'NONE', *, *, #64349, .T. ) ;
#116866 = AXIS2_PLACEMENT_3D ( 'NONE', #632, #65225, #76076 ) ;
#116867 = CARTESIAN_POINT ( 'NONE',  ( 66.18398860626901126, 28.73617430169833753, 5.000000000000000000 ) ) ;
#116868 = ORIENTED_EDGE ( 'NONE', *, *, #120751, .F. ) ;
#116869 = CARTESIAN_POINT ( 'NONE',  ( 1.499999999999987566, -4.216083040037250207, -7.486842126848659795 ) ) ;
#116870 = ADVANCED_FACE ( 'NONE', ( #77513 ), #121676, .F. ) ;
#116871 = CARTESIAN_POINT ( 'NONE',  ( 7.139999999999992575, -35.14999999999999858, -39.50000000000000000 ) ) ;
#116872 = FACE_BOUND ( 'NONE', #117547, .T. ) ;
#116873 = LINE ( 'NONE', #69848, #98861 ) ;
#116874 = DIRECTION ( 'NONE',  ( -0.000000000000000000, 0.000000000000000000, 1.000000000000000000 ) ) ;
#116875 = DIRECTION ( 'NONE',  ( -1.000000000000000000, 0.000000000000000000, 0.000000000000000000 ) ) ;
#116876 = VERTEX_POINT ( 'NONE', #125998 ) ;
#116878 = ORIENTED_EDGE ( 'NONE', *, *, #7806, .F. ) ;
#116877 = DIRECTION ( 'NONE',  ( -0.000000000000000000, -0.3543493200069152693, 0.9351131265310292928 ) ) ;
#116879 = ADVANCED_FACE ( 'NONE', ( #28823 ), #32550, .T. ) ;
#116880 = ORIENTED_EDGE ( 'NONE', *, *, #47196, .T. ) ;
#116881 = CARTESIAN_POINT ( 'NONE',  ( -32.99999999999975842, 14.58746187583908771, 4.000000000000000000 ) ) ;
#116882 = VERTEX_POINT ( 'NONE', #39716 ) ;
#116883 = EDGE_CURVE ( 'NONE', #119248, #62339, #104195, .T. ) ;
#116884 = VECTOR ( 'NONE', #138232, 999.9999999999998863 ) ;
#116885 = CARTESIAN_POINT ( 'NONE',  ( 53.72459685856478018, -1.637169565754160949, 6.109999999999997655 ) ) ;
#116886 = ORIENTED_EDGE ( 'NONE', *, *, #50563, .F. ) ;
#116887 = LINE ( 'NONE', #60400, #14036 ) ;
#116888 = VECTOR ( 'NONE', #126965, 1000.000000000000000 ) ;
#116889 = LINE ( 'NONE', #74848, #121314 ) ;
#116890 = ORIENTED_EDGE ( 'NONE', *, *, #6981, .T. ) ;
#116891 = LINE ( 'NONE', #105986, #63049 ) ;
#116892 = ADVANCED_FACE ( 'NONE', ( #25962 ), #83944, .F. ) ;
#116893 =( BOUNDED_CURVE ( )  B_SPLINE_CURVE ( 3, ( #35847, #90174, #11151, #122082 ),
 .UNSPECIFIED., .F., .F. ) 
 B_SPLINE_CURVE_WITH_KNOTS ( ( 4, 4 ),
 ( 1.964434688349484537, 3.503810798801452187 ),
 .UNSPECIFIED. ) 
 CURVE ( )  GEOMETRIC_REPRESENTATION_ITEM ( )  RATIONAL_B_SPLINE_CURVE ( ( 1.000000000000000000, 0.8120851936182271746, 0.8120851936182271746, 1.000000000000000000 ) ) 
 REPRESENTATION_ITEM ( '' )  );
#116894 = DIRECTION ( 'NONE',  ( 0.000000000000000000, 0.9647414015272156584, -0.2631995976047526442 ) ) ;
#116895 = VECTOR ( 'NONE', #47988, 1000.000000000000000 ) ;
#116896 = CARTESIAN_POINT ( 'NONE',  ( 14.99999999999989519, 7.559798855135672291, 4.979909187984731922 ) ) ;
#116897 = DIRECTION ( 'NONE',  ( 0.000000000000000000, 0.000000000000000000, 1.000000000000000000 ) ) ;
#116898 = DIRECTION ( 'NONE',  ( 0.7071067811865486830, -0.7071067811865464625, -0.000000000000000000 ) ) ;
#116899 = DIRECTION ( 'NONE',  ( -0.000000000000000000, 0.3543493200069153248, 0.9351131265310292928 ) ) ;
#116900 = VERTEX_POINT ( 'NONE', #128144 ) ;
#116901 = ORIENTED_EDGE ( 'NONE', *, *, #25455, .F. ) ;
#116902 = LINE ( 'NONE', #8114, #47404 ) ;
#116903 = DIRECTION ( 'NONE',  ( 0.000000000000000000, -1.000000000000000000, 0.000000000000000000 ) ) ;
#116904 = VERTEX_POINT ( 'NONE', #17220 ) ;
#116905 = ORIENTED_EDGE ( 'NONE', *, *, #95340, .F. ) ;
#116906 = ORIENTED_EDGE ( 'NONE', *, *, #98238, .F. ) ;
#116907 = DIRECTION ( 'NONE',  ( 1.000000000000000000, 0.000000000000000000, 0.000000000000000000 ) ) ;
#116908 = CARTESIAN_POINT ( 'NONE',  ( 54.47502705046288440, -5.819803920172573086, 5.819803920172573086 ) ) ;
#116909 = CARTESIAN_POINT ( 'NONE',  ( 30.02083333333332860, 7.949999999999998401, 2.130196079827431532 ) ) ;
#116910 = ORIENTED_EDGE ( 'NONE', *, *, #20559, .F. ) ;
#116911 = DIRECTION ( 'NONE',  ( -0.6830127018922181881, 0.6830127018922202975, -0.2588190451025214056 ) ) ;
#116912 = AXIS2_PLACEMENT_3D ( 'NONE', #11223, #90244, #134487 ) ;
#116913 = SURFACE_STYLE_USAGE ( .BOTH. , #106732 ) ;
#116914 = VECTOR ( 'NONE', #8297, 1000.000000000000227 ) ;
#116915 = CARTESIAN_POINT ( 'NONE',  ( 13.04623647476855375, -7.934999999999990727, 4.858786175617117713E-16 ) ) ;
#116916 = VECTOR ( 'NONE', #39739, 1000.000000000000000 ) ;
#116917 = CARTESIAN_POINT ( 'NONE',  ( 184.1500000000000057, -43.14999999999999147, -31.92499999999998295 ) ) ;
#116918 = ORIENTED_EDGE ( 'NONE', *, *, #39059, .F. ) ;
#116919 = CARTESIAN_POINT ( 'NONE',  ( 36.48921356237310221, -27.52281430457080802, 5.000000000000000000 ) ) ;
#116920 = COLOUR_RGB ( '', 0.40784314, 0.44705882, 0.49803922) ;
#116922 = EDGE_CURVE ( 'NONE', #122443, #40992, #60030, .T. ) ;
#116921 = LINE ( 'NONE', #17589, #9545 ) ;
#116923 = CARTESIAN_POINT ( 'NONE',  ( -5.999999999999958256, 4.552185695429124657, 5.000000000000000000 ) ) ;
#116925 = EDGE_LOOP ( 'NONE', ( #62606, #139409, #90575, #113438 ) ) ;
#116924 = CARTESIAN_POINT ( 'NONE',  ( 54.18398860626899705, 28.73617430169825226, 5.000000000000000000 ) ) ;
#116926 = CARTESIAN_POINT ( 'NONE',  ( 0.000000000000000000, 0.000000000000000000, 5.000000000000000000 ) ) ;
#116927 = ORIENTED_EDGE ( 'NONE', *, *, #21501, .F. ) ;
#116928 = FACE_OUTER_BOUND ( 'NONE', #18202, .T. ) ;
#116929 = DIRECTION ( 'NONE',  ( 0.3543493200069162685, -0.000000000000000000, -0.9351131265310288487 ) ) ;
#116930 = CARTESIAN_POINT ( 'NONE',  ( 38.53839644629405115, -9.740707523384177335, 17.74957260769619793 ) ) ;
#116931 = VERTEX_POINT ( 'NONE', #71614 ) ;
#116932 = CARTESIAN_POINT ( 'NONE',  ( 36.48921356237310221, -27.52281430457080802, 5.000000000000000000 ) ) ;
#116933 = CARTESIAN_POINT ( 'NONE',  ( -11.51078643762690490, -27.52281430457047406, 5.000000000000000000 ) ) ;
#116934 = CARTESIAN_POINT ( 'NONE',  ( -36.48921356237310221, -27.52281430457080802, 5.000000000000000000 ) ) ;
#116935 = EDGE_LOOP ( 'NONE', ( #15619, #18403, #117413, #119680 ) ) ;
#116936 = FACE_OUTER_BOUND ( 'NONE', #51493, .T. ) ;
#116937 = DIRECTION ( 'NONE',  ( 1.000000000000000000, 1.224606353822377258E-16, 0.000000000000000000 ) ) ;
#116938 = DIRECTION ( 'NONE',  ( 0.7071067811865487940, -0.7071067811865463515, 0.000000000000000000 ) ) ;
#116939 = ADVANCED_FACE ( 'NONE', ( #72366 ), #50565, .T. ) ;
#116940 = CARTESIAN_POINT ( 'NONE',  ( -21.08491323193748812, -12.74070752338414891, 18.74364270924349185 ) ) ;
#116941 = CARTESIAN_POINT ( 'NONE',  ( -22.49999999999984013, 5.696342897626483825, -7.587980461218449157 ) ) ;
#116942 = EDGE_CURVE ( 'NONE', #79481, #90561, #125154, .T. ) ;
#116943 = ORIENTED_EDGE ( 'NONE', *, *, #19785, .T. ) ;
#116944 = ORIENTED_EDGE ( 'NONE', *, *, #90137, .T. ) ;
#116945 = DIRECTION ( 'NONE',  ( 0.6830127018922180770, -0.6830127018922204085, -0.2588190451025213501 ) ) ;
#116946 = CARTESIAN_POINT ( 'NONE',  ( -36.29974487139159578, -27.71228299555231445, 4.000000000000000000 ) ) ;
#116947 = EDGE_CURVE ( 'NONE', #15939, #27059, #37564, .T. ) ;
#116948 = ADVANCED_FACE ( 'NONE', ( #91919 ), #26670, .F. ) ;
#116949 = CARTESIAN_POINT ( 'NONE',  ( 7.853736474768552966, -5.808823158059035485, -5.808823158059033709 ) ) ;
#116950 = PLANE ( 'NONE',  #120000 ) ;
#116951 = CARTESIAN_POINT ( 'NONE',  ( -51.48921356237309510, -27.52281430457091460, 5.000000000000000000 ) ) ;
#116952 = LINE ( 'NONE', #17618, #52926 ) ;
#116953 = FACE_OUTER_BOUND ( 'NONE', #136536, .T. ) ;
#116954 = ORIENTED_EDGE ( 'NONE', *, *, #18748, .F. ) ;
#116955 = EDGE_CURVE ( 'NONE', #34380, #59881, #15059, .T. ) ;
#116956 = DIRECTION ( 'NONE',  ( -0.000000000000000000, -0.3543493200069152693, 0.9351131265310292928 ) ) ;
#116957 = CARTESIAN_POINT ( 'NONE',  ( 38.99451991528749062, 28.92564299267965211, 4.000000000000000000 ) ) ;
#116958 = CARTESIAN_POINT ( 'NONE',  ( -13.49999999999990408, 7.466399257802187606, 5.000000000000000000 ) ) ;
#116959 = FACE_OUTER_BOUND ( 'NONE', #59817, .T. ) ;
#116960 = CARTESIAN_POINT ( 'NONE',  ( 43.66209685856478728, -5.291415217122919401, 3.054999999999998384 ) ) ;
#116961 = CARTESIAN_POINT ( 'NONE',  ( 10.46799328145038821, -2.055000000000000160, 2.789133085058097101E-16 ) ) ;
#116962 = EDGE_CURVE ( 'NONE', #36342, #97431, #138295, .T. ) ;
#116963 = ORIENTED_EDGE ( 'NONE', *, *, #33306, .F. ) ;
#116964 = CARTESIAN_POINT ( 'NONE',  ( 29.99999999999979039, 12.25461709320623349, -10.07315571508690333 ) ) ;
#116965 = ORIENTED_EDGE ( 'NONE', *, *, #102468, .F. ) ;
#116966 = EDGE_LOOP ( 'NONE', ( #126211, #13176, #19877, #43457 ) ) ;
#116967 = CARTESIAN_POINT ( 'NONE',  ( 36.29974487139159578, -27.71228299555231445, 4.000000000000000000 ) ) ;
#116968 = EDGE_CURVE ( 'NONE', #117536, #112494, #117713, .T. ) ;
#116969 = LINE ( 'NONE', #73486, #43885 ) ;
#116970 = CARTESIAN_POINT ( 'NONE',  ( 3.299744871391591339, -27.71228299555208352, 4.000000000000000000 ) ) ;
#116971 = LINE ( 'NONE', #19091, #136600 ) ;
#116972 = DIRECTION ( 'NONE',  ( -0.000000000000000000, -0.3543493200069152693, 0.9351131265310292928 ) ) ;
#116973 = PLANE ( 'NONE',  #66213 ) ;
#116974 = ORIENTED_EDGE ( 'NONE', *, *, #94692, .T. ) ;
#116975 = CARTESIAN_POINT ( 'NONE',  ( 9.994118527364397764, 2.500000000000000444, 0.000000000000000000 ) ) ;
#116976 = CARTESIAN_POINT ( 'NONE',  ( -12.18398860626900060, 28.73617430169795739, 5.000000000000000000 ) ) ;
#116977 = EDGE_CURVE ( 'NONE', #75725, #56540, #81072, .T. ) ;
#116978 = PLANE ( 'NONE',  #77999 ) ;
#116979 = CARTESIAN_POINT ( 'NONE',  ( 21.48921356237309155, -27.52281430457070499, 5.000000000000000000 ) ) ;
#116980 = CARTESIAN_POINT ( 'NONE',  ( 34.47516574401890921, 6.028067341115750821, 4.998110765256834398 ) ) ;
#116981 = CARTESIAN_POINT ( 'NONE',  ( 64.10002705046287019, 5.819803920172570422, 5.819803920172574863 ) ) ;
#116982 = AXIS2_PLACEMENT_3D ( 'NONE', #90257, #3242, #125034 ) ;
#116983 = DIRECTION ( 'NONE',  ( -1.000000000000000000, 0.000000000000000000, -0.000000000000000000 ) ) ;
#116984 = ORIENTED_EDGE ( 'NONE', *, *, #111138, .T. ) ;
#116985 = VERTEX_POINT ( 'NONE', #49161 ) ;
#116986 = CARTESIAN_POINT ( 'NONE',  ( 68.08333333333332860, 6.884901960086290629, -3.974999999999994316 ) ) ;
#116987 = CARTESIAN_POINT ( 'NONE',  ( -14.51078643762690490, -27.52281430457045275, 5.000000000000000000 ) ) ;
#116988 = MECHANICAL_DESIGN_GEOMETRIC_PRESENTATION_REPRESENTATION (  '', ( #119346 ), #24374 ) ;
#116989 = CARTESIAN_POINT ( 'NONE',  ( 32.29289321881323360, 2.259292476615696099, 5.000000000000000000 ) ) ;
#116990 = ADVANCED_FACE ( 'NONE', ( #103490 ), #83198, .F. ) ;
#116991 = CARTESIAN_POINT ( 'NONE',  ( 8.031592354503320763, 9.902892378096218942E-16, 0.000000000000000000 ) ) ;
#116992 = ORIENTED_EDGE ( 'NONE', *, *, #108285, .F. ) ;
#116994 = EDGE_CURVE ( 'NONE', #12991, #12275, #28102, .T. ) ;
#116993 = CARTESIAN_POINT ( 'NONE',  ( -33.48921356237309510, -27.52281430457078670, 5.000000000000000000 ) ) ;
#116995 = EDGE_CURVE ( 'NONE', #91273, #110128, #139013, .T. ) ;
#116996 = VECTOR ( 'NONE', #102187, 1000.000000000000114 ) ;
#116997 = CARTESIAN_POINT ( 'NONE',  ( -51.18398860626899705, 28.73617430169823095, 5.000000000000000000 ) ) ;
#116998 = CARTESIAN_POINT ( 'NONE',  ( 60.52126352523143282, -4.472830434245839371, -4.472830434245840259 ) ) ;
#116999 = ORIENTED_EDGE ( 'NONE', *, *, #86418, .T. ) ;
#117000 = DIRECTION ( 'NONE',  ( -0.7071067811865486830, -0.7071067811865464625, 0.000000000000000000 ) ) ;
#117001 = EDGE_LOOP ( 'NONE', ( #106367, #132057, #47986, #94909 ) ) ;
#117002 = VERTEX_POINT ( 'NONE', #31676 ) ;
#117003 = DIRECTION ( 'NONE',  ( 0.000000000000000000, 0.000000000000000000, 1.000000000000000000 ) ) ;
#117004 = EDGE_CURVE ( 'NONE', #65419, #125983, #29506, .T. ) ;
#117005 = CARTESIAN_POINT ( 'NONE',  ( -33.79289321881321939, 18.75929247661552068, 5.000000000000000000 ) ) ;
#117006 = LINE ( 'NONE', #37325, #118326 ) ;
#117007 = CARTESIAN_POINT ( 'NONE',  ( 23.51078643762690490, -27.52281430457038880, 5.000000000000000000 ) ) ;
#117008 = EDGE_CURVE ( 'NONE', #28348, #85531, #9904, .T. ) ;
#117009 = CARTESIAN_POINT ( 'NONE',  ( -3.328169399223503078, -21.74070752338406010, 4.000000000000000000 ) ) ;
#117011 = ORIENTED_EDGE ( 'NONE', *, *, #86948, .F. ) ;
#117010 = CARTESIAN_POINT ( 'NONE',  ( -23.99999999999982947, -15.41253812416059610, 4.000000000000000000 ) ) ;
#117012 = CARTESIAN_POINT ( 'NONE',  ( -21.70710678118640047, 20.25929247661551713, 5.000000000000000000 ) ) ;
#117013 = CARTESIAN_POINT ( 'NONE',  ( -39.48921356237310221, -27.52281430457082934, 5.000000000000000000 ) ) ;
#117014 = DIRECTION ( 'NONE',  ( 0.7071067811865486830, -0.7071067811865464625, -0.000000000000000000 ) ) ;
#117015 = DIRECTION ( 'NONE',  ( -0.000000000000000000, 0.3543493200069153248, 0.9351131265310292928 ) ) ;
#117016 = VECTOR ( 'NONE', #8717, 1000.000000000000000 ) ;
#117017 = VERTEX_POINT ( 'NONE', #52000 ) ;
#117018 = AXIS2_PLACEMENT_3D ( 'NONE', #38384, #93476, #138408 ) ;
#117019 = ORIENTED_EDGE ( 'NONE', *, *, #118953, .F. ) ;
#117020 = VECTOR ( 'NONE', #66267, 1000.000000000000000 ) ;
#117021 = EDGE_CURVE ( 'NONE', #50968, #27038, #116033, .T. ) ;
#117022 = DIRECTION ( 'NONE',  ( 0.000000000000000000, 0.000000000000000000, 1.000000000000000000 ) ) ;
#117023 = CARTESIAN_POINT ( 'NONE',  ( -28.49999999999978684, 4.087461875839202285, 4.000000000000000000 ) ) ;
#117024 = DIRECTION ( 'NONE',  ( -2.781805975412905890E-17, 0.3543493200069152693, 0.9351131265310292928 ) ) ;
#117025 = CARTESIAN_POINT ( 'NONE',  ( -26.56319896779154988, -12.74070752338415247, 9.898150129686436927 ) ) ;
#117026 = CARTESIAN_POINT ( 'NONE',  ( -35.57672154193625147, 11.25929247661560240, 17.85071094206592690 ) ) ;
#117027 = ORIENTED_EDGE ( 'NONE', *, *, #9579, .F. ) ;
#117028 = ORIENTED_EDGE ( 'NONE', *, *, #19958, .F. ) ;
#117029 = COLOUR_RGB ( '', 0.31764706, 0.68627451, 0.89019608) ;
#117030 = CARTESIAN_POINT ( 'NONE',  ( 33.18398860626899705, 28.73617430169810305, 5.000000000000000000 ) ) ;
#117032 = ADVANCED_FACE ( 'NONE', ( #131704 ), #96879, .F. ) ;
#117031 = CARTESIAN_POINT ( 'NONE',  ( 20.19999999999999929, -2.055000000000000160, 2.789133085058098087E-16 ) ) ;
#117033 = VERTEX_POINT ( 'NONE', #64301 ) ;
#117034 = VERTEX_POINT ( 'NONE', #75203 ) ;
#117035 = CARTESIAN_POINT ( 'NONE',  ( 3.411614905948293419, 22.22500000000000142, 4.777194822843816802 ) ) ;
#117036 = ORIENTED_EDGE ( 'NONE', *, *, #43394, .T. ) ;
#117037 = DIRECTION ( 'NONE',  ( 0.7071067811865487940, 0.7071067811865463515, 0.000000000000000000 ) ) ;
#117038 = CARTESIAN_POINT ( 'NONE',  ( 34.75611968250419181, 4.705650698524001641, 4.955485411084875835 ) ) ;
#117039 = FACE_BOUND ( 'NONE', #95022, .T. ) ;
#117040 = PLANE ( 'NONE',  #110335 ) ;
#117041 =( REPRESENTATION_RELATIONSHIP ('NONE','NONE', #69070, #108808 ) REPRESENTATION_RELATIONSHIP_WITH_TRANSFORMATION ( #96691 )SHAPE_REPRESENTATION_RELATIONSHIP( ) );
#117042 = CARTESIAN_POINT ( 'NONE',  ( 28.49999999999980460, 1.087461875839230707, 4.000000000000000000 ) ) ;
#117044 = ORIENTED_EDGE ( 'NONE', *, *, #105631, .F. ) ;
#117043 = DIRECTION ( 'NONE',  ( 0.7071067811865487940, 0.7071067811865463515, 0.000000000000000000 ) ) ;
#117045 = SHAPE_DEFINITION_REPRESENTATION ( #6386, #103311 ) ;
#117046 = ORIENTED_EDGE ( 'NONE', *, *, #9550, .T. ) ;
#117047 = ADVANCED_FACE ( 'NONE', ( #86778 ), #7142, .T. ) ;
#117048 = ORIENTED_EDGE ( 'NONE', *, *, #26619, .F. ) ;
#117049 = CARTESIAN_POINT ( 'NONE',  ( 89.59959685856476597, -6.109999999999997655, -1.637169565754160283 ) ) ;
#117050 = ORIENTED_EDGE ( 'NONE', *, *, #28958, .F. ) ;
#117051 = CARTESIAN_POINT ( 'NONE',  ( 49.99999999999998579, 0.000000000000000000, -7.950000000000000178 ) ) ;
#117052 = CARTESIAN_POINT ( 'NONE',  ( -34.92500000000001137, -22.22500000000000142, 4.500000000000000888 ) ) ;
#117053 = DIRECTION ( 'NONE',  ( 0.7071067811865486830, -0.7071067811865464625, -0.000000000000000000 ) ) ;
#117054 = ORIENTED_EDGE ( 'NONE', *, *, #142390, .F. ) ;
#117055 = CARTESIAN_POINT ( 'NONE',  ( -17.51078643762690845, -27.52281430457043143, 5.000000000000000000 ) ) ;
#117056 =( NAMED_UNIT ( * ) SI_UNIT ( $, .STERADIAN. ) SOLID_ANGLE_UNIT ( ) );
#117057 = LINE ( 'NONE', #51119, #82111 ) ;
#117058 = CARTESIAN_POINT ( 'NONE',  ( 14.99999999999988809, -13.06887692260767331, 4.000000000000000000 ) ) ;
#117059 = CARTESIAN_POINT ( 'NONE',  ( -34.49999999999976552, -8.945670655168967755, 4.994342998332164996 ) ) ;
#117060 = ORIENTED_EDGE ( 'NONE', *, *, #55753, .F. ) ;
#117061 = CARTESIAN_POINT ( 'NONE',  ( 26.43999999999999773, -2.055000000000000160, 2.789133085058098087E-16 ) ) ;
#117062 = CARTESIAN_POINT ( 'NONE',  ( -0.005480084712502889671, 28.92564299267938210, 4.000000000000000000 ) ) ;
#117063 = ORIENTED_EDGE ( 'NONE', *, *, #75338, .F. ) ;
#117064 = ORIENTED_EDGE ( 'NONE', *, *, #60359, .T. ) ;
#117065 = VERTEX_POINT ( 'NONE', #129534 ) ;
#117066 = CARTESIAN_POINT ( 'NONE',  ( 49.29209685856476852, -5.291415217122921177, 3.054999999999999272 ) ) ;
#117067 = ORIENTED_EDGE ( 'NONE', *, *, #62141, .F. ) ;
#117068 =( BOUNDED_CURVE ( )  B_SPLINE_CURVE ( 3, ( #48861, #78626, #113368, #58355 ),
 .UNSPECIFIED., .F., .T. ) 
 B_SPLINE_CURVE_WITH_KNOTS ( ( 4, 4 ),
 ( 2.779374508378134934, 4.199602562396838934 ),
 .UNSPECIFIED. ) 
 CURVE ( )  GEOMETRIC_REPRESENTATION_ITEM ( )  RATIONAL_B_SPLINE_CURVE ( ( 1.000000000000000000, 0.8388583629366627159, 0.8388583629366627159, 1.000000000000000000 ) ) 
 REPRESENTATION_ITEM ( '' )  );
#117069 = AXIS2_PLACEMENT_3D ( 'NONE', #19493, #41978, #7150 ) ;
#117070 = CARTESIAN_POINT ( 'NONE',  ( 15.35830628287044242, -1.633150327867689988, 6.094999999999989981 ) ) ;
#117071 = CARTESIAN_POINT ( 'NONE',  ( -16.42533615676552117, 1.154938085476876264, -30.62621587217987340 ) ) ;
#117072 = ORIENTED_EDGE ( 'NONE', *, *, #68491, .F. ) ;
#117073 = PRESENTATION_LAYER_ASSIGNMENT (  '', '', ( #98562 ) ) ;
#117074 = DIRECTION ( 'NONE',  ( 1.000000000000000000, 0.000000000000000000, 0.000000000000000000 ) ) ;
#117075 = ORIENTED_EDGE ( 'NONE', *, *, #103513, .T. ) ;
#117076 = FACE_OUTER_BOUND ( 'NONE', #89140, .T. ) ;
#117077 = DIRECTION ( 'NONE',  ( -0.6830127018922180770, -0.6830127018922204085, -0.2588190451025213501 ) ) ;
#117079 = ORIENTED_EDGE ( 'NONE', *, *, #107012, .T. ) ;
#117078 = LINE ( 'NONE', #7600, #49480 ) ;
#117080 = ORIENTED_EDGE ( 'NONE', *, *, #67751, .F. ) ;
#117081 = LINE ( 'NONE', #102676, #102423 ) ;
#117082 = CYLINDRICAL_SURFACE ( 'NONE', #101726, 7.950000000000000178 ) ;
#117083 = ORIENTED_EDGE ( 'NONE', *, *, #40526, .F. ) ;
#117084 = FACE_OUTER_BOUND ( 'NONE', #109362, .T. ) ;
#117085 = EDGE_LOOP ( 'NONE', ( #91519, #136688, #108089, #11654 ) ) ;
#117086 = EDGE_LOOP ( 'NONE', ( #67108, #25864, #52296, #129897, #97052, #85015 ) ) ;
#117087 = ORIENTED_EDGE ( 'NONE', *, *, #120529, .F. ) ;
#117088 = ORIENTED_EDGE ( 'NONE', *, *, #17658, .T. ) ;
#117089 = EDGE_CURVE ( 'NONE', #41151, #45672, #54179, .T. ) ;
#117090 = DIRECTION ( 'NONE',  ( -0.7071067811865486830, -0.7071067811865464625, 0.000000000000000000 ) ) ;
#117091 = DIRECTION ( 'NONE',  ( 0.3543493200069162685, -0.000000000000000000, -0.9351131265310288487 ) ) ;
#117092 = EDGE_CURVE ( 'NONE', #75992, #52339, #19141, .T. ) ;
#117093 = LINE ( 'NONE', #6167, #84455 ) ;
#117094 = CARTESIAN_POINT ( 'NONE',  ( 68.99451991528748351, 28.92564299267986172, 4.000000000000000000 ) ) ;
#117095 = EDGE_CURVE ( 'NONE', #33358, #13774, #20055, .T. ) ;
#117097 = VERTEX_POINT ( 'NONE', #141886 ) ;
#117096 = ADVANCED_FACE ( 'NONE', ( #97626 ), #17894, .F. ) ;
#117098 = CARTESIAN_POINT ( 'NONE',  ( 66.33333333333332860, -6.884901960086287964, 3.974999999999998312 ) ) ;
#117099 = ORIENTED_EDGE ( 'NONE', *, *, #17332, .F. ) ;
#117100 = LINE ( 'NONE', #114934, #30854 ) ;
#117101 = AXIS2_PLACEMENT_3D ( 'NONE', #137361, #58415, #115549 ) ;
#117102 = EDGE_CURVE ( 'NONE', #115214, #118985, #53438, .T. ) ;
#117103 = EDGE_CURVE ( 'NONE', #142129, #64647, #120062, .T. ) ;
#117104 = CARTESIAN_POINT ( 'NONE',  ( 28.27040314143521726, -7.934999999999989839, 2.126176841940957907 ) ) ;
#117105 = CARTESIAN_POINT ( 'NONE',  ( 33.48921356237309510, -27.52281430457078670, 5.000000000000000000 ) ) ;
#117106 = VECTOR ( 'NONE', #38576, 1000.000000000000227 ) ;
#117107 = ORIENTED_EDGE ( 'NONE', *, *, #123364, .T. ) ;
#117108 = CARTESIAN_POINT ( 'NONE',  ( -45.48921356237309510, -27.52281430457087197, 5.000000000000000000 ) ) ;
#117109 = CARTESIAN_POINT ( 'NONE',  ( -34.89799234656373983, 22.27000000000001023, -9.122257832017591994 ) ) ;
#117110 = EDGE_LOOP ( 'NONE', ( #74530, #46834, #46215 ) ) ;
#117111 = VECTOR ( 'NONE', #65333, 1000.000000000000000 ) ;
#117112 = ORIENTED_EDGE ( 'NONE', *, *, #1464, .F. ) ;
#117113 = EDGE_CURVE ( 'NONE', #2756, #55557, #18638, .T. ) ;
#117114 = VERTEX_POINT ( 'NONE', #117921 ) ;
#117115 = DIRECTION ( 'NONE',  ( -0.3543493200069162685, -0.000000000000000000, -0.9351131265310288487 ) ) ;
#117116 = DIRECTION ( 'NONE',  ( 1.000000000000000000, 0.000000000000000000, 0.000000000000000000 ) ) ;
#117117 = FACE_OUTER_BOUND ( 'NONE', #125968, .T. ) ;
#117118 = MECHANICAL_DESIGN_GEOMETRIC_PRESENTATION_REPRESENTATION (  '', ( #121772 ), #84747 ) ;
#117119 = DIRECTION ( 'NONE',  ( 0.6830127018922180770, -0.6830127018922204085, -0.2588190451025213501 ) ) ;
#117120 = CARTESIAN_POINT ( 'NONE',  ( 3.221442824812127625, -48.88296141031989350, -39.14553452061910832 ) ) ;
#117121 = CARTESIAN_POINT ( 'NONE',  ( 79.09959685856478018, -6.109999999999998543, -1.637169565754160727 ) ) ;
#117122 = CARTESIAN_POINT ( 'NONE',  ( -29.99999999999978328, 4.552185695429124657, 5.000000000000000000 ) ) ;
#117123 = ADVANCED_FACE ( 'NONE', ( #62898 ), #107078, .F. ) ;
#117124 = PLANE ( 'NONE',  #122506 ) ;
#117125 = CARTESIAN_POINT ( 'NONE',  ( -29.57659687702524920, -22.22500000000000142, 2.973290122897137344 ) ) ;
#117126 = DIRECTION ( 'NONE',  ( -1.000000000000000000, -0.000000000000000000, -0.000000000000000000 ) ) ;
#117127 = CARTESIAN_POINT ( 'NONE',  ( 48.29974487139158867, -27.71228299555239971, 4.000000000000000000 ) ) ;
#117128 = VERTEX_POINT ( 'NONE', #44741 ) ;
#117129 = DIRECTION ( 'NONE',  ( -0.7071067811865486830, -0.7071067811865464625, -0.000000000000000000 ) ) ;
#117130 = VERTEX_POINT ( 'NONE', #135295 ) ;
#117131 = CARTESIAN_POINT ( 'NONE',  ( -36.18398860626899705, 28.73617430169812437, 5.000000000000000000 ) ) ;
#117133 = ORIENTED_EDGE ( 'NONE', *, *, #116508, .F. ) ;
#117132 = DIRECTION ( 'NONE',  ( 0.7071067811865487940, 0.7071067811865463515, 0.000000000000000000 ) ) ;
#117134 = CARTESIAN_POINT ( 'NONE',  ( 26.20666063542134339, 21.75929247661549581, 4.998822639870700968 ) ) ;
#117135 = LINE ( 'NONE', #17814, #51862 ) ;
#117136 = VERTEX_POINT ( 'NONE', #46895 ) ;
#117137 = ORIENTED_EDGE ( 'NONE', *, *, #98549, .F. ) ;
#117138 = LINE ( 'NONE', #6206, #97564 ) ;
#117139 = LINE ( 'NONE', #119284, #120803 ) ;
#117140 = EDGE_CURVE ( 'NONE', #57564, #130156, #120808, .T. ) ;
#117141 = DIRECTION ( 'NONE',  ( -0.7071067811865486830, -0.7071067811865464625, 0.000000000000000000 ) ) ;
#117142 = CARTESIAN_POINT ( 'NONE',  ( 90.78752705046288440, 0.000000000000000000, -7.949999999999998401 ) ) ;
#117143 = CARTESIAN_POINT ( 'NONE',  ( 20.99999999999986144, -10.06887692260770173, 4.000000000000000000 ) ) ;
#117144 = ORIENTED_EDGE ( 'NONE', *, *, #75121, .T. ) ;
#117145 = DIRECTION ( 'NONE',  ( 1.000000000000000000, 0.000000000000000000, -0.000000000000000000 ) ) ;
#117146 = DIRECTION ( 'NONE',  ( 0.7071067811865486830, -0.7071067811865464625, -0.000000000000000000 ) ) ;
#117148 = CARTESIAN_POINT ( 'NONE',  ( 28.72916666666666785, -6.094999999999989093, 1.633150327867691765 ) ) ;
#117147 = B_SPLINE_CURVE_WITH_KNOTS ( 'NONE', 3,
 ( #19159, #31474, #97405, #75001, #62680, #106866, #63420, #107587, #20565, #95286 ),
 .UNSPECIFIED., .F., .F.,
 ( 4, 2, 2, 2, 4 ),
 ( 0.005493704601871781008, 0.006008885122700058715, 0.006524065643528337288, 0.007039246164356615862, 0.007554426685184895303 ),
 .UNSPECIFIED. ) ;
#117149 = ADVANCED_FACE ( 'NONE', ( #21515 ), #67917, .F. ) ;
#117150 = VECTOR ( 'NONE', #63552, 1000.000000000000227 ) ;
#117151 = CARTESIAN_POINT ( 'NONE',  ( 8.915086768062332467, -12.74070752338415602, 18.74364270924356290 ) ) ;
#117152 = ORIENTED_EDGE ( 'NONE', *, *, #35026, .T. ) ;
#117153 = LINE ( 'NONE', #74405, #109220 ) ;
#117154 = EDGE_CURVE ( 'NONE', #12722, #21741, #1837, .T. ) ;
#117155 = EDGE_LOOP ( 'NONE', ( #87416, #99004, #71248, #139687 ) ) ;
#117156 = CARTESIAN_POINT ( 'NONE',  ( 80.79209685856477563, -5.291415217122921177, 3.054999999999999272 ) ) ;
#117157 = EDGE_CURVE ( 'NONE', #114197, #40900, #76632, .T. ) ;
#117158 = LINE ( 'NONE', #74410, #45486 ) ;
#117159 = DIRECTION ( 'NONE',  ( 0.6830127018922180770, -0.6830127018922204085, -0.2588190451025213501 ) ) ;
#117160 = DIRECTION ( 'NONE',  ( -0.7071067811865486830, -0.7071067811865464625, 0.000000000000000000 ) ) ;
#117161 = ORIENTED_EDGE ( 'NONE', *, *, #66926, .T. ) ;
#117162 = LINE ( 'NONE', #95425, #90567 ) ;
#117163 = EDGE_CURVE ( 'NONE', #40291, #117136, #67161, .T. ) ;
#117164 = CARTESIAN_POINT ( 'NONE',  ( 59.99451991528749772, 28.92564299267980132, 4.000000000000000000 ) ) ;
#117165 = DIRECTION ( 'NONE',  ( 8.673617379884034239E-17, -1.000000000000000000, 0.000000000000000000 ) ) ;
#117167 = ORIENTED_EDGE ( 'NONE', *, *, #92334, .T. ) ;
#117166 = DIRECTION ( 'NONE',  ( 0.6830127018922181881, 0.6830127018922202975, -0.2588190451025214056 ) ) ;
#117168 = LINE ( 'NONE', #132390, #32181 ) ;
#117169 = SURFACE_STYLE_USAGE ( .BOTH. , #94701 ) ;
#117170 = ORIENTED_EDGE ( 'NONE', *, *, #51628, .F. ) ;
#117171 =( GEOMETRIC_REPRESENTATION_CONTEXT ( 3 ) GLOBAL_UNCERTAINTY_ASSIGNED_CONTEXT ( ( #56237 ) ) GLOBAL_UNIT_ASSIGNED_CONTEXT ( ( #14893, #25771, #117056 ) ) REPRESENTATION_CONTEXT ( 'NONE', 'WORKASPACE' ) );
#117172 = VERTEX_POINT ( 'NONE', #46146 ) ;
#117173 = CARTESIAN_POINT ( 'NONE',  ( 75.68793019189811844, 6.110000000000002984, -1.637169565754156730 ) ) ;
#117174 = ORIENTED_EDGE ( 'NONE', *, *, #31460, .T. ) ;
#117175 = AXIS2_PLACEMENT_3D ( 'NONE', #47038, #135433, #101345 ) ;
#117176 = ADVANCED_FACE ( 'NONE', ( #2585 ), #112104, .T. ) ;
#117177 = DIRECTION ( 'NONE',  ( -0.6830127018922180770, -0.6830127018922204085, -0.2588190451025213501 ) ) ;
#117178 = CARTESIAN_POINT ( 'NONE',  ( 3.328169399223503966, 14.25929247661557397, 4.000000000000000000 ) ) ;
#117179 = LINE ( 'NONE', #62126, #17640 ) ;
#117180 = VERTEX_POINT ( 'NONE', #68605 ) ;
#117181 = DIRECTION ( 'NONE',  ( 1.000000000000000000, 0.000000000000000000, 0.000000000000000000 ) ) ;
#117182 = CARTESIAN_POINT ( 'NONE',  ( -12.48921356237309155, -27.52281430457064104, 5.000000000000000000 ) ) ;
#117183 = ORIENTED_EDGE ( 'NONE', *, *, #73037, .T. ) ;
#117184 = CIRCLE ( 'NONE', #10596, 3.000000000000002665 ) ;
#117185 = DIRECTION ( 'NONE',  ( 1.000000000000000000, 0.000000000000000000, 0.000000000000000000 ) ) ;
#117186 = CARTESIAN_POINT ( 'NONE',  ( 51.18398860626899705, 28.73617430169823095, 5.000000000000000000 ) ) ;
#117187 = LINE ( 'NONE', #6974, #67845 ) ;
#117188 = ORIENTED_EDGE ( 'NONE', *, *, #74596, .T. ) ;
#117189 = ORIENTED_EDGE ( 'NONE', *, *, #119693, .F. ) ;
#117190 = ADVANCED_FACE ( 'NONE', ( #99773 ), #79513, .T. ) ;
#117191 = VECTOR ( 'NONE', #115911, 1000.000000000000000 ) ;
#117192 = FACE_OUTER_BOUND ( 'NONE', #78772, .T. ) ;
#117193 = CARTESIAN_POINT ( 'NONE',  ( -25.39999999999996305, 0.000000000000000000, 0.000000000000000000 ) ) ;
#117194 = LINE ( 'NONE', #107054, #78929 ) ;
#117195 = CARTESIAN_POINT ( 'NONE',  ( -23.99999999999982947, -21.84840872380826937, 2.849755605029552274 ) ) ;
#117196 = CARTESIAN_POINT ( 'NONE',  ( 52.43336038379622721, 2.130196079827431532, -7.949999999999996625 ) ) ;
#117197 = VECTOR ( 'NONE', #18385, 999.9999999999998863 ) ;
#117198 = VECTOR ( 'NONE', #90855, 1000.000000000000000 ) ;
#117199 = DIRECTION ( 'NONE',  ( 0.7071067811865487940, 0.7071067811865463515, 0.000000000000000000 ) ) ;
#117200 = ORIENTED_EDGE ( 'NONE', *, *, #136123, .F. ) ;
#117201 = VECTOR ( 'NONE', #31280, 1000.000000000000000 ) ;
#117202 = ORIENTED_EDGE ( 'NONE', *, *, #72116, .T. ) ;
#117203 = ORIENTED_EDGE ( 'NONE', *, *, #82428, .T. ) ;
#117204 = ORIENTED_EDGE ( 'NONE', *, *, #47966, .T. ) ;
#117205 = VECTOR ( 'NONE', #45526, 1000.000000000000227 ) ;
#117206 = ADVANCED_FACE ( 'NONE', ( #110625 ), #13453, .F. ) ;
#117208 = ADVANCED_FACE ( 'NONE', ( #88935 ), #133152, .F. ) ;
#117207 = FACE_OUTER_BOUND ( 'NONE', #73589, .T. ) ;
#117209 = ORIENTED_EDGE ( 'NONE', *, *, #106150, .F. ) ;
#117210 = PLANE ( 'NONE',  #62165 ) ;
#117211 = LINE ( 'NONE', #139006, #72741 ) ;
#117212 = CARTESIAN_POINT ( 'NONE',  ( -34.92500000000001137, -15.89852273831279028, -9.446427897663618012 ) ) ;
#117213 = DIRECTION ( 'NONE',  ( -4.681814790819591790E-17, -0.3543493200069152693, 0.9351131265310292928 ) ) ;
#117214 = CARTESIAN_POINT ( 'NONE',  ( -39.48921356237310221, -27.52281430457082934, 5.000000000000000000 ) ) ;
#117215 = ORIENTED_EDGE ( 'NONE', *, *, #36606, .F. ) ;
#117216 = PLANE ( 'NONE',  #3146 ) ;
#117217 = DIRECTION ( 'NONE',  ( 0.3543493200069162685, -0.000000000000000000, -0.9351131265310288487 ) ) ;
#117218 = ORIENTED_EDGE ( 'NONE', *, *, #24136, .F. ) ;
#117219 = CARTESIAN_POINT ( 'NONE',  ( 14.29289321881336150, -18.74070752338409562, 5.000000000000000000 ) ) ;
#117220 = ORIENTED_EDGE ( 'NONE', *, *, #33529, .F. ) ;
#117221 = EDGE_CURVE ( 'NONE', #22222, #112964, #123704, .T. ) ;
#117222 = DIRECTION ( 'NONE',  ( 0.000000000000000000, -1.000000000000000000, 0.000000000000000000 ) ) ;
#117223 = ORIENTED_EDGE ( 'NONE', *, *, #2884, .F. ) ;
#117224 = VERTEX_POINT ( 'NONE', #134576 ) ;
#117225 = CARTESIAN_POINT ( 'NONE',  ( 76.12543019189810423, 5.291415217122919401, 3.055000000000002824 ) ) ;
#117226 = ORIENTED_EDGE ( 'NONE', *, *, #86740, .F. ) ;
#117227 =( NAMED_UNIT ( * ) SI_UNIT ( $, .STERADIAN. ) SOLID_ANGLE_UNIT ( ) );
#117228 = AXIS2_PLACEMENT_3D ( 'NONE', #117955, #118702, #141160 ) ;
#117229 = CARTESIAN_POINT ( 'NONE',  ( -32.01088028653925477, -22.02621442084248216, 4.990779571109222879 ) ) ;
#117230 = CARTESIAN_POINT ( 'NONE',  ( 109.9587635252314470, 0.000000000000000000, -6.110000000000001208 ) ) ;
#117231 = DIRECTION ( 'NONE',  ( 0.000000000000000000, 1.000000000000000000, 0.000000000000000000 ) ) ;
#117233 = CARTESIAN_POINT ( 'NONE',  ( -30.48921356237309510, -27.52281430457076894, 5.000000000000000000 ) ) ;
#117232 = DIRECTION ( 'NONE',  ( 0.7071067811865487940, 0.7071067811865463515, -0.000000000000000000 ) ) ;
#117234 = PLANE ( 'NONE',  #74164 ) ;
#117235 = AXIS2_PLACEMENT_3D ( 'NONE', #23197, #2147, #67482 ) ;
#117236 = PLANE ( 'NONE',  #114113 ) ;
#117237 = DIRECTION ( 'NONE',  ( -1.000000000000000000, -0.000000000000000000, 0.000000000000000000 ) ) ;
#117238 = DIRECTION ( 'NONE',  ( 0.000000000000000000, 0.000000000000000000, -1.000000000000000000 ) ) ;
#117239 = VERTEX_POINT ( 'NONE', #33145 ) ;
#117240 = DIRECTION ( 'NONE',  ( 0.7071067811865487940, 0.7071067811865463515, 0.000000000000000000 ) ) ;
#117241 = CARTESIAN_POINT ( 'NONE',  ( -30.00000000000000355, 2.375000000000000000, 0.000000000000000000 ) ) ;
#117242 = ORIENTED_EDGE ( 'NONE', *, *, #106212, .F. ) ;
#117243 = ORIENTED_EDGE ( 'NONE', *, *, #2410, .T. ) ;
#117244 = VECTOR ( 'NONE', #90220, 999.9999999999998863 ) ;
#117245 = DIRECTION ( 'NONE',  ( 0.000000000000000000, -1.000000000000000000, 0.000000000000000000 ) ) ;
#117246 = ORIENTED_EDGE ( 'NONE', *, *, #100384, .F. ) ;
#117247 = DIRECTION ( 'NONE',  ( 0.3543493200069162685, -0.000000000000000000, -0.9351131265310288487 ) ) ;
#117248 = FACE_OUTER_BOUND ( 'NONE', #32908, .T. ) ;
#117249 = LINE ( 'NONE', #62933, #57936 ) ;
#117250 = CARTESIAN_POINT ( 'NONE',  ( 128.5894344200537773, -52.00875322212549179, -39.86617647058817226 ) ) ;
#117251 = EDGE_CURVE ( 'NONE', #88267, #53631, #24358, .T. ) ;
#117252 = ORIENTED_EDGE ( 'NONE', *, *, #99314, .F. ) ;
#117253 = CARTESIAN_POINT ( 'NONE',  ( 3.187477005606119906, -48.82538788374325378, 38.96958855984426151 ) ) ;
#117254 = VERTEX_POINT ( 'NONE', #78049 ) ;
#117255 = VECTOR ( 'NONE', #18260, 1000.000000000000000 ) ;
#117256 = ADVANCED_FACE ( 'NONE', ( #99042 ), #143280, .T. ) ;
#117257 = EDGE_CURVE ( 'NONE', #117989, #12173, #122225, .T. ) ;
#117258 = CARTESIAN_POINT ( 'NONE',  ( 7.999569808101885116, -3.967499999999998028, -6.871911579029511330 ) ) ;
#117259 = LINE ( 'NONE', #16529, #16919 ) ;
#117260 = ADVANCED_FACE ( 'NONE', ( #89611 ), #101199, .F. ) ;
#117261 = DIRECTION ( 'NONE',  ( -0.7071067811865486830, -0.7071067811865464625, 0.000000000000000000 ) ) ;
#117262 = AXIS2_PLACEMENT_3D ( 'NONE', #3948, #15548, #27898 ) ;
#117263 = CARTESIAN_POINT ( 'NONE',  ( 14.24942747710153412, -9.300561119015622324, -1.955118594580004254 ) ) ;
#117264 = VERTEX_POINT ( 'NONE', #80201 ) ;
#117265 = ORIENTED_EDGE ( 'NONE', *, *, #10564, .T. ) ;
#117266 = EDGE_CURVE ( 'NONE', #81792, #72669, #3300, .T. ) ;
#117267 = AXIS2_PLACEMENT_3D ( 'NONE', #62624, #16966, #61239 ) ;
#117268 = EDGE_LOOP ( 'NONE', ( #114740, #109448, #101533, #40679 ) ) ;
#117269 = DIRECTION ( 'NONE',  ( -0.7071067811865487940, 0.7071067811865463515, -0.000000000000000000 ) ) ;
#117270 = DIRECTION ( 'NONE',  ( 0.7071067811865487940, 0.7071067811865463515, 0.000000000000000000 ) ) ;
#117271 = DIRECTION ( 'NONE',  ( -0.000000000000000000, 0.000000000000000000, 1.000000000000000000 ) ) ;
#117272 = EDGE_CURVE ( 'NONE', #22612, #52625, #138125, .T. ) ;
#117273 = DIRECTION ( 'NONE',  ( -0.6830127018922181881, 0.6830127018922202975, -0.2588190451025214056 ) ) ;
#117274 = CARTESIAN_POINT ( 'NONE',  ( 0.000000000000000000, 0.000000000000000000, 5.000000000000000000 ) ) ;
#117275 = DIRECTION ( 'NONE',  ( 0.6830127018922180770, -0.6830127018922204085, -0.2588190451025213501 ) ) ;
#117276 = DIRECTION ( 'NONE',  ( -0.000000000000000000, -0.3543493200069152693, 0.9351131265310292928 ) ) ;
#117277 = EDGE_CURVE ( 'NONE', #13287, #44234, #15576, .T. ) ;
#117278 = LINE ( 'NONE', #62231, #97227 ) ;
#117279 = VECTOR ( 'NONE', #6827, 999.9999999999998863 ) ;
#117280 = CARTESIAN_POINT ( 'NONE',  ( -12.70701326429296252, -21.74070752338406010, 4.999753212805220670 ) ) ;
#117281 = CARTESIAN_POINT ( 'NONE',  ( 18.32816939922340893, 20.25929247661551358, 4.000000000000000000 ) ) ;
#117282 = ORIENTED_EDGE ( 'NONE', *, *, #135644, .F. ) ;
#117283 = DIRECTION ( 'NONE',  ( 0.7071067811865487940, 0.7071067811865463515, -0.000000000000000000 ) ) ;
#117284 = DIRECTION ( 'NONE',  ( -0.7071067811865486830, -0.7071067811865464625, 0.000000000000000000 ) ) ;
#117285 = ORIENTED_EDGE ( 'NONE', *, *, #14780, .F. ) ;
#117286 = ADVANCED_FACE ( 'NONE', ( #71446 ), #61327, .F. ) ;
#117287 = CARTESIAN_POINT ( 'NONE',  ( -7.140000000000001457, -35.76999999999998892, -12.10072711459627293 ) ) ;
#117289 = ORIENTED_EDGE ( 'NONE', *, *, #128662, .F. ) ;
#117288 = DIRECTION ( 'NONE',  ( -0.000000000000000000, 0.3543493200069153248, 0.9351131265310292928 ) ) ;
#117290 = AXIS2_PLACEMENT_3D ( 'NONE', #59133, #12711, #25011 ) ;
#117291 = ADVANCED_FACE ( 'NONE', ( #125833 ), #59857, .F. ) ;
#117292 = DIRECTION ( 'NONE',  ( -0.000000000000000000, 0.3543493200069153248, 0.9351131265310292928 ) ) ;
#117293 = DIRECTION ( 'NONE',  ( 0.3543493200069162685, -0.000000000000000000, -0.9351131265310288487 ) ) ;
#117294 = VERTEX_POINT ( 'NONE', #6131 ) ;
#117295 = DIRECTION ( 'NONE',  ( 0.6830127018922180770, -0.6830127018922204085, -0.2588190451025213501 ) ) ;
#117296 = UNCERTAINTY_MEASURE_WITH_UNIT (LENGTH_MEASURE( 1.000000000000000082E-05 ), #65087, 'distance_accuracy_value', 'NONE');
#117297 = ORIENTED_EDGE ( 'NONE', *, *, #75041, .T. ) ;
#117298 = EDGE_CURVE ( 'NONE', #106679, #115779, #114898, .T. ) ;
#117299 = VECTOR ( 'NONE', #15707, 999.9999999999998863 ) ;
#117300 = VECTOR ( 'NONE', #110943, 1000.000000000000000 ) ;
#117301 = DIRECTION ( 'NONE',  ( 0.7071067811865487940, 0.7071067811865463515, 0.000000000000000000 ) ) ;
#117303 = CARTESIAN_POINT ( 'NONE',  ( 122.1416937171295416, -2.130196079827424871, -7.949999999999999289 ) ) ;
#117302 = AXIS2_PLACEMENT_3D ( 'NONE', #87235, #131459, #54618 ) ;
#117304 = PLANE ( 'NONE',  #25401 ) ;
#117305 = DIRECTION ( 'NONE',  ( -0.000000000000000000, -0.3543493200069152693, 0.9351131265310292928 ) ) ;
#117306 = LINE ( 'NONE', #94837, #60794 ) ;
#117307 = DIRECTION ( 'NONE',  ( 0.7071067811865486830, -0.7071067811865464625, -0.000000000000000000 ) ) ;
#117308 = CARTESIAN_POINT ( 'NONE',  ( 5.913098576467837653, -22.22500000000000142, 20.47508215891419781 ) ) ;
#117309 = CARTESIAN_POINT ( 'NONE',  ( 27.24956980810188867, 3.967499999999998916, 6.871911579029510442 ) ) ;
#117310 = CARTESIAN_POINT ( 'NONE',  ( 9.457903141435219041, 6.871911579029515771, 3.967499999999989146 ) ) ;
#117311 = CARTESIAN_POINT ( 'NONE',  ( -23.20666063542136470, 21.75929247661548516, 4.998822639870711626 ) ) ;
#117312 = VECTOR ( 'NONE', #36432, 1000.000000000000227 ) ;
#117313 = PLANE ( 'NONE',  #81355 ) ;
#117314 = LINE ( 'NONE', #118756, #50199 ) ;
#117315 = EDGE_LOOP ( 'NONE', ( #113557, #535, #41098, #74459 ) ) ;
#117316 = ORIENTED_EDGE ( 'NONE', *, *, #63006, .T. ) ;
#117317 = CARTESIAN_POINT ( 'NONE',  ( 84.99999999999998579, 0.000000000000000000, -7.950000000000000178 ) ) ;
#117318 = FACE_OUTER_BOUND ( 'NONE', #31038, .T. ) ;
#117319 = ORIENTED_EDGE ( 'NONE', *, *, #68903, .T. ) ;
#117320 = EDGE_CURVE ( 'NONE', #79680, #109461, #139151, .T. ) ;
#117321 = CARTESIAN_POINT ( 'NONE',  ( 91.95419371712957002, 6.884901960086283523, 3.975000000000002753 ) ) ;
#117322 = CARTESIAN_POINT ( 'NONE',  ( -8.999999999999932498, -0.4125381241607516403, 4.000000000000000000 ) ) ;
#117323 = DIRECTION ( 'NONE',  ( 0.7071067811865486830, -0.7071067811865464625, -0.000000000000000000 ) ) ;
#117324 = VERTEX_POINT ( 'NONE', #27202 ) ;
#117325 = DIRECTION ( 'NONE',  ( -0.7071067811865486830, -0.7071067811865464625, 0.000000000000000000 ) ) ;
#117326 = DIRECTION ( 'NONE',  ( 0.7071067811865487940, 0.7071067811865463515, 0.000000000000000000 ) ) ;
#117327 = LINE ( 'NONE', #49281, #9332 ) ;
#117328 = DIRECTION ( 'NONE',  ( -0.000000000000000000, -0.3543493200069152693, 0.9351131265310292928 ) ) ;
#117329 = CARTESIAN_POINT ( 'NONE',  ( 0.000000000000000000, 0.000000000000000000, 5.000000000000000000 ) ) ;
#117330 = FACE_OUTER_BOUND ( 'NONE', #50632, .T. ) ;
#117331 = VECTOR ( 'NONE', #100710, 1000.000000000000000 ) ;
#117332 = PLANE ( 'NONE',  #3575 ) ;
#117333 = LINE ( 'NONE', #105055, #49318 ) ;
#117334 = DIRECTION ( 'NONE',  ( -0.000000000000000000, 0.3543493200069153248, 0.9351131265310292928 ) ) ;
#117335 = LINE ( 'NONE', #107191, #47626 ) ;
#117336 = EDGE_CURVE ( 'NONE', #45356, #80320, #127226, .T. ) ;
#117337 = CARTESIAN_POINT ( 'NONE',  ( -34.92500000000001137, 1.701930566820992308, 4.500000000000000888 ) ) ;
#117338 = EDGE_LOOP ( 'NONE', ( #15397, #22516, #25129, #22760 ) ) ;
#117339 = VERTEX_POINT ( 'NONE', #4688 ) ;
#117340 = CARTESIAN_POINT ( 'NONE',  ( 105.5837635252314328, -6.110000000000001208, -3.741295971395164515E-16 ) ) ;
#117341 = VERTEX_POINT ( 'NONE', #37387 ) ;
#117342 = ADVANCED_FACE ( 'NONE', ( #104028 ), #70060, .F. ) ;
#117343 =( NAMED_UNIT ( * ) PLANE_ANGLE_UNIT ( ) SI_UNIT ( $, .RADIAN. ) );
#117344 = VECTOR ( 'NONE', #56197, 1000.000000000000000 ) ;
#117345 = DIRECTION ( 'NONE',  ( -0.6830127018922181881, 0.6830127018922202975, -0.2588190451025214056 ) ) ;
#117346 = VERTEX_POINT ( 'NONE', #115602 ) ;
#117347 = DIRECTION ( 'NONE',  ( 0.7071067811865487940, -0.7071067811865463515, 0.000000000000000000 ) ) ;
#117348 = FACE_OUTER_BOUND ( 'NONE', #28714, .T. ) ;
#117349 = CARTESIAN_POINT ( 'NONE',  ( 99.22459685856479439, -1.637169565754160949, 6.109999999999997655 ) ) ;
#117350 = EDGE_LOOP ( 'NONE', ( #114380, #69190, #94619, #40305 ) ) ;
#117351 = EDGE_CURVE ( 'NONE', #73090, #73943, #93187, .T. ) ;
#117352 = PLANE ( 'NONE',  #99833 ) ;
#117353 = ORIENTED_EDGE ( 'NONE', *, *, #88314, .F. ) ;
#117354 = DIRECTION ( 'NONE',  ( -0.000000000000000000, 0.3543493200069153248, 0.9351131265310292928 ) ) ;
#117355 = AXIS2_PLACEMENT_3D ( 'NONE', #10336, #140844, #53891 ) ;
#117356 = LINE ( 'NONE', #63742, #97799 ) ;
#117357 = FACE_OUTER_BOUND ( 'NONE', #16486, .T. ) ;
#117358 = ORIENTED_EDGE ( 'NONE', *, *, #122105, .T. ) ;
#117359 = ORIENTED_EDGE ( 'NONE', *, *, #2258, .T. ) ;
#117360 = CIRCLE ( 'NONE', #27043, 2.500000000000000888 ) ;
#117361 = EDGE_CURVE ( 'NONE', #138157, #98423, #83033, .T. ) ;
#117362 = ORIENTED_EDGE ( 'NONE', *, *, #136662, .T. ) ;
#117363 = LINE ( 'NONE', #106473, #72327 ) ;
#117364 = CARTESIAN_POINT ( 'NONE',  ( 15.49238828748955576, -2.500000000000000000, 3.061616997868383634E-16 ) ) ;
#117365 = CARTESIAN_POINT ( 'NONE',  ( 9.108736474768551972, -5.808823158059033709, 5.808823158059035485 ) ) ;
#117366 = CARTESIAN_POINT ( 'NONE',  ( 22.02083333333333570, -6.094999999999989981, -1.633150327867689322 ) ) ;
#117367 = ORIENTED_EDGE ( 'NONE', *, *, #11952, .F. ) ;
#117368 = VECTOR ( 'NONE', #101534, 1000.000000000000227 ) ;
#117369 = ORIENTED_EDGE ( 'NONE', *, *, #65507, .T. ) ;
#117370 = DIRECTION ( 'NONE',  ( -0.6830127018922181881, 0.6830127018922202975, -0.2588190451025214056 ) ) ;
#117371 = VERTEX_POINT ( 'NONE', #116371 ) ;
#117372 = ORIENTED_EDGE ( 'NONE', *, *, #59584, .F. ) ;
#117373 = CARTESIAN_POINT ( 'NONE',  ( 25.82816939922335209, 18.75929247661552068, 4.000000000000000000 ) ) ;
#117375 = EDGE_CURVE ( 'NONE', #76282, #45436, #36654, .T. ) ;
#117374 = CARTESIAN_POINT ( 'NONE',  ( 153.6500000000000057, 7.776507174585690191E-16, -6.349999999999997868 ) ) ;
#117376 = VERTEX_POINT ( 'NONE', #16306 ) ;
#117377 = LINE ( 'NONE', #84105, #52912 ) ;
#117378 = VECTOR ( 'NONE', #94581, 1000.000000000000000 ) ;
#117379 = DIRECTION ( 'NONE',  ( -0.7071067811865486830, -0.7071067811865464625, -0.000000000000000000 ) ) ;
#117380 = DIRECTION ( 'NONE',  ( 0.000000000000000000, 1.000000000000000000, 0.000000000000000000 ) ) ;
#117381 = CARTESIAN_POINT ( 'NONE',  ( 33.79333936457825160, 21.75929247661550647, 4.998822639870711626 ) ) ;
#117382 = ORIENTED_EDGE ( 'NONE', *, *, #16461, .F. ) ;
#117383 = CARTESIAN_POINT ( 'NONE',  ( 11.29298673570687050, -21.74070752338406365, 4.999753212805220670 ) ) ;
#117385 = PLANE ( 'NONE',  #38450 ) ;
#117384 = MECHANICAL_DESIGN_GEOMETRIC_PRESENTATION_REPRESENTATION (  '', ( #31740 ), #142883 ) ;
#117386 = ORIENTED_EDGE ( 'NONE', *, *, #32275, .F. ) ;
#117387 = CARTESIAN_POINT ( 'NONE',  ( 25.39999999999999503, -2.292782931496808008, -7.607334647038449305 ) ) ;
#117388 = CARTESIAN_POINT ( 'NONE',  ( -24.59263130292903554, 0.9595543924999635488, 5.000000000000000000 ) ) ;
#117389 = DIRECTION ( 'NONE',  ( 0.7071067811865487940, 0.7071067811865463515, 0.000000000000000000 ) ) ;
#117390 = EDGE_CURVE ( 'NONE', #3647, #58008, #14188, .T. ) ;
#117391 = ORIENTED_EDGE ( 'NONE', *, *, #32502, .F. ) ;
#117392 = LINE ( 'NONE', #95660, #50486 ) ;
#117393 = ORIENTED_EDGE ( 'NONE', *, *, #1300, .F. ) ;
#117394 = VERTEX_POINT ( 'NONE', #17059 ) ;
#117395 = VECTOR ( 'NONE', #3943, 1000.000000000000000 ) ;
#117396 = ORIENTED_EDGE ( 'NONE', *, *, #6318, .T. ) ;
#117398 = VECTOR ( 'NONE', #58636, 1000.000000000000000 ) ;
#117397 = PRODUCT_DEFINITION ( 'UNKNOWN', '', #747, #140073 ) ;
#117399 = AXIS2_PLACEMENT_3D ( 'NONE', #77639, #31270, #2 ) ;
#117400 = CARTESIAN_POINT ( 'NONE',  ( 41.99451991528749062, 28.92564299267967343, 4.000000000000000000 ) ) ;
#117401 = DIRECTION ( 'NONE',  ( 0.7071067811865487940, 0.7071067811865463515, 0.000000000000000000 ) ) ;
#117402 = CARTESIAN_POINT ( 'NONE',  ( 8.999999999999937828, 7.007997736742456851, -8.085015511992091675 ) ) ;
#117403 = DIRECTION ( 'NONE',  ( -1.301042606982605074E-16, 1.000000000000000000, 0.000000000000000000 ) ) ;
#117404 = DIRECTION ( 'NONE',  ( -0.000000000000000000, 0.000000000000000000, 1.000000000000000000 ) ) ;
#117405 = CARTESIAN_POINT ( 'NONE',  ( 0.000000000000000000, 0.000000000000000000, 5.000000000000000000 ) ) ;
#117406 = PLANE ( 'NONE',  #129153 ) ;
#117407 = AXIS2_PLACEMENT_3D ( 'NONE', #55708, #1965, #57156 ) ;
#117408 = LINE ( 'NONE', #52175, #60871 ) ;
#117409 = CARTESIAN_POINT ( 'NONE',  ( -27.29974487139158512, -27.71228299555225405, 4.000000000000000000 ) ) ;
#117410 = CARTESIAN_POINT ( 'NONE',  ( 25.39999999999999858, -30.18000000000009564, 12.69999999999954454 ) ) ;
#117411 = DIRECTION ( 'NONE',  ( -1.000000000000000000, -0.000000000000000000, -0.000000000000000000 ) ) ;
#117412 = ORIENTED_EDGE ( 'NONE', *, *, #13366, .T. ) ;
#117413 = ORIENTED_EDGE ( 'NONE', *, *, #61525, .F. ) ;
#117414 = ORIENTED_EDGE ( 'NONE', *, *, #55796, .T. ) ;
#117415 = ORIENTED_EDGE ( 'NONE', *, *, #24159, .T. ) ;
#117416 = CARTESIAN_POINT ( 'NONE',  ( -1.320800000000018404, 0.08703048564677724752, 3.775643966265881613 ) ) ;
#117417 = ORIENTED_EDGE ( 'NONE', *, *, #12057, .F. ) ;
#117418 = ORIENTED_EDGE ( 'NONE', *, *, #18560, .F. ) ;
#117419 = FACE_OUTER_BOUND ( 'NONE', #140482, .T. ) ;
#117420 = CARTESIAN_POINT ( 'NONE',  ( -14.24715658456393541, 6.719242673238161601, 5.000000000000000000 ) ) ;
#117421 = LINE ( 'NONE', #103689, #80344 ) ;
#117422 = CARTESIAN_POINT ( 'NONE',  ( -24.18398860626899705, 28.73617430169804265, 5.000000000000000000 ) ) ;
#117423 = VERTEX_POINT ( 'NONE', #25778 ) ;
#117424 = AXIS2_PLACEMENT_3D ( 'NONE', #53246, #64872, #111190 ) ;
#117425 = DIRECTION ( 'NONE',  ( 0.000000000000000000, -9.130123557772670799E-17, 1.000000000000000000 ) ) ;
#117426 = ORIENTED_EDGE ( 'NONE', *, *, #67938, .T. ) ;
#117427 = CARTESIAN_POINT ( 'NONE',  ( -21.79289321881330110, 12.75929247661558996, 5.000000000000000000 ) ) ;
#117428 = DIRECTION ( 'NONE',  ( 0.6830127018922180770, -0.6830127018922204085, -0.2588190451025213501 ) ) ;
#117429 = EDGE_CURVE ( 'NONE', #74780, #9436, #60603, .T. ) ;
#117430 = VECTOR ( 'NONE', #38327, 1000.000000000000000 ) ;
#117431 = CARTESIAN_POINT ( 'NONE',  ( 5.900403141435219823, -7.934999999999989839, 2.126176841940957907 ) ) ;
#117432 = ORIENTED_EDGE ( 'NONE', *, *, #101240, .T. ) ;
#117433 = CARTESIAN_POINT ( 'NONE',  ( 94.41209685856478018, 5.291415217122922066, -3.054999999999995275 ) ) ;
#117434 =( BOUNDED_CURVE ( )  B_SPLINE_CURVE ( 3, ( #106859, #71404, #137377, #6800 ),
 .UNSPECIFIED., .F., .T. ) 
 B_SPLINE_CURVE_WITH_KNOTS ( ( 4, 4 ),
 ( 1.901594255663606736, 1.933014472006571838 ),
 .UNSPECIFIED. ) 
 CURVE ( )  GEOMETRIC_REPRESENTATION_ITEM ( )  RATIONAL_B_SPLINE_CURVE ( ( 1.000000000000000000, 0.9999177325257867510, 0.9999177325257867510, 1.000000000000000000 ) ) 
 REPRESENTATION_ITEM ( '' )  );
#117435 = CARTESIAN_POINT ( 'NONE',  ( 23.99999999999983302, -0.2811185226894059586, -5.995736974527568819 ) ) ;
#117436 = EDGE_CURVE ( 'NONE', #53397, #117371, #103323, .T. ) ;
#117437 = FILL_AREA_STYLE_COLOUR ( '', #60306 ) ;
#117438 = CARTESIAN_POINT ( 'NONE',  ( -2.510786437626908008, -27.52281430457053446, 5.000000000000000000 ) ) ;
#117439 = VERTEX_POINT ( 'NONE', #6843 ) ;
#117440 = EDGE_LOOP ( 'NONE', ( #15088, #96779, #111858, #94573 ) ) ;
#117441 = EDGE_CURVE ( 'NONE', #128359, #9541, #113657, .T. ) ;
#117442 = CARTESIAN_POINT ( 'NONE',  ( 131.6379680400227983, -49.11957940092398900, -40.22172306649559914 ) ) ;
#117443 = ORIENTED_EDGE ( 'NONE', *, *, #140298, .T. ) ;
#117444 = CIRCLE ( 'NONE', #78169, 2.055000000000000604 ) ;
#117445 = DIRECTION ( 'NONE',  ( -0.7071067811865486830, 0.7071067811865464625, 0.000000000000000000 ) ) ;
#117446 = LINE ( 'NONE', #18117, #71987 ) ;
#117447 = DIRECTION ( 'NONE',  ( -0.7071067811865487940, 0.7071067811865463515, 0.000000000000000000 ) ) ;
#117448 = DIRECTION ( 'NONE',  ( 0.6830127018922181881, 0.6830127018922202975, -0.2588190451025214056 ) ) ;
#117449 = ADVANCED_FACE ( 'NONE', ( #53234 ), #18439, .F. ) ;
#117450 = DIRECTION ( 'NONE',  ( 1.000000000000000000, 0.000000000000000000, 0.000000000000000000 ) ) ;
#117451 = ORIENTED_EDGE ( 'NONE', *, *, #101637, .T. ) ;
#117452 = LINE ( 'NONE', #127654, #115393 ) ;
#117453 = CARTESIAN_POINT ( 'NONE',  ( 0.4892135623730947680, -27.52281430457055578, 5.000000000000000000 ) ) ;
#117454 = CARTESIAN_POINT ( 'NONE',  ( 6.540657738503846907, -2.055000000000000160, 0.000000000000000000 ) ) ;
#117455 = VECTOR ( 'NONE', #74759, 999.9999999999998863 ) ;
#117456 = ORIENTED_EDGE ( 'NONE', *, *, #88891, .F. ) ;
#117457 = CARTESIAN_POINT ( 'NONE',  ( -12.18398860626900060, 28.73617430169795739, 5.000000000000000000 ) ) ;
#117458 = CARTESIAN_POINT ( 'NONE',  ( 7.171830600776422315, 18.75929247661553489, 4.000000000000000000 ) ) ;
#117459 = VERTEX_POINT ( 'NONE', #138850 ) ;
#117460 = EDGE_CURVE ( 'NONE', #65131, #65842, #51126, .T. ) ;
#117462 = EDGE_LOOP ( 'NONE', ( #22492, #17919, #80468, #128512, #60462 ) ) ;
#117461 = DIRECTION ( 'NONE',  ( -0.5735764363510503783, -0.8191520442889886899, 0.000000000000000000 ) ) ;
#117463 = EDGE_CURVE ( 'NONE', #57964, #51885, #40267, .T. ) ;
#117464 = LINE ( 'NONE', #52230, #58631 ) ;
#117465 = CARTESIAN_POINT ( 'NONE',  ( 34.92499999999998295, -5.405284025385218349, -5.470147491473914769 ) ) ;
#117466 = VERTEX_POINT ( 'NONE', #119899 ) ;
#117467 = CARTESIAN_POINT ( 'NONE',  ( 30.24169458425169310, 0.7592924766157138627, 14.37146558664976048 ) ) ;
#117468 = ADVANCED_FACE ( 'NONE', ( #83773 ), #140957, .F. ) ;
#117469 = LINE ( 'NONE', #138547, #105400 ) ;
#117470 = CARTESIAN_POINT ( 'NONE',  ( -34.49999999999976552, 18.05432934483075513, 4.994342998332167660 ) ) ;
#117471 = VECTOR ( 'NONE', #61641, 1000.000000000000000 ) ;
#117472 = FACE_OUTER_BOUND ( 'NONE', #62262, .T. ) ;
#117473 = FACE_OUTER_BOUND ( 'NONE', #12476, .T. ) ;
#117474 = LINE ( 'NONE', #97134, #127729 ) ;
#117475 = CARTESIAN_POINT ( 'NONE',  ( 47.22916666666665719, 7.950000000000001954, -2.130196079827421762 ) ) ;
#117476 = DIRECTION ( 'NONE',  ( -0.000000000000000000, -0.3543493200069152693, 0.9351131265310292928 ) ) ;
#117477 = EDGE_CURVE ( 'NONE', #30341, #40406, #85154, .T. ) ;
#117478 = CARTESIAN_POINT ( 'NONE',  ( 14.74000000000000021, 9.521314400968980422E-16, 0.000000000000000000 ) ) ;
#117479 = CARTESIAN_POINT ( 'NONE',  ( 54.48921356237310221, -27.52281430457093236, 5.000000000000000000 ) ) ;
#117480 = LINE ( 'NONE', #18154, #102140 ) ;
#117481 = DIRECTION ( 'NONE',  ( 1.000000000000000000, 0.000000000000000000, 0.000000000000000000 ) ) ;
#117482 = ORIENTED_EDGE ( 'NONE', *, *, #71108, .T. ) ;
#117483 = ORIENTED_EDGE ( 'NONE', *, *, #22690, .F. ) ;
#117484 = ORIENTED_EDGE ( 'NONE', *, *, #118336, .T. ) ;
#117485 = CARTESIAN_POINT ( 'NONE',  ( 111.3958333333333428, -2.130196079827427091, 7.949999999999999289 ) ) ;
#117486 = ORIENTED_EDGE ( 'NONE', *, *, #2891, .F. ) ;
#117487 = ORIENTED_EDGE ( 'NONE', *, *, #65353, .T. ) ;
#117488 = ORIENTED_EDGE ( 'NONE', *, *, #61599, .T. ) ;
#117489 = EDGE_CURVE ( 'NONE', #75592, #51436, #7584, .T. ) ;
#117490 = CARTESIAN_POINT ( 'NONE',  ( 18.18398860626898994, 28.73617430169800002, 5.000000000000000000 ) ) ;
#117491 = CARTESIAN_POINT ( 'NONE',  ( 18.29974487139159223, -27.71228299555219010, 4.000000000000000000 ) ) ;
#117492 = ORIENTED_EDGE ( 'NONE', *, *, #56820, .T. ) ;
#117493 = STYLED_ITEM ( 'NONE', ( #61507 ), #124881 ) ;
#117494 = CARTESIAN_POINT ( 'NONE',  ( 32.99999999999976552, -19.22509904557633575, 1.855685503482255250 ) ) ;
#117495 = LINE ( 'NONE', #62450, #141254 ) ;
#117496 = PRESENTATION_LAYER_ASSIGNMENT (  '', '', ( #89683 ) ) ;
#117497 = CARTESIAN_POINT ( 'NONE',  ( 21.48921356237309155, -27.52281430457070499, 5.000000000000000000 ) ) ;
#117498 = CARTESIAN_POINT ( 'NONE',  ( 18.93838080770422039, 22.22500000000000142, -15.41084850694827324 ) ) ;
#117499 = CARTESIAN_POINT ( 'NONE',  ( 100.1879301918980900, 6.110000000000002984, -1.637169565754156730 ) ) ;
#117500 = ORIENTED_EDGE ( 'NONE', *, *, #110234, .F. ) ;
#117501 = LINE ( 'NONE', #40696, #23238 ) ;
#117502 = DIRECTION ( 'NONE',  ( 0.6830127018922180770, -0.6830127018922204085, -0.2588190451025213501 ) ) ;
#117503 = EDGE_CURVE ( 'NONE', #64975, #59481, #72915, .T. ) ;
#117504 =( LENGTH_UNIT ( ) NAMED_UNIT ( * ) SI_UNIT ( .MILLI., .METRE. ) );
#117505 = CARTESIAN_POINT ( 'NONE',  ( 0.005480084712502889671, 28.92564299267938210, 4.000000000000000000 ) ) ;
#117506 = AXIS2_PLACEMENT_3D ( 'NONE', #41275, #31840, #132620 ) ;
#117507 = CARTESIAN_POINT ( 'NONE',  ( 3.000000000000000000, -7.600000000000061817, 31.92499999999998295 ) ) ;
#117508 = SURFACE_STYLE_USAGE ( .BOTH. , #17499 ) ;
#117509 = CARTESIAN_POINT ( 'NONE',  ( 40.03752705046288440, -9.735942053221456900E-16, 7.949999999999998401 ) ) ;
#117510 = EDGE_CURVE ( 'NONE', #55935, #8580, #95321, .T. ) ;
#117511 = DIRECTION ( 'NONE',  ( 1.000000000000000000, 0.000000000000000000, 6.938893903907222067E-15 ) ) ;
#117512 = LINE ( 'NONE', #18186, #39329 ) ;
#117513 = ORIENTED_EDGE ( 'NONE', *, *, #73489, .F. ) ;
#117514 = EDGE_LOOP ( 'NONE', ( #23822, #24223, #31423, #22106, #117063 ) ) ;
#117515 = CARTESIAN_POINT ( 'NONE',  ( 125.7087635252314470, -7.482591942790329030E-16, 6.110000000000001208 ) ) ;
#117516 = VERTEX_POINT ( 'NONE', #42406 ) ;
#117517 = CARTESIAN_POINT ( 'NONE',  ( 0.4892135623730947680, -27.52281430457055578, 5.000000000000000000 ) ) ;
#117518 = CARTESIAN_POINT ( 'NONE',  ( -36.88837638105219696, 9.759292476615614831, 17.35367589129221244 ) ) ;
#117519 = VECTOR ( 'NONE', #58975, 999.9999999999998863 ) ;
#117520 = CARTESIAN_POINT ( 'NONE',  ( 0.000000000000000000, 0.000000000000000000, 5.000000000000000000 ) ) ;
#117521 = CARTESIAN_POINT ( 'NONE',  ( -5.510786437626906675, -27.52281430457051314, 5.000000000000000000 ) ) ;
#117522 = LINE ( 'NONE', #62470, #55913 ) ;
#117523 = DIRECTION ( 'NONE',  ( -1.000000000000000000, 0.000000000000000000, 0.000000000000000000 ) ) ;
#117524 = CARTESIAN_POINT ( 'NONE',  ( 124.5995968585647944, -6.109999999999997655, -1.637169565754160283 ) ) ;
#117525 = ORIENTED_EDGE ( 'NONE', *, *, #21743, .F. ) ;
#117526 = EDGE_CURVE ( 'NONE', #44496, #128691, #139586, .T. ) ;
#117527 = DIRECTION ( 'NONE',  ( 0.7071067811865486830, -0.7071067811865464625, -0.000000000000000000 ) ) ;
#117528 = VERTEX_POINT ( 'NONE', #96028 ) ;
#117529 = DIRECTION ( 'NONE',  ( -0.7071067811865486830, -0.7071067811865464625, -0.000000000000000000 ) ) ;
#117530 = CARTESIAN_POINT ( 'NONE',  ( 27.75860074219777118, 21.72500000000000142, 5.000000000000000000 ) ) ;
#117531 = CARTESIAN_POINT ( 'NONE',  ( 30.18398860626900060, 28.73617430169808173, 5.000000000000000000 ) ) ;
#117532 = DIRECTION ( 'NONE',  ( -0.6830127018922180770, -0.6830127018922204085, -0.2588190451025214056 ) ) ;
#117533 = ORIENTED_EDGE ( 'NONE', *, *, #16872, .T. ) ;
#117534 = CARTESIAN_POINT ( 'NONE',  ( 45.93793019189810423, -6.110000000000001208, 1.637169565754158951 ) ) ;
#117535 = ADVANCED_FACE ( 'NONE', ( #19197 ), #97448, .F. ) ;
#117536 = VERTEX_POINT ( 'NONE', #8972 ) ;
#117537 = LINE ( 'NONE', #87083, #63316 ) ;
#117538 = DIRECTION ( 'NONE',  ( 0.7071067811865487940, 0.7071067811865463515, 0.000000000000000000 ) ) ;
#117539 = DIRECTION ( 'NONE',  ( -0.7071067811865487940, 0.7071067811865463515, 0.000000000000000000 ) ) ;
#117540 = MECHANICAL_DESIGN_GEOMETRIC_PRESENTATION_REPRESENTATION (  '', ( #89815 ), #131535 ) ;
#117541 = LINE ( 'NONE', #129154, #78818 ) ;
#117542 = CARTESIAN_POINT ( 'NONE',  ( 48.62043019189811588, 3.055000000000001936, -5.291415217122916737 ) ) ;
#117543 = ORIENTED_EDGE ( 'NONE', *, *, #54600, .F. ) ;
#117544 = FACE_OUTER_BOUND ( 'NONE', #31361, .T. ) ;
#117545 = FACE_OUTER_BOUND ( 'NONE', #34137, .T. ) ;
#117546 = ORIENTED_EDGE ( 'NONE', *, *, #20239, .F. ) ;
#117547 = EDGE_LOOP ( 'NONE', ( #104165, #46719, #5116, #32735 ) ) ;
#117548 = ORIENTED_EDGE ( 'NONE', *, *, #7092, .T. ) ;
#117549 = DIRECTION ( 'NONE',  ( 0.7071067811865487940, 0.7071067811865463515, -0.000000000000000000 ) ) ;
#117550 = EDGE_CURVE ( 'NONE', #81264, #60957, #64857, .T. ) ;
#117551 = ORIENTED_EDGE ( 'NONE', *, *, #11134, .F. ) ;
#117552 = LINE ( 'NONE', #126320, #15845 ) ;
#117553 = CARTESIAN_POINT ( 'NONE',  ( -9.299744871391588674, -27.71228299555212971, 4.000000000000000000 ) ) ;
#117554 = CARTESIAN_POINT ( 'NONE',  ( -9.345819385248065103, 22.22500000000000142, 14.69290773491317026 ) ) ;
#117555 = EDGE_CURVE ( 'NONE', #84791, #65885, #130842, .T. ) ;
#117556 = FACE_BOUND ( 'NONE', #30725, .T. ) ;
#117557 = CARTESIAN_POINT ( 'NONE',  ( 3.302882771356424829, -48.98543874033773449, 39.51758185027073722 ) ) ;
#117559 = ADVANCED_FACE ( 'NONE', ( #31505 ), #140267, .F. ) ;
#117558 = DIRECTION ( 'NONE',  ( -1.000000000000000000, -1.224606353822377258E-16, -0.000000000000000000 ) ) ;
#117560 = ORIENTED_EDGE ( 'NONE', *, *, #136347, .F. ) ;
#117561 = CARTESIAN_POINT ( 'NONE',  ( 78.18398860626899705, 28.73617430169841924, 5.000000000000000000 ) ) ;
#117562 = ORIENTED_EDGE ( 'NONE', *, *, #68444, .F. ) ;
#117563 = VERTEX_POINT ( 'NONE', #30056 ) ;
#117564 = CARTESIAN_POINT ( 'NONE',  ( 0.000000000000000000, 0.000000000000000000, 0.000000000000000000 ) ) ;
#117565 = ORIENTED_EDGE ( 'NONE', *, *, #120562, .F. ) ;
#117566 = CARTESIAN_POINT ( 'NONE',  ( 52.55793019189810877, 6.110000000000000320, -1.637169565754156064 ) ) ;
#117567 = ORIENTED_EDGE ( 'NONE', *, *, #77483, .T. ) ;
#117568 = VECTOR ( 'NONE', #88928, 1000.000000000000000 ) ;
#117569 = DIRECTION ( 'NONE',  ( 0.6830127018922180770, -0.6830127018922204085, -0.2588190451025213501 ) ) ;
#117570 = DIRECTION ( 'NONE',  ( 0.6830127018922180770, -0.6830127018922204085, -0.2588190451025213501 ) ) ;
#117571 = ORIENTED_EDGE ( 'NONE', *, *, #105988, .F. ) ;
#117572 = DIRECTION ( 'NONE',  ( 0.6830127018922180770, -0.6830127018922204085, -0.2588190451025213501 ) ) ;
#117573 = EDGE_CURVE ( 'NONE', #68343, #82336, #106169, .T. ) ;
#117574 = VECTOR ( 'NONE', #77088, 1000.000000000000000 ) ;
#117575 = CARTESIAN_POINT ( 'NONE',  ( -63.18398860626900415, 28.73617430169831621, 5.000000000000000000 ) ) ;
#117576 = DIRECTION ( 'NONE',  ( 0.000000000000000000, 0.000000000000000000, 1.000000000000000000 ) ) ;
#117577 = LINE ( 'NONE', #137239, #114078 ) ;
#117578 = DIRECTION ( 'NONE',  ( -0.7071067811865486830, -0.7071067811865464625, 0.000000000000000000 ) ) ;
#117579 = VERTEX_POINT ( 'NONE', #63452 ) ;
#117580 = ORIENTED_EDGE ( 'NONE', *, *, #114378, .F. ) ;
#117581 = CARTESIAN_POINT ( 'NONE',  ( 19.58747294953710849, -6.094999999999989981, 3.732111120401553285E-16 ) ) ;
#117583 = CARTESIAN_POINT ( 'NONE',  ( 36.18398860626899705, 28.73617430169812437, 5.000000000000000000 ) ) ;
#117582 = AXIS2_PLACEMENT_3D ( 'NONE', #128695, #54026, #51870 ) ;
#117584 = ORIENTED_EDGE ( 'NONE', *, *, #47220, .T. ) ;
#117585 = VERTEX_POINT ( 'NONE', #107620 ) ;
#117587 = ORIENTED_EDGE ( 'NONE', *, *, #118722, .T. ) ;
#117586 = VECTOR ( 'NONE', #28638, 1000.000000000000000 ) ;
#117588 = FACE_OUTER_BOUND ( 'NONE', #48255, .T. ) ;
#117589 = CARTESIAN_POINT ( 'NONE',  ( 10.77958563595370833, 4.584330080086930965E-16, 0.000000000000000000 ) ) ;
#117590 = ORIENTED_EDGE ( 'NONE', *, *, #137147, .F. ) ;
#117591 = DIRECTION ( 'NONE',  ( -0.000000000000000000, 0.3543493200069153248, 0.9351131265310292928 ) ) ;
#117592 = AXIS2_PLACEMENT_3D ( 'NONE', #83582, #28484, #116897 ) ;
#117593 = VECTOR ( 'NONE', #6465, 1000.000000000000227 ) ;
#117594 = FACE_OUTER_BOUND ( 'NONE', #79092, .T. ) ;
#117595 = CARTESIAN_POINT ( 'NONE',  ( 8.087903141435219823, 6.871911579029515771, 3.967499999999989146 ) ) ;
#117596 = ADVANCED_FACE ( 'NONE', ( #52528 ), #96712, .F. ) ;
#117597 = DIRECTION ( 'NONE',  ( 0.000000000000000000, -1.000000000000000000, 0.000000000000000000 ) ) ;
#117598 = ORIENTED_EDGE ( 'NONE', *, *, #86051, .F. ) ;
#117599 = DIRECTION ( 'NONE',  ( -0.5735764363510507113, 0.8191520442889885789, 1.003171929053520926E-16 ) ) ;
#117600 = ADVANCED_FACE ( 'NONE', ( #24201 ), #43808, .F. ) ;
#117601 = CARTESIAN_POINT ( 'NONE',  ( 28.17183060077628198, 12.75929247661558286, 4.000000000000000000 ) ) ;
#117602 = CARTESIAN_POINT ( 'NONE',  ( 6.299744871391586898, -27.71228299555210484, 4.000000000000000000 ) ) ;
#117604 = EDGE_LOOP ( 'NONE', ( #19856, #23827, #75780, #67676, #63393 ) ) ;
#117603 = DIRECTION ( 'NONE',  ( -0.3543493200069162685, -0.000000000000000000, -0.9351131265310288487 ) ) ;
#117605 = DIRECTION ( 'NONE',  ( 1.000000000000000000, 0.000000000000000000, 0.000000000000000000 ) ) ;
#117606 = ORIENTED_EDGE ( 'NONE', *, *, #64001, .F. ) ;
#117607 = LINE ( 'NONE', #87160, #63572 ) ;
#117608 = DIRECTION ( 'NONE',  ( -0.000000000000000000, 0.000000000000000000, 1.000000000000000000 ) ) ;
#117609 = EDGE_CURVE ( 'NONE', #66395, #129172, #133676, .T. ) ;
#117610 = EDGE_CURVE ( 'NONE', #95492, #99130, #43108, .T. ) ;
#117611 = CARTESIAN_POINT ( 'NONE',  ( 0.000000000000000000, 0.000000000000000000, 5.000000000000000000 ) ) ;
#117612 = ORIENTED_EDGE ( 'NONE', *, *, #128465, .T. ) ;
#117613 = PLANE ( 'NONE',  #49617 ) ;
#117614 = LINE ( 'NONE', #40814, #102095 ) ;
#117615 = CARTESIAN_POINT ( 'NONE',  ( 7.326124847093153925, -2.055000000000000160, 0.000000000000000000 ) ) ;
#117616 = ORIENTED_EDGE ( 'NONE', *, *, #19483, .T. ) ;
#117617 = CARTESIAN_POINT ( 'NONE',  ( 18.79653912142945060, 4.333342374871280669E-31, 2.500000000000000444 ) ) ;
#117618 = FACE_OUTER_BOUND ( 'NONE', #21632, .T. ) ;
#117620 = AXIS2_PLACEMENT_3D ( 'NONE', #75605, #30681, #20472 ) ;
#117619 = CARTESIAN_POINT ( 'NONE',  ( 11.20710678118647330, 12.75929247661558996, 5.000000000000000000 ) ) ;
#117621 = LINE ( 'NONE', #40141, #105001 ) ;
#117622 = EDGE_CURVE ( 'NONE', #133767, #87458, #33530, .T. ) ;
#117623 = DIRECTION ( 'NONE',  ( 0.000000000000000000, 0.000000000000000000, 1.000000000000000000 ) ) ;
#117624 = ORIENTED_EDGE ( 'NONE', *, *, #62882, .F. ) ;
#117625 = EDGE_CURVE ( 'NONE', #103619, #100067, #76453, .T. ) ;
#117626 = ORIENTED_EDGE ( 'NONE', *, *, #86751, .F. ) ;
#117627 = VECTOR ( 'NONE', #90531, 999.9999999999998863 ) ;
#117628 = DIRECTION ( 'NONE',  ( -0.7071067811865486830, -0.7071067811865464625, 0.000000000000000000 ) ) ;
#117629 = DIRECTION ( 'NONE',  ( 0.000000000000000000, 0.000000000000000000, 1.000000000000000000 ) ) ;
#117630 = CARTESIAN_POINT ( 'NONE',  ( 15.29123647476855297, -9.717572351234235426E-16, -7.934999999999990727 ) ) ;
#117631 = FACE_OUTER_BOUND ( 'NONE', #52919, .T. ) ;
#117632 = DIRECTION ( 'NONE',  ( 1.000000000000000000, 0.000000000000000000, 0.000000000000000000 ) ) ;
#117633 = ADVANCED_FACE ( 'NONE', ( #45971 ), #98877, .F. ) ;
#117634 = DIRECTION ( 'NONE',  ( -0.6830127018922181881, 0.6830127018922202975, -0.2588190451025214056 ) ) ;
#117635 = VERTEX_POINT ( 'NONE', #77868 ) ;
#117636 = LINE ( 'NONE', #60475, #46511 ) ;
#117637 = DIRECTION ( 'NONE',  ( 0.000000000000000000, -1.000000000000000000, 0.000000000000000000 ) ) ;
#117638 = CARTESIAN_POINT ( 'NONE',  ( 34.49999999999976552, -17.56887692260763245, 4.000000000000000000 ) ) ;
#117639 = EDGE_CURVE ( 'NONE', #38181, #22073, #90609, .T. ) ;
#117640 = VECTOR ( 'NONE', #37580, 1000.000000000000227 ) ;
#117641 = FACE_OUTER_BOUND ( 'NONE', #36718, .T. ) ;
#117642 = CARTESIAN_POINT ( 'NONE',  ( 49.78709685856478018, 3.054999999999997939, 5.291415217122920289 ) ) ;
#117643 = LINE ( 'NONE', #96597, #48750 ) ;
#117644 = VECTOR ( 'NONE', #102544, 1000.000000000000000 ) ;
#117645 = ORIENTED_EDGE ( 'NONE', *, *, #120706, .F. ) ;
#117646 = FACE_OUTER_BOUND ( 'NONE', #111981, .T. ) ;
#117647 = ORIENTED_EDGE ( 'NONE', *, *, #27169, .T. ) ;
#117648 = ORIENTED_EDGE ( 'NONE', *, *, #81637, .T. ) ;
#117649 = EDGE_CURVE ( 'NONE', #102047, #77315, #132988, .T. ) ;
#117650 = DIRECTION ( 'NONE',  ( 0.7071067811865487940, 0.7071067811865463515, 0.000000000000000000 ) ) ;
#117651 = CARTESIAN_POINT ( 'NONE',  ( 22.82816939922338051, -11.24070752338416668, 4.000000000000000000 ) ) ;
#117652 = DIRECTION ( 'NONE',  ( 0.3543493200069164351, 2.781805975412904658E-17, -0.9351131265310288487 ) ) ;
#117653 = LINE ( 'NONE', #127883, #27847 ) ;
#117654 = CARTESIAN_POINT ( 'NONE',  ( 82.52083333333331439, 7.949999999999998401, 2.130196079827431532 ) ) ;
#117655 = FACE_OUTER_BOUND ( 'NONE', #113988, .T. ) ;
#117656 = ORIENTED_EDGE ( 'NONE', *, *, #100819, .F. ) ;
#117657 = EDGE_CURVE ( 'NONE', #109897, #64492, #22722, .T. ) ;
#117658 = CARTESIAN_POINT ( 'NONE',  ( 60.48921356237309510, -27.52281430457097500, 5.000000000000000000 ) ) ;
#117659 = CARTESIAN_POINT ( 'NONE',  ( 1.499999999999987566, -1.533600742197726463, 5.000000000000000000 ) ) ;
#117660 = EDGE_CURVE ( 'NONE', #16867, #31094, #111176, .T. ) ;
#117661 = PLANE ( 'NONE',  #31016 ) ;
#117662 = FACE_OUTER_BOUND ( 'NONE', #97789, .T. ) ;
#117663 = FACE_OUTER_BOUND ( 'NONE', #49, .T. ) ;
#117664 = CARTESIAN_POINT ( 'NONE',  ( 14.51078643762690490, -27.52281430457045275, 5.000000000000000000 ) ) ;
#117665 = CARTESIAN_POINT ( 'NONE',  ( 70.07919371712955581, 3.975000000000002753, -6.884901960086283523 ) ) ;
#117666 = EDGE_CURVE ( 'NONE', #45590, #84277, #111931, .T. ) ;
#117667 = FACE_OUTER_BOUND ( 'NONE', #47538, .T. ) ;
#117668 = VERTEX_POINT ( 'NONE', #1676 ) ;
#117669 = ORIENTED_EDGE ( 'NONE', *, *, #57102, .F. ) ;
#117670 = VECTOR ( 'NONE', #51658, 1000.000000000000227 ) ;
#117671 = CARTESIAN_POINT ( 'NONE',  ( 56.12499999999999289, -7.950000000000000178, -4.867971026610729436E-16 ) ) ;
#117672 = LINE ( 'NONE', #138043, #86429 ) ;
#117673 = CARTESIAN_POINT ( 'NONE',  ( 0.000000000000000000, -21.72500000000000142, 4.500000000000000888 ) ) ;
#117674 = DIRECTION ( 'NONE',  ( 0.7071067811865487940, 0.7071067811865463515, 0.000000000000000000 ) ) ;
#117675 = EDGE_LOOP ( 'NONE', ( #69727, #134291, #47533, #71449 ) ) ;
#117676 = PLANE ( 'NONE',  #60742 ) ;
#117677 = CARTESIAN_POINT ( 'NONE',  ( 43.31293019189810423, -1.637169565754159617, -6.110000000000001208 ) ) ;
#117678 = ORIENTED_EDGE ( 'NONE', *, *, #124622, .T. ) ;
#117679 = CARTESIAN_POINT ( 'NONE',  ( 8.816011393731004731, 28.73617430169781173, 5.000000000000000000 ) ) ;
#117680 = ORIENTED_EDGE ( 'NONE', *, *, #115619, .F. ) ;
#117681 = ORIENTED_EDGE ( 'NONE', *, *, #129563, .F. ) ;
#117682 = FACE_OUTER_BOUND ( 'NONE', #127722, .T. ) ;
#117683 = VECTOR ( 'NONE', #80360, 1000.000000000000000 ) ;
#117684 = VECTOR ( 'NONE', #109441, 1000.000000000000000 ) ;
#117685 = PLANE ( 'NONE',  #73178 ) ;
#117686 = CARTESIAN_POINT ( 'NONE',  ( -6.489213562373093325, -27.52281430457059841, 5.000000000000000000 ) ) ;
#117687 = VECTOR ( 'NONE', #102629, 1000.000000000000000 ) ;
#117688 = CARTESIAN_POINT ( 'NONE',  ( 16.49999999999988987, -7.533600742197658739, 5.000000000000000000 ) ) ;
#117689 = CARTESIAN_POINT ( 'NONE',  ( -23.29298673570678702, -21.74070752338405299, 4.999753212805217117 ) ) ;
#117691 = CIRCLE ( 'NONE', #41343, 2.500000000000000888 ) ;
#117690 = DIRECTION ( 'NONE',  ( 0.7071067811865487940, 0.7071067811865463515, 0.000000000000000000 ) ) ;
#117693 = ORIENTED_EDGE ( 'NONE', *, *, #19486, .F. ) ;
#117692 = CARTESIAN_POINT ( 'NONE',  ( -16.93298150401930258, -0.6090650756136195554, -34.87030803381578181 ) ) ;
#117694 = CARTESIAN_POINT ( 'NONE',  ( 15.70710678118643955, 8.259292476615634371, 5.000000000000000000 ) ) ;
#117695 = CARTESIAN_POINT ( 'NONE',  ( 25.39999999999999858, -5.520864266206504263E-14, 33.92499999999998295 ) ) ;
#117696 = CARTESIAN_POINT ( 'NONE',  ( -45.48921356237309510, -27.52281430457087197, 5.000000000000000000 ) ) ;
#117697 = VECTOR ( 'NONE', #11493, 1000.000000000000000 ) ;
#117698 = CARTESIAN_POINT ( 'NONE',  ( -29.34505516254599655, 5.259292476615672562, 12.77922209995886682 ) ) ;
#117699 = VECTOR ( 'NONE', #80779, 999.9999999999998863 ) ;
#117700 = ORIENTED_EDGE ( 'NONE', *, *, #101062, .T. ) ;
#117701 = ORIENTED_EDGE ( 'NONE', *, *, #15473, .F. ) ;
#117702 = PLANE ( 'NONE',  #31519 ) ;
#117703 = CARTESIAN_POINT ( 'NONE',  ( 72.09959685856479439, -6.109999999999997655, -1.637169565754160283 ) ) ;
#117704 = CARTESIAN_POINT ( 'NONE',  ( 9.994118527364397764, -2.500000000000000444, 3.061616997868384127E-16 ) ) ;
#117705 = CARTESIAN_POINT ( 'NONE',  ( -32.99451991528749062, 28.92564299267960948, 4.000000000000000000 ) ) ;
#117706 = CARTESIAN_POINT ( 'NONE',  ( -34.49999999999976552, 1.464255608400471642, 4.994342998332163219 ) ) ;
#117707 = VERTEX_POINT ( 'NONE', #35097 ) ;
#117708 = VERTEX_POINT ( 'NONE', #79339 ) ;
#117709 = VECTOR ( 'NONE', #85031, 1000.000000000000000 ) ;
#117710 = CARTESIAN_POINT ( 'NONE',  ( 75.03752705046288440, -9.735942053221456900E-16, 7.949999999999998401 ) ) ;
#117711 = DIRECTION ( 'NONE',  ( 0.7071067811865487940, -0.7071067811865463515, 0.000000000000000000 ) ) ;
#117712 = ORIENTED_EDGE ( 'NONE', *, *, #54703, .T. ) ;
#117713 =( BOUNDED_CURVE ( )  B_SPLINE_CURVE ( 3, ( #93356, #104937, #3461, #49872 ),
 .UNSPECIFIED., .F., .F. ) 
 B_SPLINE_CURVE_WITH_KNOTS ( ( 4, 4 ),
 ( 5.390251506879594423, 5.422326034329064903 ),
 .UNSPECIFIED. ) 
 CURVE ( )  GEOMETRIC_REPRESENTATION_ITEM ( )  RATIONAL_B_SPLINE_CURVE ( ( 1.000000000000000000, 0.9999142705615216009, 0.9999142705615216009, 1.000000000000000000 ) ) 
 REPRESENTATION_ITEM ( '' )  );
#117714 = EDGE_LOOP ( 'NONE', ( #59273, #98021, #17678, #18585 ) ) ;
#117715 = AXIS2_PLACEMENT_3D ( 'NONE', #111264, #99680, #58390 ) ;
#117716 = LINE ( 'NONE', #16258, #44410 ) ;
#117717 = EDGE_LOOP ( 'NONE', ( #66523, #104920, #7108, #37215 ) ) ;
#117718 = CARTESIAN_POINT ( 'NONE',  ( 18.32816939922338761, -18.74070752338410273, 4.000000000000000000 ) ) ;
#117719 = VECTOR ( 'NONE', #97140, 1000.000000000000000 ) ;
#117720 = VECTOR ( 'NONE', #12109, 999.9999999999998863 ) ;
#117722 = CARTESIAN_POINT ( 'NONE',  ( 50.99451991528749062, 28.92564299267973738, 4.000000000000000000 ) ) ;
#117721 = VECTOR ( 'NONE', #107952, 1000.000000000000000 ) ;
#117723 = EDGE_CURVE ( 'NONE', #91253, #38197, #127060, .T. ) ;
#117724 = FACE_BOUND ( 'NONE', #82962, .T. ) ;
#117725 = CARTESIAN_POINT ( 'NONE',  ( 0.000000000000000000, 0.000000000000000000, -40.00000000000000000 ) ) ;
#117726 = CARTESIAN_POINT ( 'NONE',  ( 2.999999999999981792, -9.033600742197648970, 5.000000000000000000 ) ) ;
#117727 = EDGE_CURVE ( 'NONE', #82657, #67930, #125662, .T. ) ;
#117728 = DIRECTION ( 'NONE',  ( -0.6830127018922180770, 0.6830127018922202975, -0.2588190451025213501 ) ) ;
#117730 = EDGE_LOOP ( 'NONE', ( #48124, #42260, #142979, #116074 ) ) ;
#117729 = CARTESIAN_POINT ( 'NONE',  ( 54.18398860626899705, 28.73617430169825226, 5.000000000000000000 ) ) ;
#117731 = VECTOR ( 'NONE', #77598, 1000.000000000000227 ) ;
#117732 = VECTOR ( 'NONE', #76816, 1000.000000000000000 ) ;
#117733 = CONTEXT_DEPENDENT_SHAPE_REPRESENTATION ( #10545, #86399 ) ;
#117734 = ORIENTED_EDGE ( 'NONE', *, *, #4938, .F. ) ;
#117735 = ORIENTED_EDGE ( 'NONE', *, *, #97459, .F. ) ;
#117736 = CARTESIAN_POINT ( 'NONE',  ( 84.93293019189812298, 1.637169565754156508, 6.110000000000000320 ) ) ;
#117737 = EDGE_LOOP ( 'NONE', ( #119328, #27228, #52810, #82831 ) ) ;
#117738 = DIRECTION ( 'NONE',  ( 0.6830127018922180770, 0.6830127018922202975, -0.2588190451025213501 ) ) ;
#117739 = EDGE_CURVE ( 'NONE', #103883, #86102, #49547, .T. ) ;
#117740 = LINE ( 'NONE', #40940, #90648 ) ;
#117741 = LINE ( 'NONE', #18425, #37476 ) ;
#117742 = AXIS2_PLACEMENT_3D ( 'NONE', #14048, #68482, #36534 ) ;
#117743 = ADVANCED_FACE ( 'NONE', ( #27751 ), #101749, .F. ) ;
#117744 = DIRECTION ( 'NONE',  ( -0.3543493200069162685, -0.000000000000000000, -0.9351131265310288487 ) ) ;
#117745 = DIRECTION ( 'NONE',  ( 0.6830127018922180770, -0.6830127018922204085, -0.2588190451025213501 ) ) ;
#117746 = CARTESIAN_POINT ( 'NONE',  ( 26.67183060077628909, 14.25929247661557220, 4.000000000000000000 ) ) ;
#117747 = DIRECTION ( 'NONE',  ( 0.7071067811865487940, -0.7071067811865463515, 0.000000000000000000 ) ) ;
#117748 = DIRECTION ( 'NONE',  ( -0.7071067811865486830, 0.7071067811865464625, 0.000000000000000000 ) ) ;
#117749 = LINE ( 'NONE', #39538, #118721 ) ;
#117750 = CARTESIAN_POINT ( 'NONE',  ( 54.48921356237310221, -27.52281430457093236, 5.000000000000000000 ) ) ;
#117751 = EDGE_CURVE ( 'NONE', #36106, #51825, #21147, .T. ) ;
#117752 = CARTESIAN_POINT ( 'NONE',  ( -2.999999999999981792, -16.02097659208072145, -11.96015758381207839 ) ) ;
#117753 = ORIENTED_EDGE ( 'NONE', *, *, #39946, .T. ) ;
#117754 = LINE ( 'NONE', #64856, #24070 ) ;
#117755 = CARTESIAN_POINT ( 'NONE',  ( -33.18398860626899705, 28.73617430169810305, 5.000000000000000000 ) ) ;
#117756 = EDGE_LOOP ( 'NONE', ( #22917, #18659, #14128 ) ) ;
#117757 = ORIENTED_EDGE ( 'NONE', *, *, #18869, .T. ) ;
#117758 = ORIENTED_EDGE ( 'NONE', *, *, #113178, .F. ) ;
#117759 = CARTESIAN_POINT ( 'NONE',  ( 32.81293019189809002, -1.637169565754159617, -6.110000000000001208 ) ) ;
#117760 = EDGE_CURVE ( 'NONE', #125114, #100892, #122381, .T. ) ;
#117761 = ORIENTED_EDGE ( 'NONE', *, *, #35765, .T. ) ;
#117762 = CARTESIAN_POINT ( 'NONE',  ( 17.98330628287043353, 6.094999999999991758, 1.633150327867687102 ) ) ;
#117763 = CARTESIAN_POINT ( 'NONE',  ( 11.43556760655506821, 8.373926597364643953, -27.85776518686094860 ) ) ;
#117764 = VERTEX_POINT ( 'NONE', #104602 ) ;
#117765 = CARTESIAN_POINT ( 'NONE',  ( 18.51789069628991768, -2.771357050275779610, 4.325358181756080000 ) ) ;
#117766 = ADVANCED_FACE ( 'NONE', ( #14005 ), #82872, .T. ) ;
#117767 = VERTEX_POINT ( 'NONE', #59696 ) ;
#117768 = DIRECTION ( 'NONE',  ( 0.6830127018922181881, 0.6830127018922202975, -0.2588190451025214056 ) ) ;
#117769 = FACE_OUTER_BOUND ( 'NONE', #3759, .T. ) ;
#117771 = ORIENTED_EDGE ( 'NONE', *, *, #73425, .F. ) ;
#117770 = DIRECTION ( 'NONE',  ( 0.7071067811865486830, -0.7071067811865464625, -0.000000000000000000 ) ) ;
#117772 = ORIENTED_EDGE ( 'NONE', *, *, #133253, .F. ) ;
#117773 = DIRECTION ( 'NONE',  ( 0.7071067811865487940, 0.7071067811865463515, -0.000000000000000000 ) ) ;
#117774 = EDGE_CURVE ( 'NONE', #92653, #53159, #58308, .T. ) ;
#117775 = EDGE_CURVE ( 'NONE', #101752, #103464, #137961, .T. ) ;
#117776 = ORIENTED_EDGE ( 'NONE', *, *, #51807, .F. ) ;
#117777 = PLANE ( 'NONE',  #112954 ) ;
#117778 = ORIENTED_EDGE ( 'NONE', *, *, #53495, .F. ) ;
#117779 = AXIS2_PLACEMENT_3D ( 'NONE', #110150, #129777, #76123 ) ;
#117780 = ORIENTED_EDGE ( 'NONE', *, *, #127406, .F. ) ;
#117781 = EDGE_LOOP ( 'NONE', ( #29647, #35695, #75922, #42053 ) ) ;
#117782 = ORIENTED_EDGE ( 'NONE', *, *, #138310, .F. ) ;
#117783 = CARTESIAN_POINT ( 'NONE',  ( 20.70025512860841133, -27.71228299555191654, 4.000000000000000000 ) ) ;
#117784 = VECTOR ( 'NONE', #141930, 1000.000000000000000 ) ;
#117785 = VECTOR ( 'NONE', #42188, 1000.000000000000000 ) ;
#117786 = EDGE_CURVE ( 'NONE', #118176, #104855, #102490, .T. ) ;
#117787 = CARTESIAN_POINT ( 'NONE',  ( -22.80981832425537448, -18.74070752338408852, 7.910009926591561324 ) ) ;
#117788 = AXIS2_PLACEMENT_3D ( 'NONE', #56663, #89935, #34880 ) ;
#117789 = CARTESIAN_POINT ( 'NONE',  ( -8.999999999999934275, -12.03360074219761522, 5.000000000000000000 ) ) ;
#117790 = EDGE_CURVE ( 'NONE', #109084, #71690, #4506, .T. ) ;
#117791 = CARTESIAN_POINT ( 'NONE',  ( -15.83829387547370438, -6.740707523384212863, 16.75550250614863756 ) ) ;
#117792 = EDGE_LOOP ( 'NONE', ( #16676, #90882, #84248, #65595 ) ) ;
#117793 = ADVANCED_FACE ( 'NONE', ( #126351 ), #4964, .F. ) ;
#117794 = CARTESIAN_POINT ( 'NONE',  ( 28.49999999999981171, -20.94781430457062044, 5.000000000000000000 ) ) ;
#117795 = EDGE_LOOP ( 'NONE', ( #17096, #112361, #118600, #66000 ) ) ;
#117796 = AXIS2_PLACEMENT_3D ( 'NONE', #118181, #21761, #63854 ) ;
#117797 = LINE ( 'NONE', #6173, #132800 ) ;
#117798 = PLANE ( 'NONE',  #46191 ) ;
#117799 = CARTESIAN_POINT ( 'NONE',  ( 13.43359823057990354, 1.153863645259229909, 4.000000000000000000 ) ) ;
#117800 = ORIENTED_EDGE ( 'NONE', *, *, #40694, .T. ) ;
#117801 = CARTESIAN_POINT ( 'NONE',  ( 34.92499999999998295, -17.99387692260784988, 4.000000000000000000 ) ) ;
#117802 = ADVANCED_FACE ( 'NONE', ( #135813 ), #3138, .F. ) ;
#117803 = SURFACE_STYLE_USAGE ( .BOTH. , #98243 ) ;
#117804 = EDGE_LOOP ( 'NONE', ( #116071, #42726, #7393, #3955 ) ) ;
#117805 = ORIENTED_EDGE ( 'NONE', *, *, #39503, .T. ) ;
#117806 = VERTEX_POINT ( 'NONE', #48099 ) ;
#117807 = DIRECTION ( 'NONE',  ( -1.000000000000000000, -0.000000000000000000, -0.000000000000000000 ) ) ;
#117808 = CARTESIAN_POINT ( 'NONE',  ( -45.48921356237309510, -27.52281430457087197, 5.000000000000000000 ) ) ;
#117809 = DIRECTION ( 'NONE',  ( 0.7071067811865487940, 0.7071067811865463515, 0.000000000000000000 ) ) ;
#117810 = AXIS2_PLACEMENT_3D ( 'NONE', #108723, #141385, #140658 ) ;
#117811 =( GEOMETRIC_REPRESENTATION_CONTEXT ( 3 ) GLOBAL_UNCERTAINTY_ASSIGNED_CONTEXT ( ( #14449 ) ) GLOBAL_UNIT_ASSIGNED_CONTEXT ( ( #74958, #51764, #85792 ) ) REPRESENTATION_CONTEXT ( 'NONE', 'WORKASPACE' ) );
#117812 = PLANE ( 'NONE',  #140008 ) ;
#117813 = EDGE_CURVE ( 'NONE', #97758, #83926, #5265, .T. ) ;
#117814 = CARTESIAN_POINT ( 'NONE',  ( 0.1121846519734732428, -51.37040454773406850, -37.49526731630729159 ) ) ;
#117815 = CARTESIAN_POINT ( 'NONE',  ( 71.51626352523145158, -4.472830434245839371, 4.472830434245839371 ) ) ;
#117816 = CARTESIAN_POINT ( 'NONE',  ( -11.29387692260796072, 22.22500000000000142, 4.000000000000000000 ) ) ;
#117818 = DIRECTION ( 'NONE',  ( -0.000000000000000000, 0.000000000000000000, 1.000000000000000000 ) ) ;
#117817 = VECTOR ( 'NONE', #23377, 1000.000000000000227 ) ;
#117819 = CARTESIAN_POINT ( 'NONE',  ( -6.640000000000001457, -40.29840020119761590, 19.55137198191482995 ) ) ;
#117820 = DIRECTION ( 'NONE',  ( -0.000000000000000000, -0.3543493200069152693, 0.9351131265310292928 ) ) ;
#117821 = CARTESIAN_POINT ( 'NONE',  ( 127.4587635252314470, 0.000000000000000000, -6.110000000000001208 ) ) ;
#117822 = ORIENTED_EDGE ( 'NONE', *, *, #14051, .T. ) ;
#117823 = CARTESIAN_POINT ( 'NONE',  ( -0.7928932188134485415, -17.24070752338410628, 5.000000000000000000 ) ) ;
#117824 = PLANE ( 'NONE',  #107796 ) ;
#117825 = ORIENTED_EDGE ( 'NONE', *, *, #34084, .T. ) ;
#117826 = VECTOR ( 'NONE', #93131, 1000.000000000000000 ) ;
#117827 = VECTOR ( 'NONE', #141780, 1000.000000000000000 ) ;
#117828 = VECTOR ( 'NONE', #93244, 999.9999999999998863 ) ;
#117829 = CARTESIAN_POINT ( 'NONE',  ( -51.18398860626899705, 28.73617430169823095, 5.000000000000000000 ) ) ;
#117831 = ORIENTED_EDGE ( 'NONE', *, *, #74482, .T. ) ;
#117830 = CARTESIAN_POINT ( 'NONE',  ( -21.48921356237309155, -27.52281430457070499, 5.000000000000000000 ) ) ;
#117832 = DIRECTION ( 'NONE',  ( -0.7071067811865487940, 0.7071067811865463515, 0.000000000000000000 ) ) ;
#117833 = CARTESIAN_POINT ( 'NONE',  ( -15.48921356237309510, -27.52281430457066236, 5.000000000000000000 ) ) ;
#117834 = ORIENTED_EDGE ( 'NONE', *, *, #92811, .T. ) ;
#117835 = ORIENTED_EDGE ( 'NONE', *, *, #140127, .T. ) ;
#117836 = LINE ( 'NONE', #92004, #106534 ) ;
#117837 = CARTESIAN_POINT ( 'NONE',  ( -6.516654386410399624, 22.22500000000000142, 4.500000000000000888 ) ) ;
#117838 = VECTOR ( 'NONE', #52770, 1000.000000000000227 ) ;
#117839 = CARTESIAN_POINT ( 'NONE',  ( -33.77004279457769798, 21.73644205237998506, 5.000000000000000888 ) ) ;
#117840 = EDGE_CURVE ( 'NONE', #60276, #15282, #14741, .T. ) ;
#117841 = CARTESIAN_POINT ( 'NONE',  ( 95.30836038379619879, 7.949999999999997513, 2.130196079827431088 ) ) ;
#117843 = ADVANCED_FACE ( 'NONE', ( #27037 ), #71284, .T. ) ;
#117842 = DIRECTION ( 'NONE',  ( 0.6830127018922181881, 0.6830127018922202975, -0.2588190451025214056 ) ) ;
#117844 = DIRECTION ( 'NONE',  ( -0.7071067811865486830, -0.7071067811865464625, 0.000000000000000000 ) ) ;
#117845 = EDGE_LOOP ( 'NONE', ( #138292, #91411, #112010, #115554 ) ) ;
#117846 = CARTESIAN_POINT ( 'NONE',  ( 19.73159235450332005, 2.500000000000001332, 0.000000000000000000 ) ) ;
#117847 = LINE ( 'NONE', #16394, #113298 ) ;
#117848 = CARTESIAN_POINT ( 'NONE',  ( 30.18750000000000355, 4.461849672132297329, -4.461849672132302658 ) ) ;
#117849 = VECTOR ( 'NONE', #124089, 1000.000000000000227 ) ;
#117850 = ORIENTED_EDGE ( 'NONE', *, *, #98660, .T. ) ;
#117851 = PLANE ( 'NONE',  #113875 ) ;
#117852 = VERTEX_POINT ( 'NONE', #37210 ) ;
#117853 = CARTESIAN_POINT ( 'NONE',  ( 84.43793019189811844, -6.110000000000001208, 1.637169565754158951 ) ) ;
#117854 = CARTESIAN_POINT ( 'NONE',  ( -11.99999999999991296, 16.55218569542899587, 5.000000000000000000 ) ) ;
#117855 = DIRECTION ( 'NONE',  ( 0.7071067811865486830, -0.7071067811865464625, -0.000000000000000000 ) ) ;
#117856 = ORIENTED_EDGE ( 'NONE', *, *, #102626, .T. ) ;
#117857 = FACE_OUTER_BOUND ( 'NONE', #57431, .T. ) ;
#117858 = CARTESIAN_POINT ( 'NONE',  ( 117.6208603837962272, -6.884901960086286188, 3.974999999999997424 ) ) ;
#117860 = ORIENTED_EDGE ( 'NONE', *, *, #99012, .F. ) ;
#117859 = FACE_OUTER_BOUND ( 'NONE', #55064, .T. ) ;
#117861 = DIRECTION ( 'NONE',  ( 0.7071067811865486830, -0.7071067811865464625, -0.000000000000000000 ) ) ;
#117862 = PLANE ( 'NONE',  #142593 ) ;
#117863 = CARTESIAN_POINT ( 'NONE',  ( 1.689646240811447875, -4.218299268060232698, 4.823946320418484923 ) ) ;
#117864 = CARTESIAN_POINT ( 'NONE',  ( 0.1839886062690032631, 28.73617430169787568, 5.000000000000000000 ) ) ;
#117865 = ORIENTED_EDGE ( 'NONE', *, *, #119877, .F. ) ;
#117866 = ORIENTED_EDGE ( 'NONE', *, *, #20684, .T. ) ;
#117867 = CARTESIAN_POINT ( 'NONE',  ( 76.85459685856477563, -1.637169565754161615, 6.110000000000000320 ) ) ;
#117868 = EDGE_LOOP ( 'NONE', ( #136717, #62702, #138974, #2085 ) ) ;
#117869 = CARTESIAN_POINT ( 'NONE',  ( -16.49999999999988987, 1.030536316426491128, -5.498701923753763765 ) ) ;
#117870 = DIRECTION ( 'NONE',  ( -0.7071067811865486830, -0.7071067811865464625, 0.000000000000000000 ) ) ;
#117871 = DIRECTION ( 'NONE',  ( -0.7071067811865487940, 0.7071067811865463515, 0.000000000000000000 ) ) ;
#117872 = ORIENTED_EDGE ( 'NONE', *, *, #19829, .T. ) ;
#117873 = DIRECTION ( 'NONE',  ( -0.6830127018922181881, 0.6830127018922202975, -0.2588190451025214056 ) ) ;
#117874 = DIRECTION ( 'NONE',  ( -0.7071067811865487940, 0.7071067811865463515, 0.000000000000000000 ) ) ;
#117875 = ORIENTED_EDGE ( 'NONE', *, *, #131562, .F. ) ;
#117876 = CARTESIAN_POINT ( 'NONE',  ( -24.91272823266826109, 2.053671025133813277, 5.000000000000000000 ) ) ;
#117877 = VECTOR ( 'NONE', #94377, 1000.000000000000000 ) ;
#117878 = CARTESIAN_POINT ( 'NONE',  ( 5.999999999999960032, -12.41253812416063340, 4.000000000000000000 ) ) ;
#117879 = DIRECTION ( 'NONE',  ( -0.7071067811865486830, 0.7071067811865464625, 0.000000000000000000 ) ) ;
#117880 = VECTOR ( 'NONE', #50052, 1000.000000000000000 ) ;
#117881 = CIRCLE ( 'NONE', #57724, 3.999999999999996447 ) ;
#117882 = AXIS2_PLACEMENT_3D ( 'NONE', #96655, #64077, #86556 ) ;
#117883 = ORIENTED_EDGE ( 'NONE', *, *, #124988, .T. ) ;
#117884 = ORIENTED_EDGE ( 'NONE', *, *, #4928, .T. ) ;
#117886 = EDGE_CURVE ( 'NONE', #115165, #132568, #81460, .T. ) ;
#117885 = AXIS2_PLACEMENT_3D ( 'NONE', #123699, #23642, #67913 ) ;
#117887 = EDGE_CURVE ( 'NONE', #53690, #137228, #8799, .T. ) ;
#117888 = EDGE_CURVE ( 'NONE', #132587, #55809, #75556, .T. ) ;
#117889 = CARTESIAN_POINT ( 'NONE',  ( 27.70710678118635428, -6.740707523384216415, 5.000000000000000000 ) ) ;
#117890 = DIRECTION ( 'NONE',  ( -0.000000000000000000, 0.3543493200069153248, 0.9351131265310292928 ) ) ;
#117891 = LINE ( 'NONE', #73042, #27992 ) ;
#117892 = CARTESIAN_POINT ( 'NONE',  ( 0.000000000000000000, -1.600000000000086020, -34.92499999999998295 ) ) ;
#117893 = VECTOR ( 'NONE', #111627, 1000.000000000000000 ) ;
#117894 = DIRECTION ( 'NONE',  ( 0.000000000000000000, 0.000000000000000000, -1.000000000000000000 ) ) ;
#117895 =( BOUNDED_CURVE ( )  B_SPLINE_CURVE ( 3, ( #80450, #125365, #26054, #134106 ),
 .UNSPECIFIED., .F., .T. ) 
 B_SPLINE_CURVE_WITH_KNOTS ( ( 4, 4 ),
 ( 5.005968288816745826, 5.074607125596321211 ),
 .UNSPECIFIED. ) 
 CURVE ( )  GEOMETRIC_REPRESENTATION_ITEM ( )  RATIONAL_B_SPLINE_CURVE ( ( 1.000000000000000000, 0.9996074310407767616, 0.9996074310407767616, 1.000000000000000000 ) ) 
 REPRESENTATION_ITEM ( '' )  );
#117896 = ADVANCED_FACE ( 'NONE', ( #29879 ), #85688, .F. ) ;
#117897 = EDGE_CURVE ( 'NONE', #39448, #136399, #72750, .T. ) ;
#117898 = CARTESIAN_POINT ( 'NONE',  ( 12.82439460721831104, 4.202752102959690472E-16, 0.000000000000000000 ) ) ;
#117899 = EDGE_LOOP ( 'NONE', ( #28378, #37924, #69162, #129690 ) ) ;
#117900 = ORIENTED_EDGE ( 'NONE', *, *, #6137, .F. ) ;
#117901 = ORIENTED_EDGE ( 'NONE', *, *, #111222, .F. ) ;
#117902 = ADVANCED_FACE ( 'NONE', ( #95862 ), #130665, .T. ) ;
#117903 = ORIENTED_EDGE ( 'NONE', *, *, #54193, .T. ) ;
#117904 = VECTOR ( 'NONE', #123045, 1000.000000000000000 ) ;
#117905 = AXIS2_PLACEMENT_3D ( 'NONE', #9640, #65515, #130760 ) ;
#117906 = LINE ( 'NONE', #51988, #102280 ) ;
#117907 = CARTESIAN_POINT ( 'NONE',  ( 25.01459476339044130, 2.945717840782780428, 4.000000000000000000 ) ) ;
#117908 = ADVANCED_FACE ( 'NONE', ( #94429 ), #125375, .T. ) ;
#117909 = CIRCLE ( 'NONE', #136370, 14.45000000000002238 ) ;
#117910 = SURFACE_STYLE_USAGE ( .BOTH. , #73727 ) ;
#117911 = VERTEX_POINT ( 'NONE', #138680 ) ;
#117912 = CARTESIAN_POINT ( 'NONE',  ( 3.183988606268992161, 28.73617430169789699, 5.000000000000000000 ) ) ;
#117913 = DIRECTION ( 'NONE',  ( -0.7071067811865486830, 0.7071067811865464625, 0.000000000000000000 ) ) ;
#117914 = DIRECTION ( 'NONE',  ( 1.000000000000000000, -0.000000000000000000, -0.000000000000000000 ) ) ;
#117915 = CARTESIAN_POINT ( 'NONE',  ( 1.199999999999999956, 0.5999999999999987566, 4.749999999999999112 ) ) ;
#117916 = ADVANCED_FACE ( 'NONE', ( #83592 ), #31337, .F. ) ;
#117917 = LINE ( 'NONE', #41110, #130172 ) ;
#117918 = ORIENTED_EDGE ( 'NONE', *, *, #35510, .T. ) ;
#117919 = AXIS2_PLACEMENT_3D ( 'NONE', #71914, #6567, #16027 ) ;
#117920 = DIRECTION ( 'NONE',  ( -0.7071067811865486830, -0.7071067811865464625, 0.000000000000000000 ) ) ;
#117921 = CARTESIAN_POINT ( 'NONE',  ( 20.29289321881332242, -9.740707523384179112, 5.000000000000000000 ) ) ;
#117922 = VECTOR ( 'NONE', #143173, 999.9999999999998863 ) ;
#117923 = ORIENTED_EDGE ( 'NONE', *, *, #45314, .F. ) ;
#117924 = LINE ( 'NONE', #62900, #59806 ) ;
#117925 = VERTEX_POINT ( 'NONE', #42227 ) ;
#117926 = LINE ( 'NONE', #62902, #6645 ) ;
#117927 = ORIENTED_EDGE ( 'NONE', *, *, #33758, .F. ) ;
#117929 = VECTOR ( 'NONE', #19815, 1000.000000000000000 ) ;
#117928 = CARTESIAN_POINT ( 'NONE',  ( 74.37543019189810423, -5.291415217122920289, -3.055000000000001492 ) ) ;
#117930 = EDGE_CURVE ( 'NONE', #11288, #123567, #30636, .T. ) ;
#117931 = VERTEX_POINT ( 'NONE', #17574 ) ;
#117932 = ORIENTED_EDGE ( 'NONE', *, *, #42033, .T. ) ;
#117933 = LINE ( 'NONE', #40438, #99838 ) ;
#117934 = DIRECTION ( 'NONE',  ( 0.7071067811865486830, -0.7071067811865464625, -0.000000000000000000 ) ) ;
#117935 = CARTESIAN_POINT ( 'NONE',  ( 113.1670968585647756, -3.055000000000000160, -5.291415217122921177 ) ) ;
#117936 = DIRECTION ( 'NONE',  ( -1.000000000000000000, -1.224606353822377258E-16, -0.000000000000000000 ) ) ;
#117937 = CARTESIAN_POINT ( 'NONE',  ( -4.499999999999955591, 10.08746187583914278, 4.000000000000000000 ) ) ;
#117938 = EDGE_CURVE ( 'NONE', #18953, #27906, #127806, .T. ) ;
#117939 = LINE ( 'NONE', #119381, #30167 ) ;
#117940 = VECTOR ( 'NONE', #79762, 999.9999999999998863 ) ;
#117941 = CARTESIAN_POINT ( 'NONE',  ( -21.48921356237309155, -27.52281430457070499, 5.000000000000000000 ) ) ;
#117942 = CARTESIAN_POINT ( 'NONE',  ( -11.54016161050252975, 18.75929247661552424, 8.305906642995461553 ) ) ;
#117943 = DIRECTION ( 'NONE',  ( 0.000000000000000000, -1.000000000000000000, 0.000000000000000000 ) ) ;
#117945 = ADVANCED_FACE ( 'NONE', ( #6667 ), #62547, .F. ) ;
#117944 = FACE_OUTER_BOUND ( 'NONE', #138870, .T. ) ;
#117946 = ORIENTED_EDGE ( 'NONE', *, *, #106636, .T. ) ;
#117947 = CARTESIAN_POINT ( 'NONE',  ( -39.18398860626899705, 28.73617430169814568, 5.000000000000000000 ) ) ;
#117948 = VERTEX_POINT ( 'NONE', #19724 ) ;
#117949 = ADVANCED_FACE ( 'NONE', ( #73419 ), #107447, .F. ) ;
#117950 = ORIENTED_EDGE ( 'NONE', *, *, #101886, .F. ) ;
#117951 = VERTEX_POINT ( 'NONE', #51666 ) ;
#117952 = ORIENTED_EDGE ( 'NONE', *, *, #46227, .F. ) ;
#117953 = ADVANCED_FACE ( 'NONE', ( #53058 ), #140779, .F. ) ;
#117954 = DIRECTION ( 'NONE',  ( -0.000000000000000000, -1.000000000000000000, -0.000000000000000000 ) ) ;
#117955 = CARTESIAN_POINT ( 'NONE',  ( 0.000000000000000000, -21.76999999999999247, -39.50000000000000000 ) ) ;
#117956 = DIRECTION ( 'NONE',  ( -1.000000000000000000, -0.000000000000000000, -0.000000000000000000 ) ) ;
#117957 = EDGE_LOOP ( 'NONE', ( #129280, #62246, #133240, #15068 ) ) ;
#117958 = CARTESIAN_POINT ( 'NONE',  ( 14.99999999999989519, -9.033600742197645417, 5.000000000000000000 ) ) ;
#117959 = ORIENTED_EDGE ( 'NONE', *, *, #97316, .T. ) ;
#117960 = CARTESIAN_POINT ( 'NONE',  ( 3.478736474768552078, -5.808823158059033709, 5.808823158059035485 ) ) ;
#117961 = CARTESIAN_POINT ( 'NONE',  ( -32.99451991528749062, 28.92564299267960948, 4.000000000000000000 ) ) ;
#117962 = PLANE ( 'NONE',  #59795 ) ;
#117963 = EDGE_CURVE ( 'NONE', #10446, #11839, #63285, .T. ) ;
#117964 = LINE ( 'NONE', #86821, #113770 ) ;
#117965 = ORIENTED_EDGE ( 'NONE', *, *, #33720, .F. ) ;
#117966 = ORIENTED_EDGE ( 'NONE', *, *, #45029, .T. ) ;
#117967 = EDGE_LOOP ( 'NONE', ( #51615, #72738, #77417, #69329, #106126, #92690, #50440, #126519 ) ) ;
#117968 = FACE_OUTER_BOUND ( 'NONE', #30638, .T. ) ;
#117969 = FACE_OUTER_BOUND ( 'NONE', #60621, .T. ) ;
#117970 = LINE ( 'NONE', #7065, #21919 ) ;
#117971 = CARTESIAN_POINT ( 'NONE',  ( 0.1630955410174109166, -0.4000000000000003553, 2.152173700565806591 ) ) ;
#117972 = LINE ( 'NONE', #17273, #25405 ) ;
#117973 = DIRECTION ( 'NONE',  ( -0.7071067811865487940, 0.7071067811865463515, -0.000000000000000000 ) ) ;
#117974 = CARTESIAN_POINT ( 'NONE',  ( 63.18398860626900415, 28.73617430169831621, 5.000000000000000000 ) ) ;
#117975 = DIRECTION ( 'NONE',  ( 3.115803279706882722E-16, -1.000000000000000000, 0.000000000000000000 ) ) ;
#117976 = ADVANCED_FACE ( 'NONE', ( #119040 ), #63966, .T. ) ;
#117977 = CARTESIAN_POINT ( 'NONE',  ( 30.47959685856476852, 6.109999999999999432, 1.637169565754164280 ) ) ;
#117978 = FACE_OUTER_BOUND ( 'NONE', #18771, .T. ) ;
#117979 = VERTEX_POINT ( 'NONE', #78408 ) ;
#117980 = CARTESIAN_POINT ( 'NONE',  ( 15.09667064187396335, -2.240707523384257716, 15.26439735382755636 ) ) ;
#117981 = VECTOR ( 'NONE', #111006, 1000.000000000000000 ) ;
#117982 = VECTOR ( 'NONE', #136721, 1000.000000000000000 ) ;
#117983 = VECTOR ( 'NONE', #36355, 1000.000000000000000 ) ;
#117984 = DIRECTION ( 'NONE',  ( 1.000000000000000000, -0.000000000000000000, -0.000000000000000000 ) ) ;
#117985 = ORIENTED_EDGE ( 'NONE', *, *, #20302, .F. ) ;
#117986 = VECTOR ( 'NONE', #76444, 999.9999999999998863 ) ;
#117987 = LINE ( 'NONE', #7081, #136277 ) ;
#117990 = ADVANCED_FACE ( 'NONE', ( #65417 ), #136164, .F. ) ;
#117989 = VERTEX_POINT ( 'NONE', #54531 ) ;
#117988 = CARTESIAN_POINT ( 'NONE',  ( 56.39204447046056146, -48.22435659090880478, -37.54366622512048224 ) ) ;
#117991 = CARTESIAN_POINT ( 'NONE',  ( 25.49999999999982947, -13.91253812416061031, 4.000000000000000000 ) ) ;
#117992 = DIRECTION ( 'NONE',  ( -1.000000000000000000, -1.224606353822377258E-16, -0.000000000000000000 ) ) ;
#117993 = ORIENTED_EDGE ( 'NONE', *, *, #62141, .T. ) ;
#117994 = FACE_OUTER_BOUND ( 'NONE', #87822, .T. ) ;
#117995 = VERTEX_POINT ( 'NONE', #10270 ) ;
#117996 = SURFACE_STYLE_FILL_AREA ( #73825 ) ;
#117997 = EDGE_CURVE ( 'NONE', #83817, #65537, #121877, .T. ) ;
#117998 = CARTESIAN_POINT ( 'NONE',  ( 125.4958603837962272, -3.974999999999998312, -6.884901960086286188 ) ) ;
#117999 = FACE_OUTER_BOUND ( 'NONE', #29142, .T. ) ;
#118000 = VECTOR ( 'NONE', #47806, 1000.000000000000000 ) ;
#118001 = CARTESIAN_POINT ( 'NONE',  ( -65.99451991528749772, 28.92564299267984396, 4.000000000000000000 ) ) ;
#118002 = DIRECTION ( 'NONE',  ( 0.6830127018922180770, -0.6830127018922204085, -0.2588190451025213501 ) ) ;
#118003 = CARTESIAN_POINT ( 'NONE',  ( -32.67183060077623225, -18.74070752338409207, 4.000000000000000000 ) ) ;
#118004 = DIRECTION ( 'NONE',  ( 0.3543493200069163240, -0.000000000000000000, -0.9351131265310288487 ) ) ;
#118005 = CARTESIAN_POINT ( 'NONE',  ( 3.354166666666666963, 1.633150327867695095, 6.094999999999988205 ) ) ;
#118007 = VECTOR ( 'NONE', #4402, 1000.000000000000000 ) ;
#118006 = CARTESIAN_POINT ( 'NONE',  ( 4.353736474768552966, -5.808823158059035485, -5.808823158059033709 ) ) ;
#118008 = VECTOR ( 'NONE', #79614, 1000.000000000000114 ) ;
#118009 = FACE_OUTER_BOUND ( 'NONE', #4127, .T. ) ;
#118010 = DIRECTION ( 'NONE',  ( 0.7071067811865487940, -0.7071067811865463515, 0.000000000000000000 ) ) ;
#118011 = ORIENTED_EDGE ( 'NONE', *, *, #35527, .F. ) ;
#118012 = ORIENTED_EDGE ( 'NONE', *, *, #47383, .F. ) ;
#118013 = CARTESIAN_POINT ( 'NONE',  ( 84.56250000000000000, -5.819803920172572198, -5.819803920172573086 ) ) ;
#118014 = VECTOR ( 'NONE', #50156, 1000.000000000000000 ) ;
#118015 = EDGE_CURVE ( 'NONE', #82440, #67593, #98710, .T. ) ;
#118016 = EDGE_LOOP ( 'NONE', ( #71230, #29355, #78377 ) ) ;
#118017 = DIRECTION ( 'NONE',  ( -0.3543493200069162685, -0.000000000000000000, -0.9351131265310288487 ) ) ;
#118018 = FACE_OUTER_BOUND ( 'NONE', #16492, .T. ) ;
#118019 = FACE_OUTER_BOUND ( 'NONE', #83779, .T. ) ;
#118020 = CARTESIAN_POINT ( 'NONE',  ( 30.55836038379622011, -7.949999999999996625, -2.130196079827426203 ) ) ;
#118021 = ORIENTED_EDGE ( 'NONE', *, *, #60643, .T. ) ;
#118022 = AXIS2_PLACEMENT_3D ( 'NONE', #92024, #14476, #80469 ) ;
#118023 = LINE ( 'NONE', #19465, #132180 ) ;
#118024 = LINE ( 'NONE', #7120, #71924 ) ;
#118025 = LINE ( 'NONE', #19467, #81288 ) ;
#118026 = EDGE_CURVE ( 'NONE', #87748, #71142, #122604, .T. ) ;
#118027 = CIRCLE ( 'NONE', #60245, 2.055000000000000604 ) ;
#118028 = AXIS2_PLACEMENT_3D ( 'NONE', #5345, #72101, #128580 ) ;
#118029 = DIRECTION ( 'NONE',  ( 3.469446951953611033E-15, 0.000000000000000000, 1.000000000000000000 ) ) ;
#118031 = VERTEX_POINT ( 'NONE', #36846 ) ;
#118030 = CARTESIAN_POINT ( 'NONE',  ( 0.000000000000000000, 0.000000000000000000, 5.000000000000000000 ) ) ;
#118032 = LINE ( 'NONE', #75304, #292 ) ;
#118033 = CIRCLE ( 'NONE', #71514, 2.500000000000000444 ) ;
#118034 = FACE_OUTER_BOUND ( 'NONE', #85155, .T. ) ;
#118035 = DIRECTION ( 'NONE',  ( 0.7071067811865487940, 0.7071067811865463515, 0.000000000000000000 ) ) ;
#118036 = PLANE ( 'NONE',  #45258 ) ;
#118037 = CARTESIAN_POINT ( 'NONE',  ( 20.99451991528748707, 28.92564299267952777, 4.000000000000000000 ) ) ;
#118038 = CARTESIAN_POINT ( 'NONE',  ( 54.91896556007530705, -47.51495700086010743, 36.79359617903246260 ) ) ;
#118039 = ORIENTED_EDGE ( 'NONE', *, *, #130, .T. ) ;
#118040 = ORIENTED_EDGE ( 'NONE', *, *, #11216, .T. ) ;
#118041 = CARTESIAN_POINT ( 'NONE',  ( 98.43793019189811844, -6.110000000000001208, 1.637169565754158951 ) ) ;
#118042 = AXIS2_PLACEMENT_3D ( 'NONE', #30031, #74279, #42376 ) ;
#118043 = ORIENTED_EDGE ( 'NONE', *, *, #131043, .T. ) ;
#118044 = VECTOR ( 'NONE', #11033, 1000.000000000000000 ) ;
#118045 = CARTESIAN_POINT ( 'NONE',  ( 19.49999999999986144, 11.52377502935404685, -1.522421517564130022 ) ) ;
#118046 = VERTEX_POINT ( 'NONE', #47774 ) ;
#118047 = CARTESIAN_POINT ( 'NONE',  ( 54.18398860626899705, 28.73617430169825226, 5.000000000000000000 ) ) ;
#118048 = DIRECTION ( 'NONE',  ( -0.7071067811865486830, 0.7071067811865464625, 0.000000000000000000 ) ) ;
#118049 = CARTESIAN_POINT ( 'NONE',  ( 98.49543019189812298, 5.291415217122916737, 3.055000000000001936 ) ) ;
#118050 = EDGE_LOOP ( 'NONE', ( #117391, #66202, #64538 ) ) ;
#118051 = DIRECTION ( 'NONE',  ( 0.7071067811865487940, 0.7071067811865463515, -0.000000000000000000 ) ) ;
#118052 = ORIENTED_EDGE ( 'NONE', *, *, #76972, .F. ) ;
#118053 = CARTESIAN_POINT ( 'NONE',  ( -25.39999999999996305, 0.000000000000000000, 2.500000000000000000 ) ) ;
#118054 = CARTESIAN_POINT ( 'NONE',  ( -44.99451991528749772, 28.92564299267969474, 4.000000000000000000 ) ) ;
#118055 = VECTOR ( 'NONE', #102497, 1000.000000000000000 ) ;
#118056 = DIRECTION ( 'NONE',  ( -0.000000000000000000, -0.000000000000000000, 1.000000000000000000 ) ) ;
#118057 = EDGE_CURVE ( 'NONE', #79175, #104658, #44379, .T. ) ;
#118058 = VERTEX_POINT ( 'NONE', #91942 ) ;
#118059 = EDGE_LOOP ( 'NONE', ( #50835, #133113, #131336, #133888 ) ) ;
#118060 = ORIENTED_EDGE ( 'NONE', *, *, #2891, .T. ) ;
#118061 = DIRECTION ( 'NONE',  ( 0.3543493200069162685, -0.000000000000000000, -0.9351131265310288487 ) ) ;
#118062 = EDGE_CURVE ( 'NONE', #35602, #22434, #89279, .T. ) ;
#118063 = CARTESIAN_POINT ( 'NONE',  ( 21.32816939922339117, 20.25929247661551358, 4.000000000000000000 ) ) ;
#118064 = CARTESIAN_POINT ( 'NONE',  ( 11.58790314143521982, 6.871911579029515771, 3.967499999999989146 ) ) ;
#118065 = VECTOR ( 'NONE', #2658, 999.9999999999998863 ) ;
#118066 = CARTESIAN_POINT ( 'NONE',  ( 22.45833333333333215, -3.047499999999997211, -5.278424836066143655 ) ) ;
#118067 = ADVANCED_FACE ( 'NONE', ( #12415 ), #33501, .F. ) ;
#118068 = EDGE_CURVE ( 'NONE', #24388, #116780, #98019, .T. ) ;
#118069 = ADVANCED_FACE ( 'NONE', ( #132088 ), #110287, .F. ) ;
#118070 = ORIENTED_EDGE ( 'NONE', *, *, #50693, .T. ) ;
#118071 = ORIENTED_EDGE ( 'NONE', *, *, #64663, .T. ) ;
#118073 = EDGE_CURVE ( 'NONE', #109228, #49213, #133505, .T. ) ;
#118072 = DIRECTION ( 'NONE',  ( -0.7071067811865486830, -0.7071067811865464625, 0.000000000000000000 ) ) ;
#118074 = ORIENTED_EDGE ( 'NONE', *, *, #93318, .T. ) ;
#118075 = ORIENTED_EDGE ( 'NONE', *, *, #61898, .F. ) ;
#118076 = EDGE_CURVE ( 'NONE', #6847, #129216, #32781, .T. ) ;
#118077 = EDGE_CURVE ( 'NONE', #68720, #99304, #67556, .T. ) ;
#118078 = VECTOR ( 'NONE', #143314, 1000.000000000000227 ) ;
#118079 = PLANE ( 'NONE',  #11844 ) ;
#118080 = LINE ( 'NONE', #18790, #72687 ) ;
#118081 = VERTEX_POINT ( 'NONE', #10963 ) ;
#118082 = LINE ( 'NONE', #116693, #46040 ) ;
#118083 = VECTOR ( 'NONE', #98826, 1000.000000000000000 ) ;
#118084 = LINE ( 'NONE', #107238, #66390 ) ;
#118085 = LINE ( 'NONE', #52843, #39085 ) ;
#118086 = AXIS2_PLACEMENT_3D ( 'NONE', #111964, #36526, #46750 ) ;
#118087 = AXIS2_PLACEMENT_3D ( 'NONE', #73291, #106577, #96413 ) ;
#118088 = AXIS2_PLACEMENT_3D ( 'NONE', #13674, #34054, #57967 ) ;
#118089 = FILL_AREA_STYLE ('',( #27529 ) ) ;
#118090 = ORIENTED_EDGE ( 'NONE', *, *, #14525, .T. ) ;
#118091 = VECTOR ( 'NONE', #28840, 1000.000000000000000 ) ;
#118092 = EDGE_CURVE ( 'NONE', #73824, #91475, #55228, .T. ) ;
#118093 = DIRECTION ( 'NONE',  ( 0.7071067811865487940, 0.7071067811865463515, 0.000000000000000000 ) ) ;
#118094 = DIRECTION ( 'NONE',  ( -0.7071067811865486830, -0.7071067811865464625, -0.000000000000000000 ) ) ;
#118095 = EDGE_LOOP ( 'NONE', ( #14327, #75819, #18998, #105909 ) ) ;
#118096 = DIRECTION ( 'NONE',  ( 0.6830127018922180770, -0.6830127018922204085, -0.2588190451025213501 ) ) ;
#118097 = DIRECTION ( 'NONE',  ( 0.000000000000000000, -1.000000000000000000, 0.000000000000000000 ) ) ;
#118098 = LINE ( 'NONE', #73225, #5191 ) ;
#118099 = ORIENTED_EDGE ( 'NONE', *, *, #75264, .F. ) ;
#118100 = CARTESIAN_POINT ( 'NONE',  ( 14.67183060077637613, 8.259292476615641476, 4.000000000000000000 ) ) ;
#118101 = ORIENTED_EDGE ( 'NONE', *, *, #17190, .T. ) ;
#118102 = ORIENTED_EDGE ( 'NONE', *, *, #130455, .F. ) ;
#118103 = AXIS2_PLACEMENT_3D ( 'NONE', #2873, #47171, #124664 ) ;
#118104 = ADVANCED_FACE ( 'NONE', ( #132818 ), #88586, .F. ) ;
#118105 = ORIENTED_EDGE ( 'NONE', *, *, #91788, .T. ) ;
#118106 = DIRECTION ( 'NONE',  ( 0.6830127018922180770, -0.6830127018922204085, -0.2588190451025213501 ) ) ;
#118107 = CARTESIAN_POINT ( 'NONE',  ( 31.49999999999977263, 22.22500000000000142, 4.362957392718809224 ) ) ;
#118108 = DIRECTION ( 'NONE',  ( -0.000000000000000000, 0.3543493200069153248, 0.9351131265310291818 ) ) ;
#118109 = DIRECTION ( 'NONE',  ( 0.6830127018922181881, 0.6830127018922202975, -0.2588190451025214056 ) ) ;
#118110 = CARTESIAN_POINT ( 'NONE',  ( 3.710381658649933634, 4.584330080086930965E-16, 0.000000000000000000 ) ) ;
#118111 = DIRECTION ( 'NONE',  ( -0.7071067811865486830, 0.7071067811865464625, 0.000000000000000000 ) ) ;
#118112 = CARTESIAN_POINT ( 'NONE',  ( -14.99999999999989519, -5.527737879153202805, -7.983877177622336951 ) ) ;
#118113 = AXIS2_PLACEMENT_3D ( 'NONE', #34103, #122498, #23173 ) ;
#118114 = SHAPE_REPRESENTATION ( '1.5 Handle Ball', ( #127880 ), #130349 ) ;
#118115 = DIRECTION ( 'NONE',  ( 0.7071067811865487940, 0.7071067811865463515, 0.000000000000000000 ) ) ;
#118116 = AXIS2_PLACEMENT_3D ( 'NONE', #99519, #56083, #68385 ) ;
#118117 = DIRECTION ( 'NONE',  ( -0.7071067811865486830, -0.7071067811865464625, 0.000000000000000000 ) ) ;
#118118 = VECTOR ( 'NONE', #111911, 1000.000000000000000 ) ;
#118119 = LINE ( 'NONE', #84813, #140899 ) ;
#118120 = DIRECTION ( 'NONE',  ( -1.000000000000000000, -1.224606353822377258E-16, -0.000000000000000000 ) ) ;
#118121 = ORIENTED_EDGE ( 'NONE', *, *, #67503, .T. ) ;
#118122 = EDGE_CURVE ( 'NONE', #143282, #63944, #82616, .T. ) ;
#118123 = AXIS2_PLACEMENT_3D ( 'NONE', #71354, #118395, #52427 ) ;
#118124 = ORIENTED_EDGE ( 'NONE', *, *, #137841, .T. ) ;
#118125 = VERTEX_POINT ( 'NONE', #83967 ) ;
#118126 = ORIENTED_EDGE ( 'NONE', *, *, #17022, .F. ) ;
#118127 = DIRECTION ( 'NONE',  ( -0.000000000000000000, -0.000000000000000000, -1.000000000000000000 ) ) ;
#118128 = VERTEX_POINT ( 'NONE', #139769 ) ;
#118129 = AXIS2_PLACEMENT_3D ( 'NONE', #11926, #56215, #56913 ) ;
#118130 = ADVANCED_FACE ( 'NONE', ( #95505 ), #5624, .F. ) ;
#118131 = ORIENTED_EDGE ( 'NONE', *, *, #13852, .T. ) ;
#118132 = CARTESIAN_POINT ( 'NONE',  ( -13.08100000000000307, 3.174999999999997158, 4.000000000000000000 ) ) ;
#118133 = CARTESIAN_POINT ( 'NONE',  ( 12.29177708983039707, -15.74070752338412049, 19.73771281079100604 ) ) ;
#118134 = AXIS2_PLACEMENT_3D ( 'NONE', #7799, #96931, #31025 ) ;
#118135 = DIRECTION ( 'NONE',  ( 0.7071067811865487940, 0.7071067811865463515, -0.000000000000000000 ) ) ;
#118136 = ORIENTED_EDGE ( 'NONE', *, *, #95890, .T. ) ;
#118137 = CARTESIAN_POINT ( 'NONE',  ( 13.49999999999990408, 22.01701374228156283, 2.453858888625600532 ) ) ;
#118138 = ORIENTED_EDGE ( 'NONE', *, *, #126818, .F. ) ;
#118139 = EDGE_CURVE ( 'NONE', #24994, #56274, #38999, .T. ) ;
#118140 = CARTESIAN_POINT ( 'NONE',  ( -69.48921356237309510, -27.52281430457103895, 5.000000000000000000 ) ) ;
#118141 = PLANE ( 'NONE',  #89004 ) ;
#118142 = CARTESIAN_POINT ( 'NONE',  ( 8.379569808101887674, 3.967499999999998916, 6.871911579029510442 ) ) ;
#118143 = EDGE_LOOP ( 'NONE', ( #117950, #18472, #39177, #30391 ) ) ;
#118144 = CARTESIAN_POINT ( 'NONE',  ( 88.43293019189809456, 1.637169565754156730, 6.110000000000001208 ) ) ;
#118145 = CARTESIAN_POINT ( 'NONE',  ( -34.92500000000001137, 22.22500000000000142, 4.000000000000000000 ) ) ;
#118147 = EDGE_CURVE ( 'NONE', #19029, #15867, #16505, .T. ) ;
#118146 = CARTESIAN_POINT ( 'NONE',  ( 0.000000000000000000, 0.000000000000000000, 7.950000000000000178 ) ) ;
#118148 = CARTESIAN_POINT ( 'NONE',  ( -28.62823445044367432, -8.240707523384200428, 11.38925528200759096 ) ) ;
#118149 = VERTEX_POINT ( 'NONE', #60796 ) ;
#118150 = ORIENTED_EDGE ( 'NONE', *, *, #84535, .F. ) ;
#118151 = CARTESIAN_POINT ( 'NONE',  ( 174.7500000000000000, 7.919999999999947526, 21.67769999999990915 ) ) ;
#118152 = VECTOR ( 'NONE', #53532, 999.9999999999998863 ) ;
#118153 = ORIENTED_EDGE ( 'NONE', *, *, #56529, .F. ) ;
#118154 = CARTESIAN_POINT ( 'NONE',  ( -20.20666063542138957, 21.75929247661549226, 4.998822639870715179 ) ) ;
#118155 = DIRECTION ( 'NONE',  ( -1.000000000000000000, -1.224606353822377258E-16, -0.000000000000000000 ) ) ;
#118156 = LINE ( 'NONE', #19584, #102513 ) ;
#118157 = CARTESIAN_POINT ( 'NONE',  ( 18.48921356237309510, -27.52281430457068367, 5.000000000000000000 ) ) ;
#118158 = VERTEX_POINT ( 'NONE', #26695 ) ;
#118159 = CARTESIAN_POINT ( 'NONE',  ( 10.49999999999992717, -7.533600742197660516, 5.000000000000000000 ) ) ;
#118160 = ADVANCED_FACE ( 'NONE', ( #49185 ), #92640, .F. ) ;
#118161 = LINE ( 'NONE', #97876, #113782 ) ;
#118162 = CARTESIAN_POINT ( 'NONE',  ( -8.999999999999934275, -8.731860332648849976, -2.120594902707559015 ) ) ;
#118163 = VERTEX_POINT ( 'NONE', #115087 ) ;
#118164 = LINE ( 'NONE', #18873, #123075 ) ;
#118165 = VECTOR ( 'NONE', #102326, 1000.000000000000000 ) ;
#118166 = DIRECTION ( 'NONE',  ( -0.000000000000000000, -0.3543493200069152693, 0.9351131265310292928 ) ) ;
#118167 = ORIENTED_EDGE ( 'NONE', *, *, #24868, .F. ) ;
#118170 = EDGE_CURVE ( 'NONE', #23219, #87976, #17241, .T. ) ;
#118169 = VERTEX_POINT ( 'NONE', #127424 ) ;
#118168 = CARTESIAN_POINT ( 'NONE',  ( 28.49999999999981171, 5.696342897626538893, -7.587980461218336359 ) ) ;
#118171 = EDGE_LOOP ( 'NONE', ( #94281, #121144, #78971 ) ) ;
#118172 = ADVANCED_FACE ( 'NONE', ( #7031, #104958 ), #93378, .T. ) ;
#118173 = DIRECTION ( 'NONE',  ( 0.000000000000000000, 0.000000000000000000, 1.000000000000000000 ) ) ;
#118174 = CARTESIAN_POINT ( 'NONE',  ( 0.000000000000000000, 0.000000000000000000, 5.000000000000000000 ) ) ;
#118176 = VERTEX_POINT ( 'NONE', #38292 ) ;
#118175 = VECTOR ( 'NONE', #29248, 1000.000000000000000 ) ;
#118177 = DIRECTION ( 'NONE',  ( -0.7071067811865486830, 0.7071067811865463515, 0.000000000000000000 ) ) ;
#118178 = AXIS2_PLACEMENT_3D ( 'NONE', #29729, #118155, #96401 ) ;
#118179 = CARTESIAN_POINT ( 'NONE',  ( 3.299744871391591339, -27.71228299555208352, 4.000000000000000000 ) ) ;
#118180 = EDGE_CURVE ( 'NONE', #121472, #14718, #103514, .T. ) ;
#118181 = CARTESIAN_POINT ( 'NONE',  ( -12.69999999999998153, 0.000000000000000000, 0.000000000000000000 ) ) ;
#118182 = CARTESIAN_POINT ( 'NONE',  ( 7.589909354801631203, 9.759292476615618384, 11.28811694763780515 ) ) ;
#118183 = CARTESIAN_POINT ( 'NONE',  ( 0.1600000000000010858, -7.884487147571573651, 0.9551861632841017746 ) ) ;
#118184 = CARTESIAN_POINT ( 'NONE',  ( 17.51078643762690845, -27.52281430457043143, 5.000000000000000000 ) ) ;
#118185 = LINE ( 'NONE', #18896, #65726 ) ;
#118186 = CARTESIAN_POINT ( 'NONE',  ( -39.48921356237310221, -27.52281430457082934, 5.000000000000000000 ) ) ;
#118187 = CARTESIAN_POINT ( 'NONE',  ( -51.18398860626899705, 28.73617430169823095, 5.000000000000000000 ) ) ;
#118188 = DIRECTION ( 'NONE',  ( -0.5735764363510507113, 0.8191520442889885789, 1.003171929053520926E-16 ) ) ;
#118189 = CARTESIAN_POINT ( 'NONE',  ( -18.46160355370559003, -9.740707523384180888, 17.74957260769606648 ) ) ;
#118190 = VECTOR ( 'NONE', #10255, 1000.000000000000000 ) ;
#118191 = DIRECTION ( 'NONE',  ( 0.3543493200069162685, -0.000000000000000000, -0.9351131265310288487 ) ) ;
#118192 = DIRECTION ( 'NONE',  ( -0.000000000000000000, 0.000000000000000000, 1.000000000000000000 ) ) ;
#118193 = VERTEX_POINT ( 'NONE', #37587 ) ;
#118194 = EDGE_CURVE ( 'NONE', #89301, #69618, #81829, .T. ) ;
#118195 = VERTEX_POINT ( 'NONE', #85335 ) ;
#118196 = ORIENTED_EDGE ( 'NONE', *, *, #118026, .F. ) ;
#118197 = VECTOR ( 'NONE', #36991, 1000.000000000000114 ) ;
#118198 = CARTESIAN_POINT ( 'NONE',  ( 106.5833333333333286, 6.884901960086290629, -3.974999999999994316 ) ) ;
#118199 = VECTOR ( 'NONE', #135246, 1000.000000000000000 ) ;
#118200 = ADVANCED_FACE ( 'NONE', ( #65796 ), #72330, .T. ) ;
#118201 = ORIENTED_EDGE ( 'NONE', *, *, #31396, .T. ) ;
#118202 = ORIENTED_EDGE ( 'NONE', *, *, #30698, .T. ) ;
#118203 = EDGE_LOOP ( 'NONE', ( #118707, #73990, #74708, #81756 ) ) ;
#118204 = CARTESIAN_POINT ( 'NONE',  ( 45.18398860626900415, 28.73617430169818832, 5.000000000000000000 ) ) ;
#118205 = DIRECTION ( 'NONE',  ( -0.8571673007021118895, 0.000000000000000000, -0.5150380749100549327 ) ) ;
#118206 = VECTOR ( 'NONE', #6700, 1000.000000000000227 ) ;
#118207 = VECTOR ( 'NONE', #30878, 1000.000000000000000 ) ;
#118208 = VECTOR ( 'NONE', #90377, 1000.000000000000000 ) ;
#118209 = AXIS2_PLACEMENT_3D ( 'NONE', #62230, #111226, #45319 ) ;
#118210 = EDGE_LOOP ( 'NONE', ( #98746, #64670, #113522, #2339 ) ) ;
#118211 = DIRECTION ( 'NONE',  ( 1.000000000000000000, 1.224606353822377258E-16, 0.000000000000000000 ) ) ;
#118212 = CONICAL_SURFACE ( 'NONE', #53453, 2.055000000000000604, 0.9599310885968764806 ) ;
#118213 = CARTESIAN_POINT ( 'NONE',  ( -3.707106781186510602, -12.74070752338415602, 5.000000000000000000 ) ) ;
#118214 = CARTESIAN_POINT ( 'NONE',  ( -72.48921356237309510, -27.52281430457106026, 5.000000000000000000 ) ) ;
#118215 = LINE ( 'NONE', #106617, #11806 ) ;
#118216 = CARTESIAN_POINT ( 'NONE',  ( 102.8129301918981042, -1.637169565754159617, -6.110000000000001208 ) ) ;
#118217 = VERTEX_POINT ( 'NONE', #108490 ) ;
#118218 = EDGE_CURVE ( 'NONE', #27002, #51146, #20078, .T. ) ;
#118219 = CARTESIAN_POINT ( 'NONE',  ( -11.61648642849997337, 8.193565109092823207, -30.12529094710442124 ) ) ;
#118220 = CARTESIAN_POINT ( 'NONE',  ( -24.70701326429287903, -21.74070752338406365, 4.999753212805221558 ) ) ;
#118221 = CARTESIAN_POINT ( 'NONE',  ( 27.79289321881326558, 6.759292476615653023, 5.000000000000000000 ) ) ;
#118222 = DIRECTION ( 'NONE',  ( 0.000000000000000000, -1.000000000000000000, 0.000000000000000000 ) ) ;
#118223 = FACE_OUTER_BOUND ( 'NONE', #42230, .T. ) ;
#118224 = CARTESIAN_POINT ( 'NONE',  ( 45.48921356237309510, -27.52281430457087197, 5.000000000000000000 ) ) ;
#118225 = CARTESIAN_POINT ( 'NONE',  ( 33.18336038379622721, -2.130196079827426203, 7.949999999999997513 ) ) ;
#118226 = LINE ( 'NONE', #74040, #141778 ) ;
#118227 = ORIENTED_EDGE ( 'NONE', *, *, #245, .F. ) ;
#118228 = VERTEX_POINT ( 'NONE', #109954 ) ;
#118229 = CARTESIAN_POINT ( 'NONE',  ( 31.18749999999998934, -5.819803920172573086, 5.819803920172572198 ) ) ;
#118230 = VERTEX_POINT ( 'NONE', #52023 ) ;
#118231 = AXIS2_PLACEMENT_3D ( 'NONE', #95103, #127763, #27712 ) ;
#118232 = DIRECTION ( 'NONE',  ( -1.000000000000000000, -1.224606353822377258E-16, -0.000000000000000000 ) ) ;
#118233 = VECTOR ( 'NONE', #88093, 1000.000000000000000 ) ;
#118234 = DIRECTION ( 'NONE',  ( 1.000000000000000000, 0.000000000000000000, 0.000000000000000000 ) ) ;
#118235 = CARTESIAN_POINT ( 'NONE',  ( 8.510786437626906675, -27.52281430457049183, 5.000000000000000000 ) ) ;
#118236 = DIRECTION ( 'NONE',  ( 0.6830127018922180770, -0.6830127018922204085, -0.2588190451025213501 ) ) ;
#118237 = DIRECTION ( 'NONE',  ( -1.000000000000000000, 0.000000000000000000, 0.000000000000000000 ) ) ;
#118238 = DIRECTION ( 'NONE',  ( 0.000000000000000000, 1.000000000000000000, 0.000000000000000000 ) ) ;
#118239 = VECTOR ( 'NONE', #3083, 1000.000000000000000 ) ;
#118240 = AXIS2_PLACEMENT_3D ( 'NONE', #20531, #40892, #77119 ) ;
#118241 = CARTESIAN_POINT ( 'NONE',  ( 121.6829301918980946, -1.637169565754158951, -6.109999999999998543 ) ) ;
#118242 = ORIENTED_EDGE ( 'NONE', *, *, #116443, .T. ) ;
#118243 = VECTOR ( 'NONE', #35563, 1000.000000000000000 ) ;
#118244 = LINE ( 'NONE', #61773, #3873 ) ;
#118245 = ADVANCED_FACE ( 'NONE', ( #96902 ), #141148, .T. ) ;
#118246 = ORIENTED_EDGE ( 'NONE', *, *, #30443, .T. ) ;
#118247 = LINE ( 'NONE', #140046, #53179 ) ;
#118248 = AXIS2_PLACEMENT_3D ( 'NONE', #66878, #32101, #132146 ) ;
#118249 = CARTESIAN_POINT ( 'NONE',  ( 15.32816939922342669, 11.25929247661561128, 4.000000000000000000 ) ) ;
#118250 =( LENGTH_UNIT ( ) NAMED_UNIT ( * ) SI_UNIT ( .MILLI., .METRE. ) );
#118251 = CARTESIAN_POINT ( 'NONE',  ( -0.1839886062690032631, 28.73617430169787568, 5.000000000000000000 ) ) ;
#118252 = ORIENTED_EDGE ( 'NONE', *, *, #126192, .T. ) ;
#118253 = CARTESIAN_POINT ( 'NONE',  ( 41.27126352523144703, 4.472830434245839371, 4.472830434245842035 ) ) ;
#118254 = ORIENTED_EDGE ( 'NONE', *, *, #21944, .T. ) ;
#118255 = AXIS2_PLACEMENT_3D ( 'NONE', #111987, #58360, #14792 ) ;
#118256 = CARTESIAN_POINT ( 'NONE',  ( 0.000000000000000000, 0.000000000000000000, 5.000000000000000000 ) ) ;
#118257 = DIRECTION ( 'NONE',  ( 0.7071067811865487940, 0.7071067811865463515, 0.000000000000000000 ) ) ;
#118258 = CARTESIAN_POINT ( 'NONE',  ( -34.42500000000001137, 22.22500000000000142, 0.4999999999999995559 ) ) ;
#118259 = DIRECTION ( 'NONE',  ( -1.000000000000000000, -0.000000000000000000, -0.000000000000000000 ) ) ;
#118260 = EDGE_CURVE ( 'NONE', #84967, #33497, #86076, .T. ) ;
#118261 = PRESENTATION_LAYER_ASSIGNMENT (  '', '', ( #134551 ) ) ;
#118262 = CARTESIAN_POINT ( 'NONE',  ( 41.47459685856477307, 1.637169565754164058, -6.109999999999996767 ) ) ;
#118263 = EDGE_CURVE ( 'NONE', #100536, #109228, #63638, .T. ) ;
#118264 = VERTEX_POINT ( 'NONE', #142606 ) ;
#118266 = EDGE_CURVE ( 'NONE', #53028, #75919, #40450, .T. ) ;
#118265 = CARTESIAN_POINT ( 'NONE',  ( 51.18398860626899705, 28.73617430169823095, 5.000000000000000000 ) ) ;
#118267 = ORIENTED_EDGE ( 'NONE', *, *, #52842, .T. ) ;
#118268 = ORIENTED_EDGE ( 'NONE', *, *, #84339, .T. ) ;
#118269 = PRESENTATION_LAYER_ASSIGNMENT (  '', '', ( #25663 ) ) ;
#118270 = ORIENTED_EDGE ( 'NONE', *, *, #43389, .T. ) ;
#118271 = VECTOR ( 'NONE', #74723, 999.9999999999998863 ) ;
#118272 = ADVANCED_FACE ( 'NONE', ( #129561 ), #127761, .T. ) ;
#118273 = CARTESIAN_POINT ( 'NONE',  ( -1.499999999999991784, 22.01701374228155572, 2.453858888625634727 ) ) ;
#118274 = CARTESIAN_POINT ( 'NONE',  ( 80.28752705046289861, 0.000000000000000000, -7.949999999999998401 ) ) ;
#118275 = VERTEX_POINT ( 'NONE', #18639 ) ;
#118276 = DIRECTION ( 'NONE',  ( 0.000000000000000000, 0.000000000000000000, 1.000000000000000000 ) ) ;
#118277 = EDGE_CURVE ( 'NONE', #37506, #71573, #109243, .T. ) ;
#118278 = AXIS2_PLACEMENT_3D ( 'NONE', #123736, #80937, #49028 ) ;
#118279 = DIRECTION ( 'NONE',  ( 0.000000000000000000, 0.000000000000000000, 1.000000000000000000 ) ) ;
#118280 = DIRECTION ( 'NONE',  ( 0.000000000000000000, -1.000000000000000000, 0.000000000000000000 ) ) ;
#118281 = EDGE_CURVE ( 'NONE', #139751, #24590, #127045, .T. ) ;
#118282 = FACE_BOUND ( 'NONE', #141560, .T. ) ;
#118283 = ORIENTED_EDGE ( 'NONE', *, *, #97270, .T. ) ;
#118284 = EDGE_CURVE ( 'NONE', #47269, #25807, #20801, .T. ) ;
#118285 = CARTESIAN_POINT ( 'NONE',  ( 21.48921356237309155, -27.52281430457070499, 5.000000000000000000 ) ) ;
#118286 = LINE ( 'NONE', #8086, #102308 ) ;
#118287 = CARTESIAN_POINT ( 'NONE',  ( 4.969723521325230209, 4.202752102959690472E-16, 0.000000000000000000 ) ) ;
#118288 = ORIENTED_EDGE ( 'NONE', *, *, #41351, .F. ) ;
#118289 = DIRECTION ( 'NONE',  ( 0.7071067811865487940, 0.7071067811865463515, -0.000000000000000000 ) ) ;
#118290 = ORIENTED_EDGE ( 'NONE', *, *, #141850, .F. ) ;
#118291 = ORIENTED_EDGE ( 'NONE', *, *, #102498, .F. ) ;
#118292 = AXIS2_PLACEMENT_3D ( 'NONE', #73331, #105906, #51578 ) ;
#118293 = CARTESIAN_POINT ( 'NONE',  ( 19.73159235450332005, -3.851859888774471706E-31, 2.500000000000001332 ) ) ;
#118294 = EDGE_CURVE ( 'NONE', #130884, #31083, #2726, .T. ) ;
#118295 = VERTEX_POINT ( 'NONE', #65054 ) ;
#118296 = CARTESIAN_POINT ( 'NONE',  ( 57.51626352523144448, -4.472830434245838482, 4.472830434245838482 ) ) ;
#118297 = ORIENTED_EDGE ( 'NONE', *, *, #46378, .F. ) ;
#118298 =( BOUNDED_SURFACE ( )  B_SPLINE_SURFACE ( 3, 2, ( 
 ( #49993, #127533, #28230 ),
 ( #6409, #142698, #96295 ),
 ( #63731, #74604, #52114 ),
 ( #110048, #131113, #64416 ),
 ( #18749, #41229, #98475 ),
 ( #85434, #52802, #119483 ),
 ( #76753, #142007, #128958 ),
 ( #141253, #97000, #43390 ),
 ( #129662, #41964, #86179 ),
 ( #87602, #95612, #53552 ),
 ( #40543, #20173, #84746 ),
 ( #10032, #31096, #42697 ),
 ( #107889, #31796, #8556 ),
 ( #107201, #108592, #97759 ),
 ( #140539, #30359, #10722 ),
 ( #9275, #131827, #21637 ) ),
 .UNSPECIFIED., .F., .F., .F. ) 
 B_SPLINE_SURFACE_WITH_KNOTS ( ( 4, 2, 2, 2, 2, 2, 2, 4 ),
 ( 3, 3 ),
 ( 4.712388980384689674, 5.060738160973321520, 5.234912751267637887, 5.409087341561953366, 5.583261931856269733, 5.757436522150586100, 5.931611112444901579, 6.105785702739217946 ),
 ( 0.000000000000000000, 1.000000000000000000 ),
 .UNSPECIFIED. ) 
 GEOMETRIC_REPRESENTATION_ITEM ( )  RATIONAL_B_SPLINE_SURFACE ( (
 ( 1.000000000000000000, 1.000000000000000000, 1.000000000000000000),
 ( 1.000000000000000000, 1.000097732991246824, 1.000000000000000000),
 ( 1.000000000000000000, 0.9896287210064191875, 1.000000000000000000),
 ( 1.000000000000000000, 0.9608359430472837026, 1.000000000000000000),
 ( 1.000000000000000000, 0.9490805577171954610, 1.000000000000000000),
 ( 1.000000000000000000, 0.9222453908327026273, 1.000000000000000000),
 ( 1.000000000000000000, 0.9071649184813318501, 1.000000000000000000),
 ( 1.000000000000000000, 0.8751006588766834238, 1.000000000000000000),
 ( 1.000000000000000000, 0.8581174656084207264, 1.000000000000000000),
 ( 1.000000000000000000, 0.8241077986063138905, 1.000000000000000000),
 ( 1.000000000000000000, 0.8070860741946217498, 1.000000000000000000),
 ( 1.000000000000000000, 0.7752313834061490549, 1.000000000000000000),
 ( 1.000000000000000000, 0.7604116155351092754, 1.000000000000000000),
 ( 1.000000000000000000, 0.7353122387368599133, 1.000000000000000000),
 ( 1.000000000000000000, 0.7250426641248335358, 1.000000000000000000),
 ( 1.000000000000000000, 0.7180326832784525992, 1.000000000000000000) ) ) 
 REPRESENTATION_ITEM ( '' )  SURFACE ( )  );
#118299 = CYLINDRICAL_SURFACE ( 'NONE', #18577, 7.950000000000000178 ) ;
#118300 = LINE ( 'NONE', #107437, #56596 ) ;
#118301 = ORIENTED_EDGE ( 'NONE', *, *, #64950, .T. ) ;
#118302 =( LENGTH_UNIT ( ) NAMED_UNIT ( * ) SI_UNIT ( .MILLI., .METRE. ) );
#118303 = VECTOR ( 'NONE', #112790, 1000.000000000000000 ) ;
#118304 = VECTOR ( 'NONE', #4838, 999.9999999999998863 ) ;
#118305 = DIRECTION ( 'NONE',  ( -0.6830127018922180770, -0.6830127018922204085, -0.2588190451025213501 ) ) ;
#118306 = FACE_OUTER_BOUND ( 'NONE', #15033, .T. ) ;
#118307 = CARTESIAN_POINT ( 'NONE',  ( 14.39532882439692862, 2.055000000000001048, 0.000000000000000000 ) ) ;
#118308 = DIRECTION ( 'NONE',  ( -1.000000000000000000, -0.000000000000000000, -0.000000000000000000 ) ) ;
#118309 = CARTESIAN_POINT ( 'NONE',  ( -34.49999999999975131, -19.53574439159930876, 4.994342998332169437 ) ) ;
#118310 = ORIENTED_EDGE ( 'NONE', *, *, #16502, .T. ) ;
#118311 = EDGE_CURVE ( 'NONE', #26486, #62201, #76649, .T. ) ;
#118312 = VECTOR ( 'NONE', #60837, 1000.000000000000227 ) ;
#118313 = VECTOR ( 'NONE', #33040, 999.9999999999998863 ) ;
#118314 = AXIS2_PLACEMENT_3D ( 'NONE', #54751, #43159, #88810 ) ;
#118315 = ORIENTED_EDGE ( 'NONE', *, *, #112411, .T. ) ;
#118316 = AXIS2_PLACEMENT_3D ( 'NONE', #6413, #18020, #104334 ) ;
#118317 = DIRECTION ( 'NONE',  ( -1.000000000000000000, -1.224606353822377258E-16, -0.000000000000000000 ) ) ;
#118318 = CARTESIAN_POINT ( 'NONE',  ( -27.18398860626900060, 28.73617430169806042, 5.000000000000000000 ) ) ;
#118319 = VERTEX_POINT ( 'NONE', #98385 ) ;
#118320 = VECTOR ( 'NONE', #116213, 1000.000000000000000 ) ;
#118321 = ORIENTED_EDGE ( 'NONE', *, *, #128574, .F. ) ;
#118322 = ORIENTED_EDGE ( 'NONE', *, *, #22985, .T. ) ;
#118323 = CARTESIAN_POINT ( 'NONE',  ( 54.03752705046288440, -9.735942053221456900E-16, 7.949999999999998401 ) ) ;
#118324 = CARTESIAN_POINT ( 'NONE',  ( 16.17183060077635659, -11.24070752338416668, 4.000000000000000000 ) ) ;
#118325 = ORIENTED_EDGE ( 'NONE', *, *, #73757, .T. ) ;
#118326 = VECTOR ( 'NONE', #125769, 1000.000000000000114 ) ;
#118327 = FACE_OUTER_BOUND ( 'NONE', #108742, .T. ) ;
#118328 = EDGE_CURVE ( 'NONE', #55786, #89397, #7773, .T. ) ;
#118329 = DIRECTION ( 'NONE',  ( 0.7071067811865487940, 0.7071067811865463515, -0.000000000000000000 ) ) ;
#118330 = CARTESIAN_POINT ( 'NONE',  ( 21.65040314143522338, 7.934999999999989839, -2.126176841940961904 ) ) ;
#118331 = CARTESIAN_POINT ( 'NONE',  ( 28.49999999999980815, -4.796895815300988630, -3.611700055028616685 ) ) ;
#118332 = VERTEX_POINT ( 'NONE', #41133 ) ;
#118333 = CARTESIAN_POINT ( 'NONE',  ( 121.6829301918980946, -1.637169565754159173, -6.109999999999999432 ) ) ;
#118334 = VECTOR ( 'NONE', #51109, 999.9999999999998863 ) ;
#118336 = EDGE_CURVE ( 'NONE', #56372, #11859, #30254, .T. ) ;
#118335 = CARTESIAN_POINT ( 'NONE',  ( -8.381615093979984721, -2.240707523384260824, 13.37739548510241328 ) ) ;
#118337 = PLANE ( 'NONE',  #118987 ) ;
#118339 = ORIENTED_EDGE ( 'NONE', *, *, #130567, .T. ) ;
#118338 = LINE ( 'NONE', #19040, #98075 ) ;
#118340 = CARTESIAN_POINT ( 'NONE',  ( 67.16252705046288440, 7.949999999999998401, 1.460391307983218338E-15 ) ) ;
#118341 = ORIENTED_EDGE ( 'NONE', *, *, #133692, .F. ) ;
#118342 = PLANE ( 'NONE',  #121362 ) ;
#118343 = FACE_OUTER_BOUND ( 'NONE', #117155, .T. ) ;
#118344 = CARTESIAN_POINT ( 'NONE',  ( 21.48921356237309155, -27.52281430457070499, 5.000000000000000000 ) ) ;
#118345 = VERTEX_POINT ( 'NONE', #133169 ) ;
#118346 = VECTOR ( 'NONE', #2366, 999.9999999999998863 ) ;
#118347 = EDGE_CURVE ( 'NONE', #89560, #71785, #135315, .T. ) ;
#118349 = CARTESIAN_POINT ( 'NONE',  ( 25.34840764549667469, -2.499999999999996003, 0.000000000000000000 ) ) ;
#118348 = VECTOR ( 'NONE', #33324, 1000.000000000000227 ) ;
#118350 = CYLINDRICAL_SURFACE ( 'NONE', #39611, 2.500000000000000000 ) ;
#118351 = CARTESIAN_POINT ( 'NONE',  ( 3.000000000000000000, -4.600000000000061817, 28.92500000000000426 ) ) ;
#118352 = ORIENTED_EDGE ( 'NONE', *, *, #28267, .F. ) ;
#118353 = DIRECTION ( 'NONE',  ( -0.7071067811865486830, -0.7071067811865464625, 0.000000000000000000 ) ) ;
#118354 = MECHANICAL_DESIGN_GEOMETRIC_PRESENTATION_REPRESENTATION (  '', ( #106868 ), #11860 ) ;
#118355 = CARTESIAN_POINT ( 'NONE',  ( -27.48921356237309155, -27.52281430457074762, 5.000000000000000000 ) ) ;
#118356 = CARTESIAN_POINT ( 'NONE',  ( 31.92500000000001492, -6.269999999999992468, -40.00000000000000000 ) ) ;
#118357 = FACE_OUTER_BOUND ( 'NONE', #92255, .T. ) ;
#118359 = ADVANCED_FACE ( 'NONE', ( #68629 ), #113515, .F. ) ;
#118358 = VERTEX_POINT ( 'NONE', #12063 ) ;
#118360 = AXIS2_PLACEMENT_3D ( 'NONE', #36220, #23154, #100751 ) ;
#118361 = ORIENTED_EDGE ( 'NONE', *, *, #74130, .F. ) ;
#118362 = DIRECTION ( 'NONE',  ( -0.6830127018922181881, 0.6830127018922202975, -0.2588190451025214056 ) ) ;
#118363 = CARTESIAN_POINT ( 'NONE',  ( 1.499999999999997780, -20.94781430457061333, 5.000000000000000000 ) ) ;
#118364 = CARTESIAN_POINT ( 'NONE',  ( 12.66623647476855297, 7.934999999999990727, -1.457635852685135314E-15 ) ) ;
#118365 = LINE ( 'NONE', #107500, #80630 ) ;
#118366 = VECTOR ( 'NONE', #59319, 1000.000000000000000 ) ;
#118367 = CARTESIAN_POINT ( 'NONE',  ( -17.99999999999987566, -13.97847968911261951, -0.1324546996127216603 ) ) ;
#118368 = DIRECTION ( 'NONE',  ( 0.7071067811865487940, 0.7071067811865463515, -0.000000000000000000 ) ) ;
#118369 = ORIENTED_EDGE ( 'NONE', *, *, #9084, .T. ) ;
#118370 = DIRECTION ( 'NONE',  ( 0.3543493200069163240, -0.000000000000000000, -0.9351131265310288487 ) ) ;
#118371 = CARTESIAN_POINT ( 'NONE',  ( -48.48921356237309510, -27.52281430457089328, 5.000000000000000000 ) ) ;
#118372 = VECTOR ( 'NONE', #137894, 1000.000000000000000 ) ;
#118373 = CARTESIAN_POINT ( 'NONE',  ( 17.99999999999987566, 18.08204922493374767, 0.9627537363044456065 ) ) ;
#118374 = CIRCLE ( 'NONE', #55915, 2.500000000000000888 ) ;
#118375 = DIRECTION ( 'NONE',  ( 0.7071067811865486830, -0.7071067811865464625, -0.000000000000000000 ) ) ;
#118376 = CARTESIAN_POINT ( 'NONE',  ( 35.34959685856478728, 6.109999999999997655, 1.637169565754163836 ) ) ;
#118377 = CARTESIAN_POINT ( 'NONE',  ( 32.01088028653925477, -22.02621442084247860, 4.990779571109224655 ) ) ;
#118378 = EDGE_LOOP ( 'NONE', ( #29443, #81343, #4642, #132389 ) ) ;
#118379 = DIRECTION ( 'NONE',  ( 0.6830127018922180770, -0.6830127018922204085, -0.2588190451025213501 ) ) ;
#118380 = EDGE_CURVE ( 'NONE', #69099, #50102, #88222, .T. ) ;
#118381 = VERTEX_POINT ( 'NONE', #110642 ) ;
#118382 = VERTEX_POINT ( 'NONE', #132474 ) ;
#118383 = VECTOR ( 'NONE', #126227, 1000.000000000000000 ) ;
#118384 = CARTESIAN_POINT ( 'NONE',  ( 5.994519915287488843, 28.92564299267942118, 4.000000000000000000 ) ) ;
#118385 = CARTESIAN_POINT ( 'NONE',  ( 32.29298673570672662, -21.74070752338405654, 4.999753212805222446 ) ) ;
#118386 = EDGE_LOOP ( 'NONE', ( #47615, #131842, #123894, #72350 ) ) ;
#118387 = DIRECTION ( 'NONE',  ( -0.6830127018922180770, -0.6830127018922204085, -0.2588190451025213501 ) ) ;
#118388 = CARTESIAN_POINT ( 'NONE',  ( 12.70710678118645731, 8.259292476615629042, 5.000000000000000000 ) ) ;
#118389 = CARTESIAN_POINT ( 'NONE',  ( -7.499999999999944045, -9.462702396501018853, -9.474982329943495429 ) ) ;
#118390 = EDGE_CURVE ( 'NONE', #41017, #100429, #33164, .T. ) ;
#118391 = CARTESIAN_POINT ( 'NONE',  ( 6.489213562373093325, -27.52281430457059841, 5.000000000000000000 ) ) ;
#118392 = CARTESIAN_POINT ( 'NONE',  ( 42.48921356237308800, -27.52281430457085065, 5.000000000000000000 ) ) ;
#118393 = ORIENTED_EDGE ( 'NONE', *, *, #1908, .T. ) ;
#118394 = EDGE_CURVE ( 'NONE', #19799, #68975, #121539, .T. ) ;
#118395 = DIRECTION ( 'NONE',  ( -1.000000000000000000, -1.224606353822377258E-16, -0.000000000000000000 ) ) ;
#118396 = CARTESIAN_POINT ( 'NONE',  ( -8.816011393731004731, 28.73617430169781173, 5.000000000000000000 ) ) ;
#118398 = VECTOR ( 'NONE', #49434, 1000.000000000000000 ) ;
#118397 = CARTESIAN_POINT ( 'NONE',  ( 5.700255128608413102, -27.71228299555201957, 4.000000000000000000 ) ) ;
#118399 = CARTESIAN_POINT ( 'NONE',  ( 8.671830600776408104, -12.74070752338415602, 4.000000000000000000 ) ) ;
#118400 = CARTESIAN_POINT ( 'NONE',  ( 0.000000000000000000, 0.000000000000000000, 0.000000000000000000 ) ) ;
#118401 = CARTESIAN_POINT ( 'NONE',  ( 34.42499999999998295, 5.977185695429338530, 5.000000000000000000 ) ) ;
#118402 = CARTESIAN_POINT ( 'NONE',  ( 59.43336038379622011, 2.130196079827431532, -7.949999999999997513 ) ) ;
#118403 = CARTESIAN_POINT ( 'NONE',  ( 12.79333936457838483, 21.75929247661549937, 4.998822639870715179 ) ) ;
#118404 = ORIENTED_EDGE ( 'NONE', *, *, #103860, .F. ) ;
#118405 = VERTEX_POINT ( 'NONE', #100529 ) ;
#118406 = CARTESIAN_POINT ( 'NONE',  ( 54.52083333333332149, 7.949999999999999289, 2.130196079827431532 ) ) ;
#118407 = LINE ( 'NONE', #38730, #33161 ) ;
#118408 = CARTESIAN_POINT ( 'NONE',  ( 15.49238828748955576, 2.500000000000000888, 0.000000000000000000 ) ) ;
#118409 = LINE ( 'NONE', #52444, #120082 ) ;
#118410 = ORIENTED_EDGE ( 'NONE', *, *, #86020, .F. ) ;
#118411 = VECTOR ( 'NONE', #10645, 1000.000000000000000 ) ;
#118412 = ADVANCED_FACE ( 'NONE', ( #24380 ), #13469, .F. ) ;
#118413 = CARTESIAN_POINT ( 'NONE',  ( 127.3989248045490967, 0.000000000000000000, -6.349999999999997868 ) ) ;
#118414 = VECTOR ( 'NONE', #99585, 999.9999999999998863 ) ;
#118415 = AXIS2_PLACEMENT_3D ( 'NONE', #47565, #14875, #135268 ) ;
#118416 = CARTESIAN_POINT ( 'NONE',  ( 51.04209685856476852, 5.291415217122923842, -3.054999999999996163 ) ) ;
#118417 = VERTEX_POINT ( 'NONE', #80224 ) ;
#118418 = PLANE ( 'NONE',  #47936 ) ;
#118419 = ORIENTED_EDGE ( 'NONE', *, *, #84594, .F. ) ;
#118421 = ORIENTED_EDGE ( 'NONE', *, *, #112443, .T. ) ;
#118420 = VECTOR ( 'NONE', #61387, 1000.000000000000000 ) ;
#118422 = AXIS2_PLACEMENT_3D ( 'NONE', #66544, #108562, #20151 ) ;
#118423 = AXIS2_PLACEMENT_3D ( 'NONE', #89002, #1227, #77427 ) ;
#118424 = VECTOR ( 'NONE', #17861, 1000.000000000000000 ) ;
#118425 = DIRECTION ( 'NONE',  ( 0.000000000000000000, 0.000000000000000000, 1.000000000000000000 ) ) ;
#118427 = CARTESIAN_POINT ( 'NONE',  ( -34.92500000000001137, 6.324594729295654361, 11.02525794543158888 ) ) ;
#118426 = VECTOR ( 'NONE', #115278, 1000.000000000000000 ) ;
#118428 = CARTESIAN_POINT ( 'NONE',  ( 24.32816939922335919, -18.74070752338409562, 4.000000000000000000 ) ) ;
#118429 = ORIENTED_EDGE ( 'NONE', *, *, #63136, .F. ) ;
#118430 = FACE_OUTER_BOUND ( 'NONE', #63688, .T. ) ;
#118432 = ORIENTED_EDGE ( 'NONE', *, *, #23653, .T. ) ;
#118431 = CARTESIAN_POINT ( 'NONE',  ( 51.48921356237309510, -27.52281430457091460, 5.000000000000000000 ) ) ;
#118433 = CARTESIAN_POINT ( 'NONE',  ( 127.0704994235588572, 0.7945742482428581610, 6.350000000000343370 ) ) ;
#118434 = LINE ( 'NONE', #19135, #61678 ) ;
#118435 = PLANE ( 'NONE',  #137455 ) ;
#118436 = CONICAL_SURFACE ( 'NONE', #37333, 2.500000000000000888, 0.9599310885968822538 ) ;
#118437 = DIRECTION ( 'NONE',  ( 0.3543493200069162685, -0.000000000000000000, -0.9351131265310288487 ) ) ;
#118438 = CARTESIAN_POINT ( 'NONE',  ( -11.52663903635778020, -5.240707523384218192, 16.25846745537492666 ) ) ;
#118439 = EDGE_LOOP ( 'NONE', ( #77736, #64430, #61329, #79982 ) ) ;
#118440 = EDGE_CURVE ( 'NONE', #7626, #96600, #125473, .T. ) ;
#118441 = ORIENTED_EDGE ( 'NONE', *, *, #67901, .T. ) ;
#118442 = LINE ( 'NONE', #7530, #128684 ) ;
#118443 = CARTESIAN_POINT ( 'NONE',  ( 70.34959685856478018, 6.109999999999996767, 1.637169565754163836 ) ) ;
#118444 = EDGE_CURVE ( 'NONE', #130332, #132699, #91094, .T. ) ;
#118445 = CARTESIAN_POINT ( 'NONE',  ( -34.92500000000001137, -11.33753812416089346, 4.000000000000000000 ) ) ;
#118446 = DIRECTION ( 'NONE',  ( -0.7071067811865487940, 0.7071067811865463515, -0.000000000000000000 ) ) ;
#118447 = ORIENTED_EDGE ( 'NONE', *, *, #108662, .T. ) ;
#118448 = ORIENTED_EDGE ( 'NONE', *, *, #26217, .F. ) ;
#118449 = LINE ( 'NONE', #130800, #39981 ) ;
#118450 = LINE ( 'NONE', #19153, #63003 ) ;
#118451 = VERTEX_POINT ( 'NONE', #88952 ) ;
#118452 = ADVANCED_FACE ( 'NONE', ( #133860 ), #33853, .T. ) ;
#118453 = EDGE_CURVE ( 'NONE', #88279, #105080, #34553, .T. ) ;
#118454 = ORIENTED_EDGE ( 'NONE', *, *, #17869, .T. ) ;
#118455 = VECTOR ( 'NONE', #4643, 999.9999999999998863 ) ;
#118456 = DIRECTION ( 'NONE',  ( -1.000000000000000000, -0.000000000000000000, -0.000000000000000000 ) ) ;
#118457 = VERTEX_POINT ( 'NONE', #112123 ) ;
#118458 = COLOUR_RGB ( '', 0.09019608, 0.27058824, 0.51372549) ;
#118459 = CARTESIAN_POINT ( 'NONE',  ( -8.109179343494679060, 22.22500000000000142, -5.161516874765829321 ) ) ;
#118460 = DIRECTION ( 'NONE',  ( -0.7071067811865487940, 0.7071067811865463515, 0.000000000000000000 ) ) ;
#118461 = CIRCLE ( 'NONE', #56003, 2.500000000000000888 ) ;
#118462 = DIRECTION ( 'NONE',  ( -0.6830127018922181881, 0.6830127018922202975, -0.2588190451025214056 ) ) ;
#118463 = ADVANCED_FACE ( 'NONE', ( #72933 ), #94615, .F. ) ;
#118464 = FACE_BOUND ( 'NONE', #91391, .T. ) ;
#118465 = EDGE_CURVE ( 'NONE', #106952, #5802, #114243, .T. ) ;
#118466 =( NAMED_UNIT ( * ) SI_UNIT ( $, .STERADIAN. ) SOLID_ANGLE_UNIT ( ) );
#118467 = FACE_OUTER_BOUND ( 'NONE', #48206, .T. ) ;
#118468 = DIRECTION ( 'NONE',  ( 0.000000000000000000, -1.000000000000000000, 0.000000000000000000 ) ) ;
#118470 = ORIENTED_EDGE ( 'NONE', *, *, #15403, .F. ) ;
#118469 = DIRECTION ( 'NONE',  ( 0.7071067811865487940, -0.7071067811865463515, 0.000000000000000000 ) ) ;
#118471 = VECTOR ( 'NONE', #78571, 1000.000000000000000 ) ;
#118472 = DIRECTION ( 'NONE',  ( 0.7071067811865486830, -0.7071067811865464625, -0.000000000000000000 ) ) ;
#118474 = EDGE_CURVE ( 'NONE', #123094, #391, #117081, .T. ) ;
#118473 = CONTEXT_DEPENDENT_SHAPE_REPRESENTATION ( #69014, #16849 ) ;
#118475 = VERTEX_POINT ( 'NONE', #70772 ) ;
#118476 = ORIENTED_EDGE ( 'NONE', *, *, #83239, .F. ) ;
#118477 = CARTESIAN_POINT ( 'NONE',  ( 88.87043019189810877, -3.055000000000001492, 5.291415217122917625 ) ) ;
#118478 = ORIENTED_EDGE ( 'NONE', *, *, #90496, .T. ) ;
#118479 = DIRECTION ( 'NONE',  ( -0.6830127018922180770, -0.6830127018922204085, -0.2588190451025213501 ) ) ;
#118480 = VECTOR ( 'NONE', #23025, 1000.000000000000000 ) ;
#118481 = LINE ( 'NONE', #73572, #74850 ) ;
#118482 = EDGE_CURVE ( 'NONE', #60854, #3234, #118628, .T. ) ;
#118483 = VECTOR ( 'NONE', #138552, 999.9999999999998863 ) ;
#118484 = DIRECTION ( 'NONE',  ( 0.3543493200069162685, -0.000000000000000000, -0.9351131265310288487 ) ) ;
#118485 = LINE ( 'NONE', #19880, #32144 ) ;
#118486 = CARTESIAN_POINT ( 'NONE',  ( 48.18398860626899705, 28.73617430169820608, 5.000000000000000000 ) ) ;
#118487 = CARTESIAN_POINT ( 'NONE',  ( 184.1500000000000057, -57.15000000000003411, 15.92499999999935589 ) ) ;
#118488 = CYLINDRICAL_SURFACE ( 'NONE', #68150, 7.950000000000000178 ) ;
#118489 = CARTESIAN_POINT ( 'NONE',  ( -28.49999999999979039, 0.05218569542916537407, 5.000000000000000000 ) ) ;
#118490 = CARTESIAN_POINT ( 'NONE',  ( -30.18398860626900060, 28.73617430169808173, 5.000000000000000000 ) ) ;
#118491 = ADVANCED_FACE ( 'NONE', ( #81650 ), #125856, .F. ) ;
#118492 = AXIS2_PLACEMENT_3D ( 'NONE', #77735, #100197, #845 ) ;
#118493 = ORIENTED_EDGE ( 'NONE', *, *, #132031, .F. ) ;
#118494 = CARTESIAN_POINT ( 'NONE',  ( -30.32816939922331656, 17.25929247661554200, 4.000000000000000000 ) ) ;
#118495 = CARTESIAN_POINT ( 'NONE',  ( -2.510786437626908008, -27.52281430457053446, 5.000000000000000000 ) ) ;
#118496 = ORIENTED_EDGE ( 'NONE', *, *, #122611, .F. ) ;
#118497 = VERTEX_POINT ( 'NONE', #71465 ) ;
#118498 = LINE ( 'NONE', #140960, #40571 ) ;
#118499 = ORIENTED_EDGE ( 'NONE', *, *, #35558, .F. ) ;
#118500 = ADVANCED_FACE ( 'NONE', ( #50432 ), #47608, .T. ) ;
#118501 = CARTESIAN_POINT ( 'NONE',  ( 40.25043019189809712, 3.055000000000002824, -5.291415217122919401 ) ) ;
#118502 = ADVANCED_FACE ( 'NONE', ( #104050 ), #3996, .F. ) ;
#118503 = CIRCLE ( 'NONE', #12012, 2.500000000000000444 ) ;
#118504 = ORIENTED_EDGE ( 'NONE', *, *, #135511, .F. ) ;
#118505 = DIRECTION ( 'NONE',  ( -0.7071067811865486830, 0.7071067811865464625, 0.000000000000000000 ) ) ;
#118506 = EDGE_CURVE ( 'NONE', #103729, #87648, #17081, .T. ) ;
#118507 = CARTESIAN_POINT ( 'NONE',  ( 23.08747294953710494, -6.094999999999989981, 3.732111120401553285E-16 ) ) ;
#118508 = CARTESIAN_POINT ( 'NONE',  ( 13.33798170103910685, 6.458498716420526975, -28.77788784152867052 ) ) ;
#118509 = ORIENTED_EDGE ( 'NONE', *, *, #18812, .T. ) ;
#118510 = DIRECTION ( 'NONE',  ( 0.7071067811865487940, 0.7071067811865463515, -0.000000000000000000 ) ) ;
#118511 = ORIENTED_EDGE ( 'NONE', *, *, #72761, .F. ) ;
#118512 = CARTESIAN_POINT ( 'NONE',  ( 3.436801032208273821, -12.74070752338415069, 9.898150129686367649 ) ) ;
#118513 = CARTESIAN_POINT ( 'NONE',  ( -25.17183060077629619, 9.759292476615618384, 4.000000000000000000 ) ) ;
#118514 = VECTOR ( 'NONE', #134448, 1000.000000000000000 ) ;
#118515 = AXIS2_PLACEMENT_3D ( 'NONE', #142949, #43638, #88596 ) ;
#118517 = ORIENTED_EDGE ( 'NONE', *, *, #124711, .F. ) ;
#118516 = LINE ( 'NONE', #49003, #28549 ) ;
#118518 = VERTEX_POINT ( 'NONE', #80919 ) ;
#118519 = CARTESIAN_POINT ( 'NONE',  ( -17.67183060077634593, 11.25929247661560062, 4.000000000000000000 ) ) ;
#118520 = VECTOR ( 'NONE', #96205, 1000.000000000000000 ) ;
#118521 = DIRECTION ( 'NONE',  ( -0.6830127018922180770, -0.6830127018922204085, -0.2588190451025214056 ) ) ;
#118523 = ORIENTED_EDGE ( 'NONE', *, *, #51554, .T. ) ;
#118522 = VECTOR ( 'NONE', #110964, 1000.000000000000000 ) ;
#118524 = CARTESIAN_POINT ( 'NONE',  ( 109.3083603837962130, 7.949999999999996625, 2.130196079827431088 ) ) ;
#118525 = EDGE_LOOP ( 'NONE', ( #137970, #52072, #56654, #98427 ) ) ;
#118526 = EDGE_LOOP ( 'NONE', ( #113843, #128378, #52030, #71482 ) ) ;
#118527 = EDGE_LOOP ( 'NONE', ( #38934, #64564, #17923, #55431 ) ) ;
#118528 = LINE ( 'NONE', #130871, #107314 ) ;
#118529 = VECTOR ( 'NONE', #29271, 999.9999999999998863 ) ;
#118530 = COLOUR_RGB ( '', 0.40784314, 0.44705882, 0.49803922) ;
#118531 = COLOUR_RGB ( '', 0.66274510, 0.83137255, 0.94901961) ;
#118532 = CARTESIAN_POINT ( 'NONE',  ( 48.48921356237309510, -27.52281430457089328, 5.000000000000000000 ) ) ;
#118533 = LINE ( 'NONE', #117787, #42282 ) ;
#118534 = CARTESIAN_POINT ( 'NONE',  ( 39.48921356237310221, -27.52281430457082934, 5.000000000000000000 ) ) ;
#118535 = CARTESIAN_POINT ( 'NONE',  ( -6.005480084712508493, 28.92564299267933947, 4.000000000000000000 ) ) ;
#118536 = ORIENTED_EDGE ( 'NONE', *, *, #78356, .F. ) ;
#118537 = LINE ( 'NONE', #19236, #74447 ) ;
#118538 = ORIENTED_EDGE ( 'NONE', *, *, #9938, .F. ) ;
#118539 = DIRECTION ( 'NONE',  ( 0.000000000000000000, -0.2631995976047483699, -0.9647414015272167687 ) ) ;
#118540 = CARTESIAN_POINT ( 'NONE',  ( 32.49956980810188867, -3.967499999999998028, -6.871911579029511330 ) ) ;
#118541 = ORIENTED_EDGE ( 'NONE', *, *, #122617, .T. ) ;
#118542 = DIRECTION ( 'NONE',  ( -0.7071067811865486830, -0.7071067811865464625, 0.000000000000000000 ) ) ;
#118543 = PLANE ( 'NONE',  #130021 ) ;
#118544 = ORIENTED_EDGE ( 'NONE', *, *, #142032, .F. ) ;
#118545 = VERTEX_POINT ( 'NONE', #115628 ) ;
#118546 = EDGE_CURVE ( 'NONE', #122251, #3015, #92756, .T. ) ;
#118547 = DIRECTION ( 'NONE',  ( -0.7071067811865486830, 0.7071067811865464625, 0.000000000000000000 ) ) ;
#118548 = LINE ( 'NONE', #19249, #83588 ) ;
#118549 = EDGE_CURVE ( 'NONE', #82762, #92828, #58466, .T. ) ;
#118550 = PLANE ( 'NONE',  #70180 ) ;
#118551 = DIRECTION ( 'NONE',  ( 1.000000000000000000, 0.000000000000000000, -0.000000000000000000 ) ) ;
#118552 = CARTESIAN_POINT ( 'NONE',  ( 0.03269009326452938097, -47.89015928896886720, -37.22465919494650421 ) ) ;
#118553 = CARTESIAN_POINT ( 'NONE',  ( 64.22459685856478018, -1.637169565754161171, 6.109999999999998543 ) ) ;
#118554 = VECTOR ( 'NONE', #126673, 1000.000000000000000 ) ;
#118555 = CARTESIAN_POINT ( 'NONE',  ( -12.00548008471251293, 28.92564299267929684, 4.000000000000000000 ) ) ;
#118556 = CIRCLE ( 'NONE', #115944, 0.5000000000000013323 ) ;
#118557 = DIRECTION ( 'NONE',  ( -0.000000000000000000, -0.3543493200069152693, 0.9351131265310292928 ) ) ;
#118558 = CARTESIAN_POINT ( 'NONE',  ( 25.82816939922335209, 6.759292476615644141, 4.000000000000000000 ) ) ;
#118559 = AXIS2_PLACEMENT_3D ( 'NONE', #8636, #52879, #97079 ) ;
#118560 = ORIENTED_EDGE ( 'NONE', *, *, #136580, .T. ) ;
#118561 = LINE ( 'NONE', #86676, #120487 ) ;
#118562 = EDGE_LOOP ( 'NONE', ( #33859, #35432, #118978, #40022 ) ) ;
#118563 = DIRECTION ( 'NONE',  ( 0.6830127018922180770, -0.6830127018922204085, -0.2588190451025213501 ) ) ;
#118565 = AXIS2_PLACEMENT_3D ( 'NONE', #50859, #29801, #117511 ) ;
#118564 = DIRECTION ( 'NONE',  ( -0.000000000000000000, 0.3543493200069153248, 0.9351131265310292928 ) ) ;
#118566 = ORIENTED_EDGE ( 'NONE', *, *, #72519, .T. ) ;
#118567 = CARTESIAN_POINT ( 'NONE',  ( 0.000000000000000000, 21.72500000000000142, 4.500000000000000888 ) ) ;
#118569 = ORIENTED_EDGE ( 'NONE', *, *, #9064, .F. ) ;
#118568 = LINE ( 'NONE', #32297, #102096 ) ;
#118570 = DIRECTION ( 'NONE',  ( 0.7071067811865486830, -0.7071067811865464625, -0.000000000000000000 ) ) ;
#118571 = EDGE_CURVE ( 'NONE', #141686, #77389, #83050, .T. ) ;
#118572 = CARTESIAN_POINT ( 'NONE',  ( -11.90332935812586612, -2.240707523384257716, 15.26439735382749774 ) ) ;
#118573 = LINE ( 'NONE', #98952, #137543 ) ;
#118574 = EDGE_LOOP ( 'NONE', ( #60883, #56962, #111108, #80762 ) ) ;
#118575 = EDGE_CURVE ( 'NONE', #93434, #65885, #46879, .T. ) ;
#118576 = ORIENTED_EDGE ( 'NONE', *, *, #103919, .T. ) ;
#118577 = LINE ( 'NONE', #19276, #39753 ) ;
#118578 = CARTESIAN_POINT ( 'NONE',  ( 17.99451991528748351, 28.92564299267950645, 4.000000000000000000 ) ) ;
#118579 = UNCERTAINTY_MEASURE_WITH_UNIT (LENGTH_MEASURE( 1.000000000000000082E-05 ), #90180, 'distance_accuracy_value', 'NONE');
#118580 = VECTOR ( 'NONE', #21143, 1000.000000000000000 ) ;
#118581 = CARTESIAN_POINT ( 'NONE',  ( -30.48921356237309510, -27.52281430457076894, 5.000000000000000000 ) ) ;
#118582 = CARTESIAN_POINT ( 'NONE',  ( 93.55836038379622721, -7.949999999999997513, -2.130196079827425759 ) ) ;
#118583 = CARTESIAN_POINT ( 'NONE',  ( 18.47336096364204039, -5.240707523384225297, 16.25846745537499771 ) ) ;
#118584 = LINE ( 'NONE', #54784, #140918 ) ;
#118585 = VERTEX_POINT ( 'NONE', #4707 ) ;
#118586 = ADVANCED_FACE ( 'NONE', ( #49007 ), #93202, .F. ) ;
#118587 = DIRECTION ( 'NONE',  ( 0.7071067811865487940, 0.7071067811865463515, 0.000000000000000000 ) ) ;
#118588 = CARTESIAN_POINT ( 'NONE',  ( 8.423184310185783730, 4.584330080086930965E-16, 0.000000000000000000 ) ) ;
#118590 = CIRCLE ( 'NONE', #16762, 2.500000000000000444 ) ;
#118589 = DIRECTION ( 'NONE',  ( 0.000000000000000000, 0.000000000000000000, 1.000000000000000000 ) ) ;
#118591 = VECTOR ( 'NONE', #75278, 999.9999999999998863 ) ;
#118592 = VERTEX_POINT ( 'NONE', #116388 ) ;
#118593 = EDGE_CURVE ( 'NONE', #134353, #108000, #39566, .T. ) ;
#118594 = CARTESIAN_POINT ( 'NONE',  ( 68.99451991528748351, 28.92564299267986172, 4.000000000000000000 ) ) ;
#118595 = ORIENTED_EDGE ( 'NONE', *, *, #115262, .F. ) ;
#118596 = CARTESIAN_POINT ( 'NONE',  ( 78.16709685856476142, -3.055000000000000160, -5.291415217122921177 ) ) ;
#118597 = DIRECTION ( 'NONE',  ( -1.000000000000000000, -1.224606353822377258E-16, -0.000000000000000000 ) ) ;
#118599 = AXIS2_PLACEMENT_3D ( 'NONE', #123219, #23890, #101433 ) ;
#118598 = DIRECTION ( 'NONE',  ( -0.000000000000000000, -0.3543493200069152693, 0.9351131265310292928 ) ) ;
#118600 = ORIENTED_EDGE ( 'NONE', *, *, #100107, .T. ) ;
#118601 = EDGE_CURVE ( 'NONE', #118193, #131497, #60623, .T. ) ;
#118602 = FACE_OUTER_BOUND ( 'NONE', #76068, .T. ) ;
#118603 =( BOUNDED_CURVE ( )  B_SPLINE_CURVE ( 2, ( #123642, #112035, #134504, #24297, #114154, #80841, #58408, #91689, #77981, #100438, #91008, #25718, #1091 ),
 .UNSPECIFIED., .F., .T. ) 
 B_SPLINE_CURVE_WITH_KNOTS ( ( 3, 2, 2, 2, 2, 2, 3 ),
 ( 0.7833333333333333259, 0.7861111111111110938, 0.7888888888888888618, 0.7916666666666666297, 0.7944444444444443976, 0.7972222222222222765, 0.8000000000000000444 ),
 .UNSPECIFIED. ) 
 CURVE ( )  GEOMETRIC_REPRESENTATION_ITEM ( )  RATIONAL_B_SPLINE_CURVE ( ( 1.000000000000000000, 0.9659258262890683122, 1.000000000000000000, 0.9659258262890683122, 1.000000000000000000, 0.9659258262890683122, 1.000000000000000000, 0.9659258262890683122, 1.000000000000000000, 0.9659258262890683122, 1.000000000000000000, 0.9659258262890683122, 1.000000000000000000 ) ) 
 REPRESENTATION_ITEM ( '' )  );
#118604 = CARTESIAN_POINT ( 'NONE',  ( 42.29974487139158157, -27.71228299555235708, 4.000000000000000000 ) ) ;
#118605 = CARTESIAN_POINT ( 'NONE',  ( 26.99999999999980815, 1.931123077392165488, 4.000000000000000000 ) ) ;
#118606 = LINE ( 'NONE', #33081, #50915 ) ;
#118608 = ORIENTED_EDGE ( 'NONE', *, *, #47562, .T. ) ;
#118607 = CARTESIAN_POINT ( 'NONE',  ( -6.489213562373093325, -27.52281430457059841, 5.000000000000000000 ) ) ;
#118609 = DIRECTION ( 'NONE',  ( 0.3543493200069162685, -0.000000000000000000, -0.9351131265310288487 ) ) ;
#118610 = AXIS2_PLACEMENT_3D ( 'NONE', #66898, #98100, #111080 ) ;
#118611 = CARTESIAN_POINT ( 'NONE',  ( 78.00000000000000000, 0.000000000000000000, -7.950000000000000178 ) ) ;
#118612 = CARTESIAN_POINT ( 'NONE',  ( 60.06249999999998579, -5.819803920172573086, -5.819803920172573974 ) ) ;
#118613 = ORIENTED_EDGE ( 'NONE', *, *, #127014, .F. ) ;
#118614 = ORIENTED_EDGE ( 'NONE', *, *, #113865, .F. ) ;
#118615 = CARTESIAN_POINT ( 'NONE',  ( 71.16709685856477563, -3.055000000000000160, -5.291415217122921177 ) ) ;
#118616 = ORIENTED_EDGE ( 'NONE', *, *, #9655, .T. ) ;
#118617 = CARTESIAN_POINT ( 'NONE',  ( -35.99451991528749772, 28.92564299267963079, 4.000000000000000000 ) ) ;
#118618 = ADVANCED_FACE ( 'NONE', ( #128004 ), #53255, .F. ) ;
#118619 = CARTESIAN_POINT ( 'NONE',  ( -7.499999999999940492, -5.947814304570770538, 5.000000000000000000 ) ) ;
#118620 = LINE ( 'NONE', #119324, #78012 ) ;
#118621 = ORIENTED_EDGE ( 'NONE', *, *, #62707, .T. ) ;
#118622 = VECTOR ( 'NONE', #117292, 1000.000000000000000 ) ;
#118623 = VECTOR ( 'NONE', #35490, 1000.000000000000000 ) ;
#118624 = VECTOR ( 'NONE', #100648, 1000.000000000000000 ) ;
#118625 = CARTESIAN_POINT ( 'NONE',  ( 24.18398860626899705, 28.73617430169804265, 5.000000000000000000 ) ) ;
#118626 = DIRECTION ( 'NONE',  ( 0.000000000000000000, -1.000000000000000000, 0.000000000000000000 ) ) ;
#118627 = ADVANCED_FACE ( 'NONE', ( #96048 ), #6867, .F. ) ;
#118629 = EDGE_CURVE ( 'NONE', #31572, #95905, #140976, .T. ) ;
#118628 = CIRCLE ( 'NONE', #76965, 2.500000000000000888 ) ;
#118630 = AXIS2_PLACEMENT_3D ( 'NONE', #93533, #70406, #114554 ) ;
#118631 = ORIENTED_EDGE ( 'NONE', *, *, #69687, .F. ) ;
#118632 = CARTESIAN_POINT ( 'NONE',  ( 17.99999999999987566, 13.55218569542903140, 5.000000000000000000 ) ) ;
#118634 = CARTESIAN_POINT ( 'NONE',  ( -14.20710678118644488, 9.759292476615623713, 5.000000000000000000 ) ) ;
#118633 = AXIS2_PLACEMENT_3D ( 'NONE', #92941, #126981, #39290 ) ;
#118635 = PLANE ( 'NONE',  #49309 ) ;
#118636 = VECTOR ( 'NONE', #890, 999.9999999999998863 ) ;
#118637 =( GEOMETRIC_REPRESENTATION_CONTEXT ( 3 ) GLOBAL_UNCERTAINTY_ASSIGNED_CONTEXT ( ( #83829 ) ) GLOBAL_UNIT_ASSIGNED_CONTEXT ( ( #131855, #53581, #99182 ) ) REPRESENTATION_CONTEXT ( 'NONE', 'WORKASPACE' ) );
#118638 = EDGE_CURVE ( 'NONE', #21943, #68002, #31529, .T. ) ;
#118639 = ORIENTED_EDGE ( 'NONE', *, *, #68612, .F. ) ;
#118640 = ORIENTED_EDGE ( 'NONE', *, *, #82160, .F. ) ;
#118641 = EDGE_CURVE ( 'NONE', #62908, #28061, #141727, .T. ) ;
#118642 = CARTESIAN_POINT ( 'NONE',  ( 66.48921356237309510, -27.52281430457101763, 5.000000000000000000 ) ) ;
#118643 = EDGE_CURVE ( 'NONE', #83478, #122408, #9755, .T. ) ;
#118644 = CARTESIAN_POINT ( 'NONE',  ( 22.85159235450332105, -3.851859888774471706E-31, 2.500000000000001332 ) ) ;
#118645 = DIRECTION ( 'NONE',  ( -0.7071067811865487940, 0.7071067811865463515, -0.000000000000000000 ) ) ;
#118646 = DIRECTION ( 'NONE',  ( -1.000000000000000000, -0.000000000000000000, 0.000000000000000000 ) ) ;
#118647 = DIRECTION ( 'NONE',  ( -0.6830127018922181881, 0.6830127018922202975, -0.2588190451025214056 ) ) ;
#118648 = CARTESIAN_POINT ( 'NONE',  ( 15.18398860626900237, 28.73617430169797871, 5.000000000000000000 ) ) ;
#118649 = SURFACE_STYLE_FILL_AREA ( #44718 ) ;
#118650 = ORIENTED_EDGE ( 'NONE', *, *, #115746, .F. ) ;
#118651 = ADVANCED_FACE ( 'NONE', ( #106927 ), #51145, .T. ) ;
#118652 = CONICAL_SURFACE ( 'NONE', #137201, 2.055000000000001048, 0.9599310885968758145 ) ;
#118653 = ORIENTED_EDGE ( 'NONE', *, *, #108259, .T. ) ;
#118654 = ORIENTED_EDGE ( 'NONE', *, *, #79594, .F. ) ;
#118655 = ADVANCED_FACE ( 'NONE', ( #95341 ), #119921, .F. ) ;
#118656 = ORIENTED_EDGE ( 'NONE', *, *, #46347, .F. ) ;
#118657 = CARTESIAN_POINT ( 'NONE',  ( 183.9400257540257826, -51.66308182546811878, 38.35990878063730491 ) ) ;
#118658 = EDGE_CURVE ( 'NONE', #91232, #68141, #54020, .T. ) ;
#118659 = VECTOR ( 'NONE', #15238, 1000.000000000000000 ) ;
#118660 = LINE ( 'NONE', #41820, #110245 ) ;
#118661 = LINE ( 'NONE', #53406, #107286 ) ;
#118662 = ORIENTED_EDGE ( 'NONE', *, *, #112848, .F. ) ;
#118663 = CARTESIAN_POINT ( 'NONE',  ( 3.087196949643289834, 3.821174125832445049E-16, 0.000000000000000000 ) ) ;
#118664 = CARTESIAN_POINT ( 'NONE',  ( -8.994519915287490619, 28.92564299267944250, 4.000000000000000000 ) ) ;
#118665 = VECTOR ( 'NONE', #80932, 1000.000000000000227 ) ;
#118666 = CARTESIAN_POINT ( 'NONE',  ( 57.82919371712954870, -3.975000000000001865, 6.884901960086284411 ) ) ;
#118667 = CARTESIAN_POINT ( 'NONE',  ( -19.05000000000000071, 3.174999999999997158, 4.000000000000000000 ) ) ;
#118668 = VECTOR ( 'NONE', #81563, 1000.000000000000000 ) ;
#118669 = CONICAL_SURFACE ( 'NONE', #42331, 2.055000000000000604, 0.9599310885968764806 ) ;
#118670 = CARTESIAN_POINT ( 'NONE',  ( -1.171830600776462061, -14.24070752338414358, 4.000000000000000000 ) ) ;
#118671 = VERTEX_POINT ( 'NONE', #40976 ) ;
#118672 = PLANE ( 'NONE',  #14845 ) ;
#118673 = CARTESIAN_POINT ( 'NONE',  ( -33.29974487139158867, -27.71228299555229313, 4.000000000000000000 ) ) ;
#118674 = VERTEX_POINT ( 'NONE', #74331 ) ;
#118675 = LINE ( 'NONE', #40428, #48202 ) ;
#118676 = ORIENTED_EDGE ( 'NONE', *, *, #140704, .F. ) ;
#118677 = ORIENTED_EDGE ( 'NONE', *, *, #125743, .F. ) ;
#118678 = CARTESIAN_POINT ( 'NONE',  ( 60.66709685856477563, -3.055000000000000160, -5.291415217122921177 ) ) ;
#118679 = VERTEX_POINT ( 'NONE', #64162 ) ;
#118680 = ORIENTED_EDGE ( 'NONE', *, *, #70044, .F. ) ;
#118681 = EDGE_CURVE ( 'NONE', #70528, #50028, #129389, .T. ) ;
#118682 = DIRECTION ( 'NONE',  ( -3.166071393695993333E-32, 1.016133275908817741E-16, -1.000000000000000000 ) ) ;
#118683 = EDGE_CURVE ( 'NONE', #76159, #54903, #85172, .T. ) ;
#118684 = CARTESIAN_POINT ( 'NONE',  ( -20.14994871458963033, -8.240707523384193323, 17.25253755692234492 ) ) ;
#118685 = CARTESIAN_POINT ( 'NONE',  ( 102.8129301918981042, -1.637169565754159617, -6.110000000000001208 ) ) ;
#118686 = DIRECTION ( 'NONE',  ( 0.6830127018922181881, 0.6830127018922202975, -0.2588190451025214056 ) ) ;
#118687 = VECTOR ( 'NONE', #105959, 1000.000000000000000 ) ;
#118688 = CARTESIAN_POINT ( 'NONE',  ( -33.18398860626899705, 28.73617430169810305, 5.000000000000000000 ) ) ;
#118689 = VECTOR ( 'NONE', #111267, 1000.000000000000000 ) ;
#118690 = EDGE_CURVE ( 'NONE', #104350, #94114, #30078, .T. ) ;
#118691 = DIRECTION ( 'NONE',  ( -0.7071067811865486830, -0.7071067811865464625, 0.000000000000000000 ) ) ;
#118692 = CARTESIAN_POINT ( 'NONE',  ( 91.12500000000000000, -7.950000000000000178, -4.867971026610729436E-16 ) ) ;
#118693 = CARTESIAN_POINT ( 'NONE',  ( 32.12514619309215647, -14.24070752338413115, 9.401115078912585687 ) ) ;
#118694 = VERTEX_POINT ( 'NONE', #108322 ) ;
#118695 = DIRECTION ( 'NONE',  ( -1.000000000000000000, -0.000000000000000000, 0.000000000000000000 ) ) ;
#118696 = EDGE_LOOP ( 'NONE', ( #111859, #25120, #52551, #136017 ) ) ;
#118697 = VERTEX_POINT ( 'NONE', #8993 ) ;
#118698 = EDGE_LOOP ( 'NONE', ( #135999, #115529, #66144, #140781 ) ) ;
#118700 = EDGE_LOOP ( 'NONE', ( #58116, #85432, #86095, #121009, #134934 ) ) ;
#118699 = VECTOR ( 'NONE', #129498, 1000.000000000000000 ) ;
#118701 = DIRECTION ( 'NONE',  ( -0.3543493200069162685, -0.000000000000000000, -0.9351131265310288487 ) ) ;
#118702 = DIRECTION ( 'NONE',  ( -1.000000000000000000, 0.000000000000000000, 0.000000000000000000 ) ) ;
#118703 = CARTESIAN_POINT ( 'NONE',  ( 17.99999999999986855, -0.2811185226894163947, -5.995736974527558161 ) ) ;
#118704 = VERTEX_POINT ( 'NONE', #107642 ) ;
#118705 = CARTESIAN_POINT ( 'NONE',  ( 0.000000000000000000, -49.85820393249939286, 34.92500000000001847 ) ) ;
#118706 = AXIS2_PLACEMENT_3D ( 'NONE', #3409, #13569, #14307 ) ;
#118707 = ORIENTED_EDGE ( 'NONE', *, *, #74400, .T. ) ;
#118708 = CARTESIAN_POINT ( 'NONE',  ( 7.270403141435218153, -7.934999999999989839, 2.126176841940957907 ) ) ;
#118709 = LINE ( 'NONE', #19403, #89969 ) ;
#118710 = DIRECTION ( 'NONE',  ( 0.6830127018922181881, 0.6830127018922202975, -0.2588190451025214056 ) ) ;
#118711 = VERTEX_POINT ( 'NONE', #84497 ) ;
#118712 = VERTEX_POINT ( 'NONE', #118519 ) ;
#118713 = ORIENTED_EDGE ( 'NONE', *, *, #64815, .T. ) ;
#118714 = CARTESIAN_POINT ( 'NONE',  ( 17.99999999999987566, -7.447814304570745669, 5.000000000000000000 ) ) ;
#118715 = CARTESIAN_POINT ( 'NONE',  ( -54.29974487139159578, -27.71228299555243879, 4.000000000000000000 ) ) ;
#118716 = AXIS2_PLACEMENT_3D ( 'NONE', #48671, #103724, #68319 ) ;
#118717 = CARTESIAN_POINT ( 'NONE',  ( 16.82816939922341959, 21.75929247661549581, 4.000000000000000000 ) ) ;
#118718 = DIRECTION ( 'NONE',  ( -0.000000000000000000, -1.000000000000000000, -0.000000000000000000 ) ) ;
#118719 = AXIS2_PLACEMENT_3D ( 'NONE', #129220, #63989, #140805 ) ;
#118720 = PLANE ( 'NONE',  #6270 ) ;
#118721 = VECTOR ( 'NONE', #47068, 999.9999999999998863 ) ;
#118722 = EDGE_CURVE ( 'NONE', #114222, #106767, #18465, .T. ) ;
#118723 = DIRECTION ( 'NONE',  ( 1.000000000000000000, 0.000000000000000000, 0.000000000000000000 ) ) ;
#118724 = CARTESIAN_POINT ( 'NONE',  ( 25.52126352523142927, -4.472830434245839371, -4.472830434245840259 ) ) ;
#118725 = PLANE ( 'NONE',  #30152 ) ;
#118726 = PRESENTATION_STYLE_ASSIGNMENT (( #139809 ) ) ;
#118727 = ORIENTED_EDGE ( 'NONE', *, *, #38165, .F. ) ;
#118728 = CARTESIAN_POINT ( 'NONE',  ( -20.99999999999985789, 20.70535890316559957, 1.956823837851964676 ) ) ;
#118729 = VECTOR ( 'NONE', #11871, 1000.000000000000000 ) ;
#118730 = AXIS2_PLACEMENT_3D ( 'NONE', #104125, #117159, #4791 ) ;
#118731 = CYLINDRICAL_SURFACE ( 'NONE', #133302, 7.950000000000000178 ) ;
#118732 = ORIENTED_EDGE ( 'NONE', *, *, #67255, .F. ) ;
#118733 = ADVANCED_FACE ( 'NONE', ( #119228 ), #62745, .F. ) ;
#118734 = CARTESIAN_POINT ( 'NONE',  ( 42.48921356237308800, -27.52281430457085065, 5.000000000000000000 ) ) ;
#118736 = ORIENTED_EDGE ( 'NONE', *, *, #35021, .T. ) ;
#118735 = CARTESIAN_POINT ( 'NONE',  ( 54.24578869845078799, -47.96374157527412052, -37.32649486623387247 ) ) ;
#118737 = EDGE_CURVE ( 'NONE', #112685, #37409, #52552, .T. ) ;
#118738 = DIRECTION ( 'NONE',  ( -0.000000000000000000, 0.3543493200069153248, 0.9351131265310292928 ) ) ;
#118739 = VERTEX_POINT ( 'NONE', #85896 ) ;
#118740 = DIRECTION ( 'NONE',  ( 0.3543493200069162685, -0.000000000000000000, -0.9351131265310288487 ) ) ;
#118741 = VERTEX_POINT ( 'NONE', #130136 ) ;
#118742 = EDGE_CURVE ( 'NONE', #71945, #17161, #286, .T. ) ;
#118743 = EDGE_CURVE ( 'NONE', #100040, #37058, #23494, .T. ) ;
#118744 = CARTESIAN_POINT ( 'NONE',  ( 31.49999999999979039, 10.46639925780216096, 5.000000000000000000 ) ) ;
#118745 = CARTESIAN_POINT ( 'NONE',  ( 125.9333603837962414, 2.130196079827431532, -7.949999999999997513 ) ) ;
#118746 = DIRECTION ( 'NONE',  ( -0.000000000000000000, 0.3543493200069153248, 0.9351131265310292928 ) ) ;
#118747 = VECTOR ( 'NONE', #81513, 1000.000000000000000 ) ;
#118748 = LINE ( 'NONE', #143360, #71732 ) ;
#118749 = ADVANCED_FACE ( 'NONE', ( #33688 ), #1010, .T. ) ;
#118750 = DIRECTION ( 'NONE',  ( -0.3543493200069162685, -0.000000000000000000, -0.9351131265310288487 ) ) ;
#118751 = DIRECTION ( 'NONE',  ( 0.3543493200069162685, -0.000000000000000000, -0.9351131265310288487 ) ) ;
#118752 = FACE_OUTER_BOUND ( 'NONE', #62108, .T. ) ;
#118753 = CARTESIAN_POINT ( 'NONE',  ( 7.875000000000000000, -6.094999999999989981, 3.732111120401553285E-16 ) ) ;
#118754 = CARTESIAN_POINT ( 'NONE',  ( 19.81206980810188512, 7.934999999999992504, 2.126176841940951689 ) ) ;
#118755 = DIRECTION ( 'NONE',  ( -1.000000000000000000, -1.224606353822377258E-16, -0.000000000000000000 ) ) ;
#118756 = CARTESIAN_POINT ( 'NONE',  ( 54.48921356237310221, -27.52281430457093236, 5.000000000000000000 ) ) ;
#118757 = ORIENTED_EDGE ( 'NONE', *, *, #113676, .F. ) ;
#118758 = VECTOR ( 'NONE', #31861, 1000.000000000000227 ) ;
#118759 = ORIENTED_EDGE ( 'NONE', *, *, #24396, .F. ) ;
#118760 = EDGE_CURVE ( 'NONE', #137006, #26733, #77888, .T. ) ;
#118761 = CARTESIAN_POINT ( 'NONE',  ( -63.48921356237309510, -27.52281430457099631, 5.000000000000000000 ) ) ;
#118762 = ORIENTED_EDGE ( 'NONE', *, *, #45530, .F. ) ;
#118763 = PRODUCT ( '1.4 Collar', '1.4 Collar', '', ( #37363 ) ) ;
#118764 = AXIS2_PLACEMENT_3D ( 'NONE', #35859, #13321, #25645 ) ;
#118765 = LINE ( 'NONE', #86872, #89645 ) ;
#118766 = DIRECTION ( 'NONE',  ( 0.7071067811865486830, -0.7071067811865464625, -0.000000000000000000 ) ) ;
#118767 = DIRECTION ( 'NONE',  ( -1.000000000000000000, 0.000000000000000000, 0.000000000000000000 ) ) ;
#118768 = ORIENTED_EDGE ( 'NONE', *, *, #15228, .T. ) ;
#118769 = EDGE_CURVE ( 'NONE', #2157, #33478, #21364, .T. ) ;
#118770 = CARTESIAN_POINT ( 'NONE',  ( -34.45011844616454511, 3.002304141593926001, 5.000000000000000888 ) ) ;
#118771 = CARTESIAN_POINT ( 'NONE',  ( 93.16666666666667140, 6.884901960086285300, 3.975000000000003642 ) ) ;
#118772 = CARTESIAN_POINT ( 'NONE',  ( 69.29974487139159578, -27.71228299555254537, 4.000000000000000000 ) ) ;
#118773 = PLANE ( 'NONE',  #40192 ) ;
#118775 = ORIENTED_EDGE ( 'NONE', *, *, #136145, .T. ) ;
#118774 = FACE_OUTER_BOUND ( 'NONE', #16477, .T. ) ;
#118776 = CARTESIAN_POINT ( 'NONE',  ( 40.22916666666666430, 7.950000000000001954, -2.130196079827421762 ) ) ;
#118777 = EDGE_CURVE ( 'NONE', #9875, #68247, #135152, .T. ) ;
#118778 = CARTESIAN_POINT ( 'NONE',  ( -25.39999999999996305, 0.000000000000000000, 0.000000000000000000 ) ) ;
#118779 = LINE ( 'NONE', #9265, #14613 ) ;
#118780 = CARTESIAN_POINT ( 'NONE',  ( 51.48921356237309510, -27.52281430457091460, 5.000000000000000000 ) ) ;
#118781 =( BOUNDED_CURVE ( )  B_SPLINE_CURVE ( 3, ( #10840, #68851, #134829, #44239 ),
 .UNSPECIFIED., .F., .T. ) 
 B_SPLINE_CURVE_WITH_KNOTS ( ( 4, 4 ),
 ( 1.208578181583247257, 1.359146454359469125 ),
 .UNSPECIFIED. ) 
 CURVE ( )  GEOMETRIC_REPRESENTATION_ITEM ( )  RATIONAL_B_SPLINE_CURVE ( ( 1.000000000000000000, 0.9981116584018947524, 0.9981116584018947524, 1.000000000000000000 ) ) 
 REPRESENTATION_ITEM ( '' )  );
#118782 = CARTESIAN_POINT ( 'NONE',  ( 12.19999999999999574, -25.33999999999998565, 3.000000000000002665 ) ) ;
#118783 = ORIENTED_EDGE ( 'NONE', *, *, #25136, .T. ) ;
#118784 = ORIENTED_EDGE ( 'NONE', *, *, #95723, .T. ) ;
#118785 = VERTEX_POINT ( 'NONE', #77202 ) ;
#118786 = CARTESIAN_POINT ( 'NONE',  ( 105.7295968585647898, -6.110000000000000320, -1.637169565754161393 ) ) ;
#118787 = VECTOR ( 'NONE', #102534, 1000.000000000000000 ) ;
#118788 = ORIENTED_EDGE ( 'NONE', *, *, #106487, .F. ) ;
#118789 = VECTOR ( 'NONE', #103843, 1000.000000000000227 ) ;
#118790 = EDGE_CURVE ( 'NONE', #4524, #69699, #133010, .T. ) ;
#118791 = DIRECTION ( 'NONE',  ( 0.6830127018922181881, 0.6830127018922202975, -0.2588190451025214056 ) ) ;
#118792 = AXIS2_PLACEMENT_3D ( 'NONE', #14481, #23942, #90632 ) ;
#118793 = CARTESIAN_POINT ( 'NONE',  ( 35.99451991528749772, 28.92564299267963079, 4.000000000000000000 ) ) ;
#118794 = ORIENTED_EDGE ( 'NONE', *, *, #47082, .F. ) ;
#118795 = LINE ( 'NONE', #29632, #2784 ) ;
#118796 = CARTESIAN_POINT ( 'NONE',  ( 33.29974487139158867, -27.71228299555229313, 4.000000000000000000 ) ) ;
#118797 = EDGE_CURVE ( 'NONE', #92018, #10755, #2995, .T. ) ;
#118798 = CARTESIAN_POINT ( 'NONE',  ( 92.37043019189810877, -3.055000000000001492, 5.291415217122917625 ) ) ;
#118799 = VERTEX_POINT ( 'NONE', #110482 ) ;
#118800 = EDGE_CURVE ( 'NONE', #43949, #103933, #57584, .T. ) ;
#118801 = DIRECTION ( 'NONE',  ( -0.7071067811865486830, -0.7071067811865464625, -0.000000000000000000 ) ) ;
#118802 = LINE ( 'NONE', #73191, #98555 ) ;
#118803 = AXIS2_PLACEMENT_3D ( 'NONE', #59144, #48218, #103294 ) ;
#118804 = DIRECTION ( 'NONE',  ( 1.000000000000000000, 0.000000000000000000, 0.000000000000000000 ) ) ;
#118805 = CARTESIAN_POINT ( 'NONE',  ( 10.49999999999992895, -2.568876922607790103, 4.000000000000000000 ) ) ;
#118806 = EDGE_CURVE ( 'NONE', #131683, #129739, #56886, .T. ) ;
#118807 = ORIENTED_EDGE ( 'NONE', *, *, #54736, .F. ) ;
#118808 = ORIENTED_EDGE ( 'NONE', *, *, #143521, .T. ) ;
#118809 = ORIENTED_EDGE ( 'NONE', *, *, #34511, .F. ) ;
#118810 = CARTESIAN_POINT ( 'NONE',  ( 8.999999999999934275, -10.06887692260770706, 4.000000000000000000 ) ) ;
#118811 = PLANE ( 'NONE',  #17620 ) ;
#118812 = CARTESIAN_POINT ( 'NONE',  ( 18.44206980810188767, 7.934999999999992504, 2.126176841940951689 ) ) ;
#118813 = VECTOR ( 'NONE', #83718, 1000.000000000000227 ) ;
#118814 = DIRECTION ( 'NONE',  ( -0.7071067811865486830, -0.7071067811865464625, 0.000000000000000000 ) ) ;
#118815 = CARTESIAN_POINT ( 'NONE',  ( 34.45011844616451668, 12.00230414159381453, 5.000000000000000888 ) ) ;
#118816 =( NAMED_UNIT ( * ) SI_UNIT ( $, .STERADIAN. ) SOLID_ANGLE_UNIT ( ) );
#118817 = ORIENTED_EDGE ( 'NONE', *, *, #85028, .F. ) ;
#118818 = ORIENTED_EDGE ( 'NONE', *, *, #38711, .F. ) ;
#118819 = EDGE_CURVE ( 'NONE', #101003, #114903, #116893, .T. ) ;
#118820 = LINE ( 'NONE', #139181, #82782 ) ;
#118821 = ORIENTED_EDGE ( 'NONE', *, *, #61221, .F. ) ;
#118822 = VERTEX_POINT ( 'NONE', #55427 ) ;
#118823 = VECTOR ( 'NONE', #96239, 1000.000000000000227 ) ;
#118824 = EDGE_CURVE ( 'NONE', #16046, #29609, #99611, .T. ) ;
#118825 = AXIS2_PLACEMENT_3D ( 'NONE', #8109, #8793, #96538 ) ;
#118826 = DIRECTION ( 'NONE',  ( 0.7071067811865486830, -0.7071067811865464625, -0.000000000000000000 ) ) ;
#118827 = DIRECTION ( 'NONE',  ( -0.7071067811865486830, -0.7071067811865464625, -0.000000000000000000 ) ) ;
#118828 = VERTEX_POINT ( 'NONE', #88780 ) ;
#118829 = DIRECTION ( 'NONE',  ( -1.000000000000000000, 0.000000000000000000, 0.000000000000000000 ) ) ;
#118830 = SURFACE_STYLE_FILL_AREA ( #30406 ) ;
#118831 = LINE ( 'NONE', #129700, #121916 ) ;
#118832 = AXIS2_PLACEMENT_3D ( 'NONE', #48837, #40122, #104622 ) ;
#118833 = PRODUCT_DEFINITION_FORMATION_WITH_SPECIFIED_SOURCE ( 'ANY', '', #120757, .NOT_KNOWN. ) ;
#118834 = DIRECTION ( 'NONE',  ( 0.7071067811865487940, 0.7071067811865463515, 0.000000000000000000 ) ) ;
#118835 = LINE ( 'NONE', #61636, #16506 ) ;
#118836 = ORIENTED_EDGE ( 'NONE', *, *, #34008, .F. ) ;
#118837 = LINE ( 'NONE', #120974, #97399 ) ;
#118838 = CARTESIAN_POINT ( 'NONE',  ( -0.4892135623730947680, -27.52281430457055578, 5.000000000000000000 ) ) ;
#118839 = ORIENTED_EDGE ( 'NONE', *, *, #119618, .T. ) ;
#118840 = CARTESIAN_POINT ( 'NONE',  ( 25.40000000000000568, -1.106537714668802241, -7.868010767219997703 ) ) ;
#118841 = DIRECTION ( 'NONE',  ( -0.000000000000000000, 1.000000000000000000, -0.000000000000000000 ) ) ;
#118842 = EDGE_LOOP ( 'NONE', ( #21347, #141155, #45558, #70531 ) ) ;
#118843 = PRESENTATION_STYLE_ASSIGNMENT (( #86237 ) ) ;
#118844 = ORIENTED_EDGE ( 'NONE', *, *, #3330, .F. ) ;
#118845 = CARTESIAN_POINT ( 'NONE',  ( 28.49999999999980815, 4.087461875839198733, 4.000000000000000000 ) ) ;
#118846 = EDGE_LOOP ( 'NONE', ( #112456, #58977, #98757, #51912 ) ) ;
#118847 = VERTEX_POINT ( 'NONE', #1700 ) ;
#118848 = VECTOR ( 'NONE', #106334, 1000.000000000000000 ) ;
#118849 = VERTEX_POINT ( 'NONE', #45993 ) ;
#118850 = EDGE_CURVE ( 'NONE', #19554, #98048, #72421, .T. ) ;
#118851 = CARTESIAN_POINT ( 'NONE',  ( 33.16209685856478018, -5.291415217122919401, 3.054999999999997939 ) ) ;
#118852 =( GEOMETRIC_REPRESENTATION_CONTEXT ( 3 ) GLOBAL_UNCERTAINTY_ASSIGNED_CONTEXT ( ( #88109 ) ) GLOBAL_UNIT_ASSIGNED_CONTEXT ( ( #116066, #79930, #58179 ) ) REPRESENTATION_CONTEXT ( 'NONE', 'WORKASPACE' ) );
#118853 = CARTESIAN_POINT ( 'NONE',  ( 6.489213562373093325, -27.52281430457059841, 5.000000000000000000 ) ) ;
#118854 = CARTESIAN_POINT ( 'NONE',  ( 11.99999999999992006, 1.761378380278694866, -6.096875308897227619 ) ) ;
#118855 = CARTESIAN_POINT ( 'NONE',  ( 125.8545968585647614, -1.637169565754161615, 6.110000000000000320 ) ) ;
#118856 = LINE ( 'NONE', #19544, #42799 ) ;
#118857 = CARTESIAN_POINT ( 'NONE',  ( -20.99999999999985079, -12.41253812416062807, 4.000000000000000000 ) ) ;
#118858 = LINE ( 'NONE', #86250, #92086 ) ;
#118860 = DIRECTION ( 'NONE',  ( -0.7071067811865486830, -0.7071067811865464625, 0.000000000000000000 ) ) ;
#118859 = AXIS2_PLACEMENT_3D ( 'NONE', #55423, #122078, #109789 ) ;
#118861 = CARTESIAN_POINT ( 'NONE',  ( 21.79333936457832266, 21.75929247661549226, 4.998822639870715179 ) ) ;
#118862 = DIRECTION ( 'NONE',  ( -1.000000000000000000, -1.224606353822377258E-16, -0.000000000000000000 ) ) ;
#118863 = VECTOR ( 'NONE', #67013, 1000.000000000000227 ) ;
#118864 = DIRECTION ( 'NONE',  ( 0.000000000000000000, -1.000000000000000000, 0.000000000000000000 ) ) ;
#118865 = ORIENTED_EDGE ( 'NONE', *, *, #39435, .F. ) ;
#118866 = EDGE_LOOP ( 'NONE', ( #108006, #89186, #30179, #77337 ) ) ;
#118867 = ORIENTED_EDGE ( 'NONE', *, *, #51367, .F. ) ;
#118868 = VERTEX_POINT ( 'NONE', #90923 ) ;
#118869 = CARTESIAN_POINT ( 'NONE',  ( 19.58990935480156992, 9.759292476615625489, 11.28811694763783180 ) ) ;
#118870 = VERTEX_POINT ( 'NONE', #22744 ) ;
#118871 = AXIS2_PLACEMENT_3D ( 'NONE', #66324, #9010, #97486 ) ;
#118872 = EDGE_LOOP ( 'NONE', ( #101926, #120834, #36330, #136565, #2070, #65777 ) ) ;
#118873 = DIRECTION ( 'NONE',  ( 0.5735764363510451602, 0.8191520442889924647, 0.000000000000000000 ) ) ;
#118874 =( LENGTH_UNIT ( ) NAMED_UNIT ( * ) SI_UNIT ( .MILLI., .METRE. ) );
#118875 = CARTESIAN_POINT ( 'NONE',  ( -18.00548008471250583, 28.92564299267925776, 4.000000000000000000 ) ) ;
#118876 = ORIENTED_EDGE ( 'NONE', *, *, #8084, .F. ) ;
#118877 = PLANE ( 'NONE',  #48778 ) ;
#118878 = VERTEX_POINT ( 'NONE', #44586 ) ;
#118880 = VECTOR ( 'NONE', #65761, 1000.000000000000000 ) ;
#118879 = DIRECTION ( 'NONE',  ( 0.000000000000000000, 0.000000000000000000, -1.000000000000000000 ) ) ;
#118881 = LINE ( 'NONE', #52199, #98310 ) ;
#118882 = AXIS2_PLACEMENT_3D ( 'NONE', #123896, #69516, #2796 ) ;
#118883 = CARTESIAN_POINT ( 'NONE',  ( 9.546236474768553748, -7.934999999999990727, 4.858786175617117713E-16 ) ) ;
#118884 = VERTEX_POINT ( 'NONE', #67012 ) ;
#118885 = CARTESIAN_POINT ( 'NONE',  ( 89.30793019189809456, -6.109999999999999432, 1.637169565754158507 ) ) ;
#118886 = LINE ( 'NONE', #3163, #87612 ) ;
#118887 = DIRECTION ( 'NONE',  ( -0.7071067811865487940, 0.7071067811865463515, 0.000000000000000000 ) ) ;
#118888 = FACE_OUTER_BOUND ( 'NONE', #30922, .T. ) ;
#118889 = ORIENTED_EDGE ( 'NONE', *, *, #57135, .T. ) ;
#118890 = ORIENTED_EDGE ( 'NONE', *, *, #51693, .F. ) ;
#118891 = DIRECTION ( 'NONE',  ( -0.7071067811865487940, 0.7071067811865463515, -0.000000000000000000 ) ) ;
#118892 = VERTEX_POINT ( 'NONE', #100358 ) ;
#118893 = DIRECTION ( 'NONE',  ( 1.000000000000000000, 1.224606353822377258E-16, 0.000000000000000000 ) ) ;
#118894 = CARTESIAN_POINT ( 'NONE',  ( 54.29974487139159578, -27.71228299555243879, 4.000000000000000000 ) ) ;
#118895 = CARTESIAN_POINT ( 'NONE',  ( -34.45011844616454511, -13.48371918836238059, 5.000000000000000888 ) ) ;
#118896 = CARTESIAN_POINT ( 'NONE',  ( 7.001930566820925961, -22.22500000000000142, 4.500000000000000888 ) ) ;
#118897 = EDGE_LOOP ( 'NONE', ( #48104, #99310, #28770, #130041 ) ) ;
#118898 = CARTESIAN_POINT ( 'NONE',  ( 14.08373646989360317, 3.821174125832445049E-16, 0.000000000000000000 ) ) ;
#118899 = LINE ( 'NONE', #51532, #111683 ) ;
#118900 = VERTEX_POINT ( 'NONE', #2429 ) ;
#118901 = LINE ( 'NONE', #19593, #76731 ) ;
#118902 = AXIS2_PLACEMENT_3D ( 'NONE', #101051, #135842, #134429 ) ;
#118903 = DIRECTION ( 'NONE',  ( -0.7071067811865486830, -0.7071067811865464625, 0.000000000000000000 ) ) ;
#118904 = ORIENTED_EDGE ( 'NONE', *, *, #108301, .T. ) ;
#118906 = ORIENTED_EDGE ( 'NONE', *, *, #42304, .F. ) ;
#118905 = LINE ( 'NONE', #8672, #120366 ) ;
#118907 = VERTEX_POINT ( 'NONE', #54721 ) ;
#118908 = ADVANCED_FACE ( 'NONE', ( #80063 ), #98901, .F. ) ;
#118909 = EDGE_CURVE ( 'NONE', #75489, #78485, #32988, .T. ) ;
#118910 = AXIS2_PLACEMENT_3D ( 'NONE', #56468, #55716, #88345 ) ;
#118911 = CARTESIAN_POINT ( 'NONE',  ( 16.49999999999988631, 21.43112307739196609, 4.000000000000000000 ) ) ;
#118912 = DIRECTION ( 'NONE',  ( -0.7071067811865487940, 0.7071067811865463515, 0.000000000000000000 ) ) ;
#118913 = EDGE_LOOP ( 'NONE', ( #26461, #119684, #26667, #103881 ) ) ;
#118914 = LINE ( 'NONE', #87008, #116042 ) ;
#118915 = EDGE_CURVE ( 'NONE', #130332, #124489, #82896, .T. ) ;
#118916 = EDGE_CURVE ( 'NONE', #20396, #78254, #65375, .T. ) ;
#118917 = CARTESIAN_POINT ( 'NONE',  ( -32.75830541574792676, 0.7592924766157104211, 14.37146558664990259 ) ) ;
#118919 = AXIS2_PLACEMENT_3D ( 'NONE', #13462, #125106, #90338 ) ;
#118918 = DIRECTION ( 'NONE',  ( -0.6830127018922180770, -0.6830127018922204085, -0.2588190451025213501 ) ) ;
#118920 = DIRECTION ( 'NONE',  ( -8.673617379884034239E-17, 1.000000000000000000, 0.000000000000000000 ) ) ;
#118921 = CARTESIAN_POINT ( 'NONE',  ( 0.1599999999999981992, -7.755134012341974525, -1.713328601965980580 ) ) ;
#118922 = EDGE_CURVE ( 'NONE', #93631, #68320, #94454, .T. ) ;
#118923 = DIRECTION ( 'NONE',  ( -0.7071067811865486830, -0.7071067811865464625, 0.000000000000000000 ) ) ;
#118924 = LINE ( 'NONE', #50122, #88769 ) ;
#118925 = FACE_OUTER_BOUND ( 'NONE', #52607, .T. ) ;
#118926 = PLANE ( 'NONE',  #62972 ) ;
#118927 = CARTESIAN_POINT ( 'NONE',  ( -11.67183060077638501, 2.259292476615694323, 4.000000000000000000 ) ) ;
#118928 = EDGE_CURVE ( 'NONE', #14639, #93058, #24917, .T. ) ;
#118929 = CARTESIAN_POINT ( 'NONE',  ( -15.48921356237309510, -27.52281430457066236, 5.000000000000000000 ) ) ;
#118930 = DIRECTION ( 'NONE',  ( -0.7071067811865486830, 0.7071067811865464625, 0.000000000000000000 ) ) ;
#118931 = VERTEX_POINT ( 'NONE', #81484 ) ;
#118932 = AXIS2_PLACEMENT_3D ( 'NONE', #32594, #100701, #76828 ) ;
#118933 = ORIENTED_EDGE ( 'NONE', *, *, #139906, .T. ) ;
#118934 = ORIENTED_EDGE ( 'NONE', *, *, #139529, .T. ) ;
#118936 = EDGE_CURVE ( 'NONE', #79481, #78193, #103192, .T. ) ;
#118935 = CARTESIAN_POINT ( 'NONE',  ( 108.6250000000000000, -7.950000000000000178, -4.867971026610729436E-16 ) ) ;
#118937 = EDGE_LOOP ( 'NONE', ( #58785, #102390, #39213, #120922 ) ) ;
#118938 = VERTEX_POINT ( 'NONE', #125685 ) ;
#118939 = ORIENTED_EDGE ( 'NONE', *, *, #44710, .T. ) ;
#118940 = LINE ( 'NONE', #10175, #142845 ) ;
#118941 = DIRECTION ( 'NONE',  ( 1.000000000000000000, -0.000000000000000000, -0.000000000000000000 ) ) ;
#118942 = ORIENTED_EDGE ( 'NONE', *, *, #109201, .F. ) ;
#118943 = LINE ( 'NONE', #22464, #87952 ) ;
#118944 = EDGE_CURVE ( 'NONE', #50064, #88923, #103885, .T. ) ;
#118945 = DIRECTION ( 'NONE',  ( -0.7071067811865487940, 0.7071067811865463515, 0.000000000000000000 ) ) ;
#118946 = CARTESIAN_POINT ( 'NONE',  ( 13.10966639810773948, 3.759292476615678336, 4.164048746910661514 ) ) ;
#118947 = CARTESIAN_POINT ( 'NONE',  ( 36.18398860626899705, 28.73617430169812437, 5.000000000000000000 ) ) ;
#118948 = CARTESIAN_POINT ( 'NONE',  ( 105.2920968585647756, -5.291415217122921177, 3.054999999999999272 ) ) ;
#118949 = VERTEX_POINT ( 'NONE', #48122 ) ;
#118950 = CARTESIAN_POINT ( 'NONE',  ( 25.00000000000000000, 2.143131898507868051E-16, -1.749999999999999778 ) ) ;
#118951 = CARTESIAN_POINT ( 'NONE',  ( -15.79076468313838433, 8.175634574663693144, 5.000000000000000000 ) ) ;
#118953 = EDGE_CURVE ( 'NONE', #126231, #65837, #137178, .T. ) ;
#118952 = CIRCLE ( 'NONE', #137497, 2.500000000000000444 ) ;
#118954 = DIRECTION ( 'NONE',  ( 0.3543493200069162685, -0.000000000000000000, -0.9351131265310288487 ) ) ;
#118955 = LINE ( 'NONE', #10878, #124069 ) ;
#118956 = FACE_OUTER_BOUND ( 'NONE', #86985, .T. ) ;
#118957 = CARTESIAN_POINT ( 'NONE',  ( -27.70710678118634362, -15.74070752338411694, 5.000000000000000000 ) ) ;
#118958 = VECTOR ( 'NONE', #15142, 999.9999999999998863 ) ;
#118959 = ORIENTED_EDGE ( 'NONE', *, *, #55023, .F. ) ;
#118960 = ORIENTED_EDGE ( 'NONE', *, *, #56005, .F. ) ;
#118961 = CARTESIAN_POINT ( 'NONE',  ( 28.56249999999999289, -5.819803920172572198, -5.819803920172573086 ) ) ;
#118962 = ORIENTED_EDGE ( 'NONE', *, *, #15723, .F. ) ;
#118963 = DIRECTION ( 'NONE',  ( 0.000000000000000000, -1.000000000000000000, 0.000000000000000000 ) ) ;
#118964 = EDGE_CURVE ( 'NONE', #48040, #59390, #92304, .T. ) ;
#118965 = CARTESIAN_POINT ( 'NONE',  ( 5.755190629914537226, 2.055000000000001048, 0.000000000000000000 ) ) ;
#118966 = LINE ( 'NONE', #97178, #20232 ) ;
#118967 = VECTOR ( 'NONE', #63983, 999.9999999999998863 ) ;
#118968 = LINE ( 'NONE', #19661, #111492 ) ;
#118969 = PLANE ( 'NONE',  #81383 ) ;
#118970 = SURFACE_STYLE_FILL_AREA ( #18199 ) ;
#118971 = EDGE_CURVE ( 'NONE', #115630, #46893, #5987, .T. ) ;
#118972 = CARTESIAN_POINT ( 'NONE',  ( 119.7870968585647802, 3.054999999999997495, 5.291415217122919401 ) ) ;
#118973 = VECTOR ( 'NONE', #100193, 1000.000000000000000 ) ;
#118974 = ORIENTED_EDGE ( 'NONE', *, *, #16835, .F. ) ;
#118975 = VECTOR ( 'NONE', #14681, 1000.000000000000000 ) ;
#118976 = EDGE_CURVE ( 'NONE', #68517, #131359, #91615, .T. ) ;
#118977 = CARTESIAN_POINT ( 'NONE',  ( 2.510786437626908008, -27.52281430457053446, 5.000000000000000000 ) ) ;
#118978 = ORIENTED_EDGE ( 'NONE', *, *, #72676, .F. ) ;
#118979 = CARTESIAN_POINT ( 'NONE',  ( 70.37086038379622721, 6.884901960086289741, -3.974999999999993427 ) ) ;
#118981 = ADVANCED_FACE ( 'NONE', ( #80759 ), #50265, .T. ) ;
#118980 = SURFACE_STYLE_USAGE ( .BOTH. , #40726 ) ;
#118983 = EDGE_CURVE ( 'NONE', #109290, #19069, #26365, .T. ) ;
#118982 = AXIS2_PLACEMENT_3D ( 'NONE', #48854, #106036, #139455 ) ;
#118984 = DIRECTION ( 'NONE',  ( 0.7071067811865486830, -0.7071067811865464625, -0.000000000000000000 ) ) ;
#118985 = VERTEX_POINT ( 'NONE', #135834 ) ;
#118986 = CARTESIAN_POINT ( 'NONE',  ( 46.08376352523143993, -6.110000000000001208, -3.741295971395164515E-16 ) ) ;
#118987 = AXIS2_PLACEMENT_3D ( 'NONE', #119748, #19039, #124073 ) ;
#118988 = ORIENTED_EDGE ( 'NONE', *, *, #94261, .F. ) ;
#118989 = LINE ( 'NONE', #76209, #61055 ) ;
#118990 = DIRECTION ( 'NONE',  ( 0.7071067811865486830, -0.7071067811865464625, -0.000000000000000000 ) ) ;
#118991 = CARTESIAN_POINT ( 'NONE',  ( -3.183988606268992161, 28.73617430169789699, 5.000000000000000000 ) ) ;
#118992 = VECTOR ( 'NONE', #134769, 1000.000000000000000 ) ;
#118993 = AXIS2_PLACEMENT_3D ( 'NONE', #7222, #52876, #50768 ) ;
#118994 = CARTESIAN_POINT ( 'NONE',  ( 39.28709685856478018, 3.054999999999997495, 5.291415217122919401 ) ) ;
#118995 = EDGE_LOOP ( 'NONE', ( #96164, #24908, #60577, #32986 ) ) ;
#118996 = EDGE_CURVE ( 'NONE', #44540, #52184, #113343, .T. ) ;
#118997 = LINE ( 'NONE', #42178, #101172 ) ;
#118998 = ORIENTED_EDGE ( 'NONE', *, *, #40600, .F. ) ;
#118999 = VERTEX_POINT ( 'NONE', #49573 ) ;
#119000 = VECTOR ( 'NONE', #97533, 1000.000000000000227 ) ;
#119001 = VERTEX_POINT ( 'NONE', #58330 ) ;
#119002 = DIRECTION ( 'NONE',  ( -0.7071067811865486830, -0.7071067811865464625, 0.000000000000000000 ) ) ;
#119003 = CARTESIAN_POINT ( 'NONE',  ( -23.29289321881329755, 17.25929247661554200, 5.000000000000000000 ) ) ;
#119004 = ADVANCED_FACE ( 'NONE', ( #61183 ), #59725, .T. ) ;
#119005 = ORIENTED_EDGE ( 'NONE', *, *, #46585, .F. ) ;
#119006 = LINE ( 'NONE', #19689, #140883 ) ;
#119007 = AXIS2_PLACEMENT_3D ( 'NONE', #102162, #93408, #38322 ) ;
#119008 = DIRECTION ( 'NONE',  ( 0.7071067811865486830, -0.7071067811865464625, -0.000000000000000000 ) ) ;
#119009 = PLANE ( 'NONE',  #18786 ) ;
#119010 = EDGE_CURVE ( 'NONE', #107846, #27577, #114761, .T. ) ;
#119011 = FACE_BOUND ( 'NONE', #39626, .T. ) ;
#119012 = VERTEX_POINT ( 'NONE', #102512 ) ;
#119013 = CARTESIAN_POINT ( 'NONE',  ( -10.82816939922345156, -5.240707523384225297, 4.000000000000000000 ) ) ;
#119014 = CARTESIAN_POINT ( 'NONE',  ( -25.49999999999982236, -2.173586137069152713, -4.605770156576171281 ) ) ;
#119015 = VERTEX_POINT ( 'NONE', #25629 ) ;
#119016 = PRESENTATION_STYLE_ASSIGNMENT (( #50925 ) ) ;
#119017 = ORIENTED_EDGE ( 'NONE', *, *, #79102, .F. ) ;
#119018 = ORIENTED_EDGE ( 'NONE', *, *, #136043, .T. ) ;
#119019 = DIRECTION ( 'NONE',  ( 0.6830127018922181881, 0.6830127018922202975, -0.2588190451025214056 ) ) ;
#119020 = VERTEX_POINT ( 'NONE', #38667 ) ;
#119021 = CARTESIAN_POINT ( 'NONE',  ( 54.30793019189810877, -6.109999999999998543, 1.637169565754158507 ) ) ;
#119023 = ORIENTED_EDGE ( 'NONE', *, *, #40458, .T. ) ;
#119022 = VECTOR ( 'NONE', #122435, 1000.000000000000000 ) ;
#119024 = LINE ( 'NONE', #132068, #51115 ) ;
#119025 = LINE ( 'NONE', #29168, #26432 ) ;
#119026 = VERTEX_POINT ( 'NONE', #82202 ) ;
#119027 = CARTESIAN_POINT ( 'NONE',  ( 6.707106781186505273, 20.25929247661551713, 5.000000000000000000 ) ) ;
#119028 = LINE ( 'NONE', #19713, #73591 ) ;
#119030 = EDGE_CURVE ( 'NONE', #56450, #92514, #69906, .T. ) ;
#119029 = VECTOR ( 'NONE', #37931, 1000.000000000000000 ) ;
#119031 = ADVANCED_FACE ( 'NONE', ( #139442 ), #108875, .F. ) ;
#119032 = CARTESIAN_POINT ( 'NONE',  ( 65.99451991528749772, 28.92564299267984396, 4.000000000000000000 ) ) ;
#119033 = CARTESIAN_POINT ( 'NONE',  ( -34.92500000000001137, -5.337538124160958297, 4.000000000000000000 ) ) ;
#119034 = CARTESIAN_POINT ( 'NONE',  ( -30.29974487139158867, -27.71228299555227537, 4.000000000000000000 ) ) ;
#119035 = DIRECTION ( 'NONE',  ( 1.451651444332056451E-15, 1.000000000000000000, -0.000000000000000000 ) ) ;
#119036 = CARTESIAN_POINT ( 'NONE',  ( -12.32816939922343913, -18.74070752338409207, 4.000000000000000000 ) ) ;
#119037 = VERTEX_POINT ( 'NONE', #74149 ) ;
#119038 = ORIENTED_EDGE ( 'NONE', *, *, #64001, .T. ) ;
#119039 = CARTESIAN_POINT ( 'NONE',  ( 32.99999999999976552, -22.22500000000000142, 4.412002311790011788 ) ) ;
#119040 = FACE_OUTER_BOUND ( 'NONE', #103368, .T. ) ;
#119041 = EDGE_LOOP ( 'NONE', ( #132434, #53257, #55702, #91269 ) ) ;
#119042 = EDGE_LOOP ( 'NONE', ( #69902, #92085, #121566, #85831 ) ) ;
#119043 = ORIENTED_EDGE ( 'NONE', *, *, #56233, .F. ) ;
#119044 = LINE ( 'NONE', #108142, #5005 ) ;
#119045 = CARTESIAN_POINT ( 'NONE',  ( -57.48921356237308800, -27.52281430457095368, 5.000000000000000000 ) ) ;
#119046 = EDGE_CURVE ( 'NONE', #17549, #64706, #53083, .T. ) ;
#119047 = CARTESIAN_POINT ( 'NONE',  ( 19.05000000000000071, 3.174999999999997158, 4.000000000000000000 ) ) ;
#119048 = ORIENTED_EDGE ( 'NONE', *, *, #82878, .F. ) ;
#119049 = DIRECTION ( 'NONE',  ( -0.7071067811865486830, -0.7071067811865464625, 0.000000000000000000 ) ) ;
#119050 = VECTOR ( 'NONE', #92444, 1000.000000000000000 ) ;
#119051 = PLANE ( 'NONE',  #2930 ) ;
#119052 = AXIS2_PLACEMENT_3D ( 'NONE', #102734, #81718, #47673 ) ;
#119053 = CARTESIAN_POINT ( 'NONE',  ( 21.35873647476855552, 5.808823158059031044, -5.808823158059038150 ) ) ;
#119054 = ORIENTED_EDGE ( 'NONE', *, *, #6273, .T. ) ;
#119055 = CARTESIAN_POINT ( 'NONE',  ( 119.7870968585647802, 3.054999999999997939, 5.291415217122920289 ) ) ;
#119056 = CIRCLE ( 'NONE', #8207, 2.500000000000000888 ) ;
#119057 = LINE ( 'NONE', #53834, #136854 ) ;
#119058 = LINE ( 'NONE', #19749, #95904 ) ;
#119060 = VERTEX_POINT ( 'NONE', #63309 ) ;
#119059 = CARTESIAN_POINT ( 'NONE',  ( -12.00548008471251293, 28.92564299267929684, 4.000000000000000000 ) ) ;
#119061 = PLANE ( 'NONE',  #143475 ) ;
#119062 = ORIENTED_EDGE ( 'NONE', *, *, #2026, .T. ) ;
#119063 = CARTESIAN_POINT ( 'NONE',  ( 75.91252705046288440, -7.949999999999998401, -4.867971026610728450E-16 ) ) ;
#119064 = CARTESIAN_POINT ( 'NONE',  ( -21.31657961132776435, -6.740707523384205757, 11.88629033278129477 ) ) ;
#119065 = CARTESIAN_POINT ( 'NONE',  ( 0.000000000000000000, 0.000000000000000000, 5.000000000000000000 ) ) ;
#119066 = ORIENTED_EDGE ( 'NONE', *, *, #5053, .T. ) ;
#119067 = AXIS2_PLACEMENT_3D ( 'NONE', #35506, #71669, #136196 ) ;
#119068 = FACE_OUTER_BOUND ( 'NONE', #34963, .T. ) ;
#119069 = CARTESIAN_POINT ( 'NONE',  ( -4.499999999999965361, -16.91253812416058722, 4.000000000000000000 ) ) ;
#119070 = VERTEX_POINT ( 'NONE', #97279 ) ;
#119071 = FACE_OUTER_BOUND ( 'NONE', #126418, .T. ) ;
#119072 = LINE ( 'NONE', #106034, #120994 ) ;
#119073 = ORIENTED_EDGE ( 'NONE', *, *, #45056, .F. ) ;
#119074 = LINE ( 'NONE', #53857, #31039 ) ;
#119075 = DIRECTION ( 'NONE',  ( -0.000000000000000000, 0.3543493200069153248, 0.9351131265310292928 ) ) ;
#119076 = VECTOR ( 'NONE', #25096, 1000.000000000000000 ) ;
#119077 = ORIENTED_EDGE ( 'NONE', *, *, #119931, .T. ) ;
#119078 = EDGE_CURVE ( 'NONE', #109323, #81745, #140136, .T. ) ;
#119079 = EDGE_LOOP ( 'NONE', ( #135115, #107574, #76904, #54528 ) ) ;
#119080 = CARTESIAN_POINT ( 'NONE',  ( -26.99999999999980105, 17.96639925780208102, 5.000000000000000000 ) ) ;
#119081 = PLANE ( 'NONE',  #129324 ) ;
#119082 = AXIS2_PLACEMENT_3D ( 'NONE', #113892, #14580, #39196 ) ;
#119083 = CARTESIAN_POINT ( 'NONE',  ( 13.24956980810188689, 3.967499999999998916, 6.871911579029510442 ) ) ;
#119084 = DIRECTION ( 'NONE',  ( -1.000000000000000000, -0.000000000000000000, -0.000000000000000000 ) ) ;
#119085 = EDGE_CURVE ( 'NONE', #136430, #61441, #30660, .T. ) ;
#119086 = EDGE_CURVE ( 'NONE', #80231, #143132, #40125, .T. ) ;
#119087 = VECTOR ( 'NONE', #98215, 1000.000000000000000 ) ;
#119088 = STYLED_ITEM ( 'NONE', ( #1028 ), #120045 ) ;
#119089 = CARTESIAN_POINT ( 'NONE',  ( -34.92500000000001137, 22.22500000000000142, 4.000000000000000000 ) ) ;
#119090 = CARTESIAN_POINT ( 'NONE',  ( 29.99451991528749417, 28.92564299267958816, 4.000000000000000000 ) ) ;
#119091 = EDGE_CURVE ( 'NONE', #138500, #95435, #18297, .T. ) ;
#119092 = ORIENTED_EDGE ( 'NONE', *, *, #76575, .T. ) ;
#119093 = PRESENTATION_STYLE_ASSIGNMENT (( #74917 ) ) ;
#119094 = ADVANCED_FACE ( 'NONE', ( #142279 ), #8142, .F. ) ;
#119095 = CARTESIAN_POINT ( 'NONE',  ( 31.49999999999977973, 12.43112307739205669, 4.000000000000000000 ) ) ;
#119096 = LINE ( 'NONE', #72804, #102632 ) ;
#119097 = CARTESIAN_POINT ( 'NONE',  ( 126.7587378609811282, -5.618906549250023197, -3.646044159374574711 ) ) ;
#119098 = EDGE_CURVE ( 'NONE', #112107, #111218, #7432, .T. ) ;
#119099 = CARTESIAN_POINT ( 'NONE',  ( 35.05793019189811588, 6.110000000000001208, -1.637169565754156286 ) ) ;
#119100 = AXIS2_PLACEMENT_3D ( 'NONE', #106162, #139577, #107613 ) ;
#119101 = ORIENTED_EDGE ( 'NONE', *, *, #29370, .T. ) ;
#119103 = ADVANCED_FACE ( 'NONE', ( #141550 ), #50972, .T. ) ;
#119102 = DIRECTION ( 'NONE',  ( 0.3543493200069163240, 0.000000000000000000, -0.9351131265310288487 ) ) ;
#119104 = VERTEX_POINT ( 'NONE', #61865 ) ;
#119105 = EDGE_CURVE ( 'NONE', #65901, #104855, #84340, .T. ) ;
#119106 = ORIENTED_EDGE ( 'NONE', *, *, #106433, .T. ) ;
#119107 = DIRECTION ( 'NONE',  ( 0.000000000000000000, -1.000000000000000000, 0.000000000000000000 ) ) ;
#119108 = DIRECTION ( 'NONE',  ( 0.7071067811865487940, 0.7071067811865463515, -0.000000000000000000 ) ) ;
#119109 = EDGE_LOOP ( 'NONE', ( #61005, #61134, #134944, #5484, #122267 ) ) ;
#119110 =( LENGTH_UNIT ( ) NAMED_UNIT ( * ) SI_UNIT ( .MILLI., .METRE. ) );
#119111 = DIRECTION ( 'NONE',  ( -0.7071067811865486830, -0.7071067811865464625, 0.000000000000000000 ) ) ;
#119112 = EDGE_CURVE ( 'NONE', #85199, #55981, #106747, .T. ) ;
#119113 = DIRECTION ( 'NONE',  ( -0.7071067811865487940, 0.7071067811865463515, 0.000000000000000000 ) ) ;
#119114 = ADVANCED_FACE ( 'NONE', ( #6695 ), #85714, .T. ) ;
#119115 = PLANE ( 'NONE',  #39582 ) ;
#119116 = DIRECTION ( 'NONE',  ( -1.000000000000000000, -1.224606353822377258E-16, -0.000000000000000000 ) ) ;
#119117 = ORIENTED_EDGE ( 'NONE', *, *, #15404, .T. ) ;
#119118 = CARTESIAN_POINT ( 'NONE',  ( 3.183988606268992161, 28.73617430169789699, 5.000000000000000000 ) ) ;
#119119 = LINE ( 'NONE', #116976, #37633 ) ;
#119120 = CARTESIAN_POINT ( 'NONE',  ( 20.99065804761471199, -2.500000000000000000, 3.061616997868383634E-16 ) ) ;
#119121 = CARTESIAN_POINT ( 'NONE',  ( 0.000000000000000000, 0.000000000000000000, 0.000000000000000000 ) ) ;
#119122 = CARTESIAN_POINT ( 'NONE',  ( 10.82816939922345156, -17.24070752338410628, 4.000000000000000000 ) ) ;
#119123 = ADVANCED_FACE ( 'NONE', ( #128536 ), #73444, .T. ) ;
#119124 = CARTESIAN_POINT ( 'NONE',  ( 18.48921356237309510, -27.52281430457068367, 5.000000000000000000 ) ) ;
#119125 = CARTESIAN_POINT ( 'NONE',  ( 57.68336038379621300, -2.130196079827426203, 7.949999999999997513 ) ) ;
#119126 = FACE_OUTER_BOUND ( 'NONE', #110739, .T. ) ;
#119127 = ORIENTED_EDGE ( 'NONE', *, *, #20349, .T. ) ;
#119128 = ORIENTED_EDGE ( 'NONE', *, *, #74603, .T. ) ;
#119129 = CARTESIAN_POINT ( 'NONE',  ( 51.02083333333332860, 7.949999999999999289, 2.130196079827431532 ) ) ;
#119130 = CARTESIAN_POINT ( 'NONE',  ( -14.70025512860841133, -27.71228299555195917, 4.000000000000000000 ) ) ;
#119131 = CARTESIAN_POINT ( 'NONE',  ( -36.31657961132766843, -6.740707523384205757, 11.88629033278132852 ) ) ;
#119132 = ORIENTED_EDGE ( 'NONE', *, *, #96612, .T. ) ;
#119133 = VECTOR ( 'NONE', #95672, 1000.000000000000000 ) ;
#119134 = DIRECTION ( 'NONE',  ( 0.000000000000000000, -1.000000000000000000, 0.000000000000000000 ) ) ;
#119135 = CARTESIAN_POINT ( 'NONE',  ( 44.47959685856476852, 6.109999999999999432, 1.637169565754164280 ) ) ;
#119136 = ORIENTED_EDGE ( 'NONE', *, *, #57741, .T. ) ;
#119137 = EDGE_CURVE ( 'NONE', #139318, #18266, #108160, .T. ) ;
#119138 = CARTESIAN_POINT ( 'NONE',  ( 7.251592354503322291, 9.902892378096218942E-16, 0.000000000000000000 ) ) ;
#119139 = ORIENTED_EDGE ( 'NONE', *, *, #1643, .T. ) ;
#119140 = ORIENTED_EDGE ( 'NONE', *, *, #20367, .F. ) ;
#119141 = LINE ( 'NONE', #75660, #9899 ) ;
#119142 = CARTESIAN_POINT ( 'NONE',  ( 81.60002705046291283, 5.819803920172570422, 5.819803920172575751 ) ) ;
#119143 = CARTESIAN_POINT ( 'NONE',  ( 156.1500000000000057, -57.14999999999999147, 53.92499999999997584 ) ) ;
#119144 = CARTESIAN_POINT ( 'NONE',  ( -23.99999999999982592, 7.552185695429090906, 5.000000000000000000 ) ) ;
#119145 = ORIENTED_EDGE ( 'NONE', *, *, #122379, .F. ) ;
#119146 = FACE_OUTER_BOUND ( 'NONE', #96637, .T. ) ;
#119148 = EDGE_LOOP ( 'NONE', ( #84829, #134144, #75915, #50841 ) ) ;
#119147 = CARTESIAN_POINT ( 'NONE',  ( 4.499999999999972466, 16.46639925780209524, 5.000000000000000000 ) ) ;
#119149 = CARTESIAN_POINT ( 'NONE',  ( 79.91709685856476142, 3.054999999999998828, 5.291415217122922066 ) ) ;
#119150 = DIRECTION ( 'NONE',  ( 0.3543493200069162685, -0.000000000000000000, -0.9351131265310288487 ) ) ;
#119151 = DIRECTION ( 'NONE',  ( -0.6830127018922181881, 0.6830127018922202975, -0.2588190451025214056 ) ) ;
#119152 = VECTOR ( 'NONE', #66285, 1000.000000000000000 ) ;
#119153 = DIRECTION ( 'NONE',  ( -0.000000000000000000, 0.3543493200069153248, 0.9351131265310292928 ) ) ;
#119154 = EDGE_CURVE ( 'NONE', #95030, #125982, #29908, .T. ) ;
#119155 = AXIS2_PLACEMENT_3D ( 'NONE', #24637, #136977, #105051 ) ;
#119156 = ORIENTED_EDGE ( 'NONE', *, *, #117790, .T. ) ;
#119157 =( BOUNDED_CURVE ( )  B_SPLINE_CURVE ( 3, ( #80331, #4096, #114352, #124519 ),
 .UNSPECIFIED., .F., .T. ) 
 B_SPLINE_CURVE_WITH_KNOTS ( ( 4, 4 ),
 ( 4.517163242187656635, 4.562733109340372906 ),
 .UNSPECIFIED. ) 
 CURVE ( )  GEOMETRIC_REPRESENTATION_ITEM ( )  RATIONAL_B_SPLINE_CURVE ( ( 1.000000000000000000, 0.9998269564205118920, 0.9998269564205118920, 1.000000000000000000 ) ) 
 REPRESENTATION_ITEM ( '' )  );
#119158 = DIRECTION ( 'NONE',  ( 0.000000000000000000, -1.000000000000000000, 0.000000000000000000 ) ) ;
#119159 = CARTESIAN_POINT ( 'NONE',  ( 65.24543019189810877, -5.291415217122918513, -3.055000000000000160 ) ) ;
#119160 = AXIS2_PLACEMENT_3D ( 'NONE', #93100, #93807, #25690 ) ;
#119161 = FACE_OUTER_BOUND ( 'NONE', #138517, .T. ) ;
#119162 = ADVANCED_FACE ( 'NONE', ( #118343 ), #104866, .T. ) ;
#119163 = CARTESIAN_POINT ( 'NONE',  ( -41.99451991528749062, 28.92564299267967343, 4.000000000000000000 ) ) ;
#119164 = CARTESIAN_POINT ( 'NONE',  ( -27.70710678118635073, 20.25929247661551003, 5.000000000000000000 ) ) ;
#119165 = EDGE_LOOP ( 'NONE', ( #102130, #47072, #56888, #53734 ) ) ;
#119166 = ORIENTED_EDGE ( 'NONE', *, *, #66692, .F. ) ;
#119167 = LINE ( 'NONE', #12546, #104820 ) ;
#119168 = ORIENTED_EDGE ( 'NONE', *, *, #32369, .T. ) ;
#119169 = VERTEX_POINT ( 'NONE', #41503 ) ;
#119170 =( GEOMETRIC_REPRESENTATION_CONTEXT ( 3 ) GLOBAL_UNCERTAINTY_ASSIGNED_CONTEXT ( ( #38718 ) ) GLOBAL_UNIT_ASSIGNED_CONTEXT ( ( #75788, #93614, #38516 ) ) REPRESENTATION_CONTEXT ( 'NONE', 'WORKASPACE' ) );
#119171 = ADVANCED_FACE ( 'NONE', ( #34217 ), #101592, .F. ) ;
#119172 = CARTESIAN_POINT ( 'NONE',  ( 0.000000000000000000, 0.000000000000000000, 7.950000000000000178 ) ) ;
#119173 = ORIENTED_EDGE ( 'NONE', *, *, #125210, .F. ) ;
#119174 = PLANE ( 'NONE',  #93172 ) ;
#119175 = DIRECTION ( 'NONE',  ( -0.7071067811865486830, -0.7071067811865464625, 0.000000000000000000 ) ) ;
#119176 = CARTESIAN_POINT ( 'NONE',  ( -34.49999999999976552, -14.94567065516890558, 4.994342998332162331 ) ) ;
#119177 = ADVANCED_FACE ( 'NONE', ( #111776 ), #110311, .F. ) ;
#119178 = FACE_BOUND ( 'NONE', #42837, .T. ) ;
#119179 = PLANE ( 'NONE',  #128874 ) ;
#119180 = DIRECTION ( 'NONE',  ( 0.7071067811865487940, 0.7071067811865463515, 0.000000000000000000 ) ) ;
#119181 = DIRECTION ( 'NONE',  ( -0.6830127018922180770, -0.6830127018922204085, -0.2588190451025213501 ) ) ;
#119183 = ORIENTED_EDGE ( 'NONE', *, *, #81942, .T. ) ;
#119182 = CARTESIAN_POINT ( 'NONE',  ( 32.99999999999977973, 5.587461875839189851, 4.000000000000000000 ) ) ;
#119184 = CARTESIAN_POINT ( 'NONE',  ( -27.29974487139158512, -27.71228299555225405, 4.000000000000000000 ) ) ;
#119185 = VECTOR ( 'NONE', #120727, 1000.000000000000000 ) ;
#119186 = ORIENTED_EDGE ( 'NONE', *, *, #69978, .F. ) ;
#119187 = VECTOR ( 'NONE', #7431, 999.9999999999998863 ) ;
#119189 = VERTEX_POINT ( 'NONE', #100192 ) ;
#119188 = VECTOR ( 'NONE', #6307, 1000.000000000000000 ) ;
#119190 = CARTESIAN_POINT ( 'NONE',  ( 89.30793019189810877, -6.109999999999998543, 1.637169565754158507 ) ) ;
#119191 = VERTEX_POINT ( 'NONE', #11704 ) ;
#119192 = AXIS2_PLACEMENT_3D ( 'NONE', #25221, #91908, #47055 ) ;
#119193 = LINE ( 'NONE', #108284, #32798 ) ;
#119194 = ORIENTED_EDGE ( 'NONE', *, *, #63217, .F. ) ;
#119195 = LINE ( 'NONE', #19878, #83856 ) ;
#119196 = CARTESIAN_POINT ( 'NONE',  ( -15.46160355370562023, -9.740707523384180888, 17.74957260769607359 ) ) ;
#119197 = DIRECTION ( 'NONE',  ( -0.7071067811865486830, -0.7071067811865464625, -0.000000000000000000 ) ) ;
#119198 = EDGE_CURVE ( 'NONE', #68141, #33799, #77968, .T. ) ;
#119199 = DIRECTION ( 'NONE',  ( 0.7071067811865486830, -0.7071067811865464625, -0.000000000000000000 ) ) ;
#119200 = CARTESIAN_POINT ( 'NONE',  ( 26.75159235450331963, 2.500000000000001332, 0.000000000000000000 ) ) ;
#119201 = DIRECTION ( 'NONE',  ( -0.000000000000000000, 0.3543493200069153248, 0.9351131265310292928 ) ) ;
#119202 = CARTESIAN_POINT ( 'NONE',  ( -34.92500000000001137, 17.56110451772267211, 6.767324343803291953 ) ) ;
#119203 = CARTESIAN_POINT ( 'NONE',  ( -6.813775866939250747, -22.22500000000000142, -5.652393676757531793 ) ) ;
#119204 = VERTEX_POINT ( 'NONE', #10297 ) ;
#119205 = SURFACE_SIDE_STYLE ('',( #40948 ) ) ;
#119206 = VERTEX_POINT ( 'NONE', #134247 ) ;
#119207 = CARTESIAN_POINT ( 'NONE',  ( 123.0166937171295416, 7.950000000000000178, -2.130196079827421318 ) ) ;
#119208 = DIRECTION ( 'NONE',  ( -0.7071067811865486830, -0.7071067811865464625, 0.000000000000000000 ) ) ;
#119209 = ORIENTED_EDGE ( 'NONE', *, *, #16279, .F. ) ;
#119210 = ORIENTED_EDGE ( 'NONE', *, *, #131035, .T. ) ;
#119211 = EDGE_CURVE ( 'NONE', #65878, #48062, #21895, .T. ) ;
#119212 = ORIENTED_EDGE ( 'NONE', *, *, #80969, .F. ) ;
#119213 = CARTESIAN_POINT ( 'NONE',  ( 34.70876352523143282, -7.482591942790329030E-16, 6.110000000000001208 ) ) ;
#119214 = ORIENTED_EDGE ( 'NONE', *, *, #100271, .T. ) ;
#119215 = CARTESIAN_POINT ( 'NONE',  ( 13.18000000000000149, 9.521314400968980422E-16, 0.000000000000000000 ) ) ;
#119216 =( BOUNDED_CURVE ( )  B_SPLINE_CURVE ( 2, ( #23861, #65966, #1354, #110125, #101403, #21711, #2799, #57949, #66653, #89126, #44946, #12950, #133343 ),
 .UNSPECIFIED., .F., .T. ) 
 B_SPLINE_CURVE_WITH_KNOTS ( ( 3, 2, 2, 2, 2, 2, 3 ),
 ( 0.4500000000000000111, 0.4583333333333333148, 0.4666666666666666741, 0.4749999999999999778, 0.4833333333333333370, 0.4916666666666666408, 0.5000000000000000000 ),
 .UNSPECIFIED. ) 
 CURVE ( )  GEOMETRIC_REPRESENTATION_ITEM ( )  RATIONAL_B_SPLINE_CURVE ( ( 1.000000000000000000, 0.9659258262890683122, 1.000000000000000000, 0.9659258262890683122, 1.000000000000000000, 0.9659258262890683122, 1.000000000000000000, 0.9659258262890683122, 1.000000000000000000, 0.9659258262890683122, 1.000000000000000000, 0.9659258262890683122, 1.000000000000000000 ) ) 
 REPRESENTATION_ITEM ( '' )  );
#119217 = CARTESIAN_POINT ( 'NONE',  ( 22.35830628287044064, -1.633150327867689988, 6.094999999999989981 ) ) ;
#119218 = CARTESIAN_POINT ( 'NONE',  ( 0.4979396410360854008, 13.74659983411467756, -24.36742386311884090 ) ) ;
#119219 = ORIENTED_EDGE ( 'NONE', *, *, #21804, .F. ) ;
#119220 = DIRECTION ( 'NONE',  ( -0.7071067811865486830, -0.7071067811865464625, 0.000000000000000000 ) ) ;
#119221 = ORIENTED_EDGE ( 'NONE', *, *, #55667, .T. ) ;
#119222 = FACE_OUTER_BOUND ( 'NONE', #20083, .T. ) ;
#119223 = CARTESIAN_POINT ( 'NONE',  ( 32.34328999833767426, 3.759292476615685441, 13.27625715073272872 ) ) ;
#119225 = ORIENTED_EDGE ( 'NONE', *, *, #114206, .T. ) ;
#119224 = FACE_OUTER_BOUND ( 'NONE', #134063, .T. ) ;
#119226 = EDGE_LOOP ( 'NONE', ( #16458, #119626, #77370, #34912 ) ) ;
#119227 = EDGE_CURVE ( 'NONE', #80329, #121162, #99437, .T. ) ;
#119228 = FACE_OUTER_BOUND ( 'NONE', #23367, .T. ) ;
#119229 = CARTESIAN_POINT ( 'NONE',  ( 0.000000000000000000, 0.000000000000000000, 5.000000000000000000 ) ) ;
#119230 = ORIENTED_EDGE ( 'NONE', *, *, #135478, .F. ) ;
#119231 = DIRECTION ( 'NONE',  ( -0.3543493200069162685, -0.000000000000000000, -0.9351131265310288487 ) ) ;
#119232 = EDGE_LOOP ( 'NONE', ( #48114, #94235, #57357, #53588 ) ) ;
#119233 = EDGE_LOOP ( 'NONE', ( #121131, #26431, #100209, #126253 ) ) ;
#119234 = ORIENTED_EDGE ( 'NONE', *, *, #42840, .F. ) ;
#119235 = CARTESIAN_POINT ( 'NONE',  ( -9.005480084712511157, 28.92564299267931816, 4.000000000000000000 ) ) ;
#119236 = DIRECTION ( 'NONE',  ( -0.7071067811865486830, 0.7071067811865464625, 0.000000000000000000 ) ) ;
#119237 = CARTESIAN_POINT ( 'NONE',  ( 14.11162361894749395, 9.759292476615607725, 17.35367589129209520 ) ) ;
#119238 = DIRECTION ( 'NONE',  ( -0.7071067811865487940, 0.7071067811865463515, 0.000000000000000000 ) ) ;
#119239 = DIRECTION ( 'NONE',  ( 0.7071067811865486830, -0.7071067811865464625, -0.000000000000000000 ) ) ;
#119240 = CARTESIAN_POINT ( 'NONE',  ( -39.18398860626899705, 28.73617430169814568, 5.000000000000000000 ) ) ;
#119241 = EDGE_LOOP ( 'NONE', ( #31234, #73395, #60110, #75565, #143550 ) ) ;
#119242 = DIRECTION ( 'NONE',  ( -1.000000000000000000, -1.224606353822377258E-16, -0.000000000000000000 ) ) ;
#119243 = ORIENTED_EDGE ( 'NONE', *, *, #121312, .T. ) ;
#119244 = DIRECTION ( 'NONE',  ( -0.000000000000000000, -0.3543493200069152693, 0.9351131265310292928 ) ) ;
#119245 = VECTOR ( 'NONE', #72310, 1000.000000000000000 ) ;
#119246 = LINE ( 'NONE', #75778, #126954 ) ;
#119247 = ADVANCED_FACE ( 'NONE', ( #78436 ), #98733, .T. ) ;
#119248 = VERTEX_POINT ( 'NONE', #56725 ) ;
#119249 = CARTESIAN_POINT ( 'NONE',  ( -25.49999999999982592, 3.653845994658372121, -4.504631822206310865 ) ) ;
#119250 = DIRECTION ( 'NONE',  ( 0.7071067811865487940, 0.7071067811865463515, 0.000000000000000000 ) ) ;
#119251 = ORIENTED_EDGE ( 'NONE', *, *, #126994, .T. ) ;
#119252 = ADVANCED_FACE ( 'NONE', ( #68311 ), #142962, .F. ) ;
#119253 = AXIS2_PLACEMENT_3D ( 'NONE', #103095, #81369, #35737 ) ;
#119254 = VERTEX_POINT ( 'NONE', #34941 ) ;
#119255 = CARTESIAN_POINT ( 'NONE',  ( -11.70025512860841133, -27.71228299555198049, 4.000000000000000000 ) ) ;
#119256 = ADVANCED_FACE ( 'NONE', ( #132113 ), #79182, .F. ) ;
#119257 = DIRECTION ( 'NONE',  ( -1.000000000000000000, -0.000000000000000000, -0.000000000000000000 ) ) ;
#119258 = CARTESIAN_POINT ( 'NONE',  ( -34.45011844616455221, -17.99769585840585862, 5.000000000000000888 ) ) ;
#119259 = CARTESIAN_POINT ( 'NONE',  ( 0.4812208760386733064, -49.11951764990739377, -40.13200514437903621 ) ) ;
#119260 = EDGE_CURVE ( 'NONE', #126683, #73943, #132839, .T. ) ;
#119261 = CARTESIAN_POINT ( 'NONE',  ( 63.64126352523144448, 4.472830434245837594, 4.472830434245841147 ) ) ;
#119262 = CARTESIAN_POINT ( 'NONE',  ( -31.92499999999997584, -3.270000000000012452, -36.39086428169088094 ) ) ;
#119263 = PRESENTATION_STYLE_ASSIGNMENT (( #63513 ) ) ;
#119264 = AXIS2_PLACEMENT_3D ( 'NONE', #694, #44244, #10844 ) ;
#119265 = DIRECTION ( 'NONE',  ( -0.7071067811865487940, 0.7071067811865463515, 0.000000000000000000 ) ) ;
#119266 = DIRECTION ( 'NONE',  ( 0.7071067811865487940, 0.7071067811865463515, -0.000000000000000000 ) ) ;
#119267 = ORIENTED_EDGE ( 'NONE', *, *, #46508, .T. ) ;
#119268 = LINE ( 'NONE', #62787, #58072 ) ;
#119269 = EDGE_LOOP ( 'NONE', ( #47761, #84425, #75206, #63570 ) ) ;
#119270 = CARTESIAN_POINT ( 'NONE',  ( 0.000000000000000000, 0.000000000000000000, 5.000000000000000000 ) ) ;
#119271 = DIRECTION ( 'NONE',  ( -0.7071067811865486830, -0.7071067811865464625, 0.000000000000000000 ) ) ;
#119272 = ORIENTED_EDGE ( 'NONE', *, *, #126142, .T. ) ;
#119273 = DIRECTION ( 'NONE',  ( -1.000000000000000000, -1.224606353822377258E-16, -0.000000000000000000 ) ) ;
#119275 = ORIENTED_EDGE ( 'NONE', *, *, #4059, .T. ) ;
#119274 = DIRECTION ( 'NONE',  ( -0.7071067811865486830, -0.7071067811865464625, 0.000000000000000000 ) ) ;
#119276 = ADVANCED_FACE ( 'NONE', ( #66844 ), #33527, .F. ) ;
#119277 = CARTESIAN_POINT ( 'NONE',  ( 106.4374999999999858, 5.819803920172574863, -5.819803920172573086 ) ) ;
#119278 = EDGE_CURVE ( 'NONE', #115116, #59322, #32807, .T. ) ;
#119279 = DIRECTION ( 'NONE',  ( 0.6830127018922180770, -0.6830127018922204085, -0.2588190451025213501 ) ) ;
#119280 = CARTESIAN_POINT ( 'NONE',  ( -15.70710678118643422, 17.25929247661554200, 5.000000000000000000 ) ) ;
#119281 = ORIENTED_EDGE ( 'NONE', *, *, #35205, .T. ) ;
#119282 = ORIENTED_EDGE ( 'NONE', *, *, #7969, .F. ) ;
#119283 = DIRECTION ( 'NONE',  ( 0.7071067811865486830, -0.7071067811865464625, -0.000000000000000000 ) ) ;
#119284 = CARTESIAN_POINT ( 'NONE',  ( 21.18398860626899349, 28.73617430169802134, 5.000000000000000000 ) ) ;
#119285 = CARTESIAN_POINT ( 'NONE',  ( -24.18398860626899705, 28.73617430169804265, 5.000000000000000000 ) ) ;
#119286 = EDGE_CURVE ( 'NONE', #125583, #25180, #131387, .T. ) ;
#119287 = VECTOR ( 'NONE', #94871, 1000.000000000000000 ) ;
#119288 = CARTESIAN_POINT ( 'NONE',  ( 88.74586038379622721, 3.974999999999996980, 6.884901960086287964 ) ) ;
#119290 = AXIS2_PLACEMENT_3D ( 'NONE', #4703, #84492, #17077 ) ;
#119289 = CARTESIAN_POINT ( 'NONE',  ( 0.4892135623730947680, -27.52281430457055578, 5.000000000000000000 ) ) ;
#119291 = VECTOR ( 'NONE', #22133, 999.9999999999998863 ) ;
#119292 = DIRECTION ( 'NONE',  ( 0.6830127018922181881, 0.6830127018922202975, -0.2588190451025214056 ) ) ;
#119293 = EDGE_LOOP ( 'NONE', ( #54042, #32322, #94723 ) ) ;
#119294 = VECTOR ( 'NONE', #29565, 1000.000000000000000 ) ;
#119295 = LINE ( 'NONE', #85238, #83963 ) ;
#119296 = CARTESIAN_POINT ( 'NONE',  ( 24.75860074219779605, 21.72500000000000853, 5.000000000000000000 ) ) ;
#119297 = EDGE_CURVE ( 'NONE', #95628, #141405, #21184, .T. ) ;
#119298 = ORIENTED_EDGE ( 'NONE', *, *, #33839, .T. ) ;
#119299 = DIRECTION ( 'NONE',  ( -0.6830127018922181881, 0.6830127018922202975, -0.2588190451025214056 ) ) ;
#119300 = ORIENTED_EDGE ( 'NONE', *, *, #14651, .T. ) ;
#119301 = CARTESIAN_POINT ( 'NONE',  ( 73.35459685856476142, -1.637169565754161615, 6.110000000000000320 ) ) ;
#119302 = DIRECTION ( 'NONE',  ( 0.000000000000000000, 1.541976423090494844E-15, 1.000000000000000000 ) ) ;
#119303 = EDGE_CURVE ( 'NONE', #41681, #14410, #109618, .T. ) ;
#119304 = DIRECTION ( 'NONE',  ( 0.000000000000000000, 1.016133275908817741E-16, -1.000000000000000000 ) ) ;
#119305 = ORIENTED_EDGE ( 'NONE', *, *, #33371, .F. ) ;
#119306 = CARTESIAN_POINT ( 'NONE',  ( 17.29289321881334018, -9.740707523384179112, 5.000000000000000000 ) ) ;
#119307 = CARTESIAN_POINT ( 'NONE',  ( -75.48921356237309510, -27.52281430457107803, 5.000000000000000000 ) ) ;
#119308 = CARTESIAN_POINT ( 'NONE',  ( 25.49999999999983658, -17.94781430457063820, 5.000000000000000000 ) ) ;
#119309 = DIRECTION ( 'NONE',  ( -1.000000000000000000, -0.000000000000000000, -0.000000000000000000 ) ) ;
#119311 = VERTEX_POINT ( 'NONE', #121904 ) ;
#119310 = CARTESIAN_POINT ( 'NONE',  ( 11.81601139373100651, 28.73617430169779041, 5.000000000000000000 ) ) ;
#119312 = CARTESIAN_POINT ( 'NONE',  ( -36.18398860626899705, 28.73617430169812437, 5.000000000000000000 ) ) ;
#119313 = CARTESIAN_POINT ( 'NONE',  ( 5.483345613589513334, 22.22500000000000142, 4.500000000000000888 ) ) ;
#119314 = CARTESIAN_POINT ( 'NONE',  ( 76.25000000000000000, -9.735942053221458872E-16, 7.950000000000000178 ) ) ;
#119315 = DIRECTION ( 'NONE',  ( 0.7071067811865487940, -0.7071067811865463515, 0.000000000000000000 ) ) ;
#119316 = ORIENTED_EDGE ( 'NONE', *, *, #138109, .F. ) ;
#119317 = EDGE_CURVE ( 'NONE', #47321, #85516, #104444, .T. ) ;
#119318 = ORIENTED_EDGE ( 'NONE', *, *, #14346, .T. ) ;
#119319 = CARTESIAN_POINT ( 'NONE',  ( 65.47959685856477563, 6.109999999999999432, 1.637169565754164280 ) ) ;
#119320 = ORIENTED_EDGE ( 'NONE', *, *, #127973, .T. ) ;
#119321 = DIRECTION ( 'NONE',  ( 0.6830127018922180770, -0.6830127018922204085, -0.2588190451025213501 ) ) ;
#119322 = CARTESIAN_POINT ( 'NONE',  ( 27.00000000000000355, 0.000000000000000000, 7.950000000000000178 ) ) ;
#119323 = CARTESIAN_POINT ( 'NONE',  ( -50.99451991528749062, 28.92564299267973738, 4.000000000000000000 ) ) ;
#119324 = CARTESIAN_POINT ( 'NONE',  ( 6.459838389497365441, 18.75929247661552779, 8.305906642995500633 ) ) ;
#119325 = ORIENTED_EDGE ( 'NONE', *, *, #27445, .T. ) ;
#119326 = CARTESIAN_POINT ( 'NONE',  ( 45.18398860626900415, 28.73617430169818832, 5.000000000000000000 ) ) ;
#119327 = CARTESIAN_POINT ( 'NONE',  ( 12.86840764549667604, 9.139736423841732040E-16, 0.000000000000000000 ) ) ;
#119328 = ORIENTED_EDGE ( 'NONE', *, *, #112198, .T. ) ;
#119329 = EDGE_CURVE ( 'NONE', #115416, #136288, #92137, .T. ) ;
#119330 = LINE ( 'NONE', #20018, #113910 ) ;
#119331 = CARTESIAN_POINT ( 'NONE',  ( 5.691592354503320905, 9.902892378096218942E-16, 0.000000000000000000 ) ) ;
#119332 = CARTESIAN_POINT ( 'NONE',  ( -5.843876922607543989, -22.22500000000000142, 4.000000000000000000 ) ) ;
#119333 = VERTEX_POINT ( 'NONE', #27597 ) ;
#119334 = ORIENTED_EDGE ( 'NONE', *, *, #81379, .F. ) ;
#119335 = EDGE_CURVE ( 'NONE', #73203, #51894, #46566, .T. ) ;
#119336 = FACE_BOUND ( 'NONE', #20870, .T. ) ;
#119337 = CARTESIAN_POINT ( 'NONE',  ( -21.18398860626899349, 28.73617430169802134, 5.000000000000000000 ) ) ;
#119338 = CARTESIAN_POINT ( 'NONE',  ( 25.39999999999999858, -57.15000000000009095, 34.92499999999998295 ) ) ;
#119339 = CARTESIAN_POINT ( 'NONE',  ( 61.95833333333332149, 3.974999999999997424, 6.884901960086288852 ) ) ;
#119340 = LINE ( 'NONE', #75874, #74316 ) ;
#119342 = ORIENTED_EDGE ( 'NONE', *, *, #130554, .F. ) ;
#119341 = VECTOR ( 'NONE', #68914, 999.9999999999998863 ) ;
#119343 = EDGE_LOOP ( 'NONE', ( #7874, #93082, #75201, #36620, #13637 ) ) ;
#119344 = CARTESIAN_POINT ( 'NONE',  ( 116.5787635252314516, -7.482591942790325086E-16, 6.109999999999998543 ) ) ;
#119345 = EDGE_LOOP ( 'NONE', ( #50, #90299, #129546, #24624 ) ) ;
#119346 = STYLED_ITEM ( 'NONE', ( #17689 ), #90943 ) ;
#119347 = ORIENTED_EDGE ( 'NONE', *, *, #114544, .T. ) ;
#119348 = CARTESIAN_POINT ( 'NONE',  ( 183.3316408629058003, -52.14999999999999147, 41.64499999999997470 ) ) ;
#119349 = CARTESIAN_POINT ( 'NONE',  ( -32.18753812416031224, -22.22500000000000142, 4.000000000000000000 ) ) ;
#119350 = CARTESIAN_POINT ( 'NONE',  ( 13.36902924655238323, 1.333290112598358945, 4.303104124266152297 ) ) ;
#119351 = VERTEX_POINT ( 'NONE', #69724 ) ;
#119352 = VECTOR ( 'NONE', #64220, 1000.000000000000000 ) ;
#119353 = LINE ( 'NONE', #75886, #20425 ) ;
#119354 = LINE ( 'NONE', #9895, #128371 ) ;
#119355 = ADVANCED_FACE ( 'NONE', ( #4359 ), #13850, .F. ) ;
#119356 = DIRECTION ( 'NONE',  ( -0.6830127018922180770, -0.6830127018922204085, -0.2588190451025213501 ) ) ;
#119357 = LINE ( 'NONE', #111348, #85511 ) ;
#119358 = DIRECTION ( 'NONE',  ( -0.5735764363510501562, 0.8191520442889890230, 1.003171929053521419E-16 ) ) ;
#119359 = VERTEX_POINT ( 'NONE', #91458 ) ;
#119360 = DIRECTION ( 'NONE',  ( -0.6830127018922180770, -0.6830127018922204085, -0.2588190451025213501 ) ) ;
#119361 = DIRECTION ( 'NONE',  ( 0.000000000000000000, -1.000000000000000000, 0.000000000000000000 ) ) ;
#119362 = ORIENTED_EDGE ( 'NONE', *, *, #8647, .F. ) ;
#119363 = ADVANCED_FACE ( 'NONE', ( #116029 ), #102344, .F. ) ;
#119364 = DIRECTION ( 'NONE',  ( 0.000000000000000000, 1.000000000000000000, 0.000000000000000000 ) ) ;
#119365 = ORIENTED_EDGE ( 'NONE', *, *, #125350, .F. ) ;
#119366 = VERTEX_POINT ( 'NONE', #2993 ) ;
#119367 = EDGE_CURVE ( 'NONE', #82762, #135296, #5103, .T. ) ;
#119368 = EDGE_LOOP ( 'NONE', ( #32037, #50048, #55357, #139183, #27203 ) ) ;
#119369 = CARTESIAN_POINT ( 'NONE',  ( 61.10459685856476852, 1.637169565754164946, -6.109999999999999432 ) ) ;
#119370 = ORIENTED_EDGE ( 'NONE', *, *, #86994, .T. ) ;
#119371 = ORIENTED_EDGE ( 'NONE', *, *, #136580, .F. ) ;
#119372 = VECTOR ( 'NONE', #18556, 999.9999999999998863 ) ;
#119373 = DIRECTION ( 'NONE',  ( 0.000000000000000000, 0.000000000000000000, -1.000000000000000000 ) ) ;
#119374 =( GEOMETRIC_REPRESENTATION_CONTEXT ( 3 ) GLOBAL_UNCERTAINTY_ASSIGNED_CONTEXT ( ( #1061 ) ) GLOBAL_UNIT_ASSIGNED_CONTEXT ( ( #107553, #137354, #129299 ) ) REPRESENTATION_CONTEXT ( 'NONE', 'WORKASPACE' ) );
#119375 =( NAMED_UNIT ( * ) SI_UNIT ( $, .STERADIAN. ) SOLID_ANGLE_UNIT ( ) );
#119376 = CARTESIAN_POINT ( 'NONE',  ( 103.9795968585647756, 6.109999999999999432, 1.637169565754164280 ) ) ;
#119377 = DIRECTION ( 'NONE',  ( -0.5735764363510501562, 0.8191520442889890230, 1.003171929053521419E-16 ) ) ;
#119378 = VECTOR ( 'NONE', #35473, 999.9999999999998863 ) ;
#119379 = DIRECTION ( 'NONE',  ( 0.000000000000000000, 0.000000000000000000, -1.000000000000000000 ) ) ;
#119380 = ORIENTED_EDGE ( 'NONE', *, *, #135523, .T. ) ;
#119381 = CARTESIAN_POINT ( 'NONE',  ( 0.4892135623730947680, -27.52281430457055578, 5.000000000000000000 ) ) ;
#119382 = AXIS2_PLACEMENT_3D ( 'NONE', #75104, #130183, #10507 ) ;
#119383 = FACE_OUTER_BOUND ( 'NONE', #107450, .T. ) ;
#119384 = EDGE_CURVE ( 'NONE', #62368, #39664, #82035, .T. ) ;
#119385 = DIRECTION ( 'NONE',  ( -1.000000000000000000, -1.224606353822377258E-16, -0.000000000000000000 ) ) ;
#119386 = CARTESIAN_POINT ( 'NONE',  ( 76.78752705046289861, 0.000000000000000000, -7.949999999999998401 ) ) ;
#119387 = ORIENTED_EDGE ( 'NONE', *, *, #25981, .T. ) ;
#119388 = DIRECTION ( 'NONE',  ( 1.000000000000000000, 0.000000000000000000, 0.000000000000000000 ) ) ;
#119389 = ORIENTED_EDGE ( 'NONE', *, *, #93391, .T. ) ;
#119390 = VERTEX_POINT ( 'NONE', #125510 ) ;
#119391 = EDGE_LOOP ( 'NONE', ( #69784, #96216, #133026, #114723 ) ) ;
#119392 = CARTESIAN_POINT ( 'NONE',  ( 117.8912635252314516, -4.472830434245838482, -4.472830434245838482 ) ) ;
#119393 = VERTEX_POINT ( 'NONE', #16732 ) ;
#119394 = DIRECTION ( 'NONE',  ( 0.000000000000000000, 0.000000000000000000, 1.000000000000000000 ) ) ;
#119395 = LINE ( 'NONE', #77894, #54783 ) ;
#119396 = DIRECTION ( 'NONE',  ( -0.7071067811865486830, -0.7071067811865464625, -0.000000000000000000 ) ) ;
#119397 = PLANE ( 'NONE',  #32446 ) ;
#119398 = ORIENTED_EDGE ( 'NONE', *, *, #40352, .T. ) ;
#119399 = CARTESIAN_POINT ( 'NONE',  ( 0.2242312616537213421, -48.73293412427595683, 38.67339632249958470 ) ) ;
#119400 = ORIENTED_EDGE ( 'NONE', *, *, #49610, .F. ) ;
#119401 = CARTESIAN_POINT ( 'NONE',  ( -0.4587635252314473666, 0.000000000000000000, 7.934999999999990727 ) ) ;
#119402 = PLANE ( 'NONE',  #39302 ) ;
#119403 = EDGE_CURVE ( 'NONE', #72122, #58614, #61010, .T. ) ;
#119404 = CARTESIAN_POINT ( 'NONE',  ( 34.92499999999998295, 1.512461875839459680, 4.000000000000000000 ) ) ;
#119405 = CARTESIAN_POINT ( 'NONE',  ( 38.33333333333332860, -6.884901960086287964, 3.974999999999998312 ) ) ;
#119406 = ORIENTED_EDGE ( 'NONE', *, *, #99424, .F. ) ;
#119407 = EDGE_CURVE ( 'NONE', #55578, #100010, #92858, .T. ) ;
#119408 = ORIENTED_EDGE ( 'NONE', *, *, #38620, .T. ) ;
#119409 = ORIENTED_EDGE ( 'NONE', *, *, #79028, .F. ) ;
#119410 = DIRECTION ( 'NONE',  ( 0.000000000000000000, 0.000000000000000000, -1.000000000000000000 ) ) ;
#119411 = CARTESIAN_POINT ( 'NONE',  ( 26.90840764549667696, -2.500000000000000888, 0.000000000000000000 ) ) ;
#119412 = CARTESIAN_POINT ( 'NONE',  ( -0.1839886062690032631, 28.73617430169787568, 5.000000000000000000 ) ) ;
#119413 = DIRECTION ( 'NONE',  ( 0.7071067811865487940, 0.7071067811865463515, -0.000000000000000000 ) ) ;
#119414 = EDGE_CURVE ( 'NONE', #110607, #100364, #36360, .T. ) ;
#119415 = EDGE_CURVE ( 'NONE', #54885, #13795, #90753, .T. ) ;
#119416 = DIRECTION ( 'NONE',  ( 0.000000000000000000, -1.137193330093851115E-16, 1.000000000000000000 ) ) ;
#119417 = CARTESIAN_POINT ( 'NONE',  ( 31.92500000000001492, 9.947201970464227326E-15, -40.00000000000000000 ) ) ;
#119418 = CARTESIAN_POINT ( 'NONE',  ( 27.41709685856476142, 3.054999999999998828, 5.291415217122922066 ) ) ;
#119419 = LINE ( 'NONE', #63672, #71895 ) ;
#119420 = FACE_OUTER_BOUND ( 'NONE', #52419, .T. ) ;
#119421 = ORIENTED_EDGE ( 'NONE', *, *, #112848, .T. ) ;
#119422 = CARTESIAN_POINT ( 'NONE',  ( 14.71998032010587565, 0.7592924766157173044, 14.27032725228012033 ) ) ;
#119423 = ORIENTED_EDGE ( 'NONE', *, *, #82785, .F. ) ;
#119424 = DIRECTION ( 'NONE',  ( 0.6830127018922181881, 0.6830127018922202975, -0.2588190451025214056 ) ) ;
#119425 = VERTEX_POINT ( 'NONE', #49405 ) ;
#119426 =( BOUNDED_CURVE ( )  B_SPLINE_CURVE ( 3, ( #91929, #134767, #115076, #136155 ),
 .UNSPECIFIED., .F., .T. ) 
 B_SPLINE_CURVE_WITH_KNOTS ( ( 4, 4 ),
 ( 1.378368140454906854, 1.408685637663195767 ),
 .UNSPECIFIED. ) 
 CURVE ( )  GEOMETRIC_REPRESENTATION_ITEM ( )  RATIONAL_B_SPLINE_CURVE ( ( 1.000000000000000000, 0.9999234055803066790, 0.9999234055803066790, 1.000000000000000000 ) ) 
 REPRESENTATION_ITEM ( '' )  );
#119427 = CARTESIAN_POINT ( 'NONE',  ( 23.29298673570678346, -21.74070752338406720, 4.999753212805222446 ) ) ;
#119429 = ORIENTED_EDGE ( 'NONE', *, *, #65776, .T. ) ;
#119428 = CARTESIAN_POINT ( 'NONE',  ( -48.48921356237309510, -27.52281430457089328, 5.000000000000000000 ) ) ;
#119430 = ADVANCED_FACE ( 'NONE', ( #26896 ), #79905, .F. ) ;
#119431 = EDGE_CURVE ( 'NONE', #57808, #81070, #71140, .T. ) ;
#119432 = DIRECTION ( 'NONE',  ( -0.3543493200069162685, -0.000000000000000000, -0.9351131265310288487 ) ) ;
#119433 = ORIENTED_EDGE ( 'NONE', *, *, #141852, .T. ) ;
#119434 = DIRECTION ( 'NONE',  ( 0.7071067811865487940, 0.7071067811865463515, -0.000000000000000000 ) ) ;
#119435 = VERTEX_POINT ( 'NONE', #25453 ) ;
#119436 = FACE_OUTER_BOUND ( 'NONE', #30761, .T. ) ;
#119437 = ORIENTED_EDGE ( 'NONE', *, *, #109081, .T. ) ;
#119438 = CARTESIAN_POINT ( 'NONE',  ( 92.53752705046289861, -9.735942053221456900E-16, 7.949999999999998401 ) ) ;
#119439 = VECTOR ( 'NONE', #124694, 1000.000000000000000 ) ;
#119440 = CARTESIAN_POINT ( 'NONE',  ( 109.1625270504628986, 7.949999999999998401, 1.460391307983218338E-15 ) ) ;
#119441 = DIRECTION ( 'NONE',  ( -1.000000000000000000, -1.224606353822377258E-16, -0.000000000000000000 ) ) ;
#119442 = EDGE_CURVE ( 'NONE', #67004, #92014, #93591, .T. ) ;
#119443 = CARTESIAN_POINT ( 'NONE',  ( -15.47512612785036090, 14.25929247661557575, 9.797011795316599603 ) ) ;
#119444 = CARTESIAN_POINT ( 'NONE',  ( -32.29289321881322650, -3.740707523384248390, 5.000000000000000000 ) ) ;
#119445 = PLANE ( 'NONE',  #102729 ) ;
#119446 = CARTESIAN_POINT ( 'NONE',  ( 2.161706124526183714, -6.740707523384205757, 16.75550250614867664 ) ) ;
#119447 = CARTESIAN_POINT ( 'NONE',  ( 4.666666666666666963, -5.278424836066145431, -3.047499999999993658 ) ) ;
#119448 = CARTESIAN_POINT ( 'NONE',  ( 14.41623647476855297, -7.934999999999990727, 4.858786175617117713E-16 ) ) ;
#119449 = ADVANCED_FACE ( 'NONE', ( #113176 ), #47286, .T. ) ;
#119450 = CARTESIAN_POINT ( 'NONE',  ( 8.999999999999932498, 20.70535890316562089, 1.956823837851896286 ) ) ;
#119451 = PLANE ( 'NONE',  #6149 ) ;
#119452 = ORIENTED_EDGE ( 'NONE', *, *, #122190, .T. ) ;
#119453 = ORIENTED_EDGE ( 'NONE', *, *, #40880, .T. ) ;
#119454 = PLANE ( 'NONE',  #118422 ) ;
#119455 = VERTEX_POINT ( 'NONE', #15978 ) ;
#119456 = VECTOR ( 'NONE', #30134, 1000.000000000000000 ) ;
#119457 = LINE ( 'NONE', #75989, #115060 ) ;
#119458 = LINE ( 'NONE', #131801, #62504 ) ;
#119459 = FILL_AREA_STYLE ('',( #85409 ) ) ;
#119460 = EDGE_CURVE ( 'NONE', #79224, #55061, #82719, .T. ) ;
#119461 = CARTESIAN_POINT ( 'NONE',  ( 128.1415536296147479, -48.60795469097355692, -38.18754904899805780 ) ) ;
#119462 = ORIENTED_EDGE ( 'NONE', *, *, #35492, .T. ) ;
#119463 = CARTESIAN_POINT ( 'NONE',  ( -0.4892135623730947680, -27.52281430457055578, 5.000000000000000000 ) ) ;
#119464 = CARTESIAN_POINT ( 'NONE',  ( 0.000000000000000000, 0.000000000000000000, 0.000000000000000000 ) ) ;
#119465 = VECTOR ( 'NONE', #94883, 1000.000000000000000 ) ;
#119466 = CYLINDRICAL_SURFACE ( 'NONE', #37904, 6.094999999999989093 ) ;
#119468 = ORIENTED_EDGE ( 'NONE', *, *, #11334, .T. ) ;
#119467 = DIRECTION ( 'NONE',  ( 0.7071067811865487940, 0.7071067811865463515, 0.000000000000000000 ) ) ;
#119469 = CARTESIAN_POINT ( 'NONE',  ( 28.17183060077627133, 15.75929247661555443, 4.000000000000000000 ) ) ;
#119470 = ADVANCED_FACE ( 'NONE', ( #62403 ), #40645, .F. ) ;
#119471 = CARTESIAN_POINT ( 'NONE',  ( -7.056846916127231314E-14, -40.42999999999999261, 19.06900128115122328 ) ) ;
#119472 = FACE_OUTER_BOUND ( 'NONE', #127386, .T. ) ;
#119473 = VECTOR ( 'NONE', #30000, 1000.000000000000000 ) ;
#119474 = CARTESIAN_POINT ( 'NONE',  ( -45.48921356237309510, -27.52281430457087197, 5.000000000000000000 ) ) ;
#119475 = ORIENTED_EDGE ( 'NONE', *, *, #72093, .T. ) ;
#119476 = EDGE_CURVE ( 'NONE', #31146, #60580, #73280, .T. ) ;
#119477 = ORIENTED_EDGE ( 'NONE', *, *, #40269, .F. ) ;
#119478 = ORIENTED_EDGE ( 'NONE', *, *, #122190, .F. ) ;
#119479 = AXIS2_PLACEMENT_3D ( 'NONE', #56604, #100770, #45707 ) ;
#119480 = CARTESIAN_POINT ( 'NONE',  ( 104.4170968585647756, 3.054999999999998828, 5.291415217122922066 ) ) ;
#119481 = ORIENTED_EDGE ( 'NONE', *, *, #15821, .F. ) ;
#119482 = VECTOR ( 'NONE', #58032, 1000.000000000000000 ) ;
#119483 = CARTESIAN_POINT ( 'NONE',  ( 127.6280169629028762, -46.44627868284323569, 35.89947574910195272 ) ) ;
#119484 = CIRCLE ( 'NONE', #52346, 0.5000000000000000000 ) ;
#119485 = CARTESIAN_POINT ( 'NONE',  ( 21.18398860626899349, 28.73617430169802134, 5.000000000000000000 ) ) ;
#119486 = VERTEX_POINT ( 'NONE', #50095 ) ;
#119487 = CARTESIAN_POINT ( 'NONE',  ( 183.8105469881215868, -51.90335959434331414, 39.28179725402794276 ) ) ;
#119488 = LINE ( 'NONE', #120191, #129928 ) ;
#119489 = CARTESIAN_POINT ( 'NONE',  ( 99.37043019189812298, -3.055000000000001492, 5.291415217122917625 ) ) ;
#119490 = ORIENTED_EDGE ( 'NONE', *, *, #91067, .F. ) ;
#119491 = CARTESIAN_POINT ( 'NONE',  ( 26.99999999999981881, -1.447814304570811617, 5.000000000000000000 ) ) ;
#119492 = CARTESIAN_POINT ( 'NONE',  ( 23.99999999999983302, -12.03360074219761167, 5.000000000000000000 ) ) ;
#119493 = DIRECTION ( 'NONE',  ( 0.3543493200069164351, 2.781805975412904658E-17, -0.9351131265310288487 ) ) ;
#119494 = FACE_OUTER_BOUND ( 'NONE', #118050, .T. ) ;
#119495 = ORIENTED_EDGE ( 'NONE', *, *, #78913, .F. ) ;
#119496 = ORIENTED_EDGE ( 'NONE', *, *, #46354, .T. ) ;
#119497 = ORIENTED_EDGE ( 'NONE', *, *, #80007, .F. ) ;
#119498 = LINE ( 'NONE', #54308, #79260 ) ;
#119499 = DIRECTION ( 'NONE',  ( -0.7071067811865486830, -0.7071067811865464625, 0.000000000000000000 ) ) ;
#119500 = CARTESIAN_POINT ( 'NONE',  ( 18.58790314143521982, 6.871911579029515771, 3.967499999999989146 ) ) ;
#119501 = CARTESIAN_POINT ( 'NONE',  ( -13.17183060077638679, -2.240707523384260824, 4.000000000000000000 ) ) ;
#119502 = DIRECTION ( 'NONE',  ( 0.6830127018922180770, -0.6830127018922204085, -0.2588190451025213501 ) ) ;
#119503 = ORIENTED_EDGE ( 'NONE', *, *, #5413, .F. ) ;
#119504 = EDGE_LOOP ( 'NONE', ( #137225, #100269, #121726, #47918 ) ) ;
#119505 = CARTESIAN_POINT ( 'NONE',  ( -21.88339156388719431, -2.079482862307782121, 4.335713449946893228 ) ) ;
#119507 = EDGE_CURVE ( 'NONE', #27663, #46917, #96403, .T. ) ;
#119506 = ORIENTED_EDGE ( 'NONE', *, *, #112897, .T. ) ;
#119508 = EDGE_LOOP ( 'NONE', ( #108611, #109773, #1615, #7172 ) ) ;
#119509 = VECTOR ( 'NONE', #99697, 1000.000000000000000 ) ;
#119510 = CARTESIAN_POINT ( 'NONE',  ( 18.52083333333333215, -6.094999999999989981, -1.633150327867689322 ) ) ;
#119511 = CARTESIAN_POINT ( 'NONE',  ( 1.516262732464674023, -2.500000000000000000, 0.000000000000000000 ) ) ;
#119512 = ORIENTED_EDGE ( 'NONE', *, *, #71975, .F. ) ;
#119513 = CARTESIAN_POINT ( 'NONE',  ( 34.92499999999998295, 22.22500000000000142, 4.000000000000000000 ) ) ;
#119514 = EDGE_CURVE ( 'NONE', #57507, #132762, #118156, .T. ) ;
#119515 = PLANE ( 'NONE',  #89548 ) ;
#119516 = VECTOR ( 'NONE', #92699, 1000.000000000000000 ) ;
#119517 = CARTESIAN_POINT ( 'NONE',  ( -11.99999999999991651, -21.03360074219752462, 5.000000000000000000 ) ) ;
#119518 = LINE ( 'NONE', #87641, #51314 ) ;
#119519 = ORIENTED_EDGE ( 'NONE', *, *, #126843, .F. ) ;
#119520 = ORIENTED_EDGE ( 'NONE', *, *, #137968, .T. ) ;
#119521 = CARTESIAN_POINT ( 'NONE',  ( 25.40000000000001634, 6.851870715257561528, -4.022987505400126729 ) ) ;
#119522 = ADVANCED_FACE ( 'NONE', ( #31195 ), #63828, .F. ) ;
#119523 = DIRECTION ( 'NONE',  ( 0.7071067811865487940, 0.7071067811865463515, 0.000000000000000000 ) ) ;
#119524 = ORIENTED_EDGE ( 'NONE', *, *, #125262, .T. ) ;
#119525 = PLANE ( 'NONE',  #109321 ) ;
#119526 = ORIENTED_EDGE ( 'NONE', *, *, #53007, .F. ) ;
#119528 = ADVANCED_FACE ( 'NONE', ( #75412 ), #97103, .F. ) ;
#119527 = CARTESIAN_POINT ( 'NONE',  ( 23.63159235450331863, -2.500000000000000444, 3.061616997868384620E-16 ) ) ;
#119529 = VERTEX_POINT ( 'NONE', #7975 ) ;
#119530 = ORIENTED_EDGE ( 'NONE', *, *, #37258, .T. ) ;
#119531 = EDGE_CURVE ( 'NONE', #9882, #3445, #140641, .T. ) ;
#119532 = VERTEX_POINT ( 'NONE', #83436 ) ;
#119533 = ADVANCED_FACE ( 'NONE', ( #17439 ), #94984, .F. ) ;
#119534 = AXIS2_PLACEMENT_3D ( 'NONE', #32211, #66277, #9719 ) ;
#119535 = CARTESIAN_POINT ( 'NONE',  ( 27.18293019189811588, -1.637169565754158951, -6.109999999999998543 ) ) ;
#119536 = DIRECTION ( 'NONE',  ( -0.7071067811865486830, 0.7071067811865464625, 0.000000000000000000 ) ) ;
#119537 = LINE ( 'NONE', #142754, #32193 ) ;
#119538 = DIRECTION ( 'NONE',  ( 0.000000000000000000, -1.000000000000000000, 0.000000000000000000 ) ) ;
#119539 = VECTOR ( 'NONE', #121489, 1000.000000000000000 ) ;
#119540 = CARTESIAN_POINT ( 'NONE',  ( 127.4587635252314470, 0.000000000000000000, -6.110000000000001208 ) ) ;
#119541 = FACE_OUTER_BOUND ( 'NONE', #37588, .T. ) ;
#119542 = ADVANCED_FACE ( 'NONE', ( #127649 ), #28341, .T. ) ;
#119543 = CARTESIAN_POINT ( 'NONE',  ( -27.79289321881326202, -17.24070752338409918, 5.000000000000000000 ) ) ;
#119544 = DIRECTION ( 'NONE',  ( -0.7071067811865486830, 0.7071067811865464625, 0.000000000000000000 ) ) ;
#119545 = DIRECTION ( 'NONE',  ( -0.7071067811865486830, 0.7071067811865464625, 0.000000000000000000 ) ) ;
#119546 = EDGE_CURVE ( 'NONE', #118475, #127411, #32662, .T. ) ;
#119547 = PLANE ( 'NONE',  #59829 ) ;
#119548 = DIRECTION ( 'NONE',  ( -0.7071067811865486830, -0.7071067811865464625, 0.000000000000000000 ) ) ;
#119549 = LINE ( 'NONE', #142764, #37836 ) ;
#119550 = COLOUR_RGB ( '', 0.72549020, 0.75294118, 0.79215686) ;
#119551 = ORIENTED_EDGE ( 'NONE', *, *, #135943, .T. ) ;
#119552 = ORIENTED_EDGE ( 'NONE', *, *, #106887, .T. ) ;
#119553 = ORIENTED_EDGE ( 'NONE', *, *, #119704, .F. ) ;
#119554 = ORIENTED_EDGE ( 'NONE', *, *, #2424, .F. ) ;
#119555 = DIRECTION ( 'NONE',  ( 0.6830127018922181881, 0.6830127018922202975, -0.2588190451025214056 ) ) ;
#119556 = EDGE_CURVE ( 'NONE', #33921, #38622, #50798, .T. ) ;
#119557 = VERTEX_POINT ( 'NONE', #18119 ) ;
#119558 = ORIENTED_EDGE ( 'NONE', *, *, #68335, .F. ) ;
#119559 = LINE ( 'NONE', #128347, #125518 ) ;
#119560 = CARTESIAN_POINT ( 'NONE',  ( 8.994519915287490619, 28.92564299267944250, 4.000000000000000000 ) ) ;
#119561 = AXIS2_PLACEMENT_3D ( 'NONE', #23599, #24318, #45391 ) ;
#119562 = LINE ( 'NONE', #51504, #18433 ) ;
#119563 = ORIENTED_EDGE ( 'NONE', *, *, #121194, .T. ) ;
#119564 = CARTESIAN_POINT ( 'NONE',  ( 24.07469600201484283, -0.04978799960961742543, 4.760162856047378099 ) ) ;
#119565 = EDGE_CURVE ( 'NONE', #133408, #123203, #52216, .T. ) ;
#119566 = ADVANCED_FACE ( 'NONE', ( #106565 ), #128369, .F. ) ;
#119567 = ORIENTED_EDGE ( 'NONE', *, *, #136655, .F. ) ;
#119568 = AXIS2_PLACEMENT_3D ( 'NONE', #119331, #7718, #20741 ) ;
#119570 = CARTESIAN_POINT ( 'NONE',  ( 31.49999999999977973, 13.46639925780212010, 5.000000000000000000 ) ) ;
#119569 = VECTOR ( 'NONE', #122006, 999.9999999999998863 ) ;
#119571 = CARTESIAN_POINT ( 'NONE',  ( -14.99999999999988098, -19.44781430457063465, 5.000000000000000000 ) ) ;
#119572 = VECTOR ( 'NONE', #83878, 1000.000000000000000 ) ;
#119573 = CARTESIAN_POINT ( 'NONE',  ( 8.962903141435219823, -3.967499999999994476, 6.871911579029513106 ) ) ;
#119574 = ORIENTED_EDGE ( 'NONE', *, *, #48314, .T. ) ;
#119575 = CARTESIAN_POINT ( 'NONE',  ( 96.59959685856476597, -6.109999999999998543, -1.637169565754160727 ) ) ;
#119576 = CARTESIAN_POINT ( 'NONE',  ( 7.656579674618784637, -8.841847278798848464, 3.478651043998596037 ) ) ;
#119577 = LINE ( 'NONE', #131928, #60640 ) ;
#119578 = ORIENTED_EDGE ( 'NONE', *, *, #125672, .F. ) ;
#119579 = EDGE_CURVE ( 'NONE', #132258, #134235, #51524, .T. ) ;
#119580 = VERTEX_POINT ( 'NONE', #95718 ) ;
#119581 = CARTESIAN_POINT ( 'NONE',  ( 152.4000000000000057, -14.29000000000013593, 12.69999999999954632 ) ) ;
#119582 = ORIENTED_EDGE ( 'NONE', *, *, #107516, .F. ) ;
#119583 = CARTESIAN_POINT ( 'NONE',  ( -3.183988606268992161, 28.73617430169789699, 5.000000000000000000 ) ) ;
#119584 = CARTESIAN_POINT ( 'NONE',  ( -19.27928215921719612, -2.789594763390444321, 4.000000000000000000 ) ) ;
#119585 = AXIS2_PLACEMENT_3D ( 'NONE', #124479, #114311, #69402 ) ;
#119586 = DIRECTION ( 'NONE',  ( 0.6830127018922180770, -0.6830127018922204085, -0.2588190451025213501 ) ) ;
#119587 = CARTESIAN_POINT ( 'NONE',  ( 24.32816939922335919, -3.740707523384244837, 4.000000000000000000 ) ) ;
#119588 = EDGE_LOOP ( 'NONE', ( #74991, #90038, #91022, #67956 ) ) ;
#119589 = ADVANCED_FACE ( 'NONE', ( #139970 ), #30476, .F. ) ;
#119590 = EDGE_CURVE ( 'NONE', #64185, #141627, #109451, .T. ) ;
#119591 = LINE ( 'NONE', #20286, #36787 ) ;
#119592 = DIRECTION ( 'NONE',  ( 1.000000000000000000, 0.000000000000000000, 0.000000000000000000 ) ) ;
#119593 = DIRECTION ( 'NONE',  ( 0.7071067811865487940, 0.7071067811865463515, -0.000000000000000000 ) ) ;
#119594 = VERTEX_POINT ( 'NONE', #111596 ) ;
#119595 = DIRECTION ( 'NONE',  ( -0.6830127018922180770, -0.6830127018922204085, -0.2588190451025214056 ) ) ;
#119597 = EDGE_CURVE ( 'NONE', #84015, #46769, #89830, .T. ) ;
#119596 = LINE ( 'NONE', #11543, #81825 ) ;
#119598 = ORIENTED_EDGE ( 'NONE', *, *, #83540, .T. ) ;
#119600 = VERTEX_POINT ( 'NONE', #22416 ) ;
#119599 = CARTESIAN_POINT ( 'NONE',  ( -32.99451991528749062, 28.92564299267960948, 4.000000000000000000 ) ) ;
#119602 = ORIENTED_EDGE ( 'NONE', *, *, #46571, .T. ) ;
#119601 = EDGE_CURVE ( 'NONE', #16081, #89139, #121737, .T. ) ;
#119603 = LINE ( 'NONE', #20297, #109478 ) ;
#119604 = CARTESIAN_POINT ( 'NONE',  ( -34.92500000000001137, 3.006123077391908094, 4.000000000000000000 ) ) ;
#119605 = ORIENTED_EDGE ( 'NONE', *, *, #100917, .T. ) ;
#119606 = CARTESIAN_POINT ( 'NONE',  ( 26.99451991528749417, 28.92564299267956685, 4.000000000000000000 ) ) ;
#119607 = DIRECTION ( 'NONE',  ( -0.000000000000000000, 0.000000000000000000, 1.000000000000000000 ) ) ;
#119608 = EDGE_CURVE ( 'NONE', #114524, #53240, #42831, .T. ) ;
#119609 = DIRECTION ( 'NONE',  ( 1.000000000000000000, 0.000000000000000000, 0.000000000000000000 ) ) ;
#119610 = CARTESIAN_POINT ( 'NONE',  ( -33.75860074219772855, 21.72500000000000142, 5.000000000000000000 ) ) ;
#119611 = DIRECTION ( 'NONE',  ( -0.7071067811865486830, 0.7071067811865464625, 0.000000000000000000 ) ) ;
#119612 = CARTESIAN_POINT ( 'NONE',  ( 2.994519915287485734, 28.92564299267940342, 4.000000000000000000 ) ) ;
#119613 = CARTESIAN_POINT ( 'NONE',  ( 25.19159235450331735, 2.500000000000001332, 0.000000000000000000 ) ) ;
#119614 = DIRECTION ( 'NONE',  ( -1.000000000000000000, -1.224606353822377258E-16, -0.000000000000000000 ) ) ;
#119616 = CIRCLE ( 'NONE', #82610, 6.349999999999997868 ) ;
#119615 = FACE_OUTER_BOUND ( 'NONE', #24676, .T. ) ;
#119617 = PLANE ( 'NONE',  #96911 ) ;
#119618 = EDGE_CURVE ( 'NONE', #69925, #123496, #79000, .T. ) ;
#119619 = CARTESIAN_POINT ( 'NONE',  ( -26.99999999999980815, 20.96639925780204550, 5.000000000000000000 ) ) ;
#119620 = CARTESIAN_POINT ( 'NONE',  ( -34.92500000000001137, 14.93779483949078823, 7.761394445350714655 ) ) ;
#119621 = ORIENTED_EDGE ( 'NONE', *, *, #141574, .T. ) ;
#119622 = VERTEX_POINT ( 'NONE', #134074 ) ;
#119623 = ORIENTED_EDGE ( 'NONE', *, *, #102662, .T. ) ;
#119624 = CARTESIAN_POINT ( 'NONE',  ( 112.1250000000000000, -7.950000000000000178, -4.867971026610729436E-16 ) ) ;
#119625 = ORIENTED_EDGE ( 'NONE', *, *, #117113, .T. ) ;
#119626 = ORIENTED_EDGE ( 'NONE', *, *, #9833, .T. ) ;
#119627 = EDGE_LOOP ( 'NONE', ( #27225, #73361, #2736, #17631 ) ) ;
#119628 = AXIS2_PLACEMENT_3D ( 'NONE', #105898, #92177, #38540 ) ;
#119629 = CARTESIAN_POINT ( 'NONE',  ( 18.48921356237309510, -27.52281430457068367, 5.000000000000000000 ) ) ;
#119630 = CARTESIAN_POINT ( 'NONE',  ( -13.17183060077637613, 0.7592924766157069794, 4.000000000000000000 ) ) ;
#119631 = ORIENTED_EDGE ( 'NONE', *, *, #120122, .T. ) ;
#119632 = PLANE ( 'NONE',  #25427 ) ;
#119634 = CIRCLE ( 'NONE', #138197, 16.45000000000002061 ) ;
#119633 = CARTESIAN_POINT ( 'NONE',  ( 8.897059064271770623, 4.202752102959690472E-16, 0.000000000000000000 ) ) ;
#119635 = CARTESIAN_POINT ( 'NONE',  ( -23.99999999999982947, 19.93112307739197675, 4.000000000000000000 ) ) ;
#119636 = CARTESIAN_POINT ( 'NONE',  ( 99.16709685856477563, -3.055000000000000160, -5.291415217122921177 ) ) ;
#119637 = VERTEX_POINT ( 'NONE', #76120 ) ;
#119638 = FACE_OUTER_BOUND ( 'NONE', #30016, .T. ) ;
#119639 = CARTESIAN_POINT ( 'NONE',  ( -31.49999999999977973, -7.533600742197658739, 5.000000000000000000 ) ) ;
#119640 = LINE ( 'NONE', #142167, #49795 ) ;
#119641 = DIRECTION ( 'NONE',  ( 0.000000000000000000, -1.000000000000000000, 0.000000000000000000 ) ) ;
#119642 = PLANE ( 'NONE',  #128718 ) ;
#119643 = CARTESIAN_POINT ( 'NONE',  ( 27.64169371712955936, -2.130196079827424871, -7.949999999999999289 ) ) ;
#119644 = AXIS2_PLACEMENT_3D ( 'NONE', #124921, #13277, #24886 ) ;
#119645 = DIRECTION ( 'NONE',  ( 0.7071067811865487940, 0.7071067811865463515, 0.000000000000000000 ) ) ;
#119646 = ADVANCED_FACE ( 'NONE', ( #1374 ), #64522, .F. ) ;
#119647 = ORIENTED_EDGE ( 'NONE', *, *, #62250, .F. ) ;
#119648 = EDGE_LOOP ( 'NONE', ( #77194, #126838, #59462, #43402, #85902 ) ) ;
#119649 = CARTESIAN_POINT ( 'NONE',  ( 25.93749999999998224, 5.819803920172573974, -5.819803920172572198 ) ) ;
#119650 = AXIS2_PLACEMENT_3D ( 'NONE', #98161, #42370, #62690 ) ;
#119651 = ORIENTED_EDGE ( 'NONE', *, *, #138569, .F. ) ;
#119652 = CARTESIAN_POINT ( 'NONE',  ( 17.06332250466817158, 4.584330080086930965E-16, 0.000000000000000000 ) ) ;
#119653 = CARTESIAN_POINT ( 'NONE',  ( 28.82816939922332722, 18.75929247661552424, 4.000000000000000000 ) ) ;
#119654 = LINE ( 'NONE', #132745, #131304 ) ;
#119655 = PLANE ( 'NONE',  #104770 ) ;
#119656 = LINE ( 'NONE', #20353, #106781 ) ;
#119657 = LINE ( 'NONE', #142183, #23315 ) ;
#119658 = CARTESIAN_POINT ( 'NONE',  ( 123.2870968585647944, 3.054999999999997495, 5.291415217122919401 ) ) ;
#119659 = EDGE_LOOP ( 'NONE', ( #39344, #35054, #73775, #4284 ) ) ;
#119660 = ORIENTED_EDGE ( 'NONE', *, *, #30482, .T. ) ;
#119661 = CARTESIAN_POINT ( 'NONE',  ( 0.000000000000000000, 0.000000000000000000, 5.000000000000000000 ) ) ;
#119662 = CARTESIAN_POINT ( 'NONE',  ( 25.65999999999999659, 9.521314400968980422E-16, 0.000000000000000000 ) ) ;
#119663 = LINE ( 'NONE', #57162, #92991 ) ;
#119664 = DIRECTION ( 'NONE',  ( -0.3543493200069162685, -0.000000000000000000, -0.9351131265310288487 ) ) ;
#119665 = VERTEX_POINT ( 'NONE', #55087 ) ;
#119666 = CONICAL_SURFACE ( 'NONE', #96483, 2.055000000000000604, 0.9599310885968764806 ) ;
#119667 = CARTESIAN_POINT ( 'NONE',  ( 47.68793019189809712, 6.110000000000002984, -1.637169565754156730 ) ) ;
#119668 = ORIENTED_EDGE ( 'NONE', *, *, #142972, .T. ) ;
#119669 = DIRECTION ( 'NONE',  ( -0.7071067811865486830, -0.7071067811865464625, 0.000000000000000000 ) ) ;
#119670 = DIRECTION ( 'NONE',  ( 0.5735764363510448272, -0.8191520442889927978, 1.003171929053526103E-16 ) ) ;
#119671 = CARTESIAN_POINT ( 'NONE',  ( 108.2875270504628986, 0.000000000000000000, -7.949999999999998401 ) ) ;
#119672 = VECTOR ( 'NONE', #68416, 1000.000000000000000 ) ;
#119673 = AXIS2_PLACEMENT_3D ( 'NONE', #29811, #105244, #62468 ) ;
#119674 = CARTESIAN_POINT ( 'NONE',  ( 35.64126352523145158, 4.472830434245836706, 4.472830434245840259 ) ) ;
#119675 = EDGE_LOOP ( 'NONE', ( #46436, #68189, #60157, #42587 ) ) ;
#119676 = VECTOR ( 'NONE', #86888, 1000.000000000000000 ) ;
#119677 = DIRECTION ( 'NONE',  ( -0.000000000000000000, -1.000000000000000000, -0.000000000000000000 ) ) ;
#119679 = EDGE_CURVE ( 'NONE', #136567, #58719, #122453, .T. ) ;
#119678 = VERTEX_POINT ( 'NONE', #9385 ) ;
#119680 = ORIENTED_EDGE ( 'NONE', *, *, #11227, .T. ) ;
#119681 = COLOUR_RGB ( '', 0.31764706, 0.68627451, 0.89019608) ;
#119682 = EDGE_LOOP ( 'NONE', ( #77665, #4489, #72636, #107774 ) ) ;
#119683 = CARTESIAN_POINT ( 'NONE',  ( 79.41252705046289861, -7.949999999999998401, -4.867971026610728450E-16 ) ) ;
#119684 = ORIENTED_EDGE ( 'NONE', *, *, #130466, .F. ) ;
#119685 = DIRECTION ( 'NONE',  ( -1.000000000000000000, -1.224606353822377258E-16, -0.000000000000000000 ) ) ;
#119686 = PLANE ( 'NONE',  #84896 ) ;
#119687 = CARTESIAN_POINT ( 'NONE',  ( 14.29289321881335439, 20.25929247661551713, 5.000000000000000000 ) ) ;
#119688 = CARTESIAN_POINT ( 'NONE',  ( 26.67183060077628198, -21.74070752338406365, 4.000000000000000000 ) ) ;
#119689 = EDGE_CURVE ( 'NONE', #17718, #123774, #76862, .T. ) ;
#119690 = FACE_BOUND ( 'NONE', #77259, .T. ) ;
#119691 = ORIENTED_EDGE ( 'NONE', *, *, #125635, .T. ) ;
#119692 = DIRECTION ( 'NONE',  ( 0.000000000000000000, 0.000000000000000000, -1.000000000000000000 ) ) ;
#119693 = EDGE_CURVE ( 'NONE', #35104, #108780, #142797, .T. ) ;
#119694 = ADVANCED_FACE ( 'NONE', ( #44968 ), #42797, .F. ) ;
#119695 = DIRECTION ( 'NONE',  ( -1.000000000000000000, -1.224606353822377258E-16, -0.000000000000000000 ) ) ;
#119696 = CARTESIAN_POINT ( 'NONE',  ( -13.49999999999991118, -2.568876922607790103, 4.000000000000000000 ) ) ;
#119697 = VERTEX_POINT ( 'NONE', #131210 ) ;
#119698 = CARTESIAN_POINT ( 'NONE',  ( -21.12147316337133773, -20.24070752338407786, 7.412974875817839759 ) ) ;
#119699 = ORIENTED_EDGE ( 'NONE', *, *, #22328, .F. ) ;
#119700 = VECTOR ( 'NONE', #55234, 1000.000000000000000 ) ;
#119701 = VERTEX_POINT ( 'NONE', #131939 ) ;
#119702 = DIRECTION ( 'NONE',  ( -0.7071067811865486830, 0.7071067811865464625, 0.000000000000000000 ) ) ;
#119703 = ORIENTED_EDGE ( 'NONE', *, *, #132401, .T. ) ;
#119704 = EDGE_CURVE ( 'NONE', #132626, #76656, #107579, .T. ) ;
#119705 = ADVANCED_FACE ( 'NONE', ( #110147 ), #676, .F. ) ;
#119706 = CARTESIAN_POINT ( 'NONE',  ( 54.01626352523144448, -4.472830434245838482, 4.472830434245838482 ) ) ;
#119707 = DIRECTION ( 'NONE',  ( -0.6830127018922181881, 0.6830127018922202975, -0.2588190451025214056 ) ) ;
#119708 = VECTOR ( 'NONE', #60389, 1000.000000000000000 ) ;
#119709 = EDGE_LOOP ( 'NONE', ( #9667, #101517, #54700, #65049 ) ) ;
#119710 = LINE ( 'NONE', #63268, #74187 ) ;
#119711 = VERTEX_POINT ( 'NONE', #89144 ) ;
#119712 = LINE ( 'NONE', #142925, #24154 ) ;
#119713 = EDGE_CURVE ( 'NONE', #133506, #104226, #121035, .T. ) ;
#119714 = ORIENTED_EDGE ( 'NONE', *, *, #41148, .F. ) ;
#119715 = FACE_OUTER_BOUND ( 'NONE', #33978, .T. ) ;
#119716 = CARTESIAN_POINT ( 'NONE',  ( -8.999999999999937828, -0.2811185226894407085, -5.995736974527494212 ) ) ;
#119717 = VECTOR ( 'NONE', #38226, 1000.000000000000000 ) ;
#119718 = EDGE_CURVE ( 'NONE', #60604, #59118, #34057, .T. ) ;
#119719 = CARTESIAN_POINT ( 'NONE',  ( -0.005480084712502889671, 28.92564299267938210, 4.000000000000000000 ) ) ;
#119720 = CARTESIAN_POINT ( 'NONE',  ( 23.99999999999982947, 10.21212019023810846, -2.019456568337855362 ) ) ;
#119721 = CARTESIAN_POINT ( 'NONE',  ( 18.18398860626898994, 28.73617430169800002, 5.000000000000000000 ) ) ;
#119722 = DIRECTION ( 'NONE',  ( -0.7071067811865486830, -0.7071067811865464625, 0.000000000000000000 ) ) ;
#119723 = PLANE ( 'NONE',  #64969 ) ;
#119724 = ORIENTED_EDGE ( 'NONE', *, *, #134001, .F. ) ;
#119725 = AXIS2_PLACEMENT_3D ( 'NONE', #89874, #80465, #34809 ) ;
#119726 = ORIENTED_EDGE ( 'NONE', *, *, #99595, .T. ) ;
#119727 = VERTEX_POINT ( 'NONE', #35505 ) ;
#119728 = CARTESIAN_POINT ( 'NONE',  ( 18.85830628287044419, -1.633150327867709528, 6.094999999999979323 ) ) ;
#119729 = DIRECTION ( 'NONE',  ( -0.7071067811865486830, 0.7071067811865464625, 0.000000000000000000 ) ) ;
#119730 = ORIENTED_EDGE ( 'NONE', *, *, #52021, .F. ) ;
#119731 = EDGE_LOOP ( 'NONE', ( #107996, #112328, #108195, #122969 ) ) ;
#119732 = CARTESIAN_POINT ( 'NONE',  ( 9.707106781186482181, -6.740707523384216415, 5.000000000000000000 ) ) ;
#119733 = DIRECTION ( 'NONE',  ( 0.7071067811865486830, -0.7071067811865464625, -0.000000000000000000 ) ) ;
#119734 = VECTOR ( 'NONE', #35443, 1000.000000000000227 ) ;
#119735 = DIRECTION ( 'NONE',  ( -0.3543493200069162685, -0.000000000000000000, -0.9351131265310288487 ) ) ;
#119736 = EDGE_LOOP ( 'NONE', ( #19283, #6309, #61731 ) ) ;
#119737 = LINE ( 'NONE', #63295, #125028 ) ;
#119738 = EDGE_CURVE ( 'NONE', #103456, #38684, #93410, .T. ) ;
#119739 = DIRECTION ( 'NONE',  ( 0.7071067811865487940, 0.7071067811865463515, 0.000000000000000000 ) ) ;
#119740 = CARTESIAN_POINT ( 'NONE',  ( 20.19206980810188767, -7.934999999999991616, -2.126176841940955242 ) ) ;
#119741 = CARTESIAN_POINT ( 'NONE',  ( 3.299744871391591339, -27.71228299555208352, 4.000000000000000000 ) ) ;
#119742 = ORIENTED_EDGE ( 'NONE', *, *, #97396, .T. ) ;
#119743 = CARTESIAN_POINT ( 'NONE',  ( 121.9745968585647802, 1.637169565754164280, -6.109999999999997655 ) ) ;
#119744 = VECTOR ( 'NONE', #95831, 999.9999999999998863 ) ;
#119745 = AXIS2_PLACEMENT_3D ( 'NONE', #81185, #49981, #71028 ) ;
#119746 = CARTESIAN_POINT ( 'NONE',  ( 7.720000000000001528, -2.055000000000000160, 2.789133085058098087E-16 ) ) ;
#119747 = EDGE_CURVE ( 'NONE', #98330, #95580, #79738, .T. ) ;
#119748 = CARTESIAN_POINT ( 'NONE',  ( -9.183988606268997046, 28.73617430169793607, 5.000000000000000000 ) ) ;
#119750 = VERTEX_POINT ( 'NONE', #136912 ) ;
#119749 = FACE_OUTER_BOUND ( 'NONE', #135480, .T. ) ;
#119751 = CARTESIAN_POINT ( 'NONE',  ( 66.72502705046288440, 5.819803920172573974, -5.819803920172573086 ) ) ;
#119752 = ORIENTED_EDGE ( 'NONE', *, *, #130114, .F. ) ;
#119753 = CARTESIAN_POINT ( 'NONE',  ( -12.48921356237309155, -27.52281430457064104, 5.000000000000000000 ) ) ;
#119754 = DIRECTION ( 'NONE',  ( -0.000000000000000000, 0.000000000000000000, 1.000000000000000000 ) ) ;
#119755 = CARTESIAN_POINT ( 'NONE',  ( -48.29974487139158867, -27.71228299555239971, 4.000000000000000000 ) ) ;
#119756 = VERTEX_POINT ( 'NONE', #38324 ) ;
#119757 = EDGE_CURVE ( 'NONE', #60486, #2943, #114440, .T. ) ;
#119758 = AXIS2_PLACEMENT_3D ( 'NONE', #40182, #5347, #6043 ) ;
#119759 = EDGE_CURVE ( 'NONE', #53860, #101990, #47114, .T. ) ;
#119760 = CARTESIAN_POINT ( 'NONE',  ( -28.49999999999979750, 15.05218569542901186, 5.000000000000000000 ) ) ;
#119761 = LINE ( 'NONE', #43660, #93049 ) ;
#119762 = ORIENTED_EDGE ( 'NONE', *, *, #8486, .T. ) ;
#119763 = DIRECTION ( 'NONE',  ( -1.000000000000000000, -0.000000000000000000, -0.000000000000000000 ) ) ;
#119764 = VECTOR ( 'NONE', #22219, 999.9999999999998863 ) ;
#119766 = EDGE_CURVE ( 'NONE', #107904, #28826, #123922, .T. ) ;
#119765 = DIRECTION ( 'NONE',  ( -0.7071067811865486830, 0.7071067811865464625, 0.000000000000000000 ) ) ;
#119767 = ORIENTED_EDGE ( 'NONE', *, *, #44136, .T. ) ;
#119768 = CARTESIAN_POINT ( 'NONE',  ( 4.083333333333333925, -5.278424836066144543, 3.047499999999995879 ) ) ;
#119769 = VECTOR ( 'NONE', #113468, 1000.000000000000000 ) ;
#119770 = DIRECTION ( 'NONE',  ( 0.000000000000000000, 0.000000000000000000, 1.000000000000000000 ) ) ;
#119771 = ORIENTED_EDGE ( 'NONE', *, *, #96276, .F. ) ;
#119772 = EDGE_LOOP ( 'NONE', ( #30585, #106954, #117060, #39203 ) ) ;
#119773 = LINE ( 'NONE', #76314, #28764 ) ;
#119774 = LINE ( 'NONE', #108899, #69131 ) ;
#119775 = AXIS2_PLACEMENT_3D ( 'NONE', #97045, #96341, #118097 ) ;
#119776 = VECTOR ( 'NONE', #115051, 1000.000000000000000 ) ;
#119777 = DIRECTION ( 'NONE',  ( 0.7071067811865486830, -0.7071067811865464625, -0.000000000000000000 ) ) ;
#119778 = AXIS2_PLACEMENT_3D ( 'NONE', #95066, #52283, #126980 ) ;
#119779 = CARTESIAN_POINT ( 'NONE',  ( -26.51078643762690845, -27.52281430457036748, 5.000000000000000000 ) ) ;
#119780 = DIRECTION ( 'NONE',  ( 0.7071067811865487940, 0.7071067811865463515, 0.000000000000000000 ) ) ;
#119781 = ORIENTED_EDGE ( 'NONE', *, *, #66822, .F. ) ;
#119782 = ADVANCED_FACE ( 'NONE', ( #36191 ), #82539, .T. ) ;
#119783 = SURFACE_STYLE_FILL_AREA ( #53109 ) ;
#119784 = DIRECTION ( 'NONE',  ( 0.7071067811865486830, -0.7071067811865464625, -0.000000000000000000 ) ) ;
#119785 = CARTESIAN_POINT ( 'NONE',  ( 36.18398860626899705, 28.73617430169812437, 5.000000000000000000 ) ) ;
#119786 = VECTOR ( 'NONE', #89053, 1000.000000000000000 ) ;
#119787 = DIRECTION ( 'NONE',  ( 0.7071067811865487940, 0.7071067811865463515, -0.000000000000000000 ) ) ;
#119788 = CARTESIAN_POINT ( 'NONE',  ( 33.30793019189810877, -6.109999999999999432, 1.637169565754158507 ) ) ;
#119789 = DIRECTION ( 'NONE',  ( -0.7071067811865487940, 0.7071067811865463515, -0.000000000000000000 ) ) ;
#119790 = ORIENTED_EDGE ( 'NONE', *, *, #107205, .F. ) ;
#119791 = ORIENTED_EDGE ( 'NONE', *, *, #31102, .F. ) ;
#119792 = CARTESIAN_POINT ( 'NONE',  ( -18.71230993966015177, -21.73547319004781286, 4.999917730833664642 ) ) ;
#119793 = ADVANCED_FACE ( 'NONE', ( #135506 ), #14425, .F. ) ;
#119794 = ORIENTED_EDGE ( 'NONE', *, *, #24690, .T. ) ;
#119795 = VERTEX_POINT ( 'NONE', #70285 ) ;
#119796 = LINE ( 'NONE', #19790, #126570 ) ;
#119797 = DIRECTION ( 'NONE',  ( -0.000000000000000000, -0.3543493200069152693, 0.9351131265310292928 ) ) ;
#119798 = ORIENTED_EDGE ( 'NONE', *, *, #95639, .T. ) ;
#119799 = CARTESIAN_POINT ( 'NONE',  ( -17.57538274164440040, -2.608983483842240325, 5.000000000000000000 ) ) ;
#119800 = CARTESIAN_POINT ( 'NONE',  ( -14.99999999999989164, -15.41253812416060143, 4.000000000000000000 ) ) ;
#119801 = DIRECTION ( 'NONE',  ( -0.000000000000000000, -0.3543493200069152693, 0.9351131265310292928 ) ) ;
#119802 = EDGE_CURVE ( 'NONE', #54989, #9815, #60086, .T. ) ;
#119803 = FACE_OUTER_BOUND ( 'NONE', #120433, .T. ) ;
#119804 = CARTESIAN_POINT ( 'NONE',  ( 127.4587635252314470, 0.000000000000000000, -6.110000000000001208 ) ) ;
#119805 = VERTEX_POINT ( 'NONE', #81127 ) ;
#119806 = DIRECTION ( 'NONE',  ( -0.7071067811865486830, -0.7071067811865464625, 0.000000000000000000 ) ) ;
#119807 = FACE_OUTER_BOUND ( 'NONE', #43432, .T. ) ;
#119808 = AXIS2_PLACEMENT_3D ( 'NONE', #79352, #25621, #3152 ) ;
#119809 = FACE_OUTER_BOUND ( 'NONE', #61362, .T. ) ;
#119810 = CARTESIAN_POINT ( 'NONE',  ( 0.000000000000000000, -60.00000000000000000, 0.000000000000000000 ) ) ;
#119811 = CARTESIAN_POINT ( 'NONE',  ( 32.20710678118632586, -14.24070752338414181, 5.000000000000000000 ) ) ;
#119812 = LINE ( 'NONE', #163, #14409 ) ;
#119813 = CARTESIAN_POINT ( 'NONE',  ( -39.48921356237310221, -27.52281430457082934, 5.000000000000000000 ) ) ;
#119814 = CARTESIAN_POINT ( 'NONE',  ( 58.26669371712954870, -7.949999999999999289, 2.130196079827424427 ) ) ;
#119815 = EDGE_CURVE ( 'NONE', #133491, #107648, #101425, .T. ) ;
#119816 = PLANE ( 'NONE',  #97006 ) ;
#119817 = ORIENTED_EDGE ( 'NONE', *, *, #79802, .T. ) ;
#119818 = ORIENTED_EDGE ( 'NONE', *, *, #87534, .T. ) ;
#119819 = CARTESIAN_POINT ( 'NONE',  ( 51.89583333333332860, -2.130196079827427091, 7.949999999999999289 ) ) ;
#119820 = PLANE ( 'NONE',  #118792 ) ;
#119821 = DIRECTION ( 'NONE',  ( 0.3543493200069162685, -0.000000000000000000, -0.9351131265310288487 ) ) ;
#119822 = CARTESIAN_POINT ( 'NONE',  ( 20.29320749275913371, 20.25929247661551358, 20.83292124670810352 ) ) ;
#119823 = ORIENTED_EDGE ( 'NONE', *, *, #80568, .T. ) ;
#119824 = CARTESIAN_POINT ( 'NONE',  ( -33.32816939922329880, -6.740707523384212863, 4.000000000000000000 ) ) ;
#119825 =( BOUNDED_CURVE ( )  B_SPLINE_CURVE ( 3, ( #91776, #34558, #69335, #101948 ),
 .UNSPECIFIED., .F., .F. ) 
 B_SPLINE_CURVE_WITH_KNOTS ( ( 4, 4 ),
 ( 1.964434688349490754, 3.503810798801452187 ),
 .UNSPECIFIED. ) 
 CURVE ( )  GEOMETRIC_REPRESENTATION_ITEM ( )  RATIONAL_B_SPLINE_CURVE ( ( 1.000000000000000000, 0.8120851936182287290, 0.8120851936182287290, 1.000000000000000000 ) ) 
 REPRESENTATION_ITEM ( '' )  );
#119826 = CARTESIAN_POINT ( 'NONE',  ( 75.29974487139158157, -27.71228299555258445, 4.000000000000000000 ) ) ;
#119827 = EDGE_CURVE ( 'NONE', #60723, #68187, #80420, .T. ) ;
#119828 = CARTESIAN_POINT ( 'NONE',  ( 51.77126352523143993, 4.472830434245839371, 4.472830434245842035 ) ) ;
#119829 = ORIENTED_EDGE ( 'NONE', *, *, #54508, .T. ) ;
#119830 = EDGE_LOOP ( 'NONE', ( #35891, #82490, #129419, #211 ) ) ;
#119831 = ORIENTED_EDGE ( 'NONE', *, *, #36040, .T. ) ;
#119832 = DIRECTION ( 'NONE',  ( -0.7071067811865486830, -0.7071067811865464625, 0.000000000000000000 ) ) ;
#119833 = CARTESIAN_POINT ( 'NONE',  ( 26.99999999999981526, 4.552185695429121104, 5.000000000000000000 ) ) ;
#119834 = CARTESIAN_POINT ( 'NONE',  ( -33.32816939922329880, 17.25929247661554200, 4.000000000000000000 ) ) ;
#119835 = CYLINDRICAL_SURFACE ( 'NONE', #23123, 6.094999999999989093 ) ;
#119836 = ORIENTED_EDGE ( 'NONE', *, *, #107384, .T. ) ;
#119837 = EDGE_CURVE ( 'NONE', #489, #72622, #58704, .T. ) ;
#119838 = DIRECTION ( 'NONE',  ( 0.6830127018922181881, 0.6830127018922202975, -0.2588190451025214056 ) ) ;
#119840 = ORIENTED_EDGE ( 'NONE', *, *, #64471, .F. ) ;
#119839 = FACE_OUTER_BOUND ( 'NONE', #48423, .T. ) ;
#119841 = CARTESIAN_POINT ( 'NONE',  ( 80.79209685856477563, -5.291415217122921177, 3.054999999999999272 ) ) ;
#119842 = LINE ( 'NONE', #87253, #97113 ) ;
#119843 = DIRECTION ( 'NONE',  ( 0.000000000000000000, -1.000000000000000000, 0.000000000000000000 ) ) ;
#119844 = CARTESIAN_POINT ( 'NONE',  ( 24.09999999999999787, -2.055000000000000160, 2.789133085058098087E-16 ) ) ;
#119845 = VERTEX_POINT ( 'NONE', #124609 ) ;
#119846 = VECTOR ( 'NONE', #25772, 1000.000000000000000 ) ;
#119847 = FILL_AREA_STYLE ('',( #141650 ) ) ;
#119848 = CARTESIAN_POINT ( 'NONE',  ( 68.16209685856478018, -5.291415217122919401, 3.054999999999997939 ) ) ;
#119849 = DIRECTION ( 'NONE',  ( -0.7071067811865486830, -0.7071067811865464625, 0.000000000000000000 ) ) ;
#119850 = CARTESIAN_POINT ( 'NONE',  ( -27.70701326429286127, -21.74070752338406365, 4.999753212805221558 ) ) ;
#119851 = PLANE ( 'NONE',  #31645 ) ;
#119852 = ORIENTED_EDGE ( 'NONE', *, *, #19840, .T. ) ;
#119853 = EDGE_LOOP ( 'NONE', ( #53524, #103264, #130425, #106664 ) ) ;
#119854 = CARTESIAN_POINT ( 'NONE',  ( 25.39999999999999858, -30.18000000000009564, -12.70000000000045404 ) ) ;
#119855 = DIRECTION ( 'NONE',  ( 0.000000000000000000, 0.000000000000000000, 1.000000000000000000 ) ) ;
#119856 = EDGE_LOOP ( 'NONE', ( #54569, #47611, #27932, #131946, #46646, #30122, #108651, #133782 ) ) ;
#119857 = ORIENTED_EDGE ( 'NONE', *, *, #28321, .F. ) ;
#119858 = VECTOR ( 'NONE', #123454, 1000.000000000000000 ) ;
#119859 = CARTESIAN_POINT ( 'NONE',  ( 11.93159235450332112, 2.500000000000001776, 0.000000000000000000 ) ) ;
#119860 = ORIENTED_EDGE ( 'NONE', *, *, #61142, .T. ) ;
#119861 = CARTESIAN_POINT ( 'NONE',  ( 0.000000000000000000, -7.600000000000061817, 31.92499999999998295 ) ) ;
#119862 = ADVANCED_FACE ( 'NONE', ( #90571 ), #46386, .F. ) ;
#119863 = DIRECTION ( 'NONE',  ( 0.6830127018922181881, 0.6830127018922202975, -0.2588190451025214056 ) ) ;
#119864 = VECTOR ( 'NONE', #69168, 999.9999999999998863 ) ;
#119865 = FACE_OUTER_BOUND ( 'NONE', #83601, .T. ) ;
#119866 = AXIS2_PLACEMENT_3D ( 'NONE', #141674, #120592, #54671 ) ;
#119867 = FACE_BOUND ( 'NONE', #56567, .T. ) ;
#119868 = EDGE_CURVE ( 'NONE', #103662, #28826, #47803, .T. ) ;
#119869 = CARTESIAN_POINT ( 'NONE',  ( 19.05000000000000071, 3.174999999999997158, 4.000000000000000000 ) ) ;
#119870 = PLANE ( 'NONE',  #73464 ) ;
#119872 = ORIENTED_EDGE ( 'NONE', *, *, #33578, .F. ) ;
#119871 = CARTESIAN_POINT ( 'NONE',  ( 9.489213562373095101, -27.52281430457062328, 5.000000000000000000 ) ) ;
#119873 = AXIS2_PLACEMENT_3D ( 'NONE', #127051, #27743, #52350 ) ;
#119874 = AXIS2_PLACEMENT_3D ( 'NONE', #53032, #6640, #63260 ) ;
#119875 = ORIENTED_EDGE ( 'NONE', *, *, #1413, .T. ) ;
#119876 = EDGE_CURVE ( 'NONE', #38905, #134825, #113006, .T. ) ;
#119877 = EDGE_CURVE ( 'NONE', #64329, #110885, #91977, .T. ) ;
#119878 = ORIENTED_EDGE ( 'NONE', *, *, #27472, .T. ) ;
#119879 = CARTESIAN_POINT ( 'NONE',  ( 80.84959685856478018, 6.109999999999996767, 1.637169565754163836 ) ) ;
#119880 = EDGE_LOOP ( 'NONE', ( #22173, #60551, #59679, #10103, #105776, #97700 ) ) ;
#119881 = PLANE ( 'NONE',  #24505 ) ;
#119882 = EDGE_CURVE ( 'NONE', #80880, #58909, #103545, .T. ) ;
#119883 = FACE_OUTER_BOUND ( 'NONE', #70754, .T. ) ;
#119884 = ADVANCED_FACE ( 'NONE', ( #48473 ), #15790, .F. ) ;
#119885 = ORIENTED_EDGE ( 'NONE', *, *, #40496, .F. ) ;
#119886 = DIRECTION ( 'NONE',  ( 0.7071067811865487940, -0.7071067811865463515, 0.000000000000000000 ) ) ;
#119887 = EDGE_CURVE ( 'NONE', #32826, #115089, #52054, .T. ) ;
#119888 = DIRECTION ( 'NONE',  ( -1.000000000000000000, -0.000000000000000000, -0.000000000000000000 ) ) ;
#119889 = LINE ( 'NONE', #8269, #39182 ) ;
#119890 = EDGE_CURVE ( 'NONE', #115328, #125503, #47440, .T. ) ;
#119891 = FACE_OUTER_BOUND ( 'NONE', #5224, .T. ) ;
#119892 = DIRECTION ( 'NONE',  ( 0.7071067811865487940, -0.7071067811865463515, 0.000000000000000000 ) ) ;
#119893 = CARTESIAN_POINT ( 'NONE',  ( 8.999999999999937828, 5.587461875839188075, 4.000000000000000000 ) ) ;
#119894 = CARTESIAN_POINT ( 'NONE',  ( 13.29826936130429260, 3.821174125832445049E-16, 0.000000000000000000 ) ) ;
#119895 = ORIENTED_EDGE ( 'NONE', *, *, #131351, .T. ) ;
#119896 = LINE ( 'NONE', #96709, #19115 ) ;
#119897 = VERTEX_POINT ( 'NONE', #115835 ) ;
#119898 = DIRECTION ( 'NONE',  ( -0.7071067811865487940, 0.7071067811865463515, 0.000000000000000000 ) ) ;
#119899 = CARTESIAN_POINT ( 'NONE',  ( 12.86840764549667604, -2.500000000000000888, 0.000000000000000000 ) ) ;
#119900 = EDGE_CURVE ( 'NONE', #30706, #55488, #6344, .T. ) ;
#119901 = ORIENTED_EDGE ( 'NONE', *, *, #83819, .T. ) ;
#119902 = VERTEX_POINT ( 'NONE', #39770 ) ;
#119903 = ORIENTED_EDGE ( 'NONE', *, *, #102563, .T. ) ;
#119904 = CARTESIAN_POINT ( 'NONE',  ( 39.95876352523143282, 0.000000000000000000, -6.110000000000001208 ) ) ;
#119905 = VECTOR ( 'NONE', #89957, 1000.000000000000227 ) ;
#119906 = EDGE_LOOP ( 'NONE', ( #12757, #59178, #39069, #42613 ) ) ;
#119907 = CARTESIAN_POINT ( 'NONE',  ( 2.999999999999985345, -12.03360074219761877, 5.000000000000000000 ) ) ;
#119908 = EDGE_CURVE ( 'NONE', #76199, #138835, #71668, .T. ) ;
#119909 = PLANE ( 'NONE',  #35477 ) ;
#119910 = CARTESIAN_POINT ( 'NONE',  ( 20.89997294953711204, 4.461849672132297329, -4.461849672132302658 ) ) ;
#119911 = CARTESIAN_POINT ( 'NONE',  ( 8.807295529226077946, 11.91728907476091237, -25.70178564786368725 ) ) ;
#119912 = ORIENTED_EDGE ( 'NONE', *, *, #129122, .T. ) ;
#119913 = VERTEX_POINT ( 'NONE', #73799 ) ;
#119914 = CARTESIAN_POINT ( 'NONE',  ( 4.898587196589412829E-16, 60.00000000000000000, 4.000000000000000000 ) ) ;
#119915 = CARTESIAN_POINT ( 'NONE',  ( -10.22850677138658426, 20.25929247661551003, 7.808871592221746205 ) ) ;
#119916 = AXIS2_PLACEMENT_3D ( 'NONE', #119215, #19896, #98884 ) ;
#119918 = ORIENTED_EDGE ( 'NONE', *, *, #72367, .T. ) ;
#119917 = DIRECTION ( 'NONE',  ( 0.7071067811865486830, -0.7071067811865464625, -0.000000000000000000 ) ) ;
#119919 = ORIENTED_EDGE ( 'NONE', *, *, #133768, .T. ) ;
#119920 = LINE ( 'NONE', #87339, #119087 ) ;
#119921 = PLANE ( 'NONE',  #109320 ) ;
#119922 = ORIENTED_EDGE ( 'NONE', *, *, #14467, .F. ) ;
#119923 = CARTESIAN_POINT ( 'NONE',  ( 3.792893218813436551, 18.75929247661553489, 5.000000000000000000 ) ) ;
#119924 = VERTEX_POINT ( 'NONE', #105681 ) ;
#119925 = ORIENTED_EDGE ( 'NONE', *, *, #31276, .T. ) ;
#119926 = ORIENTED_EDGE ( 'NONE', *, *, #140222, .T. ) ;
#119927 = EDGE_CURVE ( 'NONE', #962, #44445, #50620, .T. ) ;
#119928 = PLANE ( 'NONE',  #70332 ) ;
#119929 = LINE ( 'NONE', #21373, #9314 ) ;
#119930 = CARTESIAN_POINT ( 'NONE',  ( -26.47234709111790707, 22.22500000000000142, 1.796973836066164898 ) ) ;
#119931 = EDGE_CURVE ( 'NONE', #109110, #98525, #83998, .T. ) ;
#119932 = DIRECTION ( 'NONE',  ( 0.3543493200069163240, -0.000000000000000000, 0.9351131265310288487 ) ) ;
#119933 = LINE ( 'NONE', #32259, #100373 ) ;
#119934 = DIRECTION ( 'NONE',  ( 0.000000000000000000, 0.000000000000000000, 1.000000000000000000 ) ) ;
#119935 = ORIENTED_EDGE ( 'NONE', *, *, #84472, .F. ) ;
#119936 = CARTESIAN_POINT ( 'NONE',  ( 97.05836038379621300, -7.949999999999996625, -2.130196079827426203 ) ) ;
#119937 = ORIENTED_EDGE ( 'NONE', *, *, #18450, .F. ) ;
#119938 = LINE ( 'NONE', #130882, #794 ) ;
#119939 = ADVANCED_FACE ( 'NONE', ( #27414 ), #39027, .F. ) ;
#119940 = CARTESIAN_POINT ( 'NONE',  ( 34.92499999999998295, 22.22500000000000142, 4.500000000000000888 ) ) ;
#119941 = ORIENTED_EDGE ( 'NONE', *, *, #2710, .T. ) ;
#119942 = FACE_OUTER_BOUND ( 'NONE', #6070, .T. ) ;
#119943 = VECTOR ( 'NONE', #101740, 1000.000000000000000 ) ;
#119944 = DIRECTION ( 'NONE',  ( 1.000000000000000000, 0.000000000000000000, 0.000000000000000000 ) ) ;
#119945 = ORIENTED_EDGE ( 'NONE', *, *, #31078, .T. ) ;
#119946 = ORIENTED_EDGE ( 'NONE', *, *, #131252, .F. ) ;
#119947 = EDGE_CURVE ( 'NONE', #31644, #117339, #116586, .T. ) ;
#119948 = DIRECTION ( 'NONE',  ( 1.000000000000000000, 0.000000000000000000, 0.000000000000000000 ) ) ;
#119949 = CARTESIAN_POINT ( 'NONE',  ( -29.22995720542185794, 21.73644205237998150, 5.000000000000000000 ) ) ;
#119950 = LINE ( 'NONE', #140316, #77091 ) ;
#119951 = CARTESIAN_POINT ( 'NONE',  ( 51.89583333333332860, -2.130196079827351596, 7.950000000000043698 ) ) ;
#119952 = CARTESIAN_POINT ( 'NONE',  ( 9.989119713460446803, -22.02621442084247505, 4.990779571109222879 ) ) ;
#119953 = CARTESIAN_POINT ( 'NONE',  ( 62.32876352523145158, 0.000000000000000000, -6.109999999999999432 ) ) ;
#119954 = CARTESIAN_POINT ( 'NONE',  ( 0.000000000000000000, 0.000000000000000000, 5.000000000000000000 ) ) ;
#119955 = DIRECTION ( 'NONE',  ( 0.7071067811865486830, -0.7071067811865464625, -0.000000000000000000 ) ) ;
#119956 = LINE ( 'NONE', #75098, #67288 ) ;
#119957 = CARTESIAN_POINT ( 'NONE',  ( 31.92500000000001492, -6.269999999999992468, -36.39086428169088094 ) ) ;
#119958 = ORIENTED_EDGE ( 'NONE', *, *, #105298, .F. ) ;
#119959 = PLANE ( 'NONE',  #127456 ) ;
#119960 = EDGE_LOOP ( 'NONE', ( #68257, #61554, #43672, #34071 ) ) ;
#119961 = CARTESIAN_POINT ( 'NONE',  ( 24.18398860626899705, 28.73617430169804265, 5.000000000000000000 ) ) ;
#119962 = DIRECTION ( 'NONE',  ( 0.7071067811865486830, -0.7071067811865464625, -0.000000000000000000 ) ) ;
#119963 = ORIENTED_EDGE ( 'NONE', *, *, #143392, .T. ) ;
#119964 = VECTOR ( 'NONE', #58471, 1000.000000000000000 ) ;
#119965 = CONICAL_SURFACE ( 'NONE', #34321, 2.055000000000001048, 0.9599310885968758145 ) ;
#119966 = CARTESIAN_POINT ( 'NONE',  ( 5.306730066903978305, -3.740707523384244837, 12.88036043432866329 ) ) ;
#119968 = EDGE_LOOP ( 'NONE', ( #83068, #4502 ) ) ;
#119967 = CARTESIAN_POINT ( 'NONE',  ( 45.29974487139158867, -27.71228299555237840, 4.000000000000000000 ) ) ;
#119969 = VECTOR ( 'NONE', #86754, 1000.000000000000000 ) ;
#119970 = CARTESIAN_POINT ( 'NONE',  ( 107.4583333333333428, 3.974999999999997424, 6.884901960086288852 ) ) ;
#119971 = EDGE_CURVE ( 'NONE', #58745, #13885, #128881, .T. ) ;
#119972 = CARTESIAN_POINT ( 'NONE',  ( -36.29974487139159578, -27.71228299555231445, 4.000000000000000000 ) ) ;
#119973 = LINE ( 'NONE', #64931, #119000 ) ;
#119974 = VERTEX_POINT ( 'NONE', #18674 ) ;
#119975 = ORIENTED_EDGE ( 'NONE', *, *, #6709, .T. ) ;
#119976 = DIRECTION ( 'NONE',  ( -0.7071067811865486830, -0.7071067811865464625, -0.000000000000000000 ) ) ;
#119977 = CARTESIAN_POINT ( 'NONE',  ( -36.18398860626899705, 28.73617430169812437, 5.000000000000000000 ) ) ;
#119978 = VECTOR ( 'NONE', #86239, 1000.000000000000000 ) ;
#119979 = LINE ( 'NONE', #139665, #75418 ) ;
#119980 = CARTESIAN_POINT ( 'NONE',  ( 85.53752705046288440, -9.735942053221456900E-16, 7.949999999999998401 ) ) ;
#119981 = DIRECTION ( 'NONE',  ( -0.7071067811865486830, 0.7071067811865464625, 0.000000000000000000 ) ) ;
#119982 = FACE_OUTER_BOUND ( 'NONE', #115493, .T. ) ;
#119983 = ORIENTED_EDGE ( 'NONE', *, *, #142324, .F. ) ;
#119984 = LINE ( 'NONE', #11220, #56250 ) ;
#119985 = CARTESIAN_POINT ( 'NONE',  ( 24.77004279457776548, 21.73644205237997795, 5.000000000000000000 ) ) ;
#119986 = CARTESIAN_POINT ( 'NONE',  ( 33.97916666666667851, 6.094999999999988205, -1.633150327867694651 ) ) ;
#119987 = VECTOR ( 'NONE', #110329, 1000.000000000000000 ) ;
#119988 = VERTEX_POINT ( 'NONE', #84677 ) ;
#119989 = ADVANCED_FACE ( 'NONE', ( #139066 ), #83251, .F. ) ;
#119990 = CARTESIAN_POINT ( 'NONE',  ( -11.99451991528749417, 28.92564299267946382, 4.000000000000000000 ) ) ;
#119991 = VERTEX_POINT ( 'NONE', #127458 ) ;
#119992 = AXIS2_PLACEMENT_3D ( 'NONE', #26588, #60692, #61408 ) ;
#119993 = EDGE_CURVE ( 'NONE', #27017, #56485, #72418, .T. ) ;
#119994 = CARTESIAN_POINT ( 'NONE',  ( 72.33376352523143282, 6.110000000000001208, 1.122388791418549305E-15 ) ) ;
#119995 = PRESENTATION_STYLE_ASSIGNMENT (( #31607 ) ) ;
#119996 = DIRECTION ( 'NONE',  ( -0.7071067811865486830, 0.7071067811865464625, 0.000000000000000000 ) ) ;
#119998 = ORIENTED_EDGE ( 'NONE', *, *, #84024, .T. ) ;
#119997 = AXIS2_PLACEMENT_3D ( 'NONE', #113039, #22448, #134846 ) ;
#119999 = DIRECTION ( 'NONE',  ( 0.000000000000000000, 1.000000000000000000, 0.000000000000000000 ) ) ;
#120000 = AXIS2_PLACEMENT_3D ( 'NONE', #62590, #61208, #140153 ) ;
#120001 = PLANE ( 'NONE',  #69747 ) ;
#120002 = COLOUR_RGB ( '', 0.08235294, 0.09019608, 0.10196078) ;
#120003 = CARTESIAN_POINT ( 'NONE',  ( 0.07735809023238590654, -0.3999999999999998002, -2.152165253127959144 ) ) ;
#120004 = EDGE_CURVE ( 'NONE', #36659, #143251, #65650, .T. ) ;
#120005 = CARTESIAN_POINT ( 'NONE',  ( -39.18398860626899705, 28.73617430169814568, 5.000000000000000000 ) ) ;
#120007 = VERTEX_POINT ( 'NONE', #43859 ) ;
#120006 = PLANE ( 'NONE',  #40632 ) ;
#120008 = DIRECTION ( 'NONE',  ( -0.7071067811865487940, 0.7071067811865463515, 0.000000000000000000 ) ) ;
#120009 = DIRECTION ( 'NONE',  ( -0.000000000000000000, 0.3543493200069153248, 0.9351131265310292928 ) ) ;
#120010 = DIRECTION ( 'NONE',  ( 0.6830127018922181881, 0.6830127018922202975, -0.2588190451025214056 ) ) ;
#120011 =( BOUNDED_CURVE ( )  B_SPLINE_CURVE ( 2, ( #45908, #90090, #135759, #69088, #34297, #134337, #114001, #92225, #135076, #35768, #91543, #13945, #102436 ),
 .UNSPECIFIED., .F., .T. ) 
 B_SPLINE_CURVE_WITH_KNOTS ( ( 3, 2, 2, 2, 2, 2, 3 ),
 ( 0.8499999999999999778, 0.8527777777777777457, 0.8555555555555555136, 0.8583333333333332815, 0.8611111111111111605, 0.8638888888888889284, 0.8666666666666666963 ),
 .UNSPECIFIED. ) 
 CURVE ( )  GEOMETRIC_REPRESENTATION_ITEM ( )  RATIONAL_B_SPLINE_CURVE ( ( 1.000000000000000000, 0.9659258262890683122, 1.000000000000000000, 0.9659258262890683122, 1.000000000000000000, 0.9659258262890683122, 1.000000000000000000, 0.9659258262890683122, 1.000000000000000000, 0.9659258262890683122, 1.000000000000000000, 0.9659258262890683122, 1.000000000000000000 ) ) 
 REPRESENTATION_ITEM ( '' )  );
#120012 = VERTEX_POINT ( 'NONE', #104988 ) ;
#120013 = ORIENTED_EDGE ( 'NONE', *, *, #137652, .T. ) ;
#120014 = CARTESIAN_POINT ( 'NONE',  ( 62.27126352523142572, 4.472830434245839371, 4.472830434245842035 ) ) ;
#120015 = ORIENTED_EDGE ( 'NONE', *, *, #9525, .T. ) ;
#120016 = PLANE ( 'NONE',  #84617 ) ;
#120017 = CARTESIAN_POINT ( 'NONE',  ( -17.84387692260746405, -22.22499999999999787, 4.000000000000000000 ) ) ;
#120018 = DIRECTION ( 'NONE',  ( -0.7071067811865487940, 0.7071067811865463515, -0.000000000000000000 ) ) ;
#120019 =( LENGTH_UNIT ( ) NAMED_UNIT ( * ) SI_UNIT ( .MILLI., .METRE. ) );
#120020 = EDGE_LOOP ( 'NONE', ( #85314, #43650, #48822, #56030 ) ) ;
#120021 = VECTOR ( 'NONE', #40142, 1000.000000000000000 ) ;
#120022 = FACE_OUTER_BOUND ( 'NONE', #26377, .T. ) ;
#120023 = CARTESIAN_POINT ( 'NONE',  ( -26.67183060077628198, 5.259292476615661016, 4.000000000000000000 ) ) ;
#120024 = VERTEX_POINT ( 'NONE', #5657 ) ;
#120025 = CARTESIAN_POINT ( 'NONE',  ( 18.70710678118642178, 20.25929247661551358, 5.000000000000000000 ) ) ;
#120026 = EDGE_CURVE ( 'NONE', #118799, #10438, #117970, .T. ) ;
#120027 = CARTESIAN_POINT ( 'NONE',  ( 1.146007053337370074, -0.3999999999999998002, -2.166563668000046405 ) ) ;
#120028 = CARTESIAN_POINT ( 'NONE',  ( -38.99451991528749062, 28.92564299267965211, 4.000000000000000000 ) ) ;
#120029 = ORIENTED_EDGE ( 'NONE', *, *, #138106, .T. ) ;
#120030 = ORIENTED_EDGE ( 'NONE', *, *, #95195, .F. ) ;
#120031 = FACE_BOUND ( 'NONE', #27332, .T. ) ;
#120032 = DIRECTION ( 'NONE',  ( 0.6830127018922180770, -0.6830127018922204085, -0.2588190451025213501 ) ) ;
#120033 = CARTESIAN_POINT ( 'NONE',  ( 13.82816939922343558, 21.75929247661549581, 4.000000000000000000 ) ) ;
#120034 = DIRECTION ( 'NONE',  ( 0.3543493200069162685, -0.000000000000000000, -0.9351131265310288487 ) ) ;
#120035 = CARTESIAN_POINT ( 'NONE',  ( -30.48921356237309510, -27.52281430457076894, 5.000000000000000000 ) ) ;
#120036 = CARTESIAN_POINT ( 'NONE',  ( -54.48921356237310221, -27.52281430457093236, 5.000000000000000000 ) ) ;
#120037 = ORIENTED_EDGE ( 'NONE', *, *, #133809, .F. ) ;
#120038 = ADVANCED_FACE ( 'NONE', ( #49926 ), #17271, .T. ) ;
#120039 = ORIENTED_EDGE ( 'NONE', *, *, #89629, .F. ) ;
#120040 = CARTESIAN_POINT ( 'NONE',  ( 112.4954301918981230, 5.291415217122916737, 3.055000000000001936 ) ) ;
#120041 = ORIENTED_EDGE ( 'NONE', *, *, #129034, .T. ) ;
#120042 = ADVANCED_FACE ( 'NONE', ( #17949 ), #139799, .F. ) ;
#120043 = ADVANCED_FACE ( 'NONE', ( #14055 ), #11914, .T. ) ;
#120044 = VERTEX_POINT ( 'NONE', #56200 ) ;
#120045 = ADVANCED_FACE ( 'NONE', ( #90946 ), #68233, .T. ) ;
#120046 =( LENGTH_UNIT ( ) NAMED_UNIT ( * ) SI_UNIT ( .MILLI., .METRE. ) );
#120047 = ADVANCED_FACE ( 'NONE', ( #67038 ), #78625, .T. ) ;
#120048 = DIRECTION ( 'NONE',  ( 0.5735764363510453823, -0.8191520442889923537, 1.003171929053525486E-16 ) ) ;
#120049 = CARTESIAN_POINT ( 'NONE',  ( 13.26601651615776767, 1.700382741644379081, 5.000000000000000000 ) ) ;
#120050 = ORIENTED_EDGE ( 'NONE', *, *, #94592, .F. ) ;
#120051 = CARTESIAN_POINT ( 'NONE',  ( 68.47502705046289861, -5.819803920172573086, 5.819803920172573086 ) ) ;
#120052 = FACE_OUTER_BOUND ( 'NONE', #115281, .T. ) ;
#120053 = EDGE_CURVE ( 'NONE', #17152, #65419, #77916, .T. ) ;
#120054 = LINE ( 'NONE', #9897, #41211 ) ;
#120055 = CARTESIAN_POINT ( 'NONE',  ( 2.044376628204111146, -6.094999999999989981, 0.4826247175876904327 ) ) ;
#120056 = VECTOR ( 'NONE', #63441, 1000.000000000000000 ) ;
#120057 = CIRCLE ( 'NONE', #15844, 25.00000000000002842 ) ;
#120058 = CARTESIAN_POINT ( 'NONE',  ( 1.499999999999990896, -8.947814304570737676, 5.000000000000000000 ) ) ;
#120059 = VECTOR ( 'NONE', #72532, 999.9999999999998863 ) ;
#120060 = VERTEX_POINT ( 'NONE', #111978 ) ;
#120061 = FACE_OUTER_BOUND ( 'NONE', #91157, .T. ) ;
#120062 = LINE ( 'NONE', #106335, #60513 ) ;
#120063 = COLOUR_RGB ( '', 0.40784314, 0.44705882, 0.49803922) ;
#120064 = ADVANCED_FACE ( 'NONE', ( #88802 ), #38168, .T. ) ;
#120065 = ORIENTED_EDGE ( 'NONE', *, *, #49724, .T. ) ;
#120066 = ORIENTED_EDGE ( 'NONE', *, *, #133756, .T. ) ;
#120067 = EDGE_CURVE ( 'NONE', #88880, #17476, #137235, .T. ) ;
#120068 = VERTEX_POINT ( 'NONE', #75824 ) ;
#120069 = CARTESIAN_POINT ( 'NONE',  ( 59.35459685856476142, -1.637169565754161615, 6.110000000000000320 ) ) ;
#120070 = AXIS2_PLACEMENT_3D ( 'NONE', #109248, #8463, #41138 ) ;
#120071 = ORIENTED_EDGE ( 'NONE', *, *, #115097, .T. ) ;
#120072 = VECTOR ( 'NONE', #129242, 1000.000000000000227 ) ;
#120073 = EDGE_CURVE ( 'NONE', #66020, #32821, #62817, .T. ) ;
#120074 = PLANE ( 'NONE',  #21189 ) ;
#120075 = CARTESIAN_POINT ( 'NONE',  ( -1.266693717129561136, -6.094999999999989981, -1.633150327867689100 ) ) ;
#120076 = CARTESIAN_POINT ( 'NONE',  ( 101.6462635252314328, -4.472830434245840259, 4.472830434245838482 ) ) ;
#120077 = CARTESIAN_POINT ( 'NONE',  ( 32.99451991528749062, 28.92564299267960948, 4.000000000000000000 ) ) ;
#120078 = DIRECTION ( 'NONE',  ( -0.7071067811865486830, -0.7071067811865464625, -0.000000000000000000 ) ) ;
#120079 = ORIENTED_EDGE ( 'NONE', *, *, #91387, .T. ) ;
#120080 = LINE ( 'NONE', #76646, #60319 ) ;
#120081 = AXIS2_PLACEMENT_3D ( 'NONE', #64373, #108543, #28893 ) ;
#120082 = VECTOR ( 'NONE', #96632, 1000.000000000000000 ) ;
#120083 = DIRECTION ( 'NONE',  ( 0.7071067811865487940, 0.7071067811865463515, 0.000000000000000000 ) ) ;
#120084 = CARTESIAN_POINT ( 'NONE',  ( 90.54166666666665719, -3.975000000000002753, 6.884901960086286188 ) ) ;
#120085 = PLANE ( 'NONE',  #47543 ) ;
#120086 = ORIENTED_EDGE ( 'NONE', *, *, #80816, .F. ) ;
#120087 = AXIS2_PLACEMENT_3D ( 'NONE', #141797, #119292, #42494 ) ;
#120088 = DIRECTION ( 'NONE',  ( 0.000000000000000000, 0.000000000000000000, 1.000000000000000000 ) ) ;
#120089 = EDGE_LOOP ( 'NONE', ( #29997, #48157, #21899, #100646 ) ) ;
#120090 = EDGE_LOOP ( 'NONE', ( #62643, #131020, #66049, #65393 ) ) ;
#120091 = ORIENTED_EDGE ( 'NONE', *, *, #72519, .F. ) ;
#120092 = EDGE_CURVE ( 'NONE', #78816, #42201, #64952, .T. ) ;
#120093 = CARTESIAN_POINT ( 'NONE',  ( 126.2037635252314658, 6.109999999999998543, 1.122388791418548911E-15 ) ) ;
#120094 = VECTOR ( 'NONE', #131974, 1000.000000000000000 ) ;
#120095 = ORIENTED_EDGE ( 'NONE', *, *, #72074, .T. ) ;
#120096 = VECTOR ( 'NONE', #95259, 1000.000000000000000 ) ;
#120097 = VECTOR ( 'NONE', #113565, 1000.000000000000000 ) ;
#120098 = LINE ( 'NONE', #20811, #2863 ) ;
#120099 = VECTOR ( 'NONE', #27257, 1000.000000000000000 ) ;
#120100 = LINE ( 'NONE', #96918, #25492 ) ;
#120101 = VERTEX_POINT ( 'NONE', #41040 ) ;
#120102 = CARTESIAN_POINT ( 'NONE',  ( -14.67183060077637080, -6.740707523384212863, 4.000000000000000000 ) ) ;
#120103 = ORIENTED_EDGE ( 'NONE', *, *, #135070, .F. ) ;
#120104 = VECTOR ( 'NONE', #36223, 1000.000000000000000 ) ;
#120105 = VECTOR ( 'NONE', #70079, 1000.000000000000227 ) ;
#120106 = EDGE_CURVE ( 'NONE', #20563, #98697, #40468, .T. ) ;
#120107 = CARTESIAN_POINT ( 'NONE',  ( 14.56206980810188334, -7.934999999999991616, -2.126176841940955242 ) ) ;
#120108 = SURFACE_STYLE_FILL_AREA ( #75934 ) ;
#120109 = LINE ( 'NONE', #88244, #106201 ) ;
#120110 = LINE ( 'NONE', #52047, #88334 ) ;
#120111 = ORIENTED_EDGE ( 'NONE', *, *, #90832, .T. ) ;
#120112 = ORIENTED_EDGE ( 'NONE', *, *, #14516, .F. ) ;
#120113 = ADVANCED_FACE ( 'NONE', ( #63545 ), #1077, .F. ) ;
#120114 = ORIENTED_EDGE ( 'NONE', *, *, #123288, .F. ) ;
#120115 = DIRECTION ( 'NONE',  ( -1.000000000000000000, -0.000000000000000000, -0.000000000000000000 ) ) ;
#120116 = CARTESIAN_POINT ( 'NONE',  ( 17.99451991528748351, 28.92564299267950645, 4.000000000000000000 ) ) ;
#120117 = PLANE ( 'NONE',  #54332 ) ;
#120118 = CARTESIAN_POINT ( 'NONE',  ( -1.828169399223514624, 9.759292476615625489, 4.000000000000000000 ) ) ;
#120119 = LINE ( 'NONE', #7807, #87361 ) ;
#120120 = PLANE ( 'NONE',  #83314 ) ;
#120121 = CARTESIAN_POINT ( 'NONE',  ( 27.27126352523142572, 4.472830434245839371, 4.472830434245842035 ) ) ;
#120122 = EDGE_CURVE ( 'NONE', #108649, #105081, #66377, .T. ) ;
#120123 = CARTESIAN_POINT ( 'NONE',  ( 0.000000000000000000, 0.000000000000000000, 5.000000000000000000 ) ) ;
#120124 = DIRECTION ( 'NONE',  ( -0.000000000000000000, -0.3543493200069152693, 0.9351131265310292928 ) ) ;
#120125 = ORIENTED_EDGE ( 'NONE', *, *, #122414, .F. ) ;
#120126 = CARTESIAN_POINT ( 'NONE',  ( 0.000000000000000000, 0.000000000000000000, 5.000000000000000000 ) ) ;
#120127 = EDGE_LOOP ( 'NONE', ( #36051, #138365, #1328, #121852 ) ) ;
#120128 = LINE ( 'NONE', #20841, #26795 ) ;
#120129 = ORIENTED_EDGE ( 'NONE', *, *, #130494, .F. ) ;
#120130 = DIRECTION ( 'NONE',  ( 1.000000000000000000, 0.000000000000000000, 0.000000000000000000 ) ) ;
#120132 = ORIENTED_EDGE ( 'NONE', *, *, #34003, .T. ) ;
#120131 = CARTESIAN_POINT ( 'NONE',  ( 43.00000000000000000, 0.000000000000000000, -7.950000000000000178 ) ) ;
#120133 = ADVANCED_FACE ( 'NONE', ( #10529 ), #77274, .F. ) ;
#120134 = LINE ( 'NONE', #91819, #6921 ) ;
#120135 = ADVANCED_FACE ( 'NONE', ( #43908 ), #122147, .F. ) ;
#120136 = ORIENTED_EDGE ( 'NONE', *, *, #77243, .T. ) ;
#120137 = CARTESIAN_POINT ( 'NONE',  ( 15.43680103220819788, -12.74070752338415602, 9.898150129686337451 ) ) ;
#120138 = EDGE_LOOP ( 'NONE', ( #107422, #70350, #3827, #14095 ) ) ;
#120139 = CARTESIAN_POINT ( 'NONE',  ( 11.20666063542144286, 21.75929247661549937, 4.998822639870701856 ) ) ;
#120140 = ORIENTED_EDGE ( 'NONE', *, *, #78552, .F. ) ;
#120141 = CARTESIAN_POINT ( 'NONE',  ( 93.70419371712957002, -6.884901960086285300, -3.975000000000000089 ) ) ;
#120142 = CARTESIAN_POINT ( 'NONE',  ( 115.5791937171295558, 3.975000000000002753, -6.884901960086283523 ) ) ;
#120143 = CARTESIAN_POINT ( 'NONE',  ( 5.999999999999956479, 7.007997736742450634, -8.085015511992098780 ) ) ;
#120144 = LINE ( 'NONE', #41927, #131953 ) ;
#120145 = CARTESIAN_POINT ( 'NONE',  ( 7.828169399223476432, -5.240707523384225297, 4.000000000000000000 ) ) ;
#120146 = DIRECTION ( 'NONE',  ( 0.000000000000000000, 0.000000000000000000, -1.000000000000000000 ) ) ;
#120147 = CARTESIAN_POINT ( 'NONE',  ( 22.49999999999984723, 9.052185695429077583, 5.000000000000000000 ) ) ;
#120148 = CARTESIAN_POINT ( 'NONE',  ( 5.104166666666667851, -1.633150327867691987, -6.094999999999989093 ) ) ;
#120149 = CARTESIAN_POINT ( 'NONE',  ( 19.37456980810188867, 6.871911579029510442, -3.967499999999998916 ) ) ;
#120150 = SURFACE_SIDE_STYLE ('',( #97725 ) ) ;
#120151 = DIRECTION ( 'NONE',  ( 0.7071067811865487940, 0.7071067811865463515, 0.000000000000000000 ) ) ;
#120152 = EDGE_LOOP ( 'NONE', ( #34813, #81076, #50840, #68318, #77938, #41278 ) ) ;
#120153 = VERTEX_POINT ( 'NONE', #45361 ) ;
#120154 = CARTESIAN_POINT ( 'NONE',  ( 34.42499999999998295, 22.22500000000000142, 5.000000000000000000 ) ) ;
#120155 = VERTEX_POINT ( 'NONE', #57654 ) ;
#120156 = B_SPLINE_CURVE_WITH_KNOTS ( 'NONE', 3,
 ( #140082, #109566, #97228, #65389, #62521, #106686, #10241, #117557, #86412, #63258, #30607, #7380 ),
 .UNSPECIFIED., .F., .F.,
 ( 4, 2, 2, 2, 2, 4 ),
 ( 0.000000000000000000, 0.001125297245559171450, 0.002250594491118342901, 0.002813243113897941853, 0.003375891736677540372, 0.004501188982236737843 ),
 .UNSPECIFIED. ) ;
#120157 = EDGE_CURVE ( 'NONE', #114421, #18107, #111269, .T. ) ;
#120158 = DIRECTION ( 'NONE',  ( 0.000000000000000000, -1.000000000000000000, 0.000000000000000000 ) ) ;
#120159 = CARTESIAN_POINT ( 'NONE',  ( -4.499999999999962697, -11.94781430457070215, 5.000000000000000000 ) ) ;
#120160 = CARTESIAN_POINT ( 'NONE',  ( 126.8009042512117333, -49.32595796886457862, -36.54674188582465888 ) ) ;
#120161 = ORIENTED_EDGE ( 'NONE', *, *, #118394, .F. ) ;
#120162 = VECTOR ( 'NONE', #2573, 1000.000000000000000 ) ;
#120163 = VECTOR ( 'NONE', #3926, 1000.000000000000000 ) ;
#120164 = DIRECTION ( 'NONE',  ( -1.000000000000000000, -4.431987436529789959E-15, 0.000000000000000000 ) ) ;
#120165 = DIRECTION ( 'NONE',  ( -0.7071067811865487940, 0.7071067811865463515, -0.000000000000000000 ) ) ;
#120166 = VECTOR ( 'NONE', #70747, 1000.000000000000000 ) ;
#120167 = FACE_OUTER_BOUND ( 'NONE', #74133, .T. ) ;
#120168 = EDGE_CURVE ( 'NONE', #20276, #93784, #1101, .T. ) ;
#120169 = EDGE_CURVE ( 'NONE', #94938, #30286, #99687, .T. ) ;
#120170 = CARTESIAN_POINT ( 'NONE',  ( -5.510786437626906675, -27.52281430457051314, 5.000000000000000000 ) ) ;
#120172 = EDGE_LOOP ( 'NONE', ( #70066, #58372, #89537, #40227 ) ) ;
#120171 = CARTESIAN_POINT ( 'NONE',  ( -1.499999999999984013, -1.533600742197719580, 5.000000000000000000 ) ) ;
#120173 = DIRECTION ( 'NONE',  ( -0.7071067811865487940, 0.7071067811865463515, 0.000000000000000000 ) ) ;
#120174 = CARTESIAN_POINT ( 'NONE',  ( 70.27083333333334281, -7.949999999999998401, -2.130196079827426203 ) ) ;
#120175 = DIRECTION ( 'NONE',  ( 0.000000000000000000, 0.000000000000000000, -1.000000000000000000 ) ) ;
#120176 = LINE ( 'NONE', #66564, #66441 ) ;
#120177 = AXIS2_PLACEMENT_3D ( 'NONE', #79208, #12464, #100905 ) ;
#120178 = DIRECTION ( 'NONE',  ( -1.000000000000000000, -1.224606353822377258E-16, -0.000000000000000000 ) ) ;
#120179 = VERTEX_POINT ( 'NONE', #11962 ) ;
#120180 = ORIENTED_EDGE ( 'NONE', *, *, #25324, .F. ) ;
#120181 = EDGE_LOOP ( 'NONE', ( #111753, #25967, #18543, #36892 ) ) ;
#120182 = CARTESIAN_POINT ( 'NONE',  ( 96.83376352523144703, 6.110000000000001208, 1.122388791418549305E-15 ) ) ;
#120183 = EDGE_LOOP ( 'NONE', ( #83071, #55908, #84540, #24088, #80859 ) ) ;
#120184 = CARTESIAN_POINT ( 'NONE',  ( 20.67183060077632817, -12.74070752338414891, 4.000000000000000000 ) ) ;
#120185 = AXIS2_PLACEMENT_3D ( 'NONE', #101998, #2661, #80971 ) ;
#120186 = VECTOR ( 'NONE', #98112, 1000.000000000000227 ) ;
#120187 = CARTESIAN_POINT ( 'NONE',  ( -8.510786437626906675, -27.52281430457049183, 5.000000000000000000 ) ) ;
#120188 = EDGE_LOOP ( 'NONE', ( #11072, #18561, #21851, #22199 ) ) ;
#120189 = EDGE_CURVE ( 'NONE', #8580, #41095, #112023, .T. ) ;
#120190 = CARTESIAN_POINT ( 'NONE',  ( -45.29974487139158867, -27.71228299555237840, 4.000000000000000000 ) ) ;
#120191 = CARTESIAN_POINT ( 'NONE',  ( 10.06000000000000050, -2.055000000000000160, 0.000000000000000000 ) ) ;
#120192 = VECTOR ( 'NONE', #66903, 1000.000000000000000 ) ;
#120193 = CARTESIAN_POINT ( 'NONE',  ( 89.16209685856478018, -5.291415217122919401, 3.054999999999997939 ) ) ;
#120194 = ORIENTED_EDGE ( 'NONE', *, *, #51149, .F. ) ;
#120195 = CARTESIAN_POINT ( 'NONE',  ( -30.18398860626900060, 28.73617430169808173, 5.000000000000000000 ) ) ;
#120196 = CARTESIAN_POINT ( 'NONE',  ( 115.0416666666666714, -3.975000000000002753, 6.884901960086286188 ) ) ;
#120197 = VECTOR ( 'NONE', #40733, 999.9999999999998863 ) ;
#120198 = VECTOR ( 'NONE', #96095, 1000.000000000000000 ) ;
#120199 = VECTOR ( 'NONE', #142477, 1000.000000000000000 ) ;
#120200 = ORIENTED_EDGE ( 'NONE', *, *, #32491, .T. ) ;
#120201 = VERTEX_POINT ( 'NONE', #121446 ) ;
#120202 = ORIENTED_EDGE ( 'NONE', *, *, #8080, .T. ) ;
#120203 = DIRECTION ( 'NONE',  ( 0.6830127018922181881, 0.6830127018922202975, -0.2588190451025214056 ) ) ;
#120204 = DIRECTION ( 'NONE',  ( -0.7071067811865486830, -0.7071067811865464625, 0.000000000000000000 ) ) ;
#120205 = DIRECTION ( 'NONE',  ( 0.7071067811865486830, -0.7071067811865464625, -0.000000000000000000 ) ) ;
#120206 = CIRCLE ( 'NONE', #78560, 3.000000000000000444 ) ;
#120207 = AXIS2_PLACEMENT_3D ( 'NONE', #133032, #141754, #30853 ) ;
#120208 = CARTESIAN_POINT ( 'NONE',  ( 166.8575281714868481, 26.96999999999994202, 31.92499999999998295 ) ) ;
#120209 = CARTESIAN_POINT ( 'NONE',  ( 31.49999999999977973, -8.568876922607721269, 4.000000000000000000 ) ) ;
#120210 = ADVANCED_FACE ( 'NONE', ( #98968 ), #143206, .F. ) ;
#120211 = VERTEX_POINT ( 'NONE', #32318 ) ;
#120212 = VERTEX_POINT ( 'NONE', #55502 ) ;
#120213 = EDGE_CURVE ( 'NONE', #6381, #11206, #1765, .T. ) ;
#120214 = CARTESIAN_POINT ( 'NONE',  ( 17.02886364525924989, -2.441401769420105339, 4.000000000000000000 ) ) ;
#120215 = ORIENTED_EDGE ( 'NONE', *, *, #42010, .F. ) ;
#120216 = ORIENTED_EDGE ( 'NONE', *, *, #92274, .F. ) ;
#120217 = VECTOR ( 'NONE', #85025, 1000.000000000000000 ) ;
#120218 = ADVANCED_FACE ( 'NONE', ( #78671 ), #122880, .F. ) ;
#120219 = ADVANCED_FACE ( 'NONE', ( #33761 ), #101841, .T. ) ;
#120220 = LINE ( 'NONE', #20932, #14980 ) ;
#120221 = ORIENTED_EDGE ( 'NONE', *, *, #61881, .F. ) ;
#120222 = LINE ( 'NONE', #20934, #36681 ) ;
#120223 = PLANE ( 'NONE',  #15418 ) ;
#120224 = CARTESIAN_POINT ( 'NONE',  ( -34.49999999999975131, 10.08746187583914100, 4.000000000000000000 ) ) ;
#120225 = ORIENTED_EDGE ( 'NONE', *, *, #11689, .T. ) ;
#120226 = EDGE_CURVE ( 'NONE', #14544, #136867, #44657, .T. ) ;
#120227 = ORIENTED_EDGE ( 'NONE', *, *, #43535, .F. ) ;
#120228 = CARTESIAN_POINT ( 'NONE',  ( 19.80737797471735107, -2.215184370838247929, -32.97705054010764769 ) ) ;
#120229 = ORIENTED_EDGE ( 'NONE', *, *, #51129, .F. ) ;
#120230 = CARTESIAN_POINT ( 'NONE',  ( -3.328169399223510627, 20.25929247661551003, 4.000000000000000000 ) ) ;
#120231 = EDGE_CURVE ( 'NONE', #90674, #136749, #56248, .T. ) ;
#120232 = ORIENTED_EDGE ( 'NONE', *, *, #3432, .T. ) ;
#120233 = FACE_OUTER_BOUND ( 'NONE', #3120, .T. ) ;
#120234 = ORIENTED_EDGE ( 'NONE', *, *, #96680, .F. ) ;
#120235 = EDGE_LOOP ( 'NONE', ( #21362, #41752, #57392, #70763 ) ) ;
#120236 = EDGE_LOOP ( 'NONE', ( #14010, #76959, #57624, #28696 ) ) ;
#120237 = ADVANCED_FACE ( 'NONE', ( #22812 ), #21435, .F. ) ;
#120238 = FACE_OUTER_BOUND ( 'NONE', #117756, .T. ) ;
#120239 = CARTESIAN_POINT ( 'NONE',  ( 30.48921356237309510, -27.52281430457076894, 5.000000000000000000 ) ) ;
#120240 = SURFACE_STYLE_FILL_AREA ( #140597 ) ;
#120241 = PLANE ( 'NONE',  #28674 ) ;
#120242 = CARTESIAN_POINT ( 'NONE',  ( 125.7087635252314470, -7.482591942790329030E-16, 6.110000000000001208 ) ) ;
#120243 = LINE ( 'NONE', #66636, #77476 ) ;
#120244 = CARTESIAN_POINT ( 'NONE',  ( -8.292893218813398803, -0.7407075233842735917, 5.000000000000000000 ) ) ;
#120245 = DIRECTION ( 'NONE',  ( 0.7071067811865486830, -0.7071067811865464625, -0.000000000000000000 ) ) ;
#120246 = EDGE_CURVE ( 'NONE', #80065, #96370, #29795, .T. ) ;
#120247 = CARTESIAN_POINT ( 'NONE',  ( 25.49999999999982592, -19.91253812416055169, 4.000000000000000000 ) ) ;
#120248 = DIRECTION ( 'NONE',  ( -0.7071067811865486830, -0.7071067811865464625, 0.000000000000000000 ) ) ;
#120249 = CARTESIAN_POINT ( 'NONE',  ( 28.49999999999980105, 0.4311230773921797543, 4.000000000000000000 ) ) ;
#120250 = DIRECTION ( 'NONE',  ( 0.3543493200069162685, -0.000000000000000000, -0.9351131265310288487 ) ) ;
#120251 = VERTEX_POINT ( 'NONE', #135219 ) ;
#120252 = EDGE_LOOP ( 'NONE', ( #44592, #126540, #81656, #116651 ) ) ;
#120254 = EDGE_LOOP ( 'NONE', ( #49312, #57120, #15514, #136002 ) ) ;
#120253 = EDGE_CURVE ( 'NONE', #15048, #118228, #36576, .T. ) ;
#120255 = LINE ( 'NONE', #32600, #98104 ) ;
#120256 = MECHANICAL_DESIGN_GEOMETRIC_PRESENTATION_REPRESENTATION (  '', ( #115595 ), #6731 ) ;
#120257 = VECTOR ( 'NONE', #46929, 1000.000000000000227 ) ;
#120258 = ORIENTED_EDGE ( 'NONE', *, *, #102104, .T. ) ;
#120259 = VECTOR ( 'NONE', #142276, 999.9999999999998863 ) ;
#120260 =( BOUNDED_CURVE ( )  B_SPLINE_CURVE ( 3, ( #12183, #76768, #33280, #65175 ),
 .UNSPECIFIED., .F., .T. ) 
 B_SPLINE_CURVE_WITH_KNOTS ( ( 4, 4 ),
 ( 2.779374508378134045, 4.199602562396851368 ),
 .UNSPECIFIED. ) 
 CURVE ( )  GEOMETRIC_REPRESENTATION_ITEM ( )  RATIONAL_B_SPLINE_CURVE ( ( 1.000000000000000000, 0.8388583629366599403, 0.8388583629366599403, 1.000000000000000000 ) ) 
 REPRESENTATION_ITEM ( '' )  );
#120262 = EDGE_LOOP ( 'NONE', ( #122537, #107985, #66266, #77310 ) ) ;
#120261 = VECTOR ( 'NONE', #46716, 1000.000000000000000 ) ;
#120263 = DIRECTION ( 'NONE',  ( -0.3543493200069163240, 0.000000000000000000, 0.9351131265310288487 ) ) ;
#120264 = DIRECTION ( 'NONE',  ( 0.000000000000000000, -1.000000000000000000, 0.000000000000000000 ) ) ;
#120265 = LINE ( 'NONE', #77549, #67222 ) ;
#120266 = ADVANCED_FACE ( 'NONE', ( #74036 ), #52041, .T. ) ;
#120267 = ORIENTED_EDGE ( 'NONE', *, *, #15388, .F. ) ;
#120268 = EDGE_CURVE ( 'NONE', #90585, #11670, #90992, .T. ) ;
#120269 = CARTESIAN_POINT ( 'NONE',  ( -11.51078643762690490, -27.52281430457047406, 5.000000000000000000 ) ) ;
#120271 = ORIENTED_EDGE ( 'NONE', *, *, #71564, .T. ) ;
#120270 = VECTOR ( 'NONE', #84026, 1000.000000000000227 ) ;
#120272 = EDGE_CURVE ( 'NONE', #40388, #100787, #135899, .T. ) ;
#120273 = CARTESIAN_POINT ( 'NONE',  ( -4.499999999999976019, 3.073033219394619930, -6.593910359670981158 ) ) ;
#120275 = VECTOR ( 'NONE', #115471, 1000.000000000000000 ) ;
#120274 = CARTESIAN_POINT ( 'NONE',  ( 21.65040314143522338, 7.934999999999989839, -2.126176841940961904 ) ) ;
#120276 = VERTEX_POINT ( 'NONE', #59099 ) ;
#120277 = CARTESIAN_POINT ( 'NONE',  ( 92.51626352523146579, -4.472830434245839371, 4.472830434245839371 ) ) ;
#120278 = CARTESIAN_POINT ( 'NONE',  ( 7.028598267277284428, -9.052066293035441191, -2.890594154426020967 ) ) ;
#120279 = CARTESIAN_POINT ( 'NONE',  ( 14.99999999999990230, -4.447814304570775867, 5.000000000000000000 ) ) ;
#120280 = EDGE_LOOP ( 'NONE', ( #135865, #30012, #118315, #1157 ) ) ;
#120281 = CARTESIAN_POINT ( 'NONE',  ( 4.171830600776443632, -11.24070752338417378, 4.000000000000000000 ) ) ;
#120282 = ORIENTED_EDGE ( 'NONE', *, *, #27974, .T. ) ;
#120283 = ORIENTED_EDGE ( 'NONE', *, *, #89615, .F. ) ;
#120284 = AXIS2_PLACEMENT_3D ( 'NONE', #126951, #39264, #17484 ) ;
#120285 = DIRECTION ( 'NONE',  ( 0.7071067811865486830, -0.7071067811865464625, -0.000000000000000000 ) ) ;
#120286 = VECTOR ( 'NONE', #19460, 1000.000000000000000 ) ;
#120287 = CARTESIAN_POINT ( 'NONE',  ( 18.18398860626898994, 28.73617430169800002, 5.000000000000000000 ) ) ;
#120288 = CARTESIAN_POINT ( 'NONE',  ( 36.18398860626899705, 28.73617430169812437, 5.000000000000000000 ) ) ;
#120289 = ORIENTED_EDGE ( 'NONE', *, *, #75041, .F. ) ;
#120290 = DIRECTION ( 'NONE',  ( 0.3543493200069162685, -0.000000000000000000, -0.9351131265310288487 ) ) ;
#120291 = AXIS2_PLACEMENT_3D ( 'NONE', #81742, #67273, #56438 ) ;
#120292 = CARTESIAN_POINT ( 'NONE',  ( 20.20710678118640757, 15.75929247661555443, 5.000000000000000000 ) ) ;
#120293 = CARTESIAN_POINT ( 'NONE',  ( 33.70701326429281153, -21.74070752338406365, 4.999753212805220670 ) ) ;
#120294 = EDGE_LOOP ( 'NONE', ( #9040, #7303, #46590, #67235, #14761 ) ) ;
#120295 = CARTESIAN_POINT ( 'NONE',  ( -40.64175702458835815, 15.75929247661555088, 19.34181609438708804 ) ) ;
#120296 = VECTOR ( 'NONE', #22831, 999.9999999999998863 ) ;
#120298 = VECTOR ( 'NONE', #103085, 1000.000000000000000 ) ;
#120297 = CARTESIAN_POINT ( 'NONE',  ( -66.48921356237309510, -27.52281430457101763, 5.000000000000000000 ) ) ;
#120299 = ORIENTED_EDGE ( 'NONE', *, *, #59737, .F. ) ;
#120300 = AXIS2_PLACEMENT_3D ( 'NONE', #133922, #133232, #23729 ) ;
#120302 = ORIENTED_EDGE ( 'NONE', *, *, #136821, .T. ) ;
#120301 = CARTESIAN_POINT ( 'NONE',  ( 19.04515773336654050, -21.74070752338406365, 21.72585301388589230 ) ) ;
#120303 = VERTEX_POINT ( 'NONE', #69976 ) ;
#120304 = VECTOR ( 'NONE', #121869, 1000.000000000000000 ) ;
#120305 = DIRECTION ( 'NONE',  ( -0.7071067811865486830, 0.7071067811865464625, 0.000000000000000000 ) ) ;
#120306 = VECTOR ( 'NONE', #38731, 1000.000000000000000 ) ;
#120307 = DIRECTION ( 'NONE',  ( -1.000000000000000000, -0.000000000000000000, -0.000000000000000000 ) ) ;
#120308 = ORIENTED_EDGE ( 'NONE', *, *, #96037, .T. ) ;
#120309 = CARTESIAN_POINT ( 'NONE',  ( 18.95159235450331892, -2.500000000000000444, 3.061616997868384620E-16 ) ) ;
#120310 = DIRECTION ( 'NONE',  ( 0.3543493200069163240, -0.000000000000000000, 0.9351131265310288487 ) ) ;
#120311 = FILL_AREA_STYLE_COLOUR ( '', #13698 ) ;
#120312 = LINE ( 'NONE', #8682, #46185 ) ;
#120313 = DIRECTION ( 'NONE',  ( 0.000000000000000000, -1.000000000000000000, 0.000000000000000000 ) ) ;
#120314 = DIRECTION ( 'NONE',  ( -0.6830127018922180770, -0.6830127018922204085, -0.2588190451025213501 ) ) ;
#120315 = CARTESIAN_POINT ( 'NONE',  ( -1.499999999999987566, 10.08746187583914633, 4.000000000000000000 ) ) ;
#120316 = SURFACE_SIDE_STYLE ('',( #131238 ) ) ;
#120318 = VECTOR ( 'NONE', #56923, 1000.000000000000227 ) ;
#120317 = CARTESIAN_POINT ( 'NONE',  ( -26.21837311707487572, 21.74787736706806740, 4.999607392498048419 ) ) ;
#120319 = CARTESIAN_POINT ( 'NONE',  ( -35.99451991528749772, 28.92564299267963079, 4.000000000000000000 ) ) ;
#120320 = CARTESIAN_POINT ( 'NONE',  ( 11.81601139373100651, 28.73617430169779041, 5.000000000000000000 ) ) ;
#120321 = CARTESIAN_POINT ( 'NONE',  ( -34.42500000000001137, 7.541399257801932876, 5.000000000000000000 ) ) ;
#120322 = CARTESIAN_POINT ( 'NONE',  ( -7.140000000000001457, -35.76999999999998892, -12.10072711459627293 ) ) ;
#120323 = ORIENTED_EDGE ( 'NONE', *, *, #110697, .F. ) ;
#120324 = VERTEX_POINT ( 'NONE', #126434 ) ;
#120325 = ORIENTED_EDGE ( 'NONE', *, *, #78541, .F. ) ;
#120326 = CARTESIAN_POINT ( 'NONE',  ( 104.9791666666666714, -7.950000000000001066, 2.130196079827424427 ) ) ;
#120327 = ORIENTED_EDGE ( 'NONE', *, *, #25642, .F. ) ;
#120328 = EDGE_LOOP ( 'NONE', ( #1201, #82019, #98906, #42575 ) ) ;
#120329 = ORIENTED_EDGE ( 'NONE', *, *, #137560, .F. ) ;
#120330 = CARTESIAN_POINT ( 'NONE',  ( 20.48831394071555678, 6.759292476615645917, 16.35960578974464852 ) ) ;
#120331 = CARTESIAN_POINT ( 'NONE',  ( 89.66666666666667140, 6.884901960086285300, 3.975000000000003642 ) ) ;
#120332 = CIRCLE ( 'NONE', #60278, 6.094999999999989093 ) ;
#120333 = ORIENTED_EDGE ( 'NONE', *, *, #101279, .F. ) ;
#120334 = CARTESIAN_POINT ( 'NONE',  ( 11.51078643762690490, -27.52281430457047406, 5.000000000000000000 ) ) ;
#120335 = CARTESIAN_POINT ( 'NONE',  ( 62.99451991528749772, 28.92564299267982264, 4.000000000000000000 ) ) ;
#120336 = FACE_OUTER_BOUND ( 'NONE', #1840, .T. ) ;
#120337 = CARTESIAN_POINT ( 'NONE',  ( 12.69999999999999574, -22.33999999999998565, -0.5000000000000004441 ) ) ;
#120338 = EDGE_CURVE ( 'NONE', #34379, #72776, #79923, .T. ) ;
#120339 = ORIENTED_EDGE ( 'NONE', *, *, #141871, .T. ) ;
#120340 = CARTESIAN_POINT ( 'NONE',  ( 13.10362284818588741, 2.655808543615126638, 5.000000000000000000 ) ) ;
#120341 = EDGE_CURVE ( 'NONE', #14857, #70673, #137341, .T. ) ;
#120342 = FACE_OUTER_BOUND ( 'NONE', #79222, .T. ) ;
#120343 = LINE ( 'NONE', #98624, #30817 ) ;
#120344 = CARTESIAN_POINT ( 'NONE',  ( 24.25645252394784990, 6.095695649681008632, 4.664440252871067116 ) ) ;
#120345 = LINE ( 'NONE', #728, #56157 ) ;
#120346 = DIRECTION ( 'NONE',  ( -0.7071067811865486830, -0.7071067811865464625, -0.000000000000000000 ) ) ;
#120347 = CARTESIAN_POINT ( 'NONE',  ( 29.24586038379621655, 3.974999999999996980, 6.884901960086287964 ) ) ;
#120348 = CARTESIAN_POINT ( 'NONE',  ( 29.99999999999979750, -4.068876922607768343, 4.000000000000000000 ) ) ;
#120349 = EDGE_LOOP ( 'NONE', ( #88389, #52664, #140106, #48231, #1045 ) ) ;
#120350 = ORIENTED_EDGE ( 'NONE', *, *, #10728, .F. ) ;
#120351 = CARTESIAN_POINT ( 'NONE',  ( 119.7295968585647614, -6.110000000000000320, -1.637169565754161393 ) ) ;
#120352 = ORIENTED_EDGE ( 'NONE', *, *, #102104, .F. ) ;
#120353 = EDGE_CURVE ( 'NONE', #77093, #9940, #125016, .T. ) ;
#120354 = DIRECTION ( 'NONE',  ( -0.5735764363510503783, -0.8191520442889886899, 0.000000000000000000 ) ) ;
#120355 = DIRECTION ( 'NONE',  ( 0.000000000000000000, -1.000000000000000000, 0.000000000000000000 ) ) ;
#120356 = DIRECTION ( 'NONE',  ( -0.6830127018922181881, 0.6830127018922202975, -0.2588190451025214056 ) ) ;
#120357 = EDGE_CURVE ( 'NONE', #85580, #54158, #80126, .T. ) ;
#120358 = LINE ( 'NONE', #11604, #88398 ) ;
#120359 = VECTOR ( 'NONE', #44017, 1000.000000000000000 ) ;
#120360 = CARTESIAN_POINT ( 'NONE',  ( 125.9120968585647802, 5.291415217122921177, -3.054999999999994831 ) ) ;
#120361 = ORIENTED_EDGE ( 'NONE', *, *, #106867, .F. ) ;
#120362 = ORIENTED_EDGE ( 'NONE', *, *, #45808, .F. ) ;
#120363 = DIRECTION ( 'NONE',  ( 0.7071067811865487940, 0.7071067811865463515, 0.000000000000000000 ) ) ;
#120365 = EDGE_CURVE ( 'NONE', #69243, #98525, #114825, .T. ) ;
#120364 = CIRCLE ( 'NONE', #48590, 2.500000000000000888 ) ;
#120366 = VECTOR ( 'NONE', #18881, 1000.000000000000000 ) ;
#120367 = VECTOR ( 'NONE', #68995, 1000.000000000000000 ) ;
#120368 = PLANE ( 'NONE',  #96389 ) ;
#120369 = VECTOR ( 'NONE', #85683, 999.9999999999998863 ) ;
#120370 = ORIENTED_EDGE ( 'NONE', *, *, #95340, .T. ) ;
#120371 = CARTESIAN_POINT ( 'NONE',  ( 49.72959685856476852, -6.110000000000000320, -1.637169565754161393 ) ) ;
#120372 = ORIENTED_EDGE ( 'NONE', *, *, #50346, .F. ) ;
#120373 = DIRECTION ( 'NONE',  ( -0.000000000000000000, -0.3543493200069152693, 0.9351131265310292928 ) ) ;
#120374 = CARTESIAN_POINT ( 'NONE',  ( 156.1500000000000057, -49.14999999999999147, -45.92499999999969162 ) ) ;
#120375 = PLANE ( 'NONE',  #91862 ) ;
#120376 = CARTESIAN_POINT ( 'NONE',  ( 42.18398860626899705, 28.73617430169816700, 5.000000000000000000 ) ) ;
#120377 = CIRCLE ( 'NONE', #88032, 2.500000000000000444 ) ;
#120378 = CARTESIAN_POINT ( 'NONE',  ( 40.16209685856478018, -5.291415217122919401, 3.054999999999997939 ) ) ;
#120379 = ORIENTED_EDGE ( 'NONE', *, *, #1875, .F. ) ;
#120380 = EDGE_CURVE ( 'NONE', #82699, #39180, #124307, .T. ) ;
#120381 = CARTESIAN_POINT ( 'NONE',  ( 47.99451991528749062, 28.92564299267971251, 4.000000000000000000 ) ) ;
#120382 = ORIENTED_EDGE ( 'NONE', *, *, #108791, .T. ) ;
#120383 = ORIENTED_EDGE ( 'NONE', *, *, #136897, .F. ) ;
#120384 = VECTOR ( 'NONE', #99095, 1000.000000000000000 ) ;
#120385 = ORIENTED_EDGE ( 'NONE', *, *, #58797, .F. ) ;
#120386 = ADVANCED_FACE ( 'NONE', ( #15504 ), #24975, .T. ) ;
#120387 = EDGE_CURVE ( 'NONE', #98744, #22050, #37303, .T. ) ;
#120388 = AXIS2_PLACEMENT_3D ( 'NONE', #65532, #141637, #121291 ) ;
#120389 = PLANE ( 'NONE',  #98407 ) ;
#120390 = FACE_OUTER_BOUND ( 'NONE', #76133, .T. ) ;
#120391 = ORIENTED_EDGE ( 'NONE', *, *, #92697, .T. ) ;
#120392 = CARTESIAN_POINT ( 'NONE',  ( 1.930039745135905704, -0.7407075233842770334, 13.87443053587610464 ) ) ;
#120393 = AXIS2_PLACEMENT_3D ( 'NONE', #102565, #114809, #3211 ) ;
#120394 = CARTESIAN_POINT ( 'NONE',  ( -27.18398860626900060, 28.73617430169806042, 5.000000000000000000 ) ) ;
#120396 = ADVANCED_FACE ( 'NONE', ( #3225 ), #25699, .F. ) ;
#120395 = VECTOR ( 'NONE', #98616, 1000.000000000000000 ) ;
#120397 = PLANE ( 'NONE',  #99941 ) ;
#120398 = FACE_BOUND ( 'NONE', #121800, .T. ) ;
#120399 = EDGE_CURVE ( 'NONE', #142744, #84062, #106703, .T. ) ;
#120400 = ORIENTED_EDGE ( 'NONE', *, *, #34397, .F. ) ;
#120401 = PLANE ( 'NONE',  #10887 ) ;
#120402 = CARTESIAN_POINT ( 'NONE',  ( 16.44013779566152778, 3.821174125832445049E-16, 0.000000000000000000 ) ) ;
#120403 = EDGE_CURVE ( 'NONE', #49613, #21069, #3905, .T. ) ;
#120404 = ORIENTED_EDGE ( 'NONE', *, *, #50001, .T. ) ;
#120405 = CARTESIAN_POINT ( 'NONE',  ( 0.000000000000000000, 0.000000000000000000, 5.000000000000000000 ) ) ;
#120406 = ORIENTED_EDGE ( 'NONE', *, *, #81725, .F. ) ;
#120407 = ORIENTED_EDGE ( 'NONE', *, *, #27776, .F. ) ;
#120408 = CARTESIAN_POINT ( 'NONE',  ( 6.499999999999999112, 7.960204194457794491E-16, -10.00000000000000000 ) ) ;
#120409 = VERTEX_POINT ( 'NONE', #70679 ) ;
#120410 = CARTESIAN_POINT ( 'NONE',  ( 45.55793019189811588, 6.110000000000000320, -1.637169565754156064 ) ) ;
#120411 = ORIENTED_EDGE ( 'NONE', *, *, #20789, .T. ) ;
#120412 = VECTOR ( 'NONE', #31483, 1000.000000000000000 ) ;
#120413 = EDGE_CURVE ( 'NONE', #112319, #7244, #138046, .T. ) ;
#120414 = CARTESIAN_POINT ( 'NONE',  ( -3.183988606268992161, 28.73617430169789699, 5.000000000000000000 ) ) ;
#120415 = CARTESIAN_POINT ( 'NONE',  ( -30.70710678118632941, 8.259292476615637923, 5.000000000000000000 ) ) ;
#120416 = CARTESIAN_POINT ( 'NONE',  ( -41.99451991528749062, 28.92564299267967343, 4.000000000000000000 ) ) ;
#120417 = EDGE_LOOP ( 'NONE', ( #23071, #134892, #40655, #117396, #85900 ) ) ;
#120418 = CARTESIAN_POINT ( 'NONE',  ( 75.18398860626899705, 28.73617430169839793, 5.000000000000000000 ) ) ;
#120419 = VECTOR ( 'NONE', #33573, 1000.000000000000000 ) ;
#120420 = ADVANCED_FACE ( 'NONE', ( #129117 ), #26583, .T. ) ;
#120421 = LINE ( 'NONE', #108127, #54812 ) ;
#120422 = DIRECTION ( 'NONE',  ( -0.7071067811865486830, -0.7071067811865464625, -0.000000000000000000 ) ) ;
#120423 = DIRECTION ( 'NONE',  ( 0.7071067811865487940, -0.7071067811865463515, 0.000000000000000000 ) ) ;
#120424 = CARTESIAN_POINT ( 'NONE',  ( 36.48921356237310221, -27.52281430457080802, 5.000000000000000000 ) ) ;
#120425 = LINE ( 'NONE', #94073, #55643 ) ;
#120426 = ORIENTED_EDGE ( 'NONE', *, *, #133646, .F. ) ;
#120427 = ORIENTED_EDGE ( 'NONE', *, *, #17137, .T. ) ;
#120428 = AXIS2_PLACEMENT_3D ( 'NONE', #84153, #106548, #7232 ) ;
#120429 = ORIENTED_EDGE ( 'NONE', *, *, #93397, .T. ) ;
#120430 = CARTESIAN_POINT ( 'NONE',  ( 2.816011393730999401, 28.73617430169785436, 5.000000000000000000 ) ) ;
#120431 = DIRECTION ( 'NONE',  ( 0.7071067811865486830, -0.7071067811865464625, -0.000000000000000000 ) ) ;
#120432 = ORIENTED_EDGE ( 'NONE', *, *, #131777, .F. ) ;
#120433 = EDGE_LOOP ( 'NONE', ( #96971, #25005, #72204, #84979 ) ) ;
#120434 = CARTESIAN_POINT ( 'NONE',  ( -17.99999999999987566, 19.55218569542897100, 5.000000000000000000 ) ) ;
#120435 = CARTESIAN_POINT ( 'NONE',  ( 15.66846741159846879, -18.74070752338408852, 20.73178291233844917 ) ) ;
#120436 = CARTESIAN_POINT ( 'NONE',  ( 36.48921356237310221, -27.52281430457080802, 5.000000000000000000 ) ) ;
#120437 = ORIENTED_EDGE ( 'NONE', *, *, #59547, .F. ) ;
#120438 = LINE ( 'NONE', #61848, #25462 ) ;
#120439 = VECTOR ( 'NONE', #137490, 1000.000000000000000 ) ;
#120440 = AXIS2_PLACEMENT_3D ( 'NONE', #113903, #47284, #126897 ) ;
#120441 = EDGE_CURVE ( 'NONE', #76924, #80396, #42853, .T. ) ;
#120442 = PLANE ( 'NONE',  #130131 ) ;
#120443 = EDGE_CURVE ( 'NONE', #59092, #20535, #32689, .T. ) ;
#120444 = CARTESIAN_POINT ( 'NONE',  ( 15.81706980810188767, -2.126176841940956130, 7.934999999999991616 ) ) ;
#120445 = CARTESIAN_POINT ( 'NONE',  ( -1.809818324255504818, -18.74070752338408852, 7.910009926591512475 ) ) ;
#120446 = VERTEX_POINT ( 'NONE', #86353 ) ;
#120447 = CARTESIAN_POINT ( 'NONE',  ( 117.8912635252314516, -4.472830434245839371, -4.472830434245839371 ) ) ;
#120448 = LINE ( 'NONE', #110302, #125273 ) ;
#120449 = PLANE ( 'NONE',  #116703 ) ;
#120451 = ORIENTED_EDGE ( 'NONE', *, *, #80528, .F. ) ;
#120450 = CARTESIAN_POINT ( 'NONE',  ( 29.67183060077626067, 5.259292476615669010, 4.000000000000000000 ) ) ;
#120452 = CARTESIAN_POINT ( 'NONE',  ( 0.000000000000000000, 0.000000000000000000, 5.000000000000000000 ) ) ;
#120453 = EDGE_LOOP ( 'NONE', ( #7714, #30136, #39486, #43699, #121812, #134312 ) ) ;
#120454 = CARTESIAN_POINT ( 'NONE',  ( -16.39656807105347625, -14.24070752338413648, 19.24067776001722052 ) ) ;
#120455 = CIRCLE ( 'NONE', #136731, 0.5000000000000013323 ) ;
#120456 = CARTESIAN_POINT ( 'NONE',  ( 14.81601139373099585, 28.73617430169776910, 5.000000000000000000 ) ) ;
#120457 = CARTESIAN_POINT ( 'NONE',  ( 33.48921356237309510, -27.52281430457078670, 5.000000000000000000 ) ) ;
#120458 = ORIENTED_EDGE ( 'NONE', *, *, #81870, .T. ) ;
#120459 = PRESENTATION_LAYER_ASSIGNMENT (  '', '', ( #97283 ) ) ;
#120460 = VECTOR ( 'NONE', #4628, 999.9999999999998863 ) ;
#120461 = DIRECTION ( 'NONE',  ( 1.000000000000000000, -0.000000000000000000, 0.000000000000000000 ) ) ;
#120462 = CARTESIAN_POINT ( 'NONE',  ( 9.792893218813393474, -20.24070752338407431, 5.000000000000000000 ) ) ;
#120463 = VERTEX_POINT ( 'NONE', #63887 ) ;
#120464 = VECTOR ( 'NONE', #139783, 1000.000000000000227 ) ;
#120465 = AXIS2_PLACEMENT_3D ( 'NONE', #11367, #65841, #109294 ) ;
#120466 = AXIS2_PLACEMENT_3D ( 'NONE', #44787, #34582, #43321 ) ;
#120467 = FACE_OUTER_BOUND ( 'NONE', #141204, .T. ) ;
#120468 = CIRCLE ( 'NONE', #111511, 2.500000000000000444 ) ;
#120469 = CARTESIAN_POINT ( 'NONE',  ( 30.18398860626900060, 28.73617430169808173, 5.000000000000000000 ) ) ;
#120470 = ORIENTED_EDGE ( 'NONE', *, *, #44476, .T. ) ;
#120471 =( NAMED_UNIT ( * ) SI_UNIT ( $, .STERADIAN. ) SOLID_ANGLE_UNIT ( ) );
#120473 = ORIENTED_EDGE ( 'NONE', *, *, #51752, .F. ) ;
#120472 = PLANE ( 'NONE',  #11 ) ;
#120474 = ORIENTED_EDGE ( 'NONE', *, *, #73362, .T. ) ;
#120475 = CARTESIAN_POINT ( 'NONE',  ( -13.84116387061258457, 6.089959206779446355, 4.000000000000000000 ) ) ;
#120476 = CONICAL_SURFACE ( 'NONE', #129718, 2.055000000000000604, 0.9599310885968764806 ) ;
#120477 = CARTESIAN_POINT ( 'NONE',  ( 42.18398860626899705, 28.73617430169816700, 5.000000000000000000 ) ) ;
#120478 = ORIENTED_EDGE ( 'NONE', *, *, #28653, .F. ) ;
#120479 = CARTESIAN_POINT ( 'NONE',  ( 15.18398860626900237, 28.73617430169797871, 5.000000000000000000 ) ) ;
#120480 = DIRECTION ( 'NONE',  ( 0.6830127018922181881, 0.6830127018922202975, -0.2588190451025214056 ) ) ;
#120481 = DIRECTION ( 'NONE',  ( -0.000000000000000000, 0.3543493200069153248, 0.9351131265310292928 ) ) ;
#120482 = VERTEX_POINT ( 'NONE', #10876 ) ;
#120483 = CARTESIAN_POINT ( 'NONE',  ( 0.000000000000000000, 0.000000000000000000, 5.000000000000000000 ) ) ;
#120485 = EDGE_CURVE ( 'NONE', #9148, #48488, #93740, .T. ) ;
#120484 = CARTESIAN_POINT ( 'NONE',  ( -2.999999999999981792, -13.97847968911260708, -0.1324546996126860776 ) ) ;
#120486 = CARTESIAN_POINT ( 'NONE',  ( 39.48921356237310221, -27.52281430457082934, 5.000000000000000000 ) ) ;
#120487 = VECTOR ( 'NONE', #21410, 1000.000000000000000 ) ;
#120488 = CARTESIAN_POINT ( 'NONE',  ( 39.57876352523144448, -7.482591942790327058E-16, 6.109999999999999432 ) ) ;
#120489 = CARTESIAN_POINT ( 'NONE',  ( 14.51078643762690490, -27.52281430457045275, 5.000000000000000000 ) ) ;
#120490 = VECTOR ( 'NONE', #78189, 1000.000000000000000 ) ;
#120491 = ORIENTED_EDGE ( 'NONE', *, *, #125546, .F. ) ;
#120492 = ORIENTED_EDGE ( 'NONE', *, *, #55950, .F. ) ;
#120493 = CARTESIAN_POINT ( 'NONE',  ( 126.4166666666666714, -6.884901960086287076, -3.975000000000000977 ) ) ;
#120494 = AXIS2_PLACEMENT_3D ( 'NONE', #30618, #63950, #121159 ) ;
#120495 = VERTEX_POINT ( 'NONE', #31256 ) ;
#120496 = AXIS2_PLACEMENT_3D ( 'NONE', #138580, #95772, #71194 ) ;
#120497 = ORIENTED_EDGE ( 'NONE', *, *, #16654, .F. ) ;
#120498 = CARTESIAN_POINT ( 'NONE',  ( 8.292893218813398803, 11.25929247661560595, 5.000000000000000000 ) ) ;
#120499 = LINE ( 'NONE', #52418, #113376 ) ;
#120500 = VECTOR ( 'NONE', #131592, 1000.000000000000000 ) ;
#120501 = EDGE_LOOP ( 'NONE', ( #116446, #66542, #134411, #120955 ) ) ;
#120502 = PRESENTATION_STYLE_ASSIGNMENT (( #121248 ) ) ;
#120503 = FACE_OUTER_BOUND ( 'NONE', #100097, .T. ) ;
#120504 = ADVANCED_FACE ( 'NONE', ( #87052 ), #66039, .F. ) ;
#120505 = LINE ( 'NONE', #109668, #30112 ) ;
#120506 = CARTESIAN_POINT ( 'NONE',  ( -24.96654721599509941, 3.964575861396866685, 4.000000000000000000 ) ) ;
#120507 = LINE ( 'NONE', #130740, #96267 ) ;
#120508 = EDGE_CURVE ( 'NONE', #111356, #126534, #97165, .T. ) ;
#120509 = EDGE_CURVE ( 'NONE', #66944, #99905, #119640, .T. ) ;
#120510 = VECTOR ( 'NONE', #126400, 1000.000000000000000 ) ;
#120511 = ORIENTED_EDGE ( 'NONE', *, *, #62965, .T. ) ;
#120512 = LINE ( 'NONE', #132892, #134428 ) ;
#120513 = FILL_AREA_STYLE_COLOUR ( '', #26032 ) ;
#120514 = LINE ( 'NONE', #141605, #95873 ) ;
#120515 = CARTESIAN_POINT ( 'NONE',  ( 21.96495920677946856, -2.033836129387410985, 4.000000000000000000 ) ) ;
#120516 = CARTESIAN_POINT ( 'NONE',  ( 81.18398860626899705, 28.73617430169844056, 5.000000000000000000 ) ) ;
#120517 = FACE_OUTER_BOUND ( 'NONE', #85139, .T. ) ;
#120518 = DIRECTION ( 'NONE',  ( 0.7071067811865487940, -0.7071067811865463515, 0.000000000000000000 ) ) ;
#120519 = EDGE_CURVE ( 'NONE', #85531, #25852, #23305, .T. ) ;
#120521 = EDGE_CURVE ( 'NONE', #36667, #4933, #109512, .T. ) ;
#120520 = CARTESIAN_POINT ( 'NONE',  ( 57.39169371712954870, 2.130196079827421762, 7.950000000000001066 ) ) ;
#120522 = CARTESIAN_POINT ( 'NONE',  ( 20.46326412755669111, -2.625232532701756494, 4.661243073242808954 ) ) ;
#120523 = DIRECTION ( 'NONE',  ( 0.7071067811865487940, 0.7071067811865463515, -0.000000000000000000 ) ) ;
#120524 = VECTOR ( 'NONE', #51904, 1000.000000000000000 ) ;
#120525 = EDGE_LOOP ( 'NONE', ( #33419, #110100, #116407, #79190 ) ) ;
#120526 = ORIENTED_EDGE ( 'NONE', *, *, #3928, .T. ) ;
#120527 = CARTESIAN_POINT ( 'NONE',  ( 55.54166666666665719, -3.975000000000002753, 6.884901960086286188 ) ) ;
#120528 = CARTESIAN_POINT ( 'NONE',  ( 0.000000000000000000, 0.000000000000000000, 5.000000000000000000 ) ) ;
#120529 = EDGE_CURVE ( 'NONE', #43087, #29352, #109972, .T. ) ;
#120530 = CARTESIAN_POINT ( 'NONE',  ( 25.49999999999981526, -14.70932175296475819, -11.46312253303843143 ) ) ;
#120531 = LINE ( 'NONE', #909, #83186 ) ;
#120532 = VERTEX_POINT ( 'NONE', #55146 ) ;
#120533 = CARTESIAN_POINT ( 'NONE',  ( 4.198949119135569656E-17, -1.320799999999990870, 4.000000000000000000 ) ) ;
#120534 = CARTESIAN_POINT ( 'NONE',  ( 156.1500000000000057, -49.14999999999999147, 45.92499999999998295 ) ) ;
#120535 = EDGE_CURVE ( 'NONE', #95348, #118892, #65330, .T. ) ;
#120536 = CARTESIAN_POINT ( 'NONE',  ( 48.27126352523143993, 4.472830434245839371, 4.472830434245842035 ) ) ;
#120537 = VERTEX_POINT ( 'NONE', #87763 ) ;
#120538 = ORIENTED_EDGE ( 'NONE', *, *, #104688, .F. ) ;
#120539 = ORIENTED_EDGE ( 'NONE', *, *, #77611, .F. ) ;
#120540 = VECTOR ( 'NONE', #135327, 1000.000000000000000 ) ;
#120541 = FACE_OUTER_BOUND ( 'NONE', #36522, .T. ) ;
#120542 = EDGE_CURVE ( 'NONE', #100333, #745, #131996, .T. ) ;
#120543 = CARTESIAN_POINT ( 'NONE',  ( 18.18398860626898994, 28.73617430169800002, 5.000000000000000000 ) ) ;
#120544 = DIRECTION ( 'NONE',  ( 0.6830127018922181881, 0.6830127018922202975, -0.2588190451025214056 ) ) ;
#120545 = CARTESIAN_POINT ( 'NONE',  ( 12.08840764549667668, 3.061616997868380183E-16, -2.500000000000001332 ) ) ;
#120546 = EDGE_LOOP ( 'NONE', ( #45638, #89761, #102385, #78520 ) ) ;
#120547 = CARTESIAN_POINT ( 'NONE',  ( 12.69999999999999574, -35.15000000000000568, 17.49210858042622618 ) ) ;
#120549 = ORIENTED_EDGE ( 'NONE', *, *, #127960, .T. ) ;
#120548 = LINE ( 'NONE', #140893, #24369 ) ;
#120550 = CARTESIAN_POINT ( 'NONE',  ( 78.89626352523143282, 4.472830434245840259, -4.472830434245838482 ) ) ;
#120551 = CARTESIAN_POINT ( 'NONE',  ( 56.99451991528749062, 28.92564299267978001, 4.000000000000000000 ) ) ;
#120552 = DIRECTION ( 'NONE',  ( 0.000000000000000000, 0.000000000000000000, -1.000000000000000000 ) ) ;
#120553 = DIRECTION ( 'NONE',  ( 0.000000000000000000, -0.9647414015272155474, 0.2631995976047525887 ) ) ;
#120554 = EDGE_CURVE ( 'NONE', #80329, #118697, #21791, .T. ) ;
#120555 = LINE ( 'NONE', #88701, #2290 ) ;
#120556 = CARTESIAN_POINT ( 'NONE',  ( 28.00000000000002487, -49.14999999999999147, -34.92499999999976978 ) ) ;
#120557 = CIRCLE ( 'NONE', #4725, 2.500000000000000444 ) ;
#120558 = ORIENTED_EDGE ( 'NONE', *, *, #136760, .F. ) ;
#120559 = DIRECTION ( 'NONE',  ( 1.000000000000000000, 0.000000000000000000, 0.000000000000000000 ) ) ;
#120560 = CARTESIAN_POINT ( 'NONE',  ( 68.01626352523145158, -4.472830434245839371, 4.472830434245839371 ) ) ;
#120561 = CARTESIAN_POINT ( 'NONE',  ( -12.69999999999998153, 0.000000000000000000, 2.500000000000000444 ) ) ;
#120562 = EDGE_CURVE ( 'NONE', #33358, #33570, #141907, .T. ) ;
#120563 = DIRECTION ( 'NONE',  ( 0.7071067811865487940, -0.7071067811865463515, 0.000000000000000000 ) ) ;
#120564 = CARTESIAN_POINT ( 'NONE',  ( 0.000000000000000000, 0.000000000000000000, 5.000000000000000000 ) ) ;
#120565 = ORIENTED_EDGE ( 'NONE', *, *, #37728, .T. ) ;
#120566 = ORIENTED_EDGE ( 'NONE', *, *, #9687, .F. ) ;
#120567 = CARTESIAN_POINT ( 'NONE',  ( -22.49999999999984013, 21.05218569542895324, 5.000000000000000000 ) ) ;
#120569 = VECTOR ( 'NONE', #129047, 999.9999999999998863 ) ;
#120568 = CARTESIAN_POINT ( 'NONE',  ( -27.48921356237309155, -27.52281430457074762, 5.000000000000000000 ) ) ;
#120570 = ORIENTED_EDGE ( 'NONE', *, *, #64284, .F. ) ;
#120572 = EDGE_CURVE ( 'NONE', #103863, #133102, #30540, .T. ) ;
#120571 = VECTOR ( 'NONE', #5434, 1000.000000000000000 ) ;
#120574 = VERTEX_POINT ( 'NONE', #22472 ) ;
#120573 = VECTOR ( 'NONE', #133290, 1000.000000000000000 ) ;
#120575 = CARTESIAN_POINT ( 'NONE',  ( -51.18398860626899705, 28.73617430169823095, 5.000000000000000000 ) ) ;
#120577 = EDGE_CURVE ( 'NONE', #54899, #101759, #52272, .T. ) ;
#120576 = ORIENTED_EDGE ( 'NONE', *, *, #101244, .F. ) ;
#120578 = PLANE ( 'NONE',  #70149 ) ;
#120579 = CARTESIAN_POINT ( 'NONE',  ( -2.816011393730999401, 28.73617430169785436, 5.000000000000000000 ) ) ;
#120580 = AXIS2_PLACEMENT_3D ( 'NONE', #52386, #29914, #74154 ) ;
#120581 = VECTOR ( 'NONE', #117652, 999.9999999999998863 ) ;
#120582 = AXIS2_PLACEMENT_3D ( 'NONE', #76508, #66345, #37075 ) ;
#120583 = VECTOR ( 'NONE', #313, 1000.000000000000227 ) ;
#120584 = EDGE_CURVE ( 'NONE', #115305, #96751, #52943, .T. ) ;
#120585 = VECTOR ( 'NONE', #127823, 1000.000000000000227 ) ;
#120586 = LINE ( 'NONE', #21309, #136881 ) ;
#120587 = FACE_BOUND ( 'NONE', #50537, .T. ) ;
#120588 = LINE ( 'NONE', #54668, #71066 ) ;
#120589 = LINE ( 'NONE', #87286, #53559 ) ;
#120591 = DIRECTION ( 'NONE',  ( -1.000000000000000000, -0.000000000000000000, -0.000000000000000000 ) ) ;
#120590 = VECTOR ( 'NONE', #54278, 1000.000000000000000 ) ;
#120593 = ORIENTED_EDGE ( 'NONE', *, *, #131759, .F. ) ;
#120592 = DIRECTION ( 'NONE',  ( -1.000000000000000000, 0.000000000000000000, 3.596245529072721644E-15 ) ) ;
#120594 = DIRECTION ( 'NONE',  ( -0.7071067811865487940, 0.7071067811865463515, 0.000000000000000000 ) ) ;
#120595 = CONTEXT_DEPENDENT_SHAPE_REPRESENTATION ( #56963, #116394 ) ;
#120596 = ORIENTED_EDGE ( 'NONE', *, *, #62718, .T. ) ;
#120597 = EDGE_LOOP ( 'NONE', ( #123702, #84987, #122207, #135990 ) ) ;
#120598 = CARTESIAN_POINT ( 'NONE',  ( 86.53709685856478018, -3.054999999999998828, -5.291415217122919401 ) ) ;
#120599 = EDGE_LOOP ( 'NONE', ( #32231, #27533, #81802, #16712, #124176, #105551 ) ) ;
#120601 = EDGE_CURVE ( 'NONE', #12106, #82511, #135570, .T. ) ;
#120600 = AXIS2_PLACEMENT_3D ( 'NONE', #57007, #92428, #37370 ) ;
#120602 = PLANE ( 'NONE',  #106851 ) ;
#120603 = VECTOR ( 'NONE', #45335, 1000.000000000000000 ) ;
#120604 = VERTEX_POINT ( 'NONE', #100075 ) ;
#120605 = DIRECTION ( 'NONE',  ( 0.7071067811865486830, -0.7071067811865464625, -0.000000000000000000 ) ) ;
#120606 = EDGE_CURVE ( 'NONE', #18405, #14052, #78324, .T. ) ;
#120607 = AXIS2_PLACEMENT_3D ( 'NONE', #90869, #125630, #115401 ) ;
#120608 = CARTESIAN_POINT ( 'NONE',  ( 26.20710678118636494, 9.759292476615616607, 5.000000000000000000 ) ) ;
#120609 = DIRECTION ( 'NONE',  ( -0.000000000000000000, 0.000000000000000000, 1.000000000000000000 ) ) ;
#120610 = AXIS2_PLACEMENT_3D ( 'NONE', #125033, #124321, #113430 ) ;
#120611 = CARTESIAN_POINT ( 'NONE',  ( 8.994519915287490619, 28.92564299267944250, 4.000000000000000000 ) ) ;
#120612 = CARTESIAN_POINT ( 'NONE',  ( -66.48921356237309510, -27.52281430457101763, 5.000000000000000000 ) ) ;
#120613 = LINE ( 'NONE', #21334, #102878 ) ;
#120614 = VECTOR ( 'NONE', #102831, 1000.000000000000000 ) ;
#120615 = CARTESIAN_POINT ( 'NONE',  ( 39.18398860626899705, 28.73617430169814568, 5.000000000000000000 ) ) ;
#120616 = DIRECTION ( 'NONE',  ( 0.6830127018922180770, -0.6830127018922204085, -0.2588190451025213501 ) ) ;
#120617 = ORIENTED_EDGE ( 'NONE', *, *, #86931, .F. ) ;
#120618 = CARTESIAN_POINT ( 'NONE',  ( 13.49999999999991118, 14.14708470758592362, -0.5283514160166871143 ) ) ;
#120619 = ORIENTED_EDGE ( 'NONE', *, *, #14225, .F. ) ;
#120620 = CIRCLE ( 'NONE', #16411, 4.999999999999998224 ) ;
#120621 = DIRECTION ( 'NONE',  ( -0.7071067811865487940, 0.7071067811865463515, -0.000000000000000000 ) ) ;
#120622 = DIRECTION ( 'NONE',  ( 0.7071067811865486830, -0.7071067811865464625, -0.000000000000000000 ) ) ;
#120623 = ORIENTED_EDGE ( 'NONE', *, *, #118506, .T. ) ;
#120624 = ORIENTED_EDGE ( 'NONE', *, *, #88681, .T. ) ;
#120625 = VECTOR ( 'NONE', #134103, 1000.000000000000000 ) ;
#120626 = EDGE_CURVE ( 'NONE', #64363, #97358, #55875, .T. ) ;
#120627 = CARTESIAN_POINT ( 'NONE',  ( 34.41709685856476852, 3.054999999999998828, 5.291415217122922066 ) ) ;
#120628 = VERTEX_POINT ( 'NONE', #13738 ) ;
#120629 = CARTESIAN_POINT ( 'NONE',  ( 45.33333333333332149, -6.884901960086287964, 3.974999999999998312 ) ) ;
#120630 = EDGE_CURVE ( 'NONE', #83015, #94514, #136253, .T. ) ;
#120631 = CARTESIAN_POINT ( 'NONE',  ( -19.80981832425539224, -18.74070752338409562, 7.910009926591554219 ) ) ;
#120632 = VECTOR ( 'NONE', #124366, 1000.000000000000000 ) ;
#120633 = CARTESIAN_POINT ( 'NONE',  ( 25.85830628287044064, -1.633150327867689988, 6.094999999999989981 ) ) ;
#120634 = CARTESIAN_POINT ( 'NONE',  ( -1.881878777429229599, 12.51266495272427193, -26.80546393447896847 ) ) ;
#120635 = ORIENTED_EDGE ( 'NONE', *, *, #130114, .T. ) ;
#120636 = PLANE ( 'NONE',  #117424 ) ;
#120637 = ORIENTED_EDGE ( 'NONE', *, *, #130387, .F. ) ;
#120638 = DIRECTION ( 'NONE',  ( 0.7071067811865486830, -0.7071067811865464625, -0.000000000000000000 ) ) ;
#120639 = VECTOR ( 'NONE', #43918, 1000.000000000000000 ) ;
#120640 = CARTESIAN_POINT ( 'NONE',  ( 34.92499999999998295, -8.671992264596198652, 16.70802535927752785 ) ) ;
#120642 = ORIENTED_EDGE ( 'NONE', *, *, #58710, .F. ) ;
#120641 = CARTESIAN_POINT ( 'NONE',  ( -23.67183060077630330, -6.740707523384212863, 4.000000000000000000 ) ) ;
#120643 = VECTOR ( 'NONE', #94481, 1000.000000000000000 ) ;
#120644 = ORIENTED_EDGE ( 'NONE', *, *, #111250, .F. ) ;
#120645 = LINE ( 'NONE', #64879, #70522 ) ;
#120646 = CARTESIAN_POINT ( 'NONE',  ( 13.18000000000000149, 2.055000000000001492, 2.516649172247811554E-16 ) ) ;
#120647 = CARTESIAN_POINT ( 'NONE',  ( -24.70701326429287903, -21.74070752338406365, 4.999753212805221558 ) ) ;
#120648 = ORIENTED_EDGE ( 'NONE', *, *, #74828, .T. ) ;
#120649 = ADVANCED_FACE ( 'NONE', ( #69610 ), #45719, .T. ) ;
#120650 = DIRECTION ( 'NONE',  ( -0.3543493200069163240, -0.000000000000000000, -0.9351131265310288487 ) ) ;
#120651 = VERTEX_POINT ( 'NONE', #100781 ) ;
#120652 = EDGE_LOOP ( 'NONE', ( #2064, #67277, #63739, #32472 ) ) ;
#120653 = AXIS2_PLACEMENT_3D ( 'NONE', #48922, #27139, #126444 ) ;
#120654 = CARTESIAN_POINT ( 'NONE',  ( 3.005480084712505828, 28.92564299267936079, 4.000000000000000000 ) ) ;
#120655 = CARTESIAN_POINT ( 'NONE',  ( 0.000000000000000000, 0.000000000000000000, 5.000000000000000000 ) ) ;
#120656 = AXIS2_PLACEMENT_3D ( 'NONE', #14605, #58887, #125522 ) ;
#120657 = CARTESIAN_POINT ( 'NONE',  ( 2.999999999999981792, -8.151047557385066256, -8.977947279169805839 ) ) ;
#120658 = CARTESIAN_POINT ( 'NONE',  ( 13.82816939922343735, -2.240707523384259492, 4.000000000000000000 ) ) ;
#120659 = PLANE ( 'NONE',  #51482 ) ;
#120660 = DIRECTION ( 'NONE',  ( 0.6830127018922181881, 0.6830127018922202975, -0.2588190451025214056 ) ) ;
#120661 = FACE_OUTER_BOUND ( 'NONE', #123328, .T. ) ;
#120662 = EDGE_CURVE ( 'NONE', #19849, #57984, #11590, .T. ) ;
#120663 = ORIENTED_EDGE ( 'NONE', *, *, #72936, .F. ) ;
#120664 = DIRECTION ( 'NONE',  ( -0.7071067811865486830, 0.7071067811865464625, 0.000000000000000000 ) ) ;
#120665 = EDGE_LOOP ( 'NONE', ( #93940, #88533, #72865, #5917 ) ) ;
#120666 = VECTOR ( 'NONE', #108043, 1000.000000000000000 ) ;
#120667 = CARTESIAN_POINT ( 'NONE',  ( 23.99999999999983302, 12.83542986846999234, -1.025386466790425333 ) ) ;
#120668 = CARTESIAN_POINT ( 'NONE',  ( -8.816011393731004731, 28.73617430169781173, 5.000000000000000000 ) ) ;
#120669 = CARTESIAN_POINT ( 'NONE',  ( -6.489213562373093325, -27.52281430457059841, 5.000000000000000000 ) ) ;
#120670 = ORIENTED_EDGE ( 'NONE', *, *, #91305, .T. ) ;
#120671 = LINE ( 'NONE', #7627, #50664 ) ;
#120672 = LINE ( 'NONE', #40484, #30268 ) ;
#120673 = CARTESIAN_POINT ( 'NONE',  ( 0.000000000000000000, 0.000000000000000000, 5.000000000000000000 ) ) ;
#120674 = ORIENTED_EDGE ( 'NONE', *, *, #33653, .F. ) ;
#120675 = ORIENTED_EDGE ( 'NONE', *, *, #5143, .T. ) ;
#120676 =( NAMED_UNIT ( * ) SI_UNIT ( $, .STERADIAN. ) SOLID_ANGLE_UNIT ( ) );
#120677 = CARTESIAN_POINT ( 'NONE',  ( 17.70025512860841488, -27.71228299555193786, 4.000000000000000000 ) ) ;
#120678 = DIRECTION ( 'NONE',  ( -0.000000000000000000, 0.000000000000000000, 1.000000000000000000 ) ) ;
#120679 = AXIS2_PLACEMENT_3D ( 'NONE', #60820, #104982, #126720 ) ;
#120680 = LINE ( 'NONE', #87374, #80661 ) ;
#120681 = CARTESIAN_POINT ( 'NONE',  ( 67.14126352523145158, 4.472830434245837594, 4.472830434245841147 ) ) ;
#120682 =( BOUNDED_CURVE ( )  B_SPLINE_CURVE ( 3, ( #75507, #41432, #50196, #105270 ),
 .UNSPECIFIED., .F., .F. ) 
 B_SPLINE_CURVE_WITH_KNOTS ( ( 4, 4 ),
 ( 4.350170835173033268, 4.500739107949267570 ),
 .UNSPECIFIED. ) 
 CURVE ( )  GEOMETRIC_REPRESENTATION_ITEM ( )  RATIONAL_B_SPLINE_CURVE ( ( 1.000000000000000000, 0.9981116584018945304, 0.9981116584018945304, 1.000000000000000000 ) ) 
 REPRESENTATION_ITEM ( '' )  );
#120683 = CARTESIAN_POINT ( 'NONE',  ( 20.99999999999985079, -21.84840872380822674, 2.849755605029657080 ) ) ;
#120684 = VECTOR ( 'NONE', #114050, 1000.000000000000000 ) ;
#120685 = VECTOR ( 'NONE', #87992, 1000.000000000000000 ) ;
#120686 = LINE ( 'NONE', #54066, #57768 ) ;
#120687 = PRESENTATION_STYLE_ASSIGNMENT (( #111994 ) ) ;
#120688 = CARTESIAN_POINT ( 'NONE',  ( 14.99999999999989875, -1.209798855135680418, 4.371887122346866050 ) ) ;
#120689 = EDGE_LOOP ( 'NONE', ( #28473, #44332, #15835 ) ) ;
#120690 = DIRECTION ( 'NONE',  ( -0.7071067811865486830, -0.7071067811865464625, 0.000000000000000000 ) ) ;
#120691 = EDGE_CURVE ( 'NONE', #89804, #15358, #46445, .T. ) ;
#120692 = ORIENTED_EDGE ( 'NONE', *, *, #34489, .T. ) ;
#120693 = VECTOR ( 'NONE', #132685, 1000.000000000000000 ) ;
#120694 = COLOUR_RGB ( '', 0.72549020, 0.75294118, 0.79215686) ;
#120695 =( GEOMETRIC_REPRESENTATION_CONTEXT ( 3 ) GLOBAL_UNCERTAINTY_ASSIGNED_CONTEXT ( ( #53504 ) ) GLOBAL_UNIT_ASSIGNED_CONTEXT ( ( #69572, #3529, #89849 ) ) REPRESENTATION_CONTEXT ( 'NONE', 'WORKASPACE' ) );
#120696 = CARTESIAN_POINT ( 'NONE',  ( -50.99451991528749062, 28.92564299267973738, 4.000000000000000000 ) ) ;
#120698 = CARTESIAN_POINT ( 'NONE',  ( 33.18398860626899705, 28.73617430169810305, 5.000000000000000000 ) ) ;
#120697 = AXIS2_PLACEMENT_3D ( 'NONE', #68909, #47191, #91374 ) ;
#120699 = ORIENTED_EDGE ( 'NONE', *, *, #72703, .F. ) ;
#120700 = VECTOR ( 'NONE', #14756, 1000.000000000000000 ) ;
#120701 = DIRECTION ( 'NONE',  ( 1.000000000000000000, 0.000000000000000000, 0.000000000000000000 ) ) ;
#120702 = LINE ( 'NONE', #74384, #35063 ) ;
#120703 = FACE_OUTER_BOUND ( 'NONE', #86302, .T. ) ;
#120704 = CARTESIAN_POINT ( 'NONE',  ( 17.99999999999987210, -10.06887692260770883, 4.000000000000000000 ) ) ;
#120705 = CARTESIAN_POINT ( 'NONE',  ( 12.18398860626900060, 28.73617430169795739, 5.000000000000000000 ) ) ;
#120706 = EDGE_CURVE ( 'NONE', #4422, #96831, #102230, .T. ) ;
#120707 = EDGE_CURVE ( 'NONE', #11393, #16533, #134137, .T. ) ;
#120708 = ORIENTED_EDGE ( 'NONE', *, *, #123265, .F. ) ;
#120709 = ORIENTED_EDGE ( 'NONE', *, *, #92583, .T. ) ;
#120710 = DIRECTION ( 'NONE',  ( -0.000000000000000000, 0.3543493200069153248, 0.9351131265310292928 ) ) ;
#120711 = DIRECTION ( 'NONE',  ( 0.7071067811865487940, 0.7071067811865463515, -0.000000000000000000 ) ) ;
#120712 = VECTOR ( 'NONE', #33079, 1000.000000000000227 ) ;
#120713 = FACE_OUTER_BOUND ( 'NONE', #38477, .T. ) ;
#120714 = FACE_OUTER_BOUND ( 'NONE', #82887, .T. ) ;
#120715 = EDGE_CURVE ( 'NONE', #60685, #64647, #1434, .T. ) ;
#120717 = EDGE_CURVE ( 'NONE', #24671, #103081, #86920, .T. ) ;
#120716 = CARTESIAN_POINT ( 'NONE',  ( 89.18336038379621300, -2.130196079827426203, 7.949999999999997513 ) ) ;
#120718 = LINE ( 'NONE', #112709, #134304 ) ;
#120719 = CARTESIAN_POINT ( 'NONE',  ( -54.18398860626899705, 28.73617430169825226, 5.000000000000000000 ) ) ;
#120721 = EDGE_CURVE ( 'NONE', #82404, #1460, #58813, .T. ) ;
#120720 = VERTEX_POINT ( 'NONE', #45021 ) ;
#120722 = CARTESIAN_POINT ( 'NONE',  ( 83.39583333333334281, -2.130196079827427091, 7.949999999999999289 ) ) ;
#120723 = VECTOR ( 'NONE', #135116, 999.9999999999998863 ) ;
#120724 = CARTESIAN_POINT ( 'NONE',  ( 1.320799999999990870, 1.617513596018363294E-16, 3.775643966265890494 ) ) ;
#120725 = EDGE_CURVE ( 'NONE', #31625, #21087, #80478, .T. ) ;
#120726 = LINE ( 'NONE', #97548, #73896 ) ;
#120727 = DIRECTION ( 'NONE',  ( 0.7071067811865487940, 0.7071067811865463515, -0.000000000000000000 ) ) ;
#120728 = EDGE_CURVE ( 'NONE', #104374, #927, #133423, .T. ) ;
#120729 = ORIENTED_EDGE ( 'NONE', *, *, #125279, .T. ) ;
#120730 = AXIS2_PLACEMENT_3D ( 'NONE', #64636, #108818, #76234 ) ;
#120731 = LINE ( 'NONE', #119990, #100028 ) ;
#120733 = ORIENTED_EDGE ( 'NONE', *, *, #69919, .T. ) ;
#120732 = EDGE_CURVE ( 'NONE', #55021, #122835, #123274, .T. ) ;
#120734 = VECTOR ( 'NONE', #12182, 1000.000000000000000 ) ;
#120735 = CARTESIAN_POINT ( 'NONE',  ( 75.54209685856477563, 5.291415217122923842, -3.054999999999996163 ) ) ;
#120736 = VECTOR ( 'NONE', #65042, 1000.000000000000000 ) ;
#120737 = DIRECTION ( 'NONE',  ( 0.7071067811865486830, -0.7071067811865464625, -0.000000000000000000 ) ) ;
#120738 = VERTEX_POINT ( 'NONE', #3571 ) ;
#120739 = VECTOR ( 'NONE', #124645, 999.9999999999998863 ) ;
#120740 = CARTESIAN_POINT ( 'NONE',  ( -42.18398860626899705, 28.73617430169816700, 5.000000000000000000 ) ) ;
#120741 = CARTESIAN_POINT ( 'NONE',  ( 6.183988606268994381, 28.73617430169791476, 5.000000000000000000 ) ) ;
#120742 = EDGE_CURVE ( 'NONE', #142125, #1490, #90636, .T. ) ;
#120743 = LINE ( 'NONE', #98982, #72025 ) ;
#120744 = DIRECTION ( 'NONE',  ( 0.3543493200069162685, -0.000000000000000000, -0.9351131265310288487 ) ) ;
#120745 = CARTESIAN_POINT ( 'NONE',  ( 55.32809448528701779, -52.14999999999999147, 41.05261164187027845 ) ) ;
#120747 = ORIENTED_EDGE ( 'NONE', *, *, #43235, .T. ) ;
#120746 = DIRECTION ( 'NONE',  ( -0.7071067811865486830, -0.7071067811865463515, 0.000000000000000000 ) ) ;
#120748 = DIRECTION ( 'NONE',  ( 0.7071067811865487940, 0.7071067811865463515, -0.000000000000000000 ) ) ;
#120749 = DIRECTION ( 'NONE',  ( -0.000000000000000000, 0.3543493200069153248, 0.9351131265310292928 ) ) ;
#120750 = CARTESIAN_POINT ( 'NONE',  ( 77.85416666666667140, -2.130196079827425759, -7.950000000000000178 ) ) ;
#120751 = EDGE_CURVE ( 'NONE', #26035, #119060, #103605, .T. ) ;
#120752 = DIRECTION ( 'NONE',  ( -0.6830127018922180770, -0.6830127018922204085, -0.2588190451025213501 ) ) ;
#120753 = ORIENTED_EDGE ( 'NONE', *, *, #17027, .F. ) ;
#120754 = ORIENTED_EDGE ( 'NONE', *, *, #58621, .T. ) ;
#120755 = CARTESIAN_POINT ( 'NONE',  ( 64.16709685856476142, -3.055000000000000160, -5.291415217122921177 ) ) ;
#120756 = ORIENTED_EDGE ( 'NONE', *, *, #71068, .F. ) ;
#120758 = LINE ( 'NONE', #118617, #12872 ) ;
#120757 = PRODUCT ( 'slotted set screw dog point_iso_ISO 7435 - M5 x 25-S', 'slotted set screw dog point_iso_ISO 7435 - M5 x 25-S', '', ( #104001 ) ) ;
#120759 = CARTESIAN_POINT ( 'NONE',  ( 0.000000000000000000, 0.000000000000000000, 5.000000000000000000 ) ) ;
#120760 = DIRECTION ( 'NONE',  ( -0.7071067811865487940, 0.7071067811865463515, -0.000000000000000000 ) ) ;
#120761 = VERTEX_POINT ( 'NONE', #40532 ) ;
#120762 = ORIENTED_EDGE ( 'NONE', *, *, #2589, .T. ) ;
#120763 = VECTOR ( 'NONE', #77755, 1000.000000000000000 ) ;
#120764 = DIRECTION ( 'NONE',  ( -0.7071067811865487940, 0.7071067811865463515, -0.000000000000000000 ) ) ;
#120765 = DIRECTION ( 'NONE',  ( 0.7071067811865486830, -0.7071067811865464625, -0.000000000000000000 ) ) ;
#120766 = EDGE_CURVE ( 'NONE', #75424, #26817, #126791, .T. ) ;
#120767 = ORIENTED_EDGE ( 'NONE', *, *, #55282, .F. ) ;
#120768 = CARTESIAN_POINT ( 'NONE',  ( 17.51078643762690845, -27.52281430457043143, 5.000000000000000000 ) ) ;
#120769 = ADVANCED_FACE ( 'NONE', ( #60152 ), #62285, .F. ) ;
#120770 = LINE ( 'NONE', #63587, #112669 ) ;
#120771 = DIRECTION ( 'NONE',  ( 0.7071067811865487940, -0.7071067811865463515, 0.000000000000000000 ) ) ;
#120772 = VECTOR ( 'NONE', #86470, 1000.000000000000000 ) ;
#120773 = EDGE_CURVE ( 'NONE', #23176, #42427, #106443, .T. ) ;
#120774 = ORIENTED_EDGE ( 'NONE', *, *, #59729, .F. ) ;
#120775 = FACE_BOUND ( 'NONE', #84166, .T. ) ;
#120776 = CARTESIAN_POINT ( 'NONE',  ( -7.998069433178966570, -22.22500000000000142, 4.500000000000000888 ) ) ;
#120777 = CARTESIAN_POINT ( 'NONE',  ( 19.41972383043609440, 4.584330080086930965E-16, 0.000000000000000000 ) ) ;
#120778 = FACE_OUTER_BOUND ( 'NONE', #91053, .T. ) ;
#120779 = VECTOR ( 'NONE', #81557, 1000.000000000000000 ) ;
#120780 = LINE ( 'NONE', #10576, #115204 ) ;
#120781 = DIRECTION ( 'NONE',  ( 0.000000000000000000, -1.000000000000000000, 0.000000000000000000 ) ) ;
#120782 = FILL_AREA_STYLE ('',( #108446 ) ) ;
#120783 = ORIENTED_EDGE ( 'NONE', *, *, #44063, .F. ) ;
#120784 = EDGE_LOOP ( 'NONE', ( #116954, #104984, #122819 ) ) ;
#120785 = CARTESIAN_POINT ( 'NONE',  ( 115.5579301918981088, 6.110000000000000320, -1.637169565754156064 ) ) ;
#120786 = ORIENTED_EDGE ( 'NONE', *, *, #103747, .T. ) ;
#120787 = ADVANCED_FACE ( 'NONE', ( #114491 ), #26084, .F. ) ;
#120788 = ORIENTED_EDGE ( 'NONE', *, *, #57115, .T. ) ;
#120789 = CARTESIAN_POINT ( 'NONE',  ( 183.7880820442500749, -48.99280962439389953, 39.49606053969937847 ) ) ;
#120790 = VECTOR ( 'NONE', #110507, 1000.000000000000000 ) ;
#120791 = VECTOR ( 'NONE', #73963, 1000.000000000000000 ) ;
#120792 = LINE ( 'NONE', #109209, #31638 ) ;
#120793 = AXIS2_PLACEMENT_3D ( 'NONE', #74505, #29526, #99057 ) ;
#120794 = VECTOR ( 'NONE', #68950, 1000.000000000000227 ) ;
#120795 = CARTESIAN_POINT ( 'NONE',  ( 13.43359823057990354, 1.153863645259229909, 4.000000000000000000 ) ) ;
#120796 = VERTEX_POINT ( 'NONE', #71740 ) ;
#120797 = CARTESIAN_POINT ( 'NONE',  ( 69.20419371712955581, -6.884901960086285300, -3.975000000000000089 ) ) ;
#120798 = DIRECTION ( 'NONE',  ( -0.6830127018922181881, 0.6830127018922202975, -0.2588190451025214056 ) ) ;
#120799 = EDGE_CURVE ( 'NONE', #86413, #8053, #128254, .T. ) ;
#120800 = CARTESIAN_POINT ( 'NONE',  ( 58.99586038379622721, -3.974999999999998312, -6.884901960086286188 ) ) ;
#120801 = DIRECTION ( 'NONE',  ( 0.7071067811865486830, -0.7071067811865464625, -0.000000000000000000 ) ) ;
#120802 = VECTOR ( 'NONE', #80828, 1000.000000000000000 ) ;
#120803 = VECTOR ( 'NONE', #17818, 1000.000000000000000 ) ;
#120804 = AXIS2_PLACEMENT_3D ( 'NONE', #76590, #65735, #121482 ) ;
#120805 = CARTESIAN_POINT ( 'NONE',  ( 0.5865329486478585430, 1.186553054598157964, 3.957575763987766670 ) ) ;
#120806 = VERTEX_POINT ( 'NONE', #49286 ) ;
#120807 = FACE_OUTER_BOUND ( 'NONE', #99343, .T. ) ;
#120808 = LINE ( 'NONE', #55581, #118303 ) ;
#120809 = ORIENTED_EDGE ( 'NONE', *, *, #7084, .F. ) ;
#120810 = EDGE_CURVE ( 'NONE', #86478, #71183, #105738, .T. ) ;
#120811 = EDGE_LOOP ( 'NONE', ( #92023, #7440, #21135, #24969 ) ) ;
#120812 = ORIENTED_EDGE ( 'NONE', *, *, #8731, .T. ) ;
#120813 = CARTESIAN_POINT ( 'NONE',  ( 63.14626352523143282, -4.472830434245840259, 4.472830434245838482 ) ) ;
#120814 = ORIENTED_EDGE ( 'NONE', *, *, #49627, .T. ) ;
#120815 = DIRECTION ( 'NONE',  ( 1.000000000000000000, 0.000000000000000000, 0.000000000000000000 ) ) ;
#120816 = EDGE_CURVE ( 'NONE', #32877, #142614, #94165, .T. ) ;
#120817 = CARTESIAN_POINT ( 'NONE',  ( -1.120860383796227655, -5.278424836066145431, -3.047499999999993658 ) ) ;
#120818 = CARTESIAN_POINT ( 'NONE',  ( 99.16709685856477563, -3.055000000000000160, -5.291415217122921177 ) ) ;
#120819 = CARTESIAN_POINT ( 'NONE',  ( 42.18398860626899705, 28.73617430169816700, 5.000000000000000000 ) ) ;
#120820 = VERTEX_POINT ( 'NONE', #139131 ) ;
#120821 = DIRECTION ( 'NONE',  ( 0.6830127018922180770, -0.6830127018922204085, -0.2588190451025213501 ) ) ;
#120822 = DIRECTION ( 'NONE',  ( 0.000000000000000000, 5.782411586589356455E-15, -1.000000000000000000 ) ) ;
#120823 = ADVANCED_FACE ( 'NONE', ( #7125 ), #27477, .F. ) ;
#120824 = CARTESIAN_POINT ( 'NONE',  ( 33.48921356237309510, -27.52281430457078670, 5.000000000000000000 ) ) ;
#120825 = CIRCLE ( 'NONE', #19009, 2.000000000000001776 ) ;
#120826 = FACE_OUTER_BOUND ( 'NONE', #112552, .T. ) ;
#120827 = EDGE_LOOP ( 'NONE', ( #14073, #62943, #17687, #49720 ) ) ;
#120828 = AXIS2_PLACEMENT_3D ( 'NONE', #130804, #19156, #9692 ) ;
#120829 = EDGE_CURVE ( 'NONE', #8757, #16774, #82596, .T. ) ;
#120830 = CARTESIAN_POINT ( 'NONE',  ( 0.000000000000000000, 0.000000000000000000, 5.000000000000000000 ) ) ;
#120831 = ORIENTED_EDGE ( 'NONE', *, *, #54152, .F. ) ;
#120832 = VECTOR ( 'NONE', #107278, 1000.000000000000000 ) ;
#120833 = EDGE_LOOP ( 'NONE', ( #14517, #107342, #102161, #32730 ) ) ;
#120834 = ORIENTED_EDGE ( 'NONE', *, *, #33224, .T. ) ;
#120835 = CARTESIAN_POINT ( 'NONE',  ( 119.9329301918981088, 1.637169565754156508, 6.110000000000000320 ) ) ;
#120836 = ORIENTED_EDGE ( 'NONE', *, *, #131844, .T. ) ;
#120837 = VECTOR ( 'NONE', #134310, 999.9999999999998863 ) ;
#120838 = CARTESIAN_POINT ( 'NONE',  ( 6.940000000000001279, 2.055000000000001492, 0.000000000000000000 ) ) ;
#120839 = LINE ( 'NONE', #110652, #132012 ) ;
#120840 = EDGE_CURVE ( 'NONE', #70901, #92286, #49982, .T. ) ;
#120841 = EDGE_LOOP ( 'NONE', ( #69674, #130819, #115906, #139637 ) ) ;
#120842 = CARTESIAN_POINT ( 'NONE',  ( -34.92500000000001137, 6.759292476615653023, 4.255531930566238685 ) ) ;
#120843 = ORIENTED_EDGE ( 'NONE', *, *, #99117, .F. ) ;
#120844 = VECTOR ( 'NONE', #61827, 1000.000000000000000 ) ;
#120845 = CARTESIAN_POINT ( 'NONE',  ( 15.14540314143522082, -2.126176841940958351, -7.934999999999989839 ) ) ;
#120846 = DIRECTION ( 'NONE',  ( -0.6830127018922181881, 0.6830127018922202975, -0.2588190451025214056 ) ) ;
#120847 = CARTESIAN_POINT ( 'NONE',  ( -0.7071067811865363595, 20.25929247661552424, 5.000000000000000000 ) ) ;
#120848 =( BOUNDED_CURVE ( )  B_SPLINE_CURVE ( 2, ( #136282, #47206, #114526, #92775, #37716, #113100, #59478, #24665, #23221, #2909, #91385, #12361, #57335, #35597, #3600, #124703, #90671, #79823, #70372, #112407, #13062, #15201, #103635, #4277, #48571, #56645, #45750, #89921, #134162, #34861, #126824, #28963, #7164, #71060, #38414, #96313, #140562, #6432, #51440, #60925, #95632, #84768, #39867, #41247, #94199, #94904, #128978, #139171, #40563, #137740, #138442, #115207, #82633, #18038, #60180, #7893, #39130, #105084, #27509, #15891, #71772, #104354, #5019, #117365, #49317, #116676, #93504, #52135, #61621, #26811, #126140, #62321, #115937, #16639, #50016, #5747, #73895, #83348, #84089, #17360, #118064, #107220, #73200, #127560, #128283, #28254, #18775, #105773, #72513, #139888, #50717, #106475, #29650, #63048, #53576, #22324, #9293, #20194, #54312, #74623, #110065, #44129, #20916, #76778, #55723, #11451, #64436, #21657, #33286, #108618, #8575, #97022, #97779, #76034, #41992, #86202, #42714, #19501, #141274, #86917, #66595, #31814, #99927, #131129, #590, #65181, #109368, #118812, #119500, #142717, #10739, #43407, #55012, #99175, #77488, #130428, #31116, #75334, #85457, #129683, #107908, #52823, #23798, #123842, #12190, #101346, #45581, #135434, #69463, #133289, #100651, #59313, #103468, #68751, #58626, #112240, #102798, #78914, #112934, #136113, #124535, #13600, #81047, #57884, #57171, #44888, #125246, #122366, #36116, #102068, #67310, #1297, #133983, #2740, #47039, #1986, #25205 ),
 .UNSPECIFIED., .F., .T. ) 
 B_SPLINE_CURVE_WITH_KNOTS ( ( 3, 2, 2, 2, 2, 2, 2, 2, 2, 2, 2, 2, 2, 2, 2, 2, 2, 2, 2, 2, 2, 2, 2, 2, 2, 2, 2, 2, 2, 2, 2, 2, 2, 2, 2, 2, 2, 2, 2, 2, 2, 2, 2, 2, 2, 2, 2, 2, 2, 2, 2, 2, 2, 2, 2, 2, 2, 2, 2, 2, 2, 2, 2, 2, 2, 2, 2, 2, 2, 2, 2, 2, 2, 2, 2, 2, 2, 2, 2, 2, 2, 2, 2, 2, 2, 2, 2, 2, 3 ),
 ( 0.05679457295752499135, 0.05833333333333333426, 0.06666666666666666574, 0.07499999999999999722, 0.08333333333333332871, 0.09166666666666666019, 0.1000000000000000056, 0.1083333333333333370, 0.1166666666666666685, 0.1250000000000000000, 0.1333333333333333315, 0.1416666666666666630, 0.1499999999999999944, 0.1583333333333333259, 0.1666666666666666574, 0.1749999999999999889, 0.1833333333333333204, 0.1916666666666666796, 0.2000000000000000111, 0.2083333333333333426, 0.2166666666666666741, 0.2250000000000000056, 0.2333333333333333093, 0.2416666666666666685, 0.2500000000000000000, 0.2583333333333333592, 0.2666666666666666630, 0.2750000000000000222, 0.2833333333333333259, 0.2916666666666666852, 0.2999999999999999889, 0.3083333333333333481, 0.3166666666666666519, 0.3250000000000000111, 0.3333333333333333148, 0.3416666666666666741, 0.3499999999999999778, 0.3583333333333333370, 0.3666666666666666408, 0.3750000000000000000, 0.3833333333333333592, 0.3916666666666666630, 0.4000000000000000222, 0.4083333333333333259, 0.4166666666666666297, 0.4249999999999999889, 0.4333333333333333481, 0.4416666666666666519, 0.4500000000000000666, 0.4583333333333332593, 0.4666666666666666741, 0.4749999999999999778, 0.4833333333333333370, 0.4916666666666666408, 0.5000000000000000000, 0.5083333333333333037, 0.5166666666666668295, 0.5250000000000001332, 0.5333333333333332149, 0.5416666666666665186, 0.5500000000000000444, 0.5583333333333333481, 0.5666666666666666519, 0.5749999999999999556, 0.5833333333333333703, 0.5916666666666666741, 0.5999999999999999778, 0.6083333333333332815, 0.6166666666666666963, 0.6250000000000000000, 0.6333333333333333037, 0.6416666666666667185, 0.6500000000000000222, 0.6583333333333333259, 0.6666666666666666297, 0.6750000000000000444, 0.6833333333333333481, 0.6916666666666666519, 0.6999999999999999556, 0.7083333333333333703, 0.7166666666666666741, 0.7249999999999999778, 0.7333333333333332815, 0.7416666666666666963, 0.7500000000000000000, 0.7583333333333333037, 0.7666666666666667185, 0.7750000000000001332, 0.7779834993852963176 ),
 .UNSPECIFIED. ) 
 CURVE ( )  GEOMETRIC_REPRESENTATION_ITEM ( )  RATIONAL_B_SPLINE_CURVE ( ( 0.9897399144606364718, 0.9937081613986249451, 1.000000000000000000, 0.9659258262890683122, 1.000000000000000000, 0.9659258262890683122, 1.000000000000000000, 0.9659258262890683122, 1.000000000000000000, 0.9659258262890683122, 1.000000000000000000, 0.9659258262890683122, 1.000000000000000000, 0.9659258262890683122, 1.000000000000000000, 0.9659258262890683122, 1.000000000000000000, 0.9659258262890683122, 1.000000000000000000, 0.9659258262890683122, 1.000000000000000000, 0.9659258262890683122, 1.000000000000000000, 0.9659258262890683122, 1.000000000000000000, 0.9659258262890683122, 1.000000000000000000, 0.9659258262890683122, 1.000000000000000000, 0.9659258262890683122, 1.000000000000000000, 0.9659258262890683122, 1.000000000000000000, 0.9659258262890683122, 1.000000000000000000, 0.9659258262890683122, 1.000000000000000000, 0.9659258262890683122, 1.000000000000000000, 0.9659258262890683122, 1.000000000000000000, 0.9659258262890683122, 1.000000000000000000, 0.9659258262890683122, 1.000000000000000000, 0.9659258262890683122, 1.000000000000000000, 0.9659258262890683122, 1.000000000000000000, 0.9659258262890683122, 1.000000000000000000, 0.9659258262890683122, 1.000000000000000000, 0.9659258262890683122, 1.000000000000000000, 0.9659258262890683122, 1.000000000000000000, 0.9659258262890683122, 1.000000000000000000, 0.9659258262890683122, 1.000000000000000000, 0.9659258262890683122, 1.000000000000000000, 0.9659258262890683122, 1.000000000000000000, 0.9659258262890683122, 1.000000000000000000, 0.9659258262890683122, 1.000000000000000000, 0.9659258262890683122, 1.000000000000000000, 0.9659258262890683122, 1.000000000000000000, 0.9659258262890683122, 1.000000000000000000, 0.9659258262890683122, 1.000000000000000000, 0.9659258262890683122, 1.000000000000000000, 0.9659258262890683122, 1.000000000000000000, 0.9659258262890683122, 1.000000000000000000, 0.9659258262890683122, 1.000000000000000000, 0.9659258262890683122, 1.000000000000000000, 0.9659258262890683122, 1.000000000000000000, 0.9659258262890683122, 1.000000000000000000, 0.9659258262890683122, 1.000000000000000000, 0.9659258262890683122, 1.000000000000000000, 0.9659258262890683122, 1.000000000000000000, 0.9659258262890683122, 1.000000000000000000, 0.9659258262890683122, 1.000000000000000000, 0.9659258262890683122, 1.000000000000000000, 0.9659258262890683122, 1.000000000000000000, 0.9659258262890683122, 1.000000000000000000, 0.9659258262890683122, 1.000000000000000000, 0.9659258262890683122, 1.000000000000000000, 0.9659258262890683122, 1.000000000000000000, 0.9659258262890683122, 1.000000000000000000, 0.9659258262890683122, 1.000000000000000000, 0.9659258262890683122, 1.000000000000000000, 0.9659258262890683122, 1.000000000000000000, 0.9659258262890683122, 1.000000000000000000, 0.9659258262890683122, 1.000000000000000000, 0.9659258262890683122, 1.000000000000000000, 0.9659258262890683122, 1.000000000000000000, 0.9659258262890683122, 1.000000000000000000, 0.9659258262890683122, 1.000000000000000000, 0.9659258262890683122, 1.000000000000000000, 0.9659258262890683122, 1.000000000000000000, 0.9659258262890683122, 1.000000000000000000, 0.9659258262890683122, 1.000000000000000000, 0.9659258262890683122, 1.000000000000000000, 0.9659258262890683122, 1.000000000000000000, 0.9659258262890683122, 1.000000000000000000, 0.9659258262890683122, 1.000000000000000000, 0.9659258262890683122, 1.000000000000000000, 0.9659258262890683122, 1.000000000000000000, 0.9659258262890683122, 1.000000000000000000, 0.9659258262890683122, 1.000000000000000000, 0.9659258262890683122, 1.000000000000000000, 0.9659258262890683122, 1.000000000000000000, 0.9659258262890683122, 1.000000000000000000, 0.9659258262890683122, 1.000000000000000000, 0.9659258262890683122, 1.000000000000000000, 0.9659258262890683122, 1.000000000000000000, 0.9659258262890683122, 1.000000000000000000, 0.9659258262890683122, 1.000000000000000000, 0.9659258262890683122, 1.000000000000000000, 0.9878007668414741094, 0.9843366707940401916 ) ) 
 REPRESENTATION_ITEM ( '' )  );
#120849 = CARTESIAN_POINT ( 'NONE',  ( -14.99999999999989164, 16.55218569542900298, 5.000000000000000000 ) ) ;
#120850 = EDGE_LOOP ( 'NONE', ( #101646, #92015, #88028, #16974 ) ) ;
#120851 = ORIENTED_EDGE ( 'NONE', *, *, #35265, .F. ) ;
#120852 = VECTOR ( 'NONE', #102053, 999.9999999999998863 ) ;
#120853 = ORIENTED_EDGE ( 'NONE', *, *, #79095, .T. ) ;
#120854 = CARTESIAN_POINT ( 'NONE',  ( 19.83333333333333570, 5.278424836066143655, -3.047499999999997655 ) ) ;
#120855 = CARTESIAN_POINT ( 'NONE',  ( 181.1500000000000057, -43.14999999999999147, 40.92499999999998295 ) ) ;
#120856 = VECTOR ( 'NONE', #116617, 999.9999999999998863 ) ;
#120857 = CARTESIAN_POINT ( 'NONE',  ( -34.92500000000001137, -22.22500000000000142, 4.500000000000000888 ) ) ;
#120858 = DIRECTION ( 'NONE',  ( -0.6830127018922180770, -0.6830127018922204085, -0.2588190451025213501 ) ) ;
#120859 = FACE_OUTER_BOUND ( 'NONE', #25626, .T. ) ;
#120860 = CARTESIAN_POINT ( 'NONE',  ( 28.29209685856476497, -5.291415217122921177, 3.054999999999999272 ) ) ;
#120861 = LINE ( 'NONE', #44798, #41758 ) ;
#120862 = DIRECTION ( 'NONE',  ( 0.7071067811865487940, 0.7071067811865463515, 0.000000000000000000 ) ) ;
#120863 = ORIENTED_EDGE ( 'NONE', *, *, #110836, .T. ) ;
#120864 = CARTESIAN_POINT ( 'NONE',  ( 15.18398860626900237, 28.73617430169797871, 5.000000000000000000 ) ) ;
#120865 = ADVANCED_FACE ( 'NONE', ( #6399 ), #38381, .F. ) ;
#120866 = VECTOR ( 'NONE', #63836, 1000.000000000000000 ) ;
#120867 = EDGE_LOOP ( 'NONE', ( #90130, #30893, #65315, #101490 ) ) ;
#120868 = CARTESIAN_POINT ( 'NONE',  ( -21.79614956108759216, 8.475608720613168501, 4.664130618528514738 ) ) ;
#120869 = ORIENTED_EDGE ( 'NONE', *, *, #47023, .T. ) ;
#120870 = CARTESIAN_POINT ( 'NONE',  ( 18.12913961620377279, 5.278424836066147208, 3.047499999999990550 ) ) ;
#120872 = ORIENTED_EDGE ( 'NONE', *, *, #17825, .T. ) ;
#120871 = CARTESIAN_POINT ( 'NONE',  ( 42.56249999999998579, -5.819803920172573086, -5.819803920172573974 ) ) ;
#120873 = CARTESIAN_POINT ( 'NONE',  ( -45.29974487139158867, -27.71228299555237840, 4.000000000000000000 ) ) ;
#120874 = EDGE_CURVE ( 'NONE', #42386, #11025, #37685, .T. ) ;
#120875 = EDGE_LOOP ( 'NONE', ( #75079, #142105, #24404 ) ) ;
#120876 = CARTESIAN_POINT ( 'NONE',  ( 15.79289321881335084, -14.24070752338414003, 5.000000000000000000 ) ) ;
#120878 = ORIENTED_EDGE ( 'NONE', *, *, #140476, .T. ) ;
#120877 = VECTOR ( 'NONE', #132710, 1000.000000000000000 ) ;
#120879 = DIRECTION ( 'NONE',  ( -0.7071067811865486830, -0.7071067811865464625, 0.000000000000000000 ) ) ;
#120880 = EDGE_LOOP ( 'NONE', ( #75752, #93969, #125004, #102108 ) ) ;
#120881 = LINE ( 'NONE', #22972, #52220 ) ;
#120883 = EDGE_CURVE ( 'NONE', #9195, #91342, #95600, .T. ) ;
#120882 = CARTESIAN_POINT ( 'NONE',  ( 112.8083603837962414, 7.949999999999997513, 2.130196079827431088 ) ) ;
#120884 = DIRECTION ( 'NONE',  ( 0.7071067811865487940, 0.7071067811865463515, 0.000000000000000000 ) ) ;
#120885 = DIRECTION ( 'NONE',  ( -0.7071067811865487940, 0.7071067811865463515, -0.000000000000000000 ) ) ;
#120886 = ADVANCED_FACE ( 'NONE', ( #81925 ), #117332, .F. ) ;
#120887 = PRESENTATION_STYLE_ASSIGNMENT (( #90413 ) ) ;
#120888 = CARTESIAN_POINT ( 'NONE',  ( 13.49999999999991473, 16.46639925780209524, 5.000000000000000000 ) ) ;
#120889 = EDGE_CURVE ( 'NONE', #69156, #42684, #18004, .T. ) ;
#120890 = CARTESIAN_POINT ( 'NONE',  ( -62.99451991528749772, 28.92564299267982264, 4.000000000000000000 ) ) ;
#120891 = CARTESIAN_POINT ( 'NONE',  ( 6.562500000000000888, 4.461849672132300881, 4.461849672132299105 ) ) ;
#120892 = CARTESIAN_POINT ( 'NONE',  ( 15.87456980810188867, 6.871911579029510442, -3.967499999999998916 ) ) ;
#120893 = AXIS2_PLACEMENT_3D ( 'NONE', #139820, #60850, #105005 ) ;
#120894 = VECTOR ( 'NONE', #67388, 999.9999999999998863 ) ;
#120896 = CARTESIAN_POINT ( 'NONE',  ( 14.99999999999990408, 10.55218569542906515, 5.000000000000000000 ) ) ;
#120895 = AXIS2_PLACEMENT_3D ( 'NONE', #102257, #13765, #2163 ) ;
#120898 = EDGE_CURVE ( 'NONE', #104048, #109338, #4985, .T. ) ;
#120897 = DIRECTION ( 'NONE',  ( 0.000000000000000000, -1.000000000000000000, 0.000000000000000000 ) ) ;
#120899 = ORIENTED_EDGE ( 'NONE', *, *, #53013, .T. ) ;
#120900 = ORIENTED_EDGE ( 'NONE', *, *, #132337, .F. ) ;
#120901 = AXIS2_PLACEMENT_3D ( 'NONE', #3318, #135996, #93912 ) ;
#120902 = VECTOR ( 'NONE', #110795, 1000.000000000000000 ) ;
#120903 = DIRECTION ( 'NONE',  ( -0.7071067811865487940, 0.7071067811865463515, -0.000000000000000000 ) ) ;
#120904 = ORIENTED_EDGE ( 'NONE', *, *, #116140, .T. ) ;
#120905 = EDGE_CURVE ( 'NONE', #69571, #32830, #131725, .T. ) ;
#120906 = CARTESIAN_POINT ( 'NONE',  ( -0.7070132642930445632, -21.74070752338405654, 4.999753212805222446 ) ) ;
#120907 = CARTESIAN_POINT ( 'NONE',  ( 0.000000000000000000, 0.000000000000000000, 5.000000000000000000 ) ) ;
#120908 = AXIS2_PLACEMENT_3D ( 'NONE', #46644, #35753, #14674 ) ;
#120910 = AXIS2_PLACEMENT_3D ( 'NONE', #61237, #93097, #126421 ) ;
#120909 = DIRECTION ( 'NONE',  ( -0.000000000000000000, -0.3543493200069152693, 0.9351131265310292928 ) ) ;
#120911 = VECTOR ( 'NONE', #65557, 1000.000000000000000 ) ;
#120912 = CARTESIAN_POINT ( 'NONE',  ( 130.9531400719789929, -48.66302742222529076, -38.53170190052241395 ) ) ;
#120913 = ORIENTED_EDGE ( 'NONE', *, *, #95956, .F. ) ;
#120914 = FACE_OUTER_BOUND ( 'NONE', #42937, .T. ) ;
#120915 = DIRECTION ( 'NONE',  ( 0.5735764363510448272, -0.8191520442889927978, 1.003171929053526103E-16 ) ) ;
#120916 = ADVANCED_FACE ( 'NONE', ( #110037 ), #86885, .F. ) ;
#120917 = DIRECTION ( 'NONE',  ( 1.000000000000000000, 0.000000000000000000, 0.000000000000000000 ) ) ;
#120918 = ADVANCED_FACE ( 'NONE', ( #118034 ), #43380, .T. ) ;
#120919 = CARTESIAN_POINT ( 'NONE',  ( 0.7933393645784738712, 21.75929247661549937, 4.998822639870705409 ) ) ;
#120920 = DIRECTION ( 'NONE',  ( -0.7071067811865486830, -0.7071067811865464625, 0.000000000000000000 ) ) ;
#120922 = ORIENTED_EDGE ( 'NONE', *, *, #71155, .T. ) ;
#120921 = CARTESIAN_POINT ( 'NONE',  ( 48.48921356237309510, -27.52281430457089328, 5.000000000000000000 ) ) ;
#120923 = CARTESIAN_POINT ( 'NONE',  ( -12.79289321881336683, -20.24070752338407431, 5.000000000000000000 ) ) ;
#120924 = CARTESIAN_POINT ( 'NONE',  ( 70.85416666666669983, -2.130196079827501698, -7.949999999999956657 ) ) ;
#120925 = LINE ( 'NONE', #129654, #78033 ) ;
#120926 = EDGE_CURVE ( 'NONE', #51106, #94631, #20163, .T. ) ;
#120927 = DIRECTION ( 'NONE',  ( -0.7071067811865486830, -0.7071067811865464625, 0.000000000000000000 ) ) ;
#120928 = VERTEX_POINT ( 'NONE', #63014 ) ;
#120929 = ORIENTED_EDGE ( 'NONE', *, *, #32400, .T. ) ;
#120930 = VERTEX_POINT ( 'NONE', #107188 ) ;
#120931 = CARTESIAN_POINT ( 'NONE',  ( 89.97959685856477563, 6.109999999999999432, 1.637169565754164280 ) ) ;
#120932 = EDGE_LOOP ( 'NONE', ( #102299, #78605, #44029, #137311 ) ) ;
#120933 = DIRECTION ( 'NONE',  ( 1.000000000000000000, 0.000000000000000000, 0.000000000000000000 ) ) ;
#120934 = CARTESIAN_POINT ( 'NONE',  ( 1.042387978378689795, -2.055000000000000160, 0.000000000000000000 ) ) ;
#120935 = ORIENTED_EDGE ( 'NONE', *, *, #6099, .T. ) ;
#120936 = DIRECTION ( 'NONE',  ( -0.7071067811865486830, 0.7071067811865464625, 0.000000000000000000 ) ) ;
#120937 = CARTESIAN_POINT ( 'NONE',  ( 17.29289321881334018, -15.74070752338412049, 5.000000000000000000 ) ) ;
#120938 = AXIS2_PLACEMENT_3D ( 'NONE', #82682, #15933, #125472 ) ;
#120939 = CARTESIAN_POINT ( 'NONE',  ( 86.39126352523146579, -4.472830434245839371, -4.472830434245839371 ) ) ;
#120940 = ORIENTED_EDGE ( 'NONE', *, *, #65388, .F. ) ;
#120941 = VECTOR ( 'NONE', #36683, 1000.000000000000000 ) ;
#120942 = LINE ( 'NONE', #32527, #104486 ) ;
#120943 = EDGE_CURVE ( 'NONE', #93492, #124824, #9264, .T. ) ;
#120944 = CARTESIAN_POINT ( 'NONE',  ( -30.70710678118632231, -9.740707523384179112, 5.000000000000000000 ) ) ;
#120945 = VECTOR ( 'NONE', #33429, 1000.000000000000227 ) ;
#120946 = ORIENTED_EDGE ( 'NONE', *, *, #66807, .F. ) ;
#120947 = ORIENTED_EDGE ( 'NONE', *, *, #51236, .T. ) ;
#120948 = ORIENTED_EDGE ( 'NONE', *, *, #19469, .F. ) ;
#120949 = DIRECTION ( 'NONE',  ( -0.000000000000000000, 0.000000000000000000, 1.000000000000000000 ) ) ;
#120950 = CARTESIAN_POINT ( 'NONE',  ( 42.48921356237308800, -27.52281430457085065, 5.000000000000000000 ) ) ;
#120951 = PLANE ( 'NONE',  #7144 ) ;
#120952 = CARTESIAN_POINT ( 'NONE',  ( 14.99999999999989875, -18.41253812416056590, 4.000000000000000000 ) ) ;
#120953 = EDGE_CURVE ( 'NONE', #49295, #114174, #97750, .T. ) ;
#120954 = CARTESIAN_POINT ( 'NONE',  ( -48.18398860626899705, 28.73617430169820608, 5.000000000000000000 ) ) ;
#120955 = ORIENTED_EDGE ( 'NONE', *, *, #8426, .T. ) ;
#120956 = ORIENTED_EDGE ( 'NONE', *, *, #92101, .T. ) ;
#120957 = B_SPLINE_CURVE_WITH_KNOTS ( 'NONE', 3,
 ( #79368, #46001, #24231, #67019 ),
 .UNSPECIFIED., .F., .F.,
 ( 4, 4 ),
 ( 0.003615568590623256459, 0.004164643302645746996 ),
 .UNSPECIFIED. ) ;
#120958 = DIRECTION ( 'NONE',  ( 0.3543493200069162685, -0.000000000000000000, -0.9351131265310288487 ) ) ;
#120960 = ORIENTED_EDGE ( 'NONE', *, *, #77486, .F. ) ;
#120959 = EDGE_CURVE ( 'NONE', #33799, #99786, #47623, .T. ) ;
#120961 = VERTEX_POINT ( 'NONE', #96282 ) ;
#120962 = AXIS2_PLACEMENT_3D ( 'NONE', #111311, #134529, #2536 ) ;
#120963 = VECTOR ( 'NONE', #142660, 1000.000000000000000 ) ;
#120964 = DIRECTION ( 'NONE',  ( 1.000000000000000000, -0.000000000000000000, -0.000000000000000000 ) ) ;
#120965 = ORIENTED_EDGE ( 'NONE', *, *, #105638, .F. ) ;
#120966 = CARTESIAN_POINT ( 'NONE',  ( -10.49999999999992895, -7.420205493532911589, -2.617629953481277028 ) ) ;
#120967 = SURFACE_STYLE_USAGE ( .BOTH. , #52840 ) ;
#120968 = EDGE_CURVE ( 'NONE', #59821, #66777, #54285, .T. ) ;
#120969 = FACE_OUTER_BOUND ( 'NONE', #59364, .T. ) ;
#120970 = PLANE ( 'NONE',  #92348 ) ;
#120971 = AXIS2_PLACEMENT_3D ( 'NONE', #17193, #73036, #4829 ) ;
#120972 = CARTESIAN_POINT ( 'NONE',  ( 16.49999999999988631, -11.94781430457070392, 5.000000000000000000 ) ) ;
#120973 = ORIENTED_EDGE ( 'NONE', *, *, #94213, .F. ) ;
#120974 = CARTESIAN_POINT ( 'NONE',  ( 25.39999999999999858, -14.29000000000013593, 12.69999999999954632 ) ) ;
#120975 = EDGE_LOOP ( 'NONE', ( #74322, #132373, #72499, #130815, #55885 ) ) ;
#120977 = ADVANCED_FACE ( 'NONE', ( #30349 ), #74592, .T. ) ;
#120976 = DIRECTION ( 'NONE',  ( 0.6830127018922180770, -0.6830127018922204085, -0.2588190451025213501 ) ) ;
#120978 = ORIENTED_EDGE ( 'NONE', *, *, #18097, .F. ) ;
#120979 = DIRECTION ( 'NONE',  ( -0.7071067811865487940, 0.7071067811865463515, 0.000000000000000000 ) ) ;
#120980 = ORIENTED_EDGE ( 'NONE', *, *, #56784, .T. ) ;
#120981 = EDGE_CURVE ( 'NONE', #135031, #24532, #23007, .T. ) ;
#120982 = CARTESIAN_POINT ( 'NONE',  ( -6.938893903907228378E-15, -16.02097659208071789, -11.96015758381208727 ) ) ;
#120983 = ORIENTED_EDGE ( 'NONE', *, *, #127962, .F. ) ;
#120984 = VERTEX_POINT ( 'NONE', #101318 ) ;
#120985 = VECTOR ( 'NONE', #14656, 1000.000000000000000 ) ;
#120986 = ORIENTED_EDGE ( 'NONE', *, *, #120766, .T. ) ;
#120987 = DIRECTION ( 'NONE',  ( -0.6830127018922180770, -0.6830127018922204085, -0.2588190451025213501 ) ) ;
#120988 = CARTESIAN_POINT ( 'NONE',  ( 30.79333936457826937, 21.75929247661550647, 4.998822639870708073 ) ) ;
#120989 = LINE ( 'NONE', #20236, #137534 ) ;
#120990 = CARTESIAN_POINT ( 'NONE',  ( 126.7295968585647756, -6.110000000000000320, -1.637169565754161393 ) ) ;
#120991 = CARTESIAN_POINT ( 'NONE',  ( -22.49999999999984723, -9.462702396501025959, -9.474982329943465231 ) ) ;
#120992 = CARTESIAN_POINT ( 'NONE',  ( -17.29289321881333663, -18.74070752338409562, 5.000000000000000000 ) ) ;
#120993 = CARTESIAN_POINT ( 'NONE',  ( -21.00548008471250938, 28.92564299267923644, 4.000000000000000000 ) ) ;
#120994 = VECTOR ( 'NONE', #74163, 1000.000000000000000 ) ;
#120995 = AXIS2_PLACEMENT_3D ( 'NONE', #64094, #87277, #108263 ) ;
#120996 = CARTESIAN_POINT ( 'NONE',  ( 20.99999999999985079, -18.03360074219755660, 5.000000000000000000 ) ) ;
#120997 = EDGE_CURVE ( 'NONE', #14168, #125750, #14305, .T. ) ;
#120998 = AXIS2_PLACEMENT_3D ( 'NONE', #45128, #76301, #89999 ) ;
#120999 = VECTOR ( 'NONE', #6125, 1000.000000000000000 ) ;
#121000 = EDGE_CURVE ( 'NONE', #23978, #119191, #123812, .T. ) ;
#121001 = DIRECTION ( 'NONE',  ( 0.6830127018922181881, 0.6830127018922202975, -0.2588190451025214056 ) ) ;
#121002 = CARTESIAN_POINT ( 'NONE',  ( 8.510786437626906675, -27.52281430457049183, 5.000000000000000000 ) ) ;
#121003 = VERTEX_POINT ( 'NONE', #1953 ) ;
#121004 = ORIENTED_EDGE ( 'NONE', *, *, #139482, .T. ) ;
#121005 = EDGE_LOOP ( 'NONE', ( #13418, #30788, #25371, #111133, #74683, #3593 ) ) ;
#121006 = VECTOR ( 'NONE', #36755, 1000.000000000000000 ) ;
#121007 =( GEOMETRIC_REPRESENTATION_CONTEXT ( 3 ) GLOBAL_UNCERTAINTY_ASSIGNED_CONTEXT ( ( #33020 ) ) GLOBAL_UNIT_ASSIGNED_CONTEXT ( ( #52138, #40566, #118816 ) ) REPRESENTATION_CONTEXT ( 'NONE', 'WORKASPACE' ) );
#121008 = FACE_OUTER_BOUND ( 'NONE', #142257, .T. ) ;
#121009 = ORIENTED_EDGE ( 'NONE', *, *, #106256, .F. ) ;
#121010 = ORIENTED_EDGE ( 'NONE', *, *, #839, .T. ) ;
#121011 = DIRECTION ( 'NONE',  ( -0.000000000000000000, 0.000000000000000000, 1.000000000000000000 ) ) ;
#121012 = CARTESIAN_POINT ( 'NONE',  ( 107.2666937171295558, -7.949999999999998401, 2.130196079827423983 ) ) ;
#121013 = CARTESIAN_POINT ( 'NONE',  ( -2.999999999999981792, 12.25461709320620507, -10.07315571508697971 ) ) ;
#121014 = EDGE_CURVE ( 'NONE', #20835, #133915, #17796, .T. ) ;
#121015 = DIRECTION ( 'NONE',  ( 1.000000000000000000, 0.000000000000000000, 0.000000000000000000 ) ) ;
#121016 = EDGE_CURVE ( 'NONE', #81493, #83949, #69428, .T. ) ;
#121017 = LINE ( 'NONE', #110824, #53343 ) ;
#121018 = EDGE_LOOP ( 'NONE', ( #32004, #26109, #109965, #95265 ) ) ;
#121019 = CARTESIAN_POINT ( 'NONE',  ( 12.48921356237309155, -27.52281430457064104, 5.000000000000000000 ) ) ;
#121020 = ORIENTED_EDGE ( 'NONE', *, *, #118077, .F. ) ;
#121021 = DIRECTION ( 'NONE',  ( 1.000000000000000000, 3.115803279706882722E-16, -0.000000000000000000 ) ) ;
#121022 = VECTOR ( 'NONE', #123597, 1000.000000000000000 ) ;
#121023 = CARTESIAN_POINT ( 'NONE',  ( 19.75456980810189123, -6.871911579029512218, 3.967499999999996252 ) ) ;
#121024 = VERTEX_POINT ( 'NONE', #78881 ) ;
#121025 = CARTESIAN_POINT ( 'NONE',  ( 84.20376352523145158, 6.109999999999999432, 1.122388791418549108E-15 ) ) ;
#121026 = CARTESIAN_POINT ( 'NONE',  ( 7.649330195115605413, -8.844083433006840522, -3.472940883649443311 ) ) ;
#121027 = DIRECTION ( 'NONE',  ( 0.6830127018922181881, 0.6830127018922202975, -0.2588190451025214056 ) ) ;
#121028 = CARTESIAN_POINT ( 'NONE',  ( -27.41161490594811667, 22.22500000000000142, 4.777194822843815913 ) ) ;
#121029 = VERTEX_POINT ( 'NONE', #89726 ) ;
#121030 = ORIENTED_EDGE ( 'NONE', *, *, #108121, .T. ) ;
#121031 = VERTEX_POINT ( 'NONE', #121624 ) ;
#121032 = FACE_OUTER_BOUND ( 'NONE', #113710, .T. ) ;
#121033 = CARTESIAN_POINT ( 'NONE',  ( 33.71757738642545377, -21.73023691814492508, 5.000000000000000000 ) ) ;
#121034 = CARTESIAN_POINT ( 'NONE',  ( 13.13598696172163116, 4.584330080086930965E-16, 0.000000000000000000 ) ) ;
#121035 = LINE ( 'NONE', #21738, #84458 ) ;
#121036 = DIRECTION ( 'NONE',  ( 0.7071067811865486830, -0.7071067811865464625, -0.000000000000000000 ) ) ;
#121037 = EDGE_CURVE ( 'NONE', #126389, #56485, #57848, .T. ) ;
#121038 = ORIENTED_EDGE ( 'NONE', *, *, #44533, .T. ) ;
#121039 = AXIS2_PLACEMENT_3D ( 'NONE', #136163, #92639, #136878 ) ;
#121040 = DIRECTION ( 'NONE',  ( -0.7071067811865486830, -0.7071067811865464625, 0.000000000000000000 ) ) ;
#121041 = VECTOR ( 'NONE', #116232, 1000.000000000000000 ) ;
#121042 = CARTESIAN_POINT ( 'NONE',  ( 0.000000000000000000, 0.000000000000000000, 5.000000000000000000 ) ) ;
#121043 = ORIENTED_EDGE ( 'NONE', *, *, #22525, .F. ) ;
#121044 = FILL_AREA_STYLE ('',( #76872 ) ) ;
#121045 = CIRCLE ( 'NONE', #77111, 2.500000000000000888 ) ;
#121046 = CARTESIAN_POINT ( 'NONE',  ( 33.18398860626899705, 28.73617430169810305, 5.000000000000000000 ) ) ;
#121047 = ORIENTED_EDGE ( 'NONE', *, *, #30090, .F. ) ;
#121049 = VERTEX_POINT ( 'NONE', #132563 ) ;
#121048 = LINE ( 'NONE', #87717, #92652 ) ;
#121050 = VERTEX_POINT ( 'NONE', #22292 ) ;
#121051 = DIRECTION ( 'NONE',  ( -0.000000000000000000, -0.3543493200069152693, 0.9351131265310292928 ) ) ;
#121052 = CARTESIAN_POINT ( 'NONE',  ( -4.998069433178984333, -22.22500000000000142, 4.500000000000000888 ) ) ;
#121053 = EDGE_LOOP ( 'NONE', ( #16619, #97067, #120426, #21716 ) ) ;
#121054 = DIRECTION ( 'NONE',  ( -0.7071067811865486830, 0.7071067811865464625, 0.000000000000000000 ) ) ;
#121055 = VECTOR ( 'NONE', #122471, 1000.000000000000000 ) ;
#121056 = CARTESIAN_POINT ( 'NONE',  ( -24.29974487139158867, -27.71228299555223273, 4.000000000000000000 ) ) ;
#121057 = ADVANCED_FACE ( 'NONE', ( #134692 ), #56444, .T. ) ;
#121058 = FACE_OUTER_BOUND ( 'NONE', #96367, .T. ) ;
#121059 = CARTESIAN_POINT ( 'NONE',  ( 0.000000000000000000, 0.000000000000000000, 5.000000000000000000 ) ) ;
#121060 = EDGE_CURVE ( 'NONE', #87749, #115239, #33256, .T. ) ;
#121061 = DIRECTION ( 'NONE',  ( 0.6830127018922180770, -0.6830127018922204085, -0.2588190451025213501 ) ) ;
#121062 = DIRECTION ( 'NONE',  ( 0.6830127018922181881, 0.6830127018922202975, -0.2588190451025214056 ) ) ;
#121063 = DIRECTION ( 'NONE',  ( -0.000000000000000000, -0.3543493200069152693, 0.9351131265310292928 ) ) ;
#121064 = CARTESIAN_POINT ( 'NONE',  ( -4.499999999999968914, 4.466399257802219580, 5.000000000000000000 ) ) ;
#121065 = LINE ( 'NONE', #40673, #61885 ) ;
#121066 = DIRECTION ( 'NONE',  ( -0.7071067811865486830, 0.7071067811865464625, 0.000000000000000000 ) ) ;
#121067 = AXIS2_PLACEMENT_3D ( 'NONE', #56614, #31426, #68889 ) ;
#121068 = CARTESIAN_POINT ( 'NONE',  ( -3.183988606268992161, 28.73617430169789699, 5.000000000000000000 ) ) ;
#121069 = CARTESIAN_POINT ( 'NONE',  ( -34.49999999999976552, 7.464255608400418573, 4.994342998332163219 ) ) ;
#121071 = EDGE_CURVE ( 'NONE', #81589, #74837, #110731, .T. ) ;
#121070 = DIRECTION ( 'NONE',  ( 0.3543493200069162685, -0.000000000000000000, -0.9351131265310288487 ) ) ;
#121073 = EDGE_CURVE ( 'NONE', #25809, #136698, #59317, .T. ) ;
#121072 = EDGE_LOOP ( 'NONE', ( #59248, #10749, #23883, #92036 ) ) ;
#121074 = ORIENTED_EDGE ( 'NONE', *, *, #29909, .T. ) ;
#121075 = CARTESIAN_POINT ( 'NONE',  ( 103.8125000000000142, 5.819803920172571310, 5.819803920172575751 ) ) ;
#121076 = EDGE_LOOP ( 'NONE', ( #134997, #7149, #9785, #133362 ) ) ;
#121077 = ORIENTED_EDGE ( 'NONE', *, *, #823, .F. ) ;
#121078 = EDGE_LOOP ( 'NONE', ( #74212, #126874, #33956, #5838 ) ) ;
#121079 = DIRECTION ( 'NONE',  ( -1.000000000000000000, 0.000000000000000000, -0.000000000000000000 ) ) ;
#121080 = FACE_OUTER_BOUND ( 'NONE', #74033, .T. ) ;
#121081 = VECTOR ( 'NONE', #26638, 1000.000000000000000 ) ;
#121082 = EDGE_LOOP ( 'NONE', ( #139591, #133176, #32302, #141706 ) ) ;
#121083 = CARTESIAN_POINT ( 'NONE',  ( 20.81601139373100295, 28.73617430169773002, 5.000000000000000000 ) ) ;
#121084 = CARTESIAN_POINT ( 'NONE',  ( 37.98012225071429526, -17.24070752338409918, 20.23474786156478089 ) ) ;
#121085 = EDGE_CURVE ( 'NONE', #98086, #133451, #133259, .T. ) ;
#121086 = FACE_OUTER_BOUND ( 'NONE', #8922, .T. ) ;
#121087 = CARTESIAN_POINT ( 'NONE',  ( 27.48921356237309155, -27.52281430457074762, 5.000000000000000000 ) ) ;
#121088 = ORIENTED_EDGE ( 'NONE', *, *, #137200, .T. ) ;
#121089 = EDGE_CURVE ( 'NONE', #14142, #96671, #112907, .T. ) ;
#121090 = CARTESIAN_POINT ( 'NONE',  ( 8.999999999999937828, -19.06887692260761469, 4.000000000000000000 ) ) ;
#121092 = AXIS2_PLACEMENT_3D ( 'NONE', #90448, #56445, #23008 ) ;
#121091 = FACE_OUTER_BOUND ( 'NONE', #41888, .T. ) ;
#121093 = DIRECTION ( 'NONE',  ( 0.3543493200069162685, -0.000000000000000000, -0.9351131265310288487 ) ) ;
#121094 = CARTESIAN_POINT ( 'NONE',  ( 0.000000000000000000, 0.000000000000000000, 5.000000000000000000 ) ) ;
#121095 = FACE_OUTER_BOUND ( 'NONE', #91739, .T. ) ;
#121096 = CARTESIAN_POINT ( 'NONE',  ( 30.41252705046289151, -7.949999999999998401, -4.867971026610728450E-16 ) ) ;
#121097 = EDGE_CURVE ( 'NONE', #57727, #89471, #78156, .T. ) ;
#121098 = CARTESIAN_POINT ( 'NONE',  ( 29.53839644629411509, -9.740707523384184441, 17.74957260769617662 ) ) ;
#121099 = ORIENTED_EDGE ( 'NONE', *, *, #75155, .F. ) ;
#121100 = ORIENTED_EDGE ( 'NONE', *, *, #109152, .F. ) ;
#121101 = CARTESIAN_POINT ( 'NONE',  ( 117.9795968585647898, 6.109999999999999432, 1.637169565754164280 ) ) ;
#121102 = ORIENTED_EDGE ( 'NONE', *, *, #27453, .T. ) ;
#121103 = DIRECTION ( 'NONE',  ( -1.000000000000000000, 0.000000000000000000, 0.000000000000000000 ) ) ;
#121104 = DIRECTION ( 'NONE',  ( -0.7071067811865486830, -0.7071067811865464625, -0.000000000000000000 ) ) ;
#121105 = EDGE_CURVE ( 'NONE', #91841, #8931, #133950, .T. ) ;
#121106 = AXIS2_PLACEMENT_3D ( 'NONE', #94994, #5115, #49415 ) ;
#121107 = PLANE ( 'NONE',  #34144 ) ;
#121108 = CARTESIAN_POINT ( 'NONE',  ( 23.00840764549667483, 3.061616997868380183E-16, -2.500000000000001332 ) ) ;
#121110 = CIRCLE ( 'NONE', #98153, 2.500000000000000888 ) ;
#121109 = CARTESIAN_POINT ( 'NONE',  ( 14.26396771883894132, 22.22500000000000142, 23.63953864884001987 ) ) ;
#121111 = CARTESIAN_POINT ( 'NONE',  ( 112.3495968585647802, 6.109999999999996767, 1.637169565754163836 ) ) ;
#121112 = VERTEX_POINT ( 'NONE', #138235 ) ;
#121113 = VERTEX_POINT ( 'NONE', #61434 ) ;
#121114 = EDGE_CURVE ( 'NONE', #90422, #52778, #67838, .T. ) ;
#121115 = VECTOR ( 'NONE', #79281, 999.9999999999998863 ) ;
#121116 = AXIS2_PLACEMENT_3D ( 'NONE', #109199, #9881, #121494 ) ;
#121117 = CARTESIAN_POINT ( 'NONE',  ( 28.17183060077627133, 6.759292476615649470, 4.000000000000000000 ) ) ;
#121118 = DIRECTION ( 'NONE',  ( 0.3543493200069162685, -0.000000000000000000, -0.9351131265310288487 ) ) ;
#121119 = VERTEX_POINT ( 'NONE', #70858 ) ;
#121120 = VERTEX_POINT ( 'NONE', #83887 ) ;
#121121 = CARTESIAN_POINT ( 'NONE',  ( 38.79209685856477563, -5.291415217122921177, 3.054999999999999272 ) ) ;
#121122 = ORIENTED_EDGE ( 'NONE', *, *, #56926, .T. ) ;
#121123 = LINE ( 'NONE', #99350, #46877 ) ;
#121124 = DIRECTION ( 'NONE',  ( 0.7071067811865487940, -0.7071067811865463515, 0.000000000000000000 ) ) ;
#121125 = EDGE_CURVE ( 'NONE', #139988, #69350, #105575, .T. ) ;
#121126 = CARTESIAN_POINT ( 'NONE',  ( 36.95376352523144448, -6.109999999999998543, -3.741295971395162543E-16 ) ) ;
#121127 = ORIENTED_EDGE ( 'NONE', *, *, #64815, .F. ) ;
#121128 = CARTESIAN_POINT ( 'NONE',  ( 39.18398860626899705, 28.73617430169814568, 5.000000000000000000 ) ) ;
#121129 = ORIENTED_EDGE ( 'NONE', *, *, #113697, .F. ) ;
#121130 = VERTEX_POINT ( 'NONE', #115009 ) ;
#121131 = ORIENTED_EDGE ( 'NONE', *, *, #133494, .F. ) ;
#121132 = AXIS2_PLACEMENT_3D ( 'NONE', #1173, #46911, #68627 ) ;
#121133 = CARTESIAN_POINT ( 'NONE',  ( 18.48921356237309510, -27.52281430457068367, 5.000000000000000000 ) ) ;
#121134 = CARTESIAN_POINT ( 'NONE',  ( 33.75860074219772855, 21.72500000000000142, 5.000000000000000000 ) ) ;
#121135 = EDGE_LOOP ( 'NONE', ( #76424, #19832, #116846, #91275 ) ) ;
#121136 = AXIS2_PLACEMENT_3D ( 'NONE', #35609, #13074, #126835 ) ;
#121137 = CARTESIAN_POINT ( 'NONE',  ( 10.49999999999993250, 19.46639925780205616, 5.000000000000000000 ) ) ;
#121138 = EDGE_CURVE ( 'NONE', #86186, #94959, #38922, .T. ) ;
#121139 = LINE ( 'NONE', #10234, #133544 ) ;
#121140 =( BOUNDED_CURVE ( )  B_SPLINE_CURVE ( 2, ( #69586, #92009, #23919, #136226, #1408, #13710, #36911, #24613, #81162, #34089, #70318, #68867, #58004, #135541, #78299, #34798, #125367, #23161, #45693, #89863, #79040, #84711, #60125, #93449, #137684, #71709, #72453, #50651, #18709, #118006, #84033, #105025, #71005, #136949, #29596, #16574, #94140, #62258, #73834, #115155, #73146, #60865, #4955, #105715, #62987, #107162, #106413, #139106, #38358, #15829, #7841, #128229, #81899, #17982, #61566, #92715, #127499, #28906, #115876, #126089, #82573, #39064, #128921, #17304, #117310, #37660, #49259, #126766, #6375, #7104, #28193, #51379, #104293, #26756, #27448, #138378, #5692, #49959, #83287, #95576, #116621, #139838, #40509, #94841, #39808, #20145, #65861, #31761, #52084, #8523, #64385, #98441, #96260, #65127, #88293, #121603, #97721, #85400, #119448, #108556, #66538, #10683, #142664, #54956, #129625, #141973, #76721, #96966, #120892, #110016, #20862, #141215, #132539, #131792, #130372, #19448, #140505, #21600, #22271, #110706, #99120, #75978, #143365, #9236, #44071, #41193, #33230, #53517, #42663, #77439, #52772, #30328, #120149, #74563, #109312, #118754, #63697, #86864, #131073, #9997, #107858, #41934, #54261, #43356, #87567, #32481, #86143, #31064, #75283, #34616, #80287, #44828, #45524, #78852, #102012, #133928, #57822, #1931, #13543, #124476, #55665, #23735, #25877, #14283, #122305, #2677, #123061, #46975, #12129, #68007, #47676, #24444, #25148, #99867, #69400 ),
 .UNSPECIFIED., .F., .F. ) 
 B_SPLINE_CURVE_WITH_KNOTS ( ( 3, 2, 2, 2, 2, 2, 2, 2, 2, 2, 2, 2, 2, 2, 2, 2, 2, 2, 2, 2, 2, 2, 2, 2, 2, 2, 2, 2, 2, 2, 2, 2, 2, 2, 2, 2, 2, 2, 2, 2, 2, 2, 2, 2, 2, 2, 2, 2, 2, 2, 2, 2, 2, 2, 2, 2, 2, 2, 2, 2, 2, 2, 2, 2, 2, 2, 2, 2, 2, 2, 2, 2, 2, 2, 2, 2, 2, 2, 2, 2, 2, 2, 2, 2, 2, 2, 2, 3 ),
 ( 0.01770235391886232357, 0.02500000000000000139, 0.03333333333333333287, 0.04166666666666666435, 0.05000000000000000278, 0.05833333333333333426, 0.06666666666666665186, 0.07499999999999998335, 0.08333333333333332871, 0.09166666666666666019, 0.1000000000000000056, 0.1083333333333333370, 0.1166666666666666685, 0.1250000000000000000, 0.1333333333333333315, 0.1416666666666666630, 0.1499999999999999944, 0.1583333333333333259, 0.1666666666666666574, 0.1749999999999999889, 0.1833333333333333204, 0.1916666666666666796, 0.1999999999999999833, 0.2083333333333333426, 0.2166666666666666463, 0.2250000000000000056, 0.2333333333333333093, 0.2416666666666666685, 0.2499999999999999722, 0.2583333333333334147, 0.2666666666666666630, 0.2750000000000000222, 0.2833333333333333259, 0.2916666666666666852, 0.2999999999999999889, 0.3083333333333333481, 0.3166666666666666519, 0.3250000000000000111, 0.3333333333333333148, 0.3416666666666666741, 0.3499999999999999778, 0.3583333333333333370, 0.3666666666666666408, 0.3750000000000000000, 0.3833333333333333592, 0.3916666666666666630, 0.4000000000000000222, 0.4083333333333333259, 0.4166666666666666852, 0.4249999999999999889, 0.4333333333333333481, 0.4416666666666666519, 0.4500000000000000111, 0.4583333333333333703, 0.4666666666666666741, 0.4749999999999999778, 0.4833333333333333370, 0.4916666666666666963, 0.5000000000000000000, 0.5083333333333333037, 0.5166666666666667185, 0.5250000000000000222, 0.5333333333333333259, 0.5416666666666666297, 0.5500000000000000444, 0.5583333333333333481, 0.5666666666666666519, 0.5749999999999999556, 0.5833333333333333703, 0.5916666666666666741, 0.5999999999999999778, 0.6083333333333332815, 0.6166666666666666963, 0.6250000000000000000, 0.6333333333333333037, 0.6416666666666667185, 0.6500000000000000222, 0.6583333333333333259, 0.6666666666666666297, 0.6750000000000000444, 0.6833333333333333481, 0.6916666666666666519, 0.6999999999999999556, 0.7083333333333333703, 0.7166666666666666741, 0.7249999999999999778, 0.7333333333333332815, 0.7388014923403734002 ),
 .UNSPECIFIED. ) 
 CURVE ( )  GEOMETRIC_REPRESENTATION_ITEM ( )  RATIONAL_B_SPLINE_CURVE ( ( 0.9925829834361643567, 0.9701606487700498160, 1.000000000000000000, 0.9659258262890683122, 1.000000000000000000, 0.9659258262890683122, 1.000000000000000000, 0.9659258262890683122, 1.000000000000000000, 0.9659258262890683122, 1.000000000000000000, 0.9659258262890683122, 1.000000000000000000, 0.9659258262890683122, 1.000000000000000000, 0.9659258262890683122, 1.000000000000000000, 0.9659258262890683122, 1.000000000000000000, 0.9659258262890683122, 1.000000000000000000, 0.9659258262890683122, 1.000000000000000000, 0.9659258262890683122, 1.000000000000000000, 0.9659258262890683122, 1.000000000000000000, 0.9659258262890683122, 1.000000000000000000, 0.9659258262890683122, 1.000000000000000000, 0.9659258262890683122, 1.000000000000000000, 0.9659258262890683122, 1.000000000000000000, 0.9659258262890683122, 1.000000000000000000, 0.9659258262890683122, 1.000000000000000000, 0.9659258262890683122, 1.000000000000000000, 0.9659258262890683122, 1.000000000000000000, 0.9659258262890683122, 1.000000000000000000, 0.9659258262890683122, 1.000000000000000000, 0.9659258262890683122, 1.000000000000000000, 0.9659258262890683122, 1.000000000000000000, 0.9659258262890683122, 1.000000000000000000, 0.9659258262890683122, 1.000000000000000000, 0.9659258262890683122, 1.000000000000000000, 0.9659258262890683122, 1.000000000000000000, 0.9659258262890683122, 1.000000000000000000, 0.9659258262890683122, 1.000000000000000000, 0.9659258262890683122, 1.000000000000000000, 0.9659258262890683122, 1.000000000000000000, 0.9659258262890683122, 1.000000000000000000, 0.9659258262890683122, 1.000000000000000000, 0.9659258262890683122, 1.000000000000000000, 0.9659258262890683122, 1.000000000000000000, 0.9659258262890683122, 1.000000000000000000, 0.9659258262890683122, 1.000000000000000000, 0.9659258262890683122, 1.000000000000000000, 0.9659258262890683122, 1.000000000000000000, 0.9659258262890683122, 1.000000000000000000, 0.9659258262890683122, 1.000000000000000000, 0.9659258262890683122, 1.000000000000000000, 0.9659258262890683122, 1.000000000000000000, 0.9659258262890683122, 1.000000000000000000, 0.9659258262890683122, 1.000000000000000000, 0.9659258262890683122, 1.000000000000000000, 0.9659258262890683122, 1.000000000000000000, 0.9659258262890683122, 1.000000000000000000, 0.9659258262890683122, 1.000000000000000000, 0.9659258262890683122, 1.000000000000000000, 0.9659258262890683122, 1.000000000000000000, 0.9659258262890683122, 1.000000000000000000, 0.9659258262890683122, 1.000000000000000000, 0.9659258262890683122, 1.000000000000000000, 0.9659258262890683122, 1.000000000000000000, 0.9659258262890683122, 1.000000000000000000, 0.9659258262890683122, 1.000000000000000000, 0.9659258262890683122, 1.000000000000000000, 0.9659258262890683122, 1.000000000000000000, 0.9659258262890683122, 1.000000000000000000, 0.9659258262890683122, 1.000000000000000000, 0.9659258262890683122, 1.000000000000000000, 0.9659258262890683122, 1.000000000000000000, 0.9659258262890683122, 1.000000000000000000, 0.9659258262890683122, 1.000000000000000000, 0.9659258262890683122, 1.000000000000000000, 0.9659258262890683122, 1.000000000000000000, 0.9659258262890683122, 1.000000000000000000, 0.9659258262890683122, 1.000000000000000000, 0.9659258262890683122, 1.000000000000000000, 0.9659258262890683122, 1.000000000000000000, 0.9659258262890683122, 1.000000000000000000, 0.9659258262890683122, 1.000000000000000000, 0.9659258262890683122, 1.000000000000000000, 0.9659258262890683122, 1.000000000000000000, 0.9659258262890683122, 1.000000000000000000, 0.9659258262890683122, 1.000000000000000000, 0.9659258262890683122, 1.000000000000000000, 0.9659258262890683122, 1.000000000000000000, 0.9659258262890683122, 1.000000000000000000, 0.9659258262890683122, 1.000000000000000000, 0.9659258262890683122, 1.000000000000000000, 0.9659258262890683122, 1.000000000000000000, 0.9659258262890683122, 1.000000000000000000, 0.9776412400138145831, 0.9846251811807589238 ) ) 
 REPRESENTATION_ITEM ( '' )  );
#121141 = CARTESIAN_POINT ( 'NONE',  ( -18.18398860626898994, 28.73617430169800002, 5.000000000000000000 ) ) ;
#121142 = VECTOR ( 'NONE', #102687, 1000.000000000000000 ) ;
#121143 = FACE_BOUND ( 'NONE', #118846, .T. ) ;
#121144 = ORIENTED_EDGE ( 'NONE', *, *, #106500, .T. ) ;
#121145 = FACE_OUTER_BOUND ( 'NONE', #143474, .T. ) ;
#121146 = EDGE_CURVE ( 'NONE', #88713, #52625, #106276, .T. ) ;
#121147 = DIRECTION ( 'NONE',  ( 0.6830127018922181881, 0.6830127018922202975, -0.2588190451025214056 ) ) ;
#121148 = CARTESIAN_POINT ( 'NONE',  ( 32.29289321881323360, -15.74070752338412049, 5.000000000000000000 ) ) ;
#121149 = EDGE_LOOP ( 'NONE', ( #1264, #67014, #96908, #127469 ) ) ;
#121150 = LINE ( 'NONE', #134195, #59707 ) ;
#121151 = ORIENTED_EDGE ( 'NONE', *, *, #135848, .T. ) ;
#121152 = ORIENTED_EDGE ( 'NONE', *, *, #103393, .T. ) ;
#121153 = CARTESIAN_POINT ( 'NONE',  ( 2.999999999999999112, 1.399999999999986366, 20.40202195861970580 ) ) ;
#121154 = ORIENTED_EDGE ( 'NONE', *, *, #125963, .F. ) ;
#121155 = AXIS2_PLACEMENT_3D ( 'NONE', #59846, #115585, #27914 ) ;
#121156 = CARTESIAN_POINT ( 'NONE',  ( 47.59959685856477307, -6.109999999999997655, -1.637169565754160283 ) ) ;
#121158 = ORIENTED_EDGE ( 'NONE', *, *, #87721, .F. ) ;
#121157 = VECTOR ( 'NONE', #36694, 1000.000000000000000 ) ;
#121159 = DIRECTION ( 'NONE',  ( 1.000000000000000000, 0.000000000000000000, 0.000000000000000000 ) ) ;
#121160 = PLANE ( 'NONE',  #65894 ) ;
#121161 = DIRECTION ( 'NONE',  ( 0.7071067811865486830, -0.7071067811865464625, -0.000000000000000000 ) ) ;
#121162 = VERTEX_POINT ( 'NONE', #4083 ) ;
#121163 = CARTESIAN_POINT ( 'NONE',  ( 14.99999999999990230, -10.44781430457071814, 5.000000000000000000 ) ) ;
#121164 = DIRECTION ( 'NONE',  ( 1.000000000000000000, -0.000000000000000000, 0.000000000000000000 ) ) ;
#121165 = AXIS2_PLACEMENT_3D ( 'NONE', #20882, #43375, #63010 ) ;
#121166 =( NAMED_UNIT ( * ) PLANE_ANGLE_UNIT ( ) SI_UNIT ( $, .RADIAN. ) );
#121167 = LINE ( 'NONE', #21863, #113398 ) ;
#121168 = EDGE_CURVE ( 'NONE', #92202, #138457, #97398, .T. ) ;
#121169 = LINE ( 'NONE', #108129, #27476 ) ;
#121170 = DIRECTION ( 'NONE',  ( -0.7071067811865487940, 0.7071067811865463515, -0.000000000000000000 ) ) ;
#121171 = CARTESIAN_POINT ( 'NONE',  ( -10.01987774928541519, -17.24070752338410273, 20.23474786156467076 ) ) ;
#121172 = ORIENTED_EDGE ( 'NONE', *, *, #80644, .T. ) ;
#121174 = ORIENTED_EDGE ( 'NONE', *, *, #75699, .T. ) ;
#121173 = AXIS2_PLACEMENT_3D ( 'NONE', #67126, #112064, #111320 ) ;
#121175 = VERTEX_POINT ( 'NONE', #16421 ) ;
#121176 = DIRECTION ( 'NONE',  ( -0.6830127018922180770, -0.6830127018922204085, -0.2588190451025213501 ) ) ;
#121177 = CARTESIAN_POINT ( 'NONE',  ( -23.99999999999983302, 9.631307414974306980, -9.079085613539598754 ) ) ;
#121178 = ORIENTED_EDGE ( 'NONE', *, *, #75340, .T. ) ;
#121179 = EDGE_LOOP ( 'NONE', ( #84956, #119243, #109935, #135831 ) ) ;
#121180 = PLANE ( 'NONE',  #139306 ) ;
#121181 = DIRECTION ( 'NONE',  ( -0.6830127018922180770, -0.6830127018922202975, -0.2588190451025213501 ) ) ;
#121182 = ADVANCED_FACE ( 'NONE', ( #6236 ), #103246, .T. ) ;
#121183 = EDGE_CURVE ( 'NONE', #63923, #37409, #112255, .T. ) ;
#121184 = DIRECTION ( 'NONE',  ( 0.6830127018922180770, -0.6830127018922204085, -0.2588190451025213501 ) ) ;
#121185 = CONICAL_SURFACE ( 'NONE', #58761, 2.500000000000000888, 0.9599310885968822538 ) ;
#121186 = ORIENTED_EDGE ( 'NONE', *, *, #65192, .F. ) ;
#121187 = CARTESIAN_POINT ( 'NONE',  ( 15.18398860626900237, 28.73617430169797871, 5.000000000000000000 ) ) ;
#121188 = DIRECTION ( 'NONE',  ( -0.000000000000000000, -0.3543493200069152693, 0.9351131265310292928 ) ) ;
#121189 = CARTESIAN_POINT ( 'NONE',  ( 16.40040314143521982, -7.934999999999989839, 2.126176841940957907 ) ) ;
#121190 = AXIS2_PLACEMENT_3D ( 'NONE', #38991, #40443, #49892 ) ;
#121191 = DIRECTION ( 'NONE',  ( 0.3543493200069162685, -0.000000000000000000, -0.9351131265310288487 ) ) ;
#121192 = VERTEX_POINT ( 'NONE', #138963 ) ;
#121193 = CARTESIAN_POINT ( 'NONE',  ( 115.9954301918981230, 5.291415217122917625, 3.055000000000002380 ) ) ;
#121194 = EDGE_CURVE ( 'NONE', #138878, #49384, #73018, .T. ) ;
#121195 = DIRECTION ( 'NONE',  ( -0.6830127018922181881, 0.6830127018922202975, -0.2588190451025214056 ) ) ;
#121196 = CARTESIAN_POINT ( 'NONE',  ( -22.82816939922335919, 21.75929247661550647, 4.000000000000000000 ) ) ;
#121198 = VERTEX_POINT ( 'NONE', #15008 ) ;
#121197 = CARTESIAN_POINT ( 'NONE',  ( 9.524001385854420576, 22.03583458319438293, 4.979811245910088502 ) ) ;
#121199 = CARTESIAN_POINT ( 'NONE',  ( 11.99999999999992717, 11.96639925780213964, 5.000000000000000000 ) ) ;
#121200 = ORIENTED_EDGE ( 'NONE', *, *, #142397, .T. ) ;
#121201 = B_SPLINE_CURVE_WITH_KNOTS ( 'NONE', 3,
 ( #81544, #6049, #103250, #93813 ),
 .UNSPECIFIED., .F., .F.,
 ( 4, 4 ),
 ( 0.001201692628195026894, 0.001634763834691506899 ),
 .UNSPECIFIED. ) ;
#121202 = CARTESIAN_POINT ( 'NONE',  ( 26.99999999999981526, 15.45873954670187977, -0.03131636524300249191 ) ) ;
#121203 = CARTESIAN_POINT ( 'NONE',  ( 33.48921356237309510, -27.52281430457078670, 5.000000000000000000 ) ) ;
#121204 = DIRECTION ( 'NONE',  ( -0.3543493200069162685, -0.000000000000000000, -0.9351131265310288487 ) ) ;
#121205 = ADVANCED_FACE ( 'NONE', ( #15688 ), #26615, .F. ) ;
#121207 = VERTEX_POINT ( 'NONE', #125941 ) ;
#121206 = VECTOR ( 'NONE', #60022, 1000.000000000000227 ) ;
#121208 = DIRECTION ( 'NONE',  ( -0.000000000000000000, 1.000000000000000000, -0.000000000000000000 ) ) ;
#121209 = CARTESIAN_POINT ( 'NONE',  ( 23.48831394071553547, 6.759292476615649470, 16.35960578974464141 ) ) ;
#121210 = ORIENTED_EDGE ( 'NONE', *, *, #53594, .F. ) ;
#121211 = PRODUCT_DEFINITION_FORMATION_WITH_SPECIFIED_SOURCE ( 'ANY', '', #54028, .NOT_KNOWN. ) ;
#121212 = PLANE ( 'NONE',  #83280 ) ;
#121213 = LINE ( 'NONE', #87170, #14523 ) ;
#121214 = EDGE_LOOP ( 'NONE', ( #70734, #68708, #29717, #48028 ) ) ;
#121215 = FACE_OUTER_BOUND ( 'NONE', #108247, .T. ) ;
#121217 = EDGE_LOOP ( 'NONE', ( #39723, #115311, #138077, #76678 ) ) ;
#121216 = LINE ( 'NONE', #140306, #138845 ) ;
#121218 = ORIENTED_EDGE ( 'NONE', *, *, #48582, .T. ) ;
#121219 = DIRECTION ( 'NONE',  ( 0.000000000000000000, 0.000000000000000000, -1.000000000000000000 ) ) ;
#121220 = CARTESIAN_POINT ( 'NONE',  ( -11.20710678118646264, 6.759292476615651246, 5.000000000000000000 ) ) ;
#121221 = AXIS2_PLACEMENT_3D ( 'NONE', #139393, #75531, #128489 ) ;
#121222 = VERTEX_POINT ( 'NONE', #36765 ) ;
#121223 = EDGE_CURVE ( 'NONE', #61200, #134689, #81014, .T. ) ;
#121224 = AXIS2_PLACEMENT_3D ( 'NONE', #42659, #31758, #110703 ) ;
#121225 = ADVANCED_FACE ( 'NONE', ( #59972 ), #70173, .F. ) ;
#121226 = DIRECTION ( 'NONE',  ( 0.7071067811865487940, 0.7071067811865463515, -0.000000000000000000 ) ) ;
#121227 = CARTESIAN_POINT ( 'NONE',  ( -30.48921356237309510, -27.52281430457076894, 5.000000000000000000 ) ) ;
#121228 = ORIENTED_EDGE ( 'NONE', *, *, #112350, .F. ) ;
#121229 = EDGE_CURVE ( 'NONE', #132912, #13889, #137531, .T. ) ;
#121230 = CARTESIAN_POINT ( 'NONE',  ( -2.671830600776463172, 17.25929247661555266, 4.000000000000000000 ) ) ;
#121231 = PLANE ( 'NONE',  #21216 ) ;
#121232 = LINE ( 'NONE', #88634, #14661 ) ;
#121233 = LINE ( 'NONE', #131420, #89929 ) ;
#121234 = CARTESIAN_POINT ( 'NONE',  ( 32.14126352523144448, 4.472830434245837594, 4.472830434245841147 ) ) ;
#121235 = AXIS2_PLACEMENT_3D ( 'NONE', #40120, #116216, #51689 ) ;
#121236 = DIRECTION ( 'NONE',  ( 0.7071067811865487940, 0.7071067811865463515, 0.000000000000000000 ) ) ;
#121237 = EDGE_CURVE ( 'NONE', #135883, #42588, #27989, .T. ) ;
#121238 = EDGE_CURVE ( 'NONE', #27726, #115014, #63851, .T. ) ;
#121239 = ORIENTED_EDGE ( 'NONE', *, *, #75869, .F. ) ;
#121240 = ORIENTED_EDGE ( 'NONE', *, *, #5595, .T. ) ;
#121241 = CARTESIAN_POINT ( 'NONE',  ( 125.6875000000000000, -5.819803920172573086, 5.819803920172572198 ) ) ;
#121242 = ORIENTED_EDGE ( 'NONE', *, *, #108139, .F. ) ;
#121243 = EDGE_LOOP ( 'NONE', ( #100555, #60815, #6089, #107956 ) ) ;
#121244 = CARTESIAN_POINT ( 'NONE',  ( 34.92499999999998295, 22.22500000000000142, 4.000000000000000000 ) ) ;
#121245 = CARTESIAN_POINT ( 'NONE',  ( -17.51078643762690845, -27.52281430457043143, 5.000000000000000000 ) ) ;
#121246 = EDGE_CURVE ( 'NONE', #108262, #99716, #54118, .T. ) ;
#121247 = ORIENTED_EDGE ( 'NONE', *, *, #29011, .T. ) ;
#121248 = SURFACE_STYLE_USAGE ( .BOTH. , #10339 ) ;
#121250 = VECTOR ( 'NONE', #114776, 1000.000000000000000 ) ;
#121249 = CARTESIAN_POINT ( 'NONE',  ( 31.17183060077625356, -2.240707523384262601, 4.000000000000000000 ) ) ;
#121251 = DIRECTION ( 'NONE',  ( -1.000000000000000000, -0.000000000000000000, -0.000000000000000000 ) ) ;
#121252 = ADVANCED_FACE ( 'NONE', ( #139697 ), #96826, .T. ) ;
#121253 = LINE ( 'NONE', #88656, #14088 ) ;
#121254 = CARTESIAN_POINT ( 'NONE',  ( 121.1879301918980900, 6.110000000000002984, -1.637169565754156730 ) ) ;
#121255 = VERTEX_POINT ( 'NONE', #140367 ) ;
#121256 = EDGE_CURVE ( 'NONE', #4323, #136798, #53356, .T. ) ;
#121257 = FACE_OUTER_BOUND ( 'NONE', #19387, .T. ) ;
#121258 = FACE_OUTER_BOUND ( 'NONE', #25776, .T. ) ;
#121259 = CARTESIAN_POINT ( 'NONE',  ( 1.499999999999992673, 16.77039438581779152, 0.4657186855307696716 ) ) ;
#121260 = TOROIDAL_SURFACE ( 'NONE', #139825, 2.500000000000000000, 0.5000000000000000000 ) ;
#121261 = PLANE ( 'NONE',  #52017 ) ;
#121262 = DIRECTION ( 'NONE',  ( 0.5735764363510444941, 0.8191520442889929088, 0.000000000000000000 ) ) ;
#121263 = DIRECTION ( 'NONE',  ( 0.7071067811865487940, -0.7071067811865463515, 0.000000000000000000 ) ) ;
#121264 = VECTOR ( 'NONE', #43096, 1000.000000000000227 ) ;
#121265 = CARTESIAN_POINT ( 'NONE',  ( 52.72502705046289861, 5.819803920172573086, -5.819803920172572198 ) ) ;
#121266 = DIRECTION ( 'NONE',  ( 0.6830127018922180770, -0.6830127018922204085, -0.2588190451025213501 ) ) ;
#121267 = EDGE_CURVE ( 'NONE', #123220, #25358, #75150, .T. ) ;
#121268 = VECTOR ( 'NONE', #89122, 1000.000000000000000 ) ;
#121269 = PLANE ( 'NONE',  #32284 ) ;
#121270 = VERTEX_POINT ( 'NONE', #84580 ) ;
#121271 = ORIENTED_EDGE ( 'NONE', *, *, #98456, .F. ) ;
#121272 = CARTESIAN_POINT ( 'NONE',  ( 43.72916666666667140, 7.950000000000001954, -2.130196079827421762 ) ) ;
#121273 = EDGE_CURVE ( 'NONE', #7243, #141894, #77710, .T. ) ;
#121274 = DIRECTION ( 'NONE',  ( 0.7071067811865486830, -0.7071067811865464625, -0.000000000000000000 ) ) ;
#121275 = VECTOR ( 'NONE', #103397, 999.9999999999998863 ) ;
#121276 = DIRECTION ( 'NONE',  ( -1.321231229586337907E-16, 0.9647414015272155474, -0.2631995976047525887 ) ) ;
#121277 = ORIENTED_EDGE ( 'NONE', *, *, #72580, .F. ) ;
#121278 = ADVANCED_FACE ( 'NONE', ( #130950 ), #117862, .F. ) ;
#121279 = FACE_OUTER_BOUND ( 'NONE', #120875, .T. ) ;
#121280 = CARTESIAN_POINT ( 'NONE',  ( 20.99451991528748707, 28.92564299267952777, 4.000000000000000000 ) ) ;
#121281 = CARTESIAN_POINT ( 'NONE',  ( 34.85459685856477563, -1.637169565754161615, 6.110000000000000320 ) ) ;
#121282 = ORIENTED_EDGE ( 'NONE', *, *, #42703, .F. ) ;
#121283 = CARTESIAN_POINT ( 'NONE',  ( 0.1600000000000007527, 1.128416843727507501, -7.874460342569484794 ) ) ;
#121284 = ORIENTED_EDGE ( 'NONE', *, *, #77140, .T. ) ;
#121285 = ORIENTED_EDGE ( 'NONE', *, *, #67631, .F. ) ;
#121287 = EDGE_CURVE ( 'NONE', #13816, #52532, #57659, .T. ) ;
#121286 = CIRCLE ( 'NONE', #26307, 2.500000000000000444 ) ;
#121288 = FACE_OUTER_BOUND ( 'NONE', #122781, .T. ) ;
#121289 = CARTESIAN_POINT ( 'NONE',  ( -36.48921356237310221, -27.52281430457080802, 5.000000000000000000 ) ) ;
#121290 = CARTESIAN_POINT ( 'NONE',  ( 21.98155265364317046, 18.75929247661553134, 20.33588619593438196 ) ) ;
#121291 = DIRECTION ( 'NONE',  ( 1.000000000000000000, 0.000000000000000000, 0.000000000000000000 ) ) ;
#121292 = VERTEX_POINT ( 'NONE', #6951 ) ;
#121293 = CARTESIAN_POINT ( 'NONE',  ( -27.48921356237309155, -27.52281430457074762, 5.000000000000000000 ) ) ;
#121295 = ORIENTED_EDGE ( 'NONE', *, *, #115290, .T. ) ;
#121294 = CARTESIAN_POINT ( 'NONE',  ( 12.19999999999999574, 0.000000000000000000, -39.50000000000000000 ) ) ;
#121296 = CARTESIAN_POINT ( 'NONE',  ( 82.10459685856476142, 1.637169565754164946, -6.109999999999999432 ) ) ;
#121297 = FACE_OUTER_BOUND ( 'NONE', #107354, .T. ) ;
#121298 = DIRECTION ( 'NONE',  ( 0.000000000000000000, 0.000000000000000000, 1.000000000000000000 ) ) ;
#121299 = EDGE_CURVE ( 'NONE', #3326, #30242, #51240, .T. ) ;
#121300 = FILL_AREA_STYLE ('',( #43054 ) ) ;
#121301 = EDGE_CURVE ( 'NONE', #44009, #104716, #5944, .T. ) ;
#121302 = EDGE_LOOP ( 'NONE', ( #114510, #140074, #138166, #48858 ) ) ;
#121303 = AXIS2_PLACEMENT_3D ( 'NONE', #111944, #99597, #45281 ) ;
#121304 = CYLINDRICAL_SURFACE ( 'NONE', #103219, 0.5000000000000004441 ) ;
#121305 = CARTESIAN_POINT ( 'NONE',  ( 63.34959685856478018, 6.109999999999996767, 1.637169565754163836 ) ) ;
#121306 = LINE ( 'NONE', #45919, #23308 ) ;
#121307 = FACE_OUTER_BOUND ( 'NONE', #35884, .T. ) ;
#121308 = DIRECTION ( 'NONE',  ( -0.6830127018922180770, -0.6830127018922204085, -0.2588190451025213501 ) ) ;
#121309 = ORIENTED_EDGE ( 'NONE', *, *, #59524, .T. ) ;
#121310 = ORIENTED_EDGE ( 'NONE', *, *, #108652, .F. ) ;
#121311 = CARTESIAN_POINT ( 'NONE',  ( 11.20666063542144286, 21.75929247661549937, 4.998822639870701856 ) ) ;
#121312 = EDGE_CURVE ( 'NONE', #63081, #132053, #108410, .T. ) ;
#121313 = VERTEX_POINT ( 'NONE', #62838 ) ;
#121314 = VECTOR ( 'NONE', #138663, 1000.000000000000000 ) ;
#121315 = ORIENTED_EDGE ( 'NONE', *, *, #94203, .F. ) ;
#121316 = LINE ( 'NONE', #32176, #74509 ) ;
#121317 = ORIENTED_EDGE ( 'NONE', *, *, #41090, .T. ) ;
#121318 = CARTESIAN_POINT ( 'NONE',  ( 19.49999999999986500, -13.53360074219760101, 5.000000000000000000 ) ) ;
#121319 = LINE ( 'NONE', #122747, #101171 ) ;
#121320 = LINE ( 'NONE', #54664, #53482 ) ;
#121321 = FACE_BOUND ( 'NONE', #56555, .T. ) ;
#121322 = CARTESIAN_POINT ( 'NONE',  ( -14.14114973822191423, 6.572112357556697759, 4.331981551378865092 ) ) ;
#121323 = CARTESIAN_POINT ( 'NONE',  ( 40.91252705046288440, -7.949999999999998401, -4.867971026610728450E-16 ) ) ;
#121324 = LINE ( 'NONE', #44530, #52639 ) ;
#121326 = EDGE_LOOP ( 'NONE', ( #40281, #2972, #54529, #138343 ) ) ;
#121325 = DIRECTION ( 'NONE',  ( -0.6830127018922180770, -0.6830127018922204085, -0.2588190451025213501 ) ) ;
#121327 = VECTOR ( 'NONE', #37386, 1000.000000000000000 ) ;
#121328 = FACE_OUTER_BOUND ( 'NONE', #12393, .T. ) ;
#121329 = ORIENTED_EDGE ( 'NONE', *, *, #108159, .T. ) ;
#121330 = AXIS2_PLACEMENT_3D ( 'NONE', #24804, #77778, #11767 ) ;
#121331 = ORIENTED_EDGE ( 'NONE', *, *, #36199, .F. ) ;
#121332 = CARTESIAN_POINT ( 'NONE',  ( 74.14126352523145158, 4.472830434245835818, 4.472830434245840259 ) ) ;
#121333 = ORIENTED_EDGE ( 'NONE', *, *, #50450, .T. ) ;
#121334 = FACE_OUTER_BOUND ( 'NONE', #116861, .T. ) ;
#121335 = LINE ( 'NONE', #56131, #62915 ) ;
#121336 = EDGE_CURVE ( 'NONE', #102047, #33411, #80114, .T. ) ;
#121337 = ORIENTED_EDGE ( 'NONE', *, *, #27374, .T. ) ;
#121338 = CARTESIAN_POINT ( 'NONE',  ( -57.18398860626899705, 28.73617430169827358, 5.000000000000000000 ) ) ;
#121339 = CARTESIAN_POINT ( 'NONE',  ( 122.7708333333333286, -7.949999999999998401, -2.130196079827426203 ) ) ;
#121340 = DIRECTION ( 'NONE',  ( 1.000000000000000000, 0.000000000000000000, 0.000000000000000000 ) ) ;
#121341 = DIRECTION ( 'NONE',  ( -0.6830127018922181881, 0.6830127018922202975, -0.2588190451025214056 ) ) ;
#121342 = AXIS2_PLACEMENT_3D ( 'NONE', #55088, #66679, #99259 ) ;
#121343 = CARTESIAN_POINT ( 'NONE',  ( -5.999999999999952927, -4.068876922607767455, 4.000000000000000000 ) ) ;
#121344 = DIRECTION ( 'NONE',  ( -0.000000000000000000, 0.000000000000000000, 1.000000000000000000 ) ) ;
#121345 = DIRECTION ( 'NONE',  ( 0.000000000000000000, -1.000000000000000000, 0.000000000000000000 ) ) ;
#121346 = ORIENTED_EDGE ( 'NONE', *, *, #93905, .T. ) ;
#121347 = ORIENTED_EDGE ( 'NONE', *, *, #16840, .T. ) ;
#121348 = DIRECTION ( 'NONE',  ( -0.7071067811865487940, 0.7071067811865463515, 0.000000000000000000 ) ) ;
#121349 = DIRECTION ( 'NONE',  ( -1.000000000000000000, -0.000000000000000000, 0.000000000000000000 ) ) ;
#121350 = ORIENTED_EDGE ( 'NONE', *, *, #135622, .T. ) ;
#121351 = ORIENTED_EDGE ( 'NONE', *, *, #9925, .F. ) ;
#121352 = AXIS2_PLACEMENT_3D ( 'NONE', #30653, #140799, #8818 ) ;
#121353 = EDGE_CURVE ( 'NONE', #103613, #73568, #129481, .T. ) ;
#121354 = EDGE_CURVE ( 'NONE', #123367, #108418, #47730, .T. ) ;
#121355 = CARTESIAN_POINT ( 'NONE',  ( 26.99999999999981526, 2.587461875839214720, 4.000000000000000000 ) ) ;
#121356 = EDGE_LOOP ( 'NONE', ( #21441, #87119, #7514 ) ) ;
#121357 = LINE ( 'NONE', #44569, #16229 ) ;
#121359 = EDGE_CURVE ( 'NONE', #61259, #49419, #41780, .T. ) ;
#121358 = AXIS2_PLACEMENT_3D ( 'NONE', #47079, #35459, #102119 ) ;
#121360 = EDGE_CURVE ( 'NONE', #85633, #51247, #19308, .T. ) ;
#121361 = DIRECTION ( 'NONE',  ( 0.7071067811865486830, 0.7071067811865464625, 0.000000000000000000 ) ) ;
#121362 = AXIS2_PLACEMENT_3D ( 'NONE', #97277, #41502, #76299 ) ;
#121363 = CARTESIAN_POINT ( 'NONE',  ( 25.42080628287044064, 3.047499999999997655, 5.278424836066143655 ) ) ;
#121364 = DIRECTION ( 'NONE',  ( -0.000000000000000000, 0.3543493200069153248, 0.9351131265310292928 ) ) ;
#121365 = ORIENTED_EDGE ( 'NONE', *, *, #27330, .T. ) ;
#121366 = EDGE_CURVE ( 'NONE', #79450, #626, #130228, .T. ) ;
#121367 = DIRECTION ( 'NONE',  ( 0.000000000000000000, 0.000000000000000000, 1.000000000000000000 ) ) ;
#121368 = ORIENTED_EDGE ( 'NONE', *, *, #115404, .F. ) ;
#121369 = LINE ( 'NONE', #12608, #3473 ) ;
#121371 = ORIENTED_EDGE ( 'NONE', *, *, #455, .T. ) ;
#121370 = CARTESIAN_POINT ( 'NONE',  ( 72.48921356237309510, -27.52281430457106026, 5.000000000000000000 ) ) ;
#121372 = VERTEX_POINT ( 'NONE', #86722 ) ;
#121373 = DIRECTION ( 'NONE',  ( -0.7071067811865487940, 0.7071067811865463515, -0.000000000000000000 ) ) ;
#121374 = DIRECTION ( 'NONE',  ( 0.000000000000000000, 0.000000000000000000, -1.000000000000000000 ) ) ;
#121375 = CARTESIAN_POINT ( 'NONE',  ( 23.81601139373100295, 28.73617430169770870, 5.000000000000000000 ) ) ;
#121376 = EDGE_CURVE ( 'NONE', #19510, #85156, #75843, .T. ) ;
#121377 = ORIENTED_EDGE ( 'NONE', *, *, #17042, .F. ) ;
#121378 = AXIS2_PLACEMENT_3D ( 'NONE', #8965, #110450, #96023 ) ;
#121379 = DIRECTION ( 'NONE',  ( -0.5735764363510507113, 0.8191520442889885789, 1.003171929053520926E-16 ) ) ;
#121380 = ORIENTED_EDGE ( 'NONE', *, *, #66738, .F. ) ;
#121381 = DIRECTION ( 'NONE',  ( 0.7071067811865487940, 0.7071067811865463515, -0.000000000000000000 ) ) ;
#121382 = CARTESIAN_POINT ( 'NONE',  ( 3.299744871391591339, -27.71228299555208352, 4.000000000000000000 ) ) ;
#121383 = EDGE_CURVE ( 'NONE', #85323, #93595, #24996, .T. ) ;
#121384 = DIRECTION ( 'NONE',  ( -0.000000000000000000, 0.3543493200069153248, 0.9351131265310292928 ) ) ;
#121385 = FILL_AREA_STYLE_COLOUR ( '', #35413 ) ;
#121386 = CARTESIAN_POINT ( 'NONE',  ( 16.49999999999988631, -2.568876922607793212, 4.000000000000000000 ) ) ;
#121387 = FACE_OUTER_BOUND ( 'NONE', #103499, .T. ) ;
#121388 = LINE ( 'NONE', #75075, #96933 ) ;
#121389 = EDGE_LOOP ( 'NONE', ( #115683, #72731, #107896, #114523 ) ) ;
#121390 = FACE_OUTER_BOUND ( 'NONE', #38074, .T. ) ;
#121391 = ORIENTED_EDGE ( 'NONE', *, *, #122322, .T. ) ;
#121392 = EDGE_CURVE ( 'NONE', #92828, #109156, #135236, .T. ) ;
#121393 = DIRECTION ( 'NONE',  ( 0.000000000000000000, -0.9647414015272164356, 0.2631995976047502017 ) ) ;
#121394 = DIRECTION ( 'NONE',  ( 1.000000000000000000, 0.000000000000000000, 0.000000000000000000 ) ) ;
#121395 = CARTESIAN_POINT ( 'NONE',  ( -34.42500000000001137, 21.72500000000000142, 0.5000000000000000000 ) ) ;
#121396 = VERTEX_POINT ( 'NONE', #112041 ) ;
#121397 = LINE ( 'NONE', #87363, #62274 ) ;
#121398 = DIRECTION ( 'NONE',  ( 0.6830127018922180770, -0.6830127018922204085, -0.2588190451025213501 ) ) ;
#121399 = DIRECTION ( 'NONE',  ( 0.3543493200069162685, -0.000000000000000000, -0.9351131265310288487 ) ) ;
#121400 = ORIENTED_EDGE ( 'NONE', *, *, #60870, .T. ) ;
#121401 = EDGE_CURVE ( 'NONE', #39324, #107217, #109881, .T. ) ;
#121402 = FILL_AREA_STYLE_COLOUR ( '', #23366 ) ;
#121403 = CARTESIAN_POINT ( 'NONE',  ( 12.29974487139158512, -27.71228299555214747, 4.000000000000000000 ) ) ;
#121404 = UNCERTAINTY_MEASURE_WITH_UNIT (LENGTH_MEASURE( 1.000000000000000082E-05 ), #97784, 'distance_accuracy_value', 'NONE');
#121405 = DIRECTION ( 'NONE',  ( -0.000000000000000000, 0.3543493200069153248, 0.9351131265310292928 ) ) ;
#121406 = SURFACE_STYLE_FILL_AREA ( #122117 ) ;
#121407 = DIRECTION ( 'NONE',  ( -0.000000000000000000, 0.000000000000000000, 1.000000000000000000 ) ) ;
#121408 = CARTESIAN_POINT ( 'NONE',  ( 62.03709685856478728, -3.054999999999999272, -5.291415217122919401 ) ) ;
#121409 = CIRCLE ( 'NONE', #58980, 2.055000000000001048 ) ;
#121410 = DIRECTION ( 'NONE',  ( -0.000000000000000000, -0.3543493200069152693, 0.9351131265310292928 ) ) ;
#121411 = EDGE_CURVE ( 'NONE', #100628, #45393, #80145, .T. ) ;
#121412 = EDGE_CURVE ( 'NONE', #6385, #95968, #67105, .T. ) ;
#121413 = DIRECTION ( 'NONE',  ( -0.7071067811865486830, -0.7071067811865464625, 0.000000000000000000 ) ) ;
#121414 = LINE ( 'NONE', #54759, #37157 ) ;
#121415 = LINE ( 'NONE', #22777, #108874 ) ;
#121416 = ORIENTED_EDGE ( 'NONE', *, *, #124245, .T. ) ;
#121417 = CARTESIAN_POINT ( 'NONE',  ( -5.206660635421487271, 21.75929247661549937, 4.998822639870708073 ) ) ;
#121418 = EDGE_LOOP ( 'NONE', ( #20172, #93487, #47259, #126067 ) ) ;
#121419 = CARTESIAN_POINT ( 'NONE',  ( -24.29974487139158867, -27.71228299555223273, 4.000000000000000000 ) ) ;
#121420 = DIRECTION ( 'NONE',  ( 0.7071067811865487940, -0.7071067811865463515, 0.000000000000000000 ) ) ;
#121421 = EDGE_CURVE ( 'NONE', #99607, #80827, #122905, .T. ) ;
#121422 = CARTESIAN_POINT ( 'NONE',  ( 30.32816939922332367, 20.25929247661551003, 4.000000000000000000 ) ) ;
#121423 = CARTESIAN_POINT ( 'NONE',  ( 69.48921356237309510, -27.52281430457103895, 5.000000000000000000 ) ) ;
#121424 = LINE ( 'NONE', #99666, #6799 ) ;
#121425 = EDGE_CURVE ( 'NONE', #31789, #139138, #110568, .T. ) ;
#121426 = LINE ( 'NONE', #101099, #27868 ) ;
#121427 = DIRECTION ( 'NONE',  ( 0.000000000000000000, 0.000000000000000000, 1.000000000000000000 ) ) ;
#121428 = ORIENTED_EDGE ( 'NONE', *, *, #92658, .T. ) ;
#121429 = EDGE_LOOP ( 'NONE', ( #133258, #96485, #81487, #119495 ) ) ;
#121430 = CARTESIAN_POINT ( 'NONE',  ( 17.51078643762690845, -27.52281430457043143, 5.000000000000000000 ) ) ;
#121431 = SURFACE_STYLE_USAGE ( .BOTH. , #34433 ) ;
#121432 = UNCERTAINTY_MEASURE_WITH_UNIT (LENGTH_MEASURE( 1.000000000000000082E-05 ), #1627, 'distance_accuracy_value', 'NONE');
#121433 = CONICAL_SURFACE ( 'NONE', #139987, 1.249999999999969802, 0.2617993877991415808 ) ;
#121434 = CARTESIAN_POINT ( 'NONE',  ( -24.32816939922336275, -12.74070752338415602, 4.000000000000000000 ) ) ;
#121435 = CARTESIAN_POINT ( 'NONE',  ( 23.99451991528749062, 28.92564299267954908, 4.000000000000000000 ) ) ;
#121436 = CARTESIAN_POINT ( 'NONE',  ( 86.26669371712955581, -7.949999999999999289, 2.130196079827424427 ) ) ;
#121437 = DIRECTION ( 'NONE',  ( -0.7071067811865486830, 0.7071067811865464625, 0.000000000000000000 ) ) ;
#121438 = AXIS2_PLACEMENT_3D ( 'NONE', #76917, #12329, #43542 ) ;
#121439 = CARTESIAN_POINT ( 'NONE',  ( 34.92499999999998295, -22.22500000000000142, 4.500000000000000888 ) ) ;
#121440 = ORIENTED_EDGE ( 'NONE', *, *, #1519, .F. ) ;
#121441 = CARTESIAN_POINT ( 'NONE',  ( 73.47916666666664298, -7.950000000000001066, 2.130196079827424427 ) ) ;
#121442 = EDGE_CURVE ( 'NONE', #68957, #3959, #22835, .T. ) ;
#121443 = PLANE ( 'NONE',  #74747 ) ;
#121444 = VECTOR ( 'NONE', #132170, 1000.000000000000000 ) ;
#121445 = DIRECTION ( 'NONE',  ( 0.3543493200069162685, -0.000000000000000000, -0.9351131265310288487 ) ) ;
#121446 = CARTESIAN_POINT ( 'NONE',  ( 184.1500000000000057, -30.18000000000009564, 12.69999999999954454 ) ) ;
#121447 = EDGE_LOOP ( 'NONE', ( #114173, #14313, #53232, #113171 ) ) ;
#121448 = EDGE_CURVE ( 'NONE', #85002, #77505, #72497, .T. ) ;
#121449 = LINE ( 'NONE', #31604, #14330 ) ;
#121450 = VERTEX_POINT ( 'NONE', #44677 ) ;
#121451 = PRESENTATION_LAYER_ASSIGNMENT (  '', '', ( #5732 ) ) ;
#121452 = CARTESIAN_POINT ( 'NONE',  ( -4.396568071053548188, -14.24070752338413648, 19.24067776001725250 ) ) ;
#121453 = CARTESIAN_POINT ( 'NONE',  ( 71.31293019189810423, -1.637169565754159617, -6.110000000000001208 ) ) ;
#121454 = ORIENTED_EDGE ( 'NONE', *, *, #24593, .F. ) ;
#121455 = DIRECTION ( 'NONE',  ( -0.6830127018922180770, -0.6830127018922204085, -0.2588190451025213501 ) ) ;
#121456 = CARTESIAN_POINT ( 'NONE',  ( 20.20519093902540320, 3.061616997868383634E-16, -2.500000000000000444 ) ) ;
#121457 = DIRECTION ( 'NONE',  ( -0.7071067811865486830, -0.7071067811865464625, 0.000000000000000000 ) ) ;
#121458 = DIRECTION ( 'NONE',  ( 0.7071067811865486830, -0.7071067811865464625, -0.000000000000000000 ) ) ;
#121459 = DIRECTION ( 'NONE',  ( -0.7071067811865486830, -0.7071067811865464625, 0.000000000000000000 ) ) ;
#121461 = EDGE_LOOP ( 'NONE', ( #66434, #121186, #79998, #70896 ) ) ;
#121460 = DIRECTION ( 'NONE',  ( -0.3543493200069163240, -0.000000000000000000, -0.9351131265310288487 ) ) ;
#121462 = FACE_OUTER_BOUND ( 'NONE', #26166, .T. ) ;
#121463 = PLANE ( 'NONE',  #123513 ) ;
#121464 = FACE_OUTER_BOUND ( 'NONE', #142577, .T. ) ;
#121465 = ORIENTED_EDGE ( 'NONE', *, *, #32094, .F. ) ;
#121466 = VECTOR ( 'NONE', #88120, 1000.000000000000000 ) ;
#121467 = EDGE_CURVE ( 'NONE', #125463, #138848, #34470, .T. ) ;
#121468 = EDGE_LOOP ( 'NONE', ( #33539, #90354, #93421, #88613 ) ) ;
#121469 = CARTESIAN_POINT ( 'NONE',  ( 66.20876352523144703, -7.482591942790329030E-16, 6.110000000000001208 ) ) ;
#121470 = AXIS2_PLACEMENT_3D ( 'NONE', #113648, #14348, #58632 ) ;
#121471 = VECTOR ( 'NONE', #69547, 1000.000000000000000 ) ;
#121472 = VERTEX_POINT ( 'NONE', #88871 ) ;
#121473 =( GEOMETRIC_REPRESENTATION_CONTEXT ( 3 ) GLOBAL_UNCERTAINTY_ASSIGNED_CONTEXT ( ( #43507 ) ) GLOBAL_UNIT_ASSIGNED_CONTEXT ( ( #29495, #15725, #126666 ) ) REPRESENTATION_CONTEXT ( 'NONE', 'WORKASPACE' ) );
#121474 = DIRECTION ( 'NONE',  ( -0.7071067811865486830, 0.7071067811865464625, 0.000000000000000000 ) ) ;
#121475 = CARTESIAN_POINT ( 'NONE',  ( -1.499999999999984013, -4.912538124160710673, 4.000000000000000000 ) ) ;
#121476 = CARTESIAN_POINT ( 'NONE',  ( 30.48921356237309510, -27.52281430457076894, 5.000000000000000000 ) ) ;
#121477 = CARTESIAN_POINT ( 'NONE',  ( -9.328169399223467551, 11.25929247661560240, 4.000000000000000000 ) ) ;
#121478 = PLANE ( 'NONE',  #110358 ) ;
#121479 = ORIENTED_EDGE ( 'NONE', *, *, #71199, .T. ) ;
#121480 = ORIENTED_EDGE ( 'NONE', *, *, #66494, .T. ) ;
#121481 = LINE ( 'NONE', #86008, #12089 ) ;
#121482 = DIRECTION ( 'NONE',  ( 0.000000000000000000, -1.000000000000000000, 0.000000000000000000 ) ) ;
#121483 = ORIENTED_EDGE ( 'NONE', *, *, #112399, .T. ) ;
#121484 = DIRECTION ( 'NONE',  ( -0.7071067811865486830, -0.7071067811865464625, -0.000000000000000000 ) ) ;
#121485 = CARTESIAN_POINT ( 'NONE',  ( 23.30673006690386728, -3.740707523384244837, 12.88036043432862243 ) ) ;
#121486 = PLANE ( 'NONE',  #109502 ) ;
#121487 = ORIENTED_EDGE ( 'NONE', *, *, #80699, .F. ) ;
#121488 = FACE_OUTER_BOUND ( 'NONE', #94266, .T. ) ;
#121489 = DIRECTION ( 'NONE',  ( -0.7071067811865486830, -0.7071067811865464625, 0.000000000000000000 ) ) ;
#121490 = DIRECTION ( 'NONE',  ( -1.000000000000000000, -0.000000000000000000, -0.000000000000000000 ) ) ;
#121491 = DIRECTION ( 'NONE',  ( 0.000000000000000000, -1.000000000000000000, 0.000000000000000000 ) ) ;
#121492 = SURFACE_SIDE_STYLE ('',( #65749 ) ) ;
#121493 = FILL_AREA_STYLE_COLOUR ( '', #85998 ) ;
#121494 = DIRECTION ( 'NONE',  ( 1.000000000000000000, 0.000000000000000000, 0.000000000000000000 ) ) ;
#121495 = VERTEX_POINT ( 'NONE', #11982 ) ;
#121496 = ORIENTED_EDGE ( 'NONE', *, *, #57373, .T. ) ;
#121497 = CARTESIAN_POINT ( 'NONE',  ( 107.5370968585647944, -3.054999999999998828, -5.291415217122919401 ) ) ;
#121498 = ORIENTED_EDGE ( 'NONE', *, *, #116671, .F. ) ;
#121499 = VERTEX_POINT ( 'NONE', #88147 ) ;
#121500 = DIRECTION ( 'NONE',  ( -0.000000000000000000, -0.000000000000000000, 1.000000000000000000 ) ) ;
#121501 = AXIS2_PLACEMENT_3D ( 'NONE', #47765, #68795, #80384 ) ;
#121502 = CARTESIAN_POINT ( 'NONE',  ( 11.99999999999991296, -8.151047557385055597, -8.977947279169828931 ) ) ;
#121503 = CARTESIAN_POINT ( 'NONE',  ( -12.20000000000000284, -25.83999999999998565, -1.121314957791154772E-16 ) ) ;
#121504 = VERTEX_POINT ( 'NONE', #56270 ) ;
#121505 = DIRECTION ( 'NONE',  ( -1.000000000000000000, -1.224606353822377258E-16, -0.000000000000000000 ) ) ;
#121506 = CARTESIAN_POINT ( 'NONE',  ( 0.000000000000000000, 0.000000000000000000, 5.000000000000000000 ) ) ;
#121507 = CARTESIAN_POINT ( 'NONE',  ( 35.99999999999999289, 0.000000000000000000, -7.950000000000000178 ) ) ;
#121508 = ADVANCED_FACE ( 'NONE', ( #56965 ), #98991, .F. ) ;
#121511 = EDGE_CURVE ( 'NONE', #91841, #41843, #122166, .T. ) ;
#121510 = CARTESIAN_POINT ( 'NONE',  ( -42.18398860626899705, 28.73617430169816700, 5.000000000000000000 ) ) ;
#121509 = LINE ( 'NONE', #66452, #94376 ) ;
#121512 = CARTESIAN_POINT ( 'NONE',  ( 11.51078643762690490, -27.52281430457047406, 5.000000000000000000 ) ) ;
#121513 = ADVANCED_FACE ( 'NONE', ( #121462 ), #100444, .T. ) ;
#121514 = FACE_OUTER_BOUND ( 'NONE', #141787, .T. ) ;
#121515 = EDGE_LOOP ( 'NONE', ( #140190, #93209, #51591, #140085 ) ) ;
#121516 = DIRECTION ( 'NONE',  ( -0.7071067811865487940, 0.7071067811865463515, 0.000000000000000000 ) ) ;
#121517 = DIRECTION ( 'NONE',  ( -0.000000000000000000, 0.000000000000000000, 1.000000000000000000 ) ) ;
#121518 = ADVANCED_FACE ( 'NONE', ( #123648 ), #66398, .F. ) ;
#121519 = ORIENTED_EDGE ( 'NONE', *, *, #37258, .F. ) ;
#121520 = ORIENTED_EDGE ( 'NONE', *, *, #13862, .T. ) ;
#121521 = EDGE_CURVE ( 'NONE', #138330, #110525, #75433, .T. ) ;
#121522 = ADVANCED_FACE ( 'NONE', ( #101138 ), #133785, .F. ) ;
#121523 = ORIENTED_EDGE ( 'NONE', *, *, #133885, .T. ) ;
#121524 = CARTESIAN_POINT ( 'NONE',  ( 56.43793019189809712, -6.110000000000001208, 1.637169565754158951 ) ) ;
#121525 = ORIENTED_EDGE ( 'NONE', *, *, #39422, .F. ) ;
#121526 = EDGE_CURVE ( 'NONE', #2478, #16173, #36119, .T. ) ;
#121527 = EDGE_CURVE ( 'NONE', #46199, #85411, #38750, .T. ) ;
#121528 = FACE_OUTER_BOUND ( 'NONE', #66461, .T. ) ;
#121529 = AXIS2_PLACEMENT_3D ( 'NONE', #47695, #35386, #49102 ) ;
#121530 = CARTESIAN_POINT ( 'NONE',  ( 0.7749729495371054933, 4.461849672132300881, 4.461849672132299105 ) ) ;
#121531 = CARTESIAN_POINT ( 'NONE',  ( 102.3754301918981184, -5.291415217122920289, -3.055000000000001492 ) ) ;
#121532 = CARTESIAN_POINT ( 'NONE',  ( 30.70701326429282929, -21.74070752338406365, 4.999753212805224223 ) ) ;
#121533 = AXIS2_PLACEMENT_3D ( 'NONE', #4412, #135725, #125575 ) ;
#121534 = ADVANCED_FACE ( 'NONE', ( #105413 ), #116305, .F. ) ;
#121535 = ORIENTED_EDGE ( 'NONE', *, *, #127854, .F. ) ;
#121536 = FACE_OUTER_BOUND ( 'NONE', #4394, .T. ) ;
#121537 = DIRECTION ( 'NONE',  ( 1.000000000000000000, 0.000000000000000000, 0.000000000000000000 ) ) ;
#121538 =( BOUNDED_CURVE ( )  B_SPLINE_CURVE ( 2, ( #78008, #57699, #101878, #2544, #67878, #46851, #1805, #101161, #11270, #35948, #112063, #55540, #25020 ),
 .UNSPECIFIED., .F., .F. ) 
 B_SPLINE_CURVE_WITH_KNOTS ( ( 3, 2, 2, 2, 2, 2, 3 ),
 ( 0.1499999999999999944, 0.1527777777777777901, 0.1555555555555555580, 0.1583333333333333259, 0.1611111111111111216, 0.1638888888888888895, 0.1666666666666666574 ),
 .UNSPECIFIED. ) 
 CURVE ( )  GEOMETRIC_REPRESENTATION_ITEM ( )  RATIONAL_B_SPLINE_CURVE ( ( 1.000000000000000000, 0.9659258262890683122, 1.000000000000000000, 0.9659258262890683122, 1.000000000000000000, 0.9659258262890683122, 1.000000000000000000, 0.9659258262890683122, 1.000000000000000000, 0.9659258262890683122, 1.000000000000000000, 0.9659258262890683122, 1.000000000000000000 ) ) 
 REPRESENTATION_ITEM ( '' )  );
#121539 = LINE ( 'NONE', #90348, #14323 ) ;
#121540 = LINE ( 'NONE', #88223, #142401 ) ;
#121541 = ADVANCED_FACE ( 'NONE', ( #113433 ), #16999, .T. ) ;
#121542 = ORIENTED_EDGE ( 'NONE', *, *, #67771, .F. ) ;
#121543 = DIRECTION ( 'NONE',  ( -0.000000000000000000, -0.3543493200069152693, 0.9351131265310292928 ) ) ;
#121544 = VECTOR ( 'NONE', #15818, 999.9999999999998863 ) ;
#121545 = AXIS2_PLACEMENT_3D ( 'NONE', #37884, #60351, #116841 ) ;
#121546 = ORIENTED_EDGE ( 'NONE', *, *, #105046, .T. ) ;
#121547 = VERTEX_POINT ( 'NONE', #59805 ) ;
#121548 = ORIENTED_EDGE ( 'NONE', *, *, #19629, .F. ) ;
#121549 = CARTESIAN_POINT ( 'NONE',  ( 123.5787635252314516, -7.482591942790325086E-16, 6.109999999999998543 ) ) ;
#121550 =( BOUNDED_CURVE ( )  B_SPLINE_CURVE ( 2, ( #116558, #85336, #108491, #141909, #18641, #105653, #139770, #84651, #29527, #42601, #139034, #131018, #119386 ),
 .UNSPECIFIED., .F., .T. ) 
 B_SPLINE_CURVE_WITH_KNOTS ( ( 3, 2, 2, 2, 2, 2, 3 ),
 ( 0.4833333333333333370, 0.4861111111111111049, 0.4888888888888888729, 0.4916666666666666408, 0.4944444444444444642, 0.4972222222222222321, 0.5000000000000000000 ),
 .UNSPECIFIED. ) 
 CURVE ( )  GEOMETRIC_REPRESENTATION_ITEM ( )  RATIONAL_B_SPLINE_CURVE ( ( 1.000000000000000000, 0.9659258262890683122, 1.000000000000000000, 0.9659258262890683122, 1.000000000000000000, 0.9659258262890683122, 1.000000000000000000, 0.9659258262890683122, 1.000000000000000000, 0.9659258262890683122, 1.000000000000000000, 0.9659258262890683122, 1.000000000000000000 ) ) 
 REPRESENTATION_ITEM ( '' )  );
#121551 = CARTESIAN_POINT ( 'NONE',  ( 10.32500000000000107, -9.500000000000001776, 0.000000000000000000 ) ) ;
#121552 = DIRECTION ( 'NONE',  ( 1.000000000000000000, 0.000000000000000000, 0.000000000000000000 ) ) ;
#121553 = ORIENTED_EDGE ( 'NONE', *, *, #44094, .F. ) ;
#121554 = LINE ( 'NONE', #87518, #65029 ) ;
#121555 = ORIENTED_EDGE ( 'NONE', *, *, #37070, .T. ) ;
#121556 = EDGE_CURVE ( 'NONE', #91883, #56418, #135653, .T. ) ;
#121557 = COLOUR_RGB ( '', 0.66274510, 0.83137255, 0.94901961) ;
#121558 = VECTOR ( 'NONE', #50426, 1000.000000000000000 ) ;
#121559 = CARTESIAN_POINT ( 'NONE',  ( 15.72873647476855297, 5.808823158059031044, -5.808823158059038150 ) ) ;
#121560 = CARTESIAN_POINT ( 'NONE',  ( -11.51078643762690490, -27.52281430457047406, 5.000000000000000000 ) ) ;
#121561 =( GEOMETRIC_REPRESENTATION_CONTEXT ( 3 ) GLOBAL_UNCERTAINTY_ASSIGNED_CONTEXT ( ( #67822 ) ) GLOBAL_UNIT_ASSIGNED_CONTEXT ( ( #14391, #102843, #70252 ) ) REPRESENTATION_CONTEXT ( 'NONE', 'WORKASPACE' ) );
#121562 = CARTESIAN_POINT ( 'NONE',  ( 27.99999999999996803, -57.14999999999999147, 49.92499999999997584 ) ) ;
#121563 = VECTOR ( 'NONE', #47777, 1000.000000000000000 ) ;
#121564 = LINE ( 'NONE', #487, #18861 ) ;
#121565 = VERTEX_POINT ( 'NONE', #16239 ) ;
#121566 = ORIENTED_EDGE ( 'NONE', *, *, #43042, .T. ) ;
#121568 = ORIENTED_EDGE ( 'NONE', *, *, #89791, .T. ) ;
#121567 = EDGE_CURVE ( 'NONE', #76029, #69406, #69996, .T. ) ;
#121569 =( NAMED_UNIT ( * ) PLANE_ANGLE_UNIT ( ) SI_UNIT ( $, .RADIAN. ) );
#121570 = CARTESIAN_POINT ( 'NONE',  ( -6.489213562373093325, -27.52281430457059841, 5.000000000000000000 ) ) ;
#121571 = FACE_OUTER_BOUND ( 'NONE', #15963, .T. ) ;
#121572 = ADVANCED_FACE ( 'NONE', ( #102597 ), #138066, .T. ) ;
#121573 = LINE ( 'NONE', #56382, #124795 ) ;
#121574 = FACE_OUTER_BOUND ( 'NONE', #81959, .T. ) ;
#121575 = DIRECTION ( 'NONE',  ( 0.7071067811865486830, -0.7071067811865464625, -0.000000000000000000 ) ) ;
#121576 = CARTESIAN_POINT ( 'NONE',  ( -20.51078643762690490, -27.52281430457041012, 5.000000000000000000 ) ) ;
#121577 = EDGE_CURVE ( 'NONE', #60821, #1343, #50348, .T. ) ;
#121578 = ORIENTED_EDGE ( 'NONE', *, *, #45677, .F. ) ;
#121579 = CARTESIAN_POINT ( 'NONE',  ( -32.99999999999976552, -10.44781430457071991, 5.000000000000000000 ) ) ;
#121580 = ORIENTED_EDGE ( 'NONE', *, *, #8265, .F. ) ;
#121581 = CARTESIAN_POINT ( 'NONE',  ( 5.755190629914537226, 2.055000000000001048, 2.516649172247811554E-16 ) ) ;
#121582 = VERTEX_POINT ( 'NONE', #136618 ) ;
#121583 = ADVANCED_FACE ( 'NONE', ( #60536 ), #125037, .F. ) ;
#121584 = ADVANCED_FACE ( 'NONE', ( #3245 ), #71386, .T. ) ;
#121585 = CARTESIAN_POINT ( 'NONE',  ( -16.49999999999988276, -1.592773361805376098, -6.492772025301186467 ) ) ;
#121587 = ORIENTED_EDGE ( 'NONE', *, *, #38489, .F. ) ;
#121586 = CARTESIAN_POINT ( 'NONE',  ( -27.18398860626900060, 28.73617430169806042, 5.000000000000000000 ) ) ;
#121588 = LINE ( 'NONE', #77423, #35359 ) ;
#121589 = ORIENTED_EDGE ( 'NONE', *, *, #30395, .F. ) ;
#121590 = ORIENTED_EDGE ( 'NONE', *, *, #20592, .T. ) ;
#121591 = CARTESIAN_POINT ( 'NONE',  ( -24.18398860626899705, 28.73617430169804265, 5.000000000000000000 ) ) ;
#121592 = UNCERTAINTY_MEASURE_WITH_UNIT (LENGTH_MEASURE( 1.000000000000000082E-05 ), #83434, 'distance_accuracy_value', 'NONE');
#121593 = ORIENTED_EDGE ( 'NONE', *, *, #96225, .T. ) ;
#121594 = ADVANCED_FACE ( 'NONE', ( #27149 ), #82277, .F. ) ;
#121595 = CARTESIAN_POINT ( 'NONE',  ( 22.93003974513577603, -0.7407075233842735917, 13.87443053587605490 ) ) ;
#121596 = CARTESIAN_POINT ( 'NONE',  ( 110.6208603837962272, -6.884901960086286188, 3.974999999999997424 ) ) ;
#121597 = PRESENTATION_STYLE_ASSIGNMENT (( #77433 ) ) ;
#121598 = LINE ( 'NONE', #107852, #6558 ) ;
#121599 = ADVANCED_FACE ( 'NONE', ( #135920 ), #93837, .F. ) ;
#121600 = CARTESIAN_POINT ( 'NONE',  ( -31.49999999999977973, -13.91253812416061386, 4.000000000000000000 ) ) ;
#121601 = LINE ( 'NONE', #131071, #136384 ) ;
#121602 = CARTESIAN_POINT ( 'NONE',  ( 15.16666666666666785, -5.278424836066145431, -3.047499999999993658 ) ) ;
#121603 = CARTESIAN_POINT ( 'NONE',  ( 13.97873647476855119, -5.808823158059033709, 5.808823158059035485 ) ) ;
#121604 = LINE ( 'NONE', #533, #99844 ) ;
#121605 = CARTESIAN_POINT ( 'NONE',  ( -27.48921356237309155, -27.52281430457074762, 5.000000000000000000 ) ) ;
#121606 = VERTEX_POINT ( 'NONE', #127171 ) ;
#121607 = ORIENTED_EDGE ( 'NONE', *, *, #75237, .T. ) ;
#121608 = CARTESIAN_POINT ( 'NONE',  ( 15.70710678118643422, 20.25929247661551003, 5.000000000000000000 ) ) ;
#121609 = ORIENTED_EDGE ( 'NONE', *, *, #87957, .T. ) ;
#121610 = EDGE_CURVE ( 'NONE', #98423, #110210, #70697, .T. ) ;
#121611 = PLANE ( 'NONE',  #110215 ) ;
#121612 = CARTESIAN_POINT ( 'NONE',  ( -31.17183060077624646, -17.24070752338410273, 4.000000000000000000 ) ) ;
#121613 = DIRECTION ( 'NONE',  ( -0.000000000000000000, 0.3543493200069153248, 0.9351131265310292928 ) ) ;
#121614 = CARTESIAN_POINT ( 'NONE',  ( 128.5065401839123069, -48.97294124528379911, -39.12804664298174373 ) ) ;
#121615 = EDGE_LOOP ( 'NONE', ( #44105, #130217, #50991, #87796 ) ) ;
#121616 = DIRECTION ( 'NONE',  ( 0.7071067811865487940, 0.7071067811865463515, 0.000000000000000000 ) ) ;
#121617 = LINE ( 'NONE', #78148, #141476 ) ;
#121618 = FACE_OUTER_BOUND ( 'NONE', #66931, .T. ) ;
#121619 = EDGE_CURVE ( 'NONE', #135612, #21613, #92389, .T. ) ;
#121620 =( LENGTH_UNIT ( ) NAMED_UNIT ( * ) SI_UNIT ( .MILLI., .METRE. ) );
#121621 = DIRECTION ( 'NONE',  ( -0.000000000000000000, -0.000000000000000000, 1.000000000000000000 ) ) ;
#121623 = ORIENTED_EDGE ( 'NONE', *, *, #83391, .F. ) ;
#121622 = DIRECTION ( 'NONE',  ( 0.7071067811865486830, -0.7071067811865464625, -0.000000000000000000 ) ) ;
#121624 = CARTESIAN_POINT ( 'NONE',  ( 28.82816939922332722, 21.75929247661549581, 4.000000000000000000 ) ) ;
#121625 = DIRECTION ( 'NONE',  ( -0.7071067811865486830, -0.7071067811865464625, 0.000000000000000000 ) ) ;
#121626 = CARTESIAN_POINT ( 'NONE',  ( 36.48921356237310221, -27.52281430457080802, 5.000000000000000000 ) ) ;
#121627 = LINE ( 'NONE', #23012, #132585 ) ;
#121628 = ORIENTED_EDGE ( 'NONE', *, *, #98340, .T. ) ;
#121629 = VECTOR ( 'NONE', #80843, 1000.000000000000227 ) ;
#121630 = ORIENTED_EDGE ( 'NONE', *, *, #131088, .T. ) ;
#121631 = ORIENTED_EDGE ( 'NONE', *, *, #110862, .F. ) ;
#121632 = CARTESIAN_POINT ( 'NONE',  ( 91.72959685856477563, -6.110000000000000320, -1.637169565754161393 ) ) ;
#121633 = EDGE_LOOP ( 'NONE', ( #75622, #8806, #114297, #26215 ) ) ;
#121634 = VECTOR ( 'NONE', #88155, 1000.000000000000000 ) ;
#121635 = DIRECTION ( 'NONE',  ( 0.7071067811865486830, -0.7071067811865464625, -0.000000000000000000 ) ) ;
#121636 = CARTESIAN_POINT ( 'NONE',  ( -27.48921356237309155, -27.52281430457074762, 5.000000000000000000 ) ) ;
#121637 = DIRECTION ( 'NONE',  ( 0.6830127018922180770, -0.6830127018922204085, -0.2588190451025213501 ) ) ;
#121638 = DIRECTION ( 'NONE',  ( -0.7071067811865486830, 0.7071067811865463515, 0.000000000000000000 ) ) ;
#121639 = EDGE_LOOP ( 'NONE', ( #8286, #103922, #55425, #3597 ) ) ;
#121640 = CARTESIAN_POINT ( 'NONE',  ( -16.40128505106373780, 22.22500000000000142, 12.01932804697904800 ) ) ;
#121642 = EDGE_CURVE ( 'NONE', #136740, #98772, #81571, .T. ) ;
#121641 = CARTESIAN_POINT ( 'NONE',  ( 48.25000000000000000, -9.735942053221458872E-16, 7.950000000000000178 ) ) ;
#121643 = CARTESIAN_POINT ( 'NONE',  ( 81.57876352523143737, -7.482591942790325086E-16, 6.109999999999998543 ) ) ;
#121644 = EDGE_CURVE ( 'NONE', #15282, #32517, #114847, .T. ) ;
#121645 = AXIS2_PLACEMENT_3D ( 'NONE', #75968, #9986, #87558 ) ;
#121646 = EDGE_LOOP ( 'NONE', ( #95864, #67580, #41814, #130464 ) ) ;
#121647 = DIRECTION ( 'NONE',  ( -1.000000000000000000, -0.000000000000000000, -0.000000000000000000 ) ) ;
#121648 = DIRECTION ( 'NONE',  ( 0.000000000000000000, -1.000000000000000000, 0.000000000000000000 ) ) ;
#121649 = EDGE_LOOP ( 'NONE', ( #51136, #116200, #34865, #27749 ) ) ;
#121650 = ORIENTED_EDGE ( 'NONE', *, *, #81954, .T. ) ;
#121651 = ORIENTED_EDGE ( 'NONE', *, *, #56782, .T. ) ;
#121652 = FACE_OUTER_BOUND ( 'NONE', #3743, .T. ) ;
#121653 = EDGE_CURVE ( 'NONE', #35333, #107292, #98136, .T. ) ;
#121654 = DIRECTION ( 'NONE',  ( 0.7071067811865486830, -0.7071067811865464625, -0.000000000000000000 ) ) ;
#121655 = CARTESIAN_POINT ( 'NONE',  ( 22.82816939922337340, -8.240707523384203981, 4.000000000000000000 ) ) ;
#121656 = DIRECTION ( 'NONE',  ( 0.6830127018922180770, -0.6830127018922204085, -0.2588190451025213501 ) ) ;
#121657 = VECTOR ( 'NONE', #125398, 1000.000000000000227 ) ;
#121658 = CARTESIAN_POINT ( 'NONE',  ( 14.99451991528749595, 28.92564299267948513, 4.000000000000000000 ) ) ;
#121659 = FACE_OUTER_BOUND ( 'NONE', #87251, .T. ) ;
#121660 =( LENGTH_UNIT ( ) NAMED_UNIT ( * ) SI_UNIT ( .MILLI., .METRE. ) );
#121661 = VECTOR ( 'NONE', #63017, 999.9999999999998863 ) ;
#121662 = VERTEX_POINT ( 'NONE', #106845 ) ;
#121664 = ORIENTED_EDGE ( 'NONE', *, *, #140890, .F. ) ;
#121663 = VECTOR ( 'NONE', #57399, 999.9999999999998863 ) ;
#121665 = LINE ( 'NONE', #22335, #94239 ) ;
#121666 = VERTEX_POINT ( 'NONE', #85102 ) ;
#121667 = ORIENTED_EDGE ( 'NONE', *, *, #79391, .F. ) ;
#121668 = FACE_OUTER_BOUND ( 'NONE', #32347, .T. ) ;
#121669 = EDGE_LOOP ( 'NONE', ( #142034, #14989, #102450, #5383 ) ) ;
#121670 = CARTESIAN_POINT ( 'NONE',  ( -33.48921356237309510, -27.52281430457078670, 5.000000000000000000 ) ) ;
#121671 = DIRECTION ( 'NONE',  ( -0.000000000000000000, 0.3543493200069153248, 0.9351131265310292928 ) ) ;
#121672 = CARTESIAN_POINT ( 'NONE',  ( 15.29974487139158867, -27.71228299555216879, 4.000000000000000000 ) ) ;
#121673 = LINE ( 'NONE', #54336, #136342 ) ;
#121674 = FACE_OUTER_BOUND ( 'NONE', #10330, .T. ) ;
#121675 = ORIENTED_EDGE ( 'NONE', *, *, #91513, .F. ) ;
#121676 = CYLINDRICAL_SURFACE ( 'NONE', #111274, 6.094999999999989093 ) ;
#121677 = VERTEX_POINT ( 'NONE', #97379 ) ;
#121678 = CARTESIAN_POINT ( 'NONE',  ( 32.99451991528749062, 28.92564299267960948, 4.000000000000000000 ) ) ;
#121679 = ORIENTED_EDGE ( 'NONE', *, *, #115738, .T. ) ;
#121680 = CARTESIAN_POINT ( 'NONE',  ( -34.92500000000001137, 15.85612307739227944, 4.000000000000000000 ) ) ;
#121682 = ORIENTED_EDGE ( 'NONE', *, *, #135795, .T. ) ;
#121681 = ADVANCED_FACE ( 'NONE', ( #75671 ), #30751, .F. ) ;
#121683 = APPLICATION_CONTEXT ( 'automotive_design' ) ;
#121684 = DIRECTION ( 'NONE',  ( 0.7071067811865486830, -0.7071067811865464625, -0.000000000000000000 ) ) ;
#121685 = ORIENTED_EDGE ( 'NONE', *, *, #63146, .T. ) ;
#121686 = ORIENTED_EDGE ( 'NONE', *, *, #95006, .F. ) ;
#121687 = ORIENTED_EDGE ( 'NONE', *, *, #11058, .F. ) ;
#121688 = EDGE_CURVE ( 'NONE', #89682, #41509, #64796, .T. ) ;
#121689 = EDGE_CURVE ( 'NONE', #77053, #13854, #118434, .T. ) ;
#121690 = LINE ( 'NONE', #45616, #141454 ) ;
#121692 = EDGE_CURVE ( 'NONE', #113754, #88854, #142361, .T. ) ;
#121691 = DIRECTION ( 'NONE',  ( -0.7071067811865486830, 0.7071067811865464625, 0.000000000000000000 ) ) ;
#121693 =( LENGTH_UNIT ( ) NAMED_UNIT ( * ) SI_UNIT ( .MILLI., .METRE. ) );
#121694 = DIRECTION ( 'NONE',  ( -0.000000000000000000, 0.000000000000000000, 1.000000000000000000 ) ) ;
#121695 = EDGE_CURVE ( 'NONE', #373, #42048, #17680, .T. ) ;
#121696 = CARTESIAN_POINT ( 'NONE',  ( 11.35681257248254106, -20.24070752338407431, 21.22881796311215652 ) ) ;
#121697 = DIRECTION ( 'NONE',  ( -1.369518533665900312E-16, 1.000000000000000000, -0.000000000000000000 ) ) ;
#121698 = EDGE_CURVE ( 'NONE', #109084, #81908, #41594, .T. ) ;
#121699 = CARTESIAN_POINT ( 'NONE',  ( 34.57058949319513630, 22.20469455417148907, 4.123089426795141677 ) ) ;
#121700 = DIRECTION ( 'NONE',  ( 0.7071067811865487940, 0.7071067811865463515, -0.000000000000000000 ) ) ;
#121701 = EDGE_CURVE ( 'NONE', #98903, #112793, #43051, .T. ) ;
#121702 = VERTEX_POINT ( 'NONE', #87254 ) ;
#121703 = LINE ( 'NONE', #20969, #94536 ) ;
#121704 = DIRECTION ( 'NONE',  ( 0.7071067811865487940, 0.7071067811865463515, 0.000000000000000000 ) ) ;
#121705 = ORIENTED_EDGE ( 'NONE', *, *, #30439, .T. ) ;
#121706 = ORIENTED_EDGE ( 'NONE', *, *, #70559, .T. ) ;
#121707 = VERTEX_POINT ( 'NONE', #130050 ) ;
#121708 = DIRECTION ( 'NONE',  ( -0.7071067811865486830, -0.7071067811865464625, 0.000000000000000000 ) ) ;
#121709 = VERTEX_POINT ( 'NONE', #51062 ) ;
#121710 = VERTEX_POINT ( 'NONE', #19835 ) ;
#121711 = CARTESIAN_POINT ( 'NONE',  ( 30.32816939922331656, 14.25929247661557042, 4.000000000000000000 ) ) ;
#121712 = CARTESIAN_POINT ( 'NONE',  ( -30.48921356237309510, -27.52281430457076894, 5.000000000000000000 ) ) ;
#121714 = EDGE_CURVE ( 'NONE', #109897, #5522, #28603, .T. ) ;
#121713 = LINE ( 'NONE', #91953, #117331 ) ;
#121715 = ADVANCED_FACE ( 'NONE', ( #64076 ), #72858, .F. ) ;
#121716 = CARTESIAN_POINT ( 'NONE',  ( -12.70000000000000284, -40.29840020119761590, 19.55137198191482995 ) ) ;
#121717 = CARTESIAN_POINT ( 'NONE',  ( -4.499999999999970690, 0.4311230773921797543, 4.000000000000000000 ) ) ;
#121718 = ORIENTED_EDGE ( 'NONE', *, *, #13209, .F. ) ;
#121719 = FACE_OUTER_BOUND ( 'NONE', #109173, .T. ) ;
#121720 = ORIENTED_EDGE ( 'NONE', *, *, #36890, .F. ) ;
#121722 = EDGE_CURVE ( 'NONE', #81702, #46533, #40862, .T. ) ;
#121721 =( BOUNDED_CURVE ( )  B_SPLINE_CURVE ( 2, ( #4736, #49039, #93235, #104823, #137469, #25105, #102700, #38162, #17110, #93944, #138178, #83083, #129423 ),
 .UNSPECIFIED., .F., .T. ) 
 B_SPLINE_CURVE_WITH_KNOTS ( ( 3, 2, 2, 2, 2, 2, 3 ),
 ( 0.3166666666666666519, 0.3194444444444444198, 0.3222222222222222432, 0.3250000000000000111, 0.3277777777777777790, 0.3305555555555555469, 0.3333333333333333148 ),
 .UNSPECIFIED. ) 
 CURVE ( )  GEOMETRIC_REPRESENTATION_ITEM ( )  RATIONAL_B_SPLINE_CURVE ( ( 1.000000000000000000, 0.9659258262890683122, 1.000000000000000000, 0.9659258262890683122, 1.000000000000000000, 0.9659258262890683122, 1.000000000000000000, 0.9659258262890683122, 1.000000000000000000, 0.9659258262890683122, 1.000000000000000000, 0.9659258262890683122, 1.000000000000000000 ) ) 
 REPRESENTATION_ITEM ( '' )  );
#121723 = SURFACE_STYLE_FILL_AREA ( #55798 ) ;
#121724 = AXIS2_PLACEMENT_3D ( 'NONE', #59469, #50006, #81947 ) ;
#121725 = CARTESIAN_POINT ( 'NONE',  ( 16.69206980810189123, -7.934999999999991616, -2.126176841940955242 ) ) ;
#121726 = ORIENTED_EDGE ( 'NONE', *, *, #22857, .T. ) ;
#121727 = CARTESIAN_POINT ( 'NONE',  ( 80.55793019189812298, 6.110000000000001208, -1.637169565754156286 ) ) ;
#121728 = CARTESIAN_POINT ( 'NONE',  ( 7.038781720212028858, -9.048404391359483157, 2.901793228214030851 ) ) ;
#121729 = FACE_OUTER_BOUND ( 'NONE', #2890, .T. ) ;
#121730 = ORIENTED_EDGE ( 'NONE', *, *, #75768, .F. ) ;
#121731 = ORIENTED_EDGE ( 'NONE', *, *, #8245, .T. ) ;
#121732 = VERTEX_POINT ( 'NONE', #106109 ) ;
#121733 = FACE_OUTER_BOUND ( 'NONE', #91166, .T. ) ;
#121734 = CARTESIAN_POINT ( 'NONE',  ( 34.78752705046288440, 0.000000000000000000, -7.949999999999998401 ) ) ;
#121735 = DIRECTION ( 'NONE',  ( 0.7071067811865487940, 0.7071067811865463515, -0.000000000000000000 ) ) ;
#121736 = CARTESIAN_POINT ( 'NONE',  ( 16.64450715494396604, 0.4096876026223312262, -33.72258372513044122 ) ) ;
#121737 = LINE ( 'NONE', #23119, #45058 ) ;
#121738 = DIRECTION ( 'NONE',  ( 0.7071067811865486830, -0.7071067811865464625, -0.000000000000000000 ) ) ;
#121739 = EDGE_LOOP ( 'NONE', ( #53471, #10479, #19266, #24407 ) ) ;
#121740 = LINE ( 'NONE', #57254, #122107 ) ;
#121741 = VECTOR ( 'NONE', #90973, 999.9999999999998863 ) ;
#121742 = CARTESIAN_POINT ( 'NONE',  ( -34.92500000000001137, -22.22500000000000142, 4.000000000000000000 ) ) ;
#121743 = DIRECTION ( 'NONE',  ( -0.7071067811865486830, -0.7071067811865464625, 0.000000000000000000 ) ) ;
#121744 = EDGE_CURVE ( 'NONE', #56146, #104888, #87272, .T. ) ;
#121745 = VERTEX_POINT ( 'NONE', #40212 ) ;
#121746 = CARTESIAN_POINT ( 'NONE',  ( 15.18079593298623564, 2.055000000000001048, 2.516649172247811554E-16 ) ) ;
#121747 = DIRECTION ( 'NONE',  ( 0.6830127018922180770, -0.6830127018922204085, -0.2588190451025213501 ) ) ;
#121748 = ORIENTED_EDGE ( 'NONE', *, *, #26823, .F. ) ;
#121750 = ORIENTED_EDGE ( 'NONE', *, *, #6383, .T. ) ;
#121749 = LINE ( 'NONE', #31207, #90286 ) ;
#121751 = ORIENTED_EDGE ( 'NONE', *, *, #112688, .F. ) ;
#121752 = CARTESIAN_POINT ( 'NONE',  ( -9.489213562373095101, -27.52281430457062328, 5.000000000000000000 ) ) ;
#121753 = CARTESIAN_POINT ( 'NONE',  ( 0.7071067811865450192, 5.259292476615662792, 5.000000000000000000 ) ) ;
#121754 = VERTEX_POINT ( 'NONE', #130785 ) ;
#121755 = CARTESIAN_POINT ( 'NONE',  ( -34.92500000000001137, 8.718490437204135191, 4.759050581649341360 ) ) ;
#121756 = UNCERTAINTY_MEASURE_WITH_UNIT (LENGTH_MEASURE( 1.000000000000000082E-05 ), #136385, 'distance_accuracy_value', 'NONE');
#121757 = EDGE_CURVE ( 'NONE', #59558, #31597, #140209, .T. ) ;
#121758 = AXIS2_PLACEMENT_3D ( 'NONE', #82433, #32336, #95431 ) ;
#121759 = FACE_OUTER_BOUND ( 'NONE', #121447, .T. ) ;
#121760 = VECTOR ( 'NONE', #27857, 1000.000000000000227 ) ;
#121761 = DIRECTION ( 'NONE',  ( 0.7071067811865487940, -0.7071067811865463515, 0.000000000000000000 ) ) ;
#121762 = DIRECTION ( 'NONE',  ( 0.7071067811865486830, -0.7071067811865464625, -0.000000000000000000 ) ) ;
#121764 = AXIS2_PLACEMENT_3D ( 'NONE', #118224, #104509, #61753 ) ;
#121763 = CYLINDRICAL_SURFACE ( 'NONE', #11866, 0.5000000000000000000 ) ;
#121765 = EDGE_CURVE ( 'NONE', #60839, #43089, #52465, .T. ) ;
#121766 = FACE_OUTER_BOUND ( 'NONE', #40223, .T. ) ;
#121767 = DIRECTION ( 'NONE',  ( 0.3543493200069162685, -0.000000000000000000, -0.9351131265310288487 ) ) ;
#121768 = CARTESIAN_POINT ( 'NONE',  ( -78.48921356237309510, -27.52281430457109934, 5.000000000000000000 ) ) ;
#121769 = CARTESIAN_POINT ( 'NONE',  ( 21.27040314143522437, -7.934999999999989839, 2.126176841940957907 ) ) ;
#121770 = DIRECTION ( 'NONE',  ( -0.7071067811865486830, 0.7071067811865464625, 0.000000000000000000 ) ) ;
#121771 = CARTESIAN_POINT ( 'NONE',  ( 35.14818355038124054, 17.25929247661554200, 8.802941693769282594 ) ) ;
#121772 = STYLED_ITEM ( 'NONE', ( #30515 ), #133817 ) ;
#121773 = CARTESIAN_POINT ( 'NONE',  ( 110.5208333333333286, 7.949999999999998401, 2.130196079827431532 ) ) ;
#121774 = LINE ( 'NONE', #22450, #91678 ) ;
#121775 = ORIENTED_EDGE ( 'NONE', *, *, #80106, .F. ) ;
#121776 = ORIENTED_EDGE ( 'NONE', *, *, #97143, .F. ) ;
#121777 = CARTESIAN_POINT ( 'NONE',  ( 102.9375000000000000, 5.819803920172573974, -5.819803920172572198 ) ) ;
#121778 = VERTEX_POINT ( 'NONE', #108242 ) ;
#121779 = ORIENTED_EDGE ( 'NONE', *, *, #56043, .T. ) ;
#121780 = EDGE_CURVE ( 'NONE', #43690, #134514, #8910, .T. ) ;
#121781 = ORIENTED_EDGE ( 'NONE', *, *, #65201, .T. ) ;
#121782 = DIRECTION ( 'NONE',  ( -1.000000000000000000, -1.224606353822377258E-16, -0.000000000000000000 ) ) ;
#121783 = CARTESIAN_POINT ( 'NONE',  ( 0.000000000000000000, 0.000000000000000000, 5.000000000000000000 ) ) ;
#121784 = ORIENTED_EDGE ( 'NONE', *, *, #67446, .F. ) ;
#121785 = CARTESIAN_POINT ( 'NONE',  ( 8.700255128608413102, -27.71228299555199825, 4.000000000000000000 ) ) ;
#121786 = CARTESIAN_POINT ( 'NONE',  ( 24.18398860626899705, 28.73617430169804265, 5.000000000000000000 ) ) ;
#121787 = CARTESIAN_POINT ( 'NONE',  ( 0.000000000000000000, 0.000000000000000000, 5.000000000000000000 ) ) ;
#121788 = LINE ( 'NONE', #43539, #102183 ) ;
#121789 = EDGE_CURVE ( 'NONE', #98685, #113921, #32904, .T. ) ;
#121790 = ORIENTED_EDGE ( 'NONE', *, *, #47766, .F. ) ;
#121791 = DIRECTION ( 'NONE',  ( -0.000000000000000000, 0.000000000000000000, 1.000000000000000000 ) ) ;
#121792 = FACE_OUTER_BOUND ( 'NONE', #17357, .T. ) ;
#121793 = CARTESIAN_POINT ( 'NONE',  ( 4.526428939989314948, -22.22500000000000142, -9.949621197219423507 ) ) ;
#121794 = CARTESIAN_POINT ( 'NONE',  ( -17.29289321881333308, 14.25929247661557042, 5.000000000000000000 ) ) ;
#121795 = DIRECTION ( 'NONE',  ( -0.7071067811865487940, 0.7071067811865463515, -0.000000000000000000 ) ) ;
#121796 = CARTESIAN_POINT ( 'NONE',  ( 87.28752705046288440, 0.000000000000000000, -7.949999999999998401 ) ) ;
#121797 = CARTESIAN_POINT ( 'NONE',  ( 61.46640106136307935, -43.14999999999999147, 34.92499999999998295 ) ) ;
#121798 = EDGE_CURVE ( 'NONE', #141085, #19388, #99527, .T. ) ;
#121799 = VERTEX_POINT ( 'NONE', #57501 ) ;
#121800 = EDGE_LOOP ( 'NONE', ( #19579, #132921, #142447, #139542 ) ) ;
#121801 = CARTESIAN_POINT ( 'NONE',  ( 120.7504301918981184, 3.055000000000002824, -5.291415217122919401 ) ) ;
#121802 = ORIENTED_EDGE ( 'NONE', *, *, #80787, .T. ) ;
#121803 = EDGE_CURVE ( 'NONE', #92723, #61905, #17650, .T. ) ;
#121804 = CARTESIAN_POINT ( 'NONE',  ( 42.48921356237308800, -27.52281430457085065, 5.000000000000000000 ) ) ;
#121805 = VECTOR ( 'NONE', #80995, 1000.000000000000000 ) ;
#121806 = DIRECTION ( 'NONE',  ( 0.000000000000000000, -1.000000000000000000, 0.000000000000000000 ) ) ;
#121807 = CARTESIAN_POINT ( 'NONE',  ( -69.48921356237309510, -27.52281430457103895, 5.000000000000000000 ) ) ;
#121809 = ADVANCED_FACE ( 'NONE', ( #66229 ), #13232, .F. ) ;
#121808 = DIRECTION ( 'NONE',  ( -0.000000000000000000, -1.000000000000000000, -0.000000000000000000 ) ) ;
#121810 = CARTESIAN_POINT ( 'NONE',  ( 117.3079301918980946, -6.109999999999998543, 1.637169565754158063 ) ) ;
#121811 = EDGE_CURVE ( 'NONE', #32452, #61250, #121996, .T. ) ;
#121812 = ORIENTED_EDGE ( 'NONE', *, *, #7277, .F. ) ;
#121813 = VERTEX_POINT ( 'NONE', #44499 ) ;
#121814 = AXIS2_PLACEMENT_3D ( 'NONE', #103924, #40168, #95213 ) ;
#121815 = PLANE ( 'NONE',  #67070 ) ;
#121816 = CARTESIAN_POINT ( 'NONE',  ( 97.54166666666667140, -3.975000000000002753, 6.884901960086286188 ) ) ;
#121817 = EDGE_LOOP ( 'NONE', ( #84743, #133994, #121284, #92130, #122341 ) ) ;
#121818 = ORIENTED_EDGE ( 'NONE', *, *, #56937, .F. ) ;
#121819 = CARTESIAN_POINT ( 'NONE',  ( 37.47959685856476852, 6.109999999999999432, 1.637169565754164280 ) ) ;
#121820 = ORIENTED_EDGE ( 'NONE', *, *, #137058, .T. ) ;
#121821 = DIRECTION ( 'NONE',  ( 0.7071067811865487940, -0.7071067811865463515, 0.000000000000000000 ) ) ;
#121822 = ADVANCED_FACE ( 'NONE', ( #11079, #2347 ), #123485, .T. ) ;
#121823 = CARTESIAN_POINT ( 'NONE',  ( -5.816011393731002066, 28.73617430169783304, 5.000000000000000000 ) ) ;
#121824 = CARTESIAN_POINT ( 'NONE',  ( -48.48921356237309510, -27.52281430457089328, 5.000000000000000000 ) ) ;
#121825 = CARTESIAN_POINT ( 'NONE',  ( 26.45376352523144803, -6.109999999999998543, -3.741295971395162543E-16 ) ) ;
#121826 = ORIENTED_EDGE ( 'NONE', *, *, #103222, .F. ) ;
#121827 = VECTOR ( 'NONE', #58625, 1000.000000000000227 ) ;
#121828 = DIRECTION ( 'NONE',  ( -0.6830127018922180770, -0.6830127018922204085, -0.2588190451025213501 ) ) ;
#121829 = ORIENTED_EDGE ( 'NONE', *, *, #109684, .T. ) ;
#121830 = ORIENTED_EDGE ( 'NONE', *, *, #135199, .F. ) ;
#121831 = ORIENTED_EDGE ( 'NONE', *, *, #76577, .T. ) ;
#121832 =( NAMED_UNIT ( * ) PLANE_ANGLE_UNIT ( ) SI_UNIT ( $, .RADIAN. ) );
#121833 = LINE ( 'NONE', #78368, #136767 ) ;
#121834 = ORIENTED_EDGE ( 'NONE', *, *, #110283, .T. ) ;
#121835 = DIRECTION ( 'NONE',  ( 0.6830127018922180770, -0.6830127018922204085, -0.2588190451025213501 ) ) ;
#121836 =( GEOMETRIC_REPRESENTATION_CONTEXT ( 3 ) GLOBAL_UNCERTAINTY_ASSIGNED_CONTEXT ( ( #50640 ) ) GLOBAL_UNIT_ASSIGNED_CONTEXT ( ( #38963, #50550, #62883 ) ) REPRESENTATION_CONTEXT ( 'NONE', 'WORKASPACE' ) );
#121837 = DIRECTION ( 'NONE',  ( -0.000000000000000000, 0.3543493200069153248, 0.9351131265310292928 ) ) ;
#121838 = CARTESIAN_POINT ( 'NONE',  ( 0.000000000000000000, 0.000000000000000000, 5.000000000000000000 ) ) ;
#121839 = LINE ( 'NONE', #22521, #34980 ) ;
#121841 = FACE_BOUND ( 'NONE', #12350, .T. ) ;
#121840 = AXIS2_PLACEMENT_3D ( 'NONE', #572, #44870, #89054 ) ;
#121842 = EDGE_LOOP ( 'NONE', ( #62510, #138893, #46739, #53191 ) ) ;
#121843 = LINE ( 'NONE', #41, #131376 ) ;
#121844 = CARTESIAN_POINT ( 'NONE',  ( 9.183988606268997046, 28.73617430169793607, 5.000000000000000000 ) ) ;
#121845 = CARTESIAN_POINT ( 'NONE',  ( 34.92499999999998295, -11.24070752338416490, 4.255531930566169407 ) ) ;
#121846 = ORIENTED_EDGE ( 'NONE', *, *, #94563, .F. ) ;
#121847 = CARTESIAN_POINT ( 'NONE',  ( 24.69163961620376924, 6.094999999999988205, -1.633150327867694651 ) ) ;
#121848 = ORIENTED_EDGE ( 'NONE', *, *, #26127, .T. ) ;
#121849 = VERTEX_POINT ( 'NONE', #76389 ) ;
#121850 = FILL_AREA_STYLE ('',( #10940 ) ) ;
#121851 = VECTOR ( 'NONE', #119843, 1000.000000000000000 ) ;
#121852 = ORIENTED_EDGE ( 'NONE', *, *, #93396, .T. ) ;
#121853 = VECTOR ( 'NONE', #8233, 1000.000000000000000 ) ;
#121855 = ADVANCED_FACE ( 'NONE', ( #43747 ), #23405, .F. ) ;
#121854 = VECTOR ( 'NONE', #122275, 1000.000000000000000 ) ;
#121856 = CARTESIAN_POINT ( 'NONE',  ( 50.37043019189811588, -3.055000000000001492, 5.291415217122917625 ) ) ;
#121857 = VERTEX_POINT ( 'NONE', #24141 ) ;
#121858 = DIRECTION ( 'NONE',  ( 0.7071067811865486830, -0.7071067811865464625, -0.000000000000000000 ) ) ;
#121859 = ADVANCED_FACE ( 'NONE', ( #65540 ), #100276, .F. ) ;
#121860 = SURFACE_SIDE_STYLE ('',( #54515 ) ) ;
#121861 = CARTESIAN_POINT ( 'NONE',  ( 25.49999999999982947, 0.4497235411627699131, -5.599840258123482073 ) ) ;
#121862 = VERTEX_POINT ( 'NONE', #45215 ) ;
#121863 = EDGE_CURVE ( 'NONE', #5696, #117806, #111869, .T. ) ;
#121864 = CARTESIAN_POINT ( 'NONE',  ( 0.5240013858544890768, 22.03583458319437938, 4.979811245910086726 ) ) ;
#121865 = PLANE ( 'NONE',  #80537 ) ;
#121866 = CONICAL_SURFACE ( 'NONE', #119585, 2.500000000000000444, 0.9599310885968830309 ) ;
#121867 = ADVANCED_FACE ( 'NONE', ( #67682 ), #12532, .F. ) ;
#121868 = DIRECTION ( 'NONE',  ( -0.7071067811865486830, -0.7071067811865464625, -0.000000000000000000 ) ) ;
#121869 = DIRECTION ( 'NONE',  ( -0.7071067811865486830, -0.7071067811865464625, 0.000000000000000000 ) ) ;
#121870 = DIRECTION ( 'NONE',  ( 0.6830127018922180770, -0.6830127018922204085, -0.2588190451025213501 ) ) ;
#121871 = DIRECTION ( 'NONE',  ( -0.7071067811865486830, -0.7071067811865464625, 0.000000000000000000 ) ) ;
#121872 = DIRECTION ( 'NONE',  ( -0.6830127018922181881, 0.6830127018922202975, -0.2588190451025214056 ) ) ;
#121873 = VERTEX_POINT ( 'NONE', #82128 ) ;
#121874 = EDGE_LOOP ( 'NONE', ( #21868, #78006, #2656, #117226 ) ) ;
#121875 = EDGE_LOOP ( 'NONE', ( #36997, #4272, #33254, #3397 ) ) ;
#121876 = DIRECTION ( 'NONE',  ( -0.7071067811865487940, 0.7071067811865463515, 0.000000000000000000 ) ) ;
#121877 = LINE ( 'NONE', #21871, #109210 ) ;
#121878 = ORIENTED_EDGE ( 'NONE', *, *, #127434, .T. ) ;
#121879 = VERTEX_POINT ( 'NONE', #37155 ) ;
#121880 = SURFACE_STYLE_FILL_AREA ( #101567 ) ;
#121882 = EDGE_CURVE ( 'NONE', #83429, #54589, #60364, .T. ) ;
#121881 = PLANE ( 'NONE',  #138268 ) ;
#121883 = EDGE_CURVE ( 'NONE', #142433, #67739, #25552, .T. ) ;
#121884 = LINE ( 'NONE', #142946, #13895 ) ;
#121885 = EDGE_LOOP ( 'NONE', ( #82754, #94552, #12242, #122399 ) ) ;
#121886 = CARTESIAN_POINT ( 'NONE',  ( 29.67183060077626067, -6.740707523384216415, 4.000000000000000000 ) ) ;
#121887 = EDGE_CURVE ( 'NONE', #32567, #56766, #124162, .T. ) ;
#121888 = DIRECTION ( 'NONE',  ( -0.7071067811865487940, 0.7071067811865463515, 0.000000000000000000 ) ) ;
#121889 = CARTESIAN_POINT ( 'NONE',  ( 31.42123647476855552, -9.717572351234235426E-16, -7.934999999999990727 ) ) ;
#121890 = VECTOR ( 'NONE', #114423, 1000.000000000000000 ) ;
#121891 = CARTESIAN_POINT ( 'NONE',  ( -15.00548008471250228, 28.92564299267927552, 4.000000000000000000 ) ) ;
#121892 = ORIENTED_EDGE ( 'NONE', *, *, #114002, .T. ) ;
#121893 = CARTESIAN_POINT ( 'NONE',  ( 115.4120968585647944, 5.291415217122922066, -3.054999999999995275 ) ) ;
#121894 = DIRECTION ( 'NONE',  ( -0.000000000000000000, 1.000000000000000000, -0.000000000000000000 ) ) ;
#121895 = CARTESIAN_POINT ( 'NONE',  ( -26.99451991528749417, 28.92564299267956685, 4.000000000000000000 ) ) ;
#121896 = EDGE_CURVE ( 'NONE', #121495, #108472, #124877, .T. ) ;
#121898 = VERTEX_POINT ( 'NONE', #59648 ) ;
#121897 = PLANE ( 'NONE',  #93514 ) ;
#121899 = AXIS2_PLACEMENT_3D ( 'NONE', #55887, #101495, #737 ) ;
#121900 = CARTESIAN_POINT ( 'NONE',  ( 27.18398860626900060, 28.73617430169806042, 5.000000000000000000 ) ) ;
#121901 = VERTEX_POINT ( 'NONE', #3765 ) ;
#121902 = PLANE ( 'NONE',  #14976 ) ;
#121903 = DIRECTION ( 'NONE',  ( -0.000000000000000000, 0.3543493200069153248, 0.9351131265310292928 ) ) ;
#121904 = CARTESIAN_POINT ( 'NONE',  ( 184.1500000000000057, -49.85820393249935023, -34.92499999999998295 ) ) ;
#121905 = DIRECTION ( 'NONE',  ( 1.000000000000000000, 0.000000000000000000, 0.000000000000000000 ) ) ;
#121906 = ORIENTED_EDGE ( 'NONE', *, *, #59400, .F. ) ;
#121907 = DIRECTION ( 'NONE',  ( -0.000000000000000000, 0.3543493200069153248, 0.9351131265310292928 ) ) ;
#121908 = PLANE ( 'NONE',  #116229 ) ;
#121909 = EDGE_CURVE ( 'NONE', #114745, #30259, #5211, .T. ) ;
#121910 = VECTOR ( 'NONE', #87039, 1000.000000000000000 ) ;
#121911 = ORIENTED_EDGE ( 'NONE', *, *, #10607, .F. ) ;
#121912 = DIRECTION ( 'NONE',  ( -0.3543493200069162685, -0.000000000000000000, -0.9351131265310288487 ) ) ;
#121913 = FACE_OUTER_BOUND ( 'NONE', #25171, .T. ) ;
#121914 = ORIENTED_EDGE ( 'NONE', *, *, #97854, .T. ) ;
#121915 = DIRECTION ( 'NONE',  ( 0.7071067811865487940, -0.7071067811865463515, 0.000000000000000000 ) ) ;
#121916 = VECTOR ( 'NONE', #139193, 1000.000000000000227 ) ;
#121918 = ORIENTED_EDGE ( 'NONE', *, *, #134703, .T. ) ;
#121917 = CARTESIAN_POINT ( 'NONE',  ( 25.97159235450331849, 9.902892378096218942E-16, 0.000000000000000000 ) ) ;
#121919 = EDGE_LOOP ( 'NONE', ( #50024, #29013, #114629, #122733 ) ) ;
#121920 = PLANE ( 'NONE',  #142191 ) ;
#121921 = PLANE ( 'NONE',  #133892 ) ;
#121922 = ORIENTED_EDGE ( 'NONE', *, *, #85117, .T. ) ;
#121923 = ADVANCED_FACE ( 'NONE', ( #69824 ), #126302, .F. ) ;
#121924 = CIRCLE ( 'NONE', #87291, 5.999999999999998224 ) ;
#121925 = DIRECTION ( 'NONE',  ( -1.000000000000000000, -1.369518533665900312E-16, 0.000000000000000000 ) ) ;
#121926 = DIRECTION ( 'NONE',  ( 0.000000000000000000, -1.000000000000000000, 0.000000000000000000 ) ) ;
#121927 = CARTESIAN_POINT ( 'NONE',  ( -12.29974487139158512, -27.71228299555214747, 4.000000000000000000 ) ) ;
#121928 = VECTOR ( 'NONE', #107592, 1000.000000000000227 ) ;
#121929 = VERTEX_POINT ( 'NONE', #82821 ) ;
#121930 = DIRECTION ( 'NONE',  ( -1.000000000000000000, -0.000000000000000000, -0.000000000000000000 ) ) ;
#121931 = EDGE_CURVE ( 'NONE', #140411, #72185, #58972, .T. ) ;
#121933 = AXIS2_PLACEMENT_3D ( 'NONE', #129274, #82941, #94503 ) ;
#121932 = CARTESIAN_POINT ( 'NONE',  ( -20.81601139373100295, 28.73617430169773002, 5.000000000000000000 ) ) ;
#121934 = DIRECTION ( 'NONE',  ( 0.5735764363510444941, 0.8191520442889929088, 0.000000000000000000 ) ) ;
#121935 = LINE ( 'NONE', #66876, #138603 ) ;
#121936 = CARTESIAN_POINT ( 'NONE',  ( 26.45376352523144803, -6.109999999999999432, -3.741295971395163529E-16 ) ) ;
#121937 = DIRECTION ( 'NONE',  ( 0.7071067811865487940, -0.7071067811865463515, 0.000000000000000000 ) ) ;
#121938 = ORIENTED_EDGE ( 'NONE', *, *, #92964, .F. ) ;
#121939 = ORIENTED_EDGE ( 'NONE', *, *, #43223, .T. ) ;
#121940 = CARTESIAN_POINT ( 'NONE',  ( 125.1041666666666714, 2.130196079827422206, 7.950000000000001954 ) ) ;
#121941 = VERTEX_POINT ( 'NONE', #47378 ) ;
#121942 = VECTOR ( 'NONE', #27912, 1000.000000000000000 ) ;
#121943 = EDGE_CURVE ( 'NONE', #36373, #9222, #103125, .T. ) ;
#121944 = ORIENTED_EDGE ( 'NONE', *, *, #60946, .F. ) ;
#121945 = DIRECTION ( 'NONE',  ( -0.7071067811865486830, -0.7071067811865464625, 0.000000000000000000 ) ) ;
#121946 = DIRECTION ( 'NONE',  ( -0.000000000000000000, 0.3543493200069153248, 0.9351131265310292928 ) ) ;
#121947 = ORIENTED_EDGE ( 'NONE', *, *, #29455, .T. ) ;
#121948 = DIRECTION ( 'NONE',  ( -0.6830127018922180770, -0.6830127018922204085, -0.2588190451025213501 ) ) ;
#121949 = CARTESIAN_POINT ( 'NONE',  ( 25.39999999999999858, 3.495127910064749877, 5.104374744108353568 ) ) ;
#121950 = PLANE ( 'NONE',  #20899 ) ;
#121951 =( GEOMETRIC_REPRESENTATION_CONTEXT ( 3 ) GLOBAL_UNCERTAINTY_ASSIGNED_CONTEXT ( ( #12664 ) ) GLOBAL_UNIT_ASSIGNED_CONTEXT ( ( #120019, #132408, #65731 ) ) REPRESENTATION_CONTEXT ( 'NONE', 'WORKASPACE' ) );
#121952 = DIRECTION ( 'NONE',  ( 0.000000000000000000, -1.000000000000000000, 0.000000000000000000 ) ) ;
#121953 = CARTESIAN_POINT ( 'NONE',  ( 124.9795968585647756, 6.109999999999999432, 1.637169565754164280 ) ) ;
#121954 = EDGE_CURVE ( 'NONE', #53059, #22625, #103804, .T. ) ;
#121955 = VERTEX_POINT ( 'NONE', #102438 ) ;
#121956 = DIRECTION ( 'NONE',  ( 0.7071067811865486830, -0.7071067811865464625, -0.000000000000000000 ) ) ;
#121957 = CARTESIAN_POINT ( 'NONE',  ( 21.70710678118639692, -12.74070752338415247, 5.000000000000000000 ) ) ;
#121958 = CARTESIAN_POINT ( 'NONE',  ( 0.000000000000000000, 0.000000000000000000, 5.000000000000000000 ) ) ;
#121959 = LINE ( 'NONE', #141607, #61963 ) ;
#121960 = FACE_OUTER_BOUND ( 'NONE', #107806, .T. ) ;
#121961 = VECTOR ( 'NONE', #53005, 1000.000000000000000 ) ;
#121962 = PLANE ( 'NONE',  #51583 ) ;
#121963 = CARTESIAN_POINT ( 'NONE',  ( 7.828169399223478209, 3.759292476615683665, 4.000000000000000000 ) ) ;
#121964 = VECTOR ( 'NONE', #79831, 1000.000000000000000 ) ;
#121965 = CARTESIAN_POINT ( 'NONE',  ( 46.60002705046288440, 5.819803920172570422, 5.819803920172574863 ) ) ;
#121966 = CARTESIAN_POINT ( 'NONE',  ( 48.29974487139158867, -27.71228299555239971, 4.000000000000000000 ) ) ;
#121967 = AXIS2_PLACEMENT_3D ( 'NONE', #116471, #127334, #86534 ) ;
#121968 = FACE_OUTER_BOUND ( 'NONE', #39464, .T. ) ;
#121969 = VERTEX_POINT ( 'NONE', #116132 ) ;
#121970 = VERTEX_POINT ( 'NONE', #3089 ) ;
#121971 = CARTESIAN_POINT ( 'NONE',  ( 50.14583333333333570, 2.130196079827431976, -7.949999999999999289 ) ) ;
#121972 = LINE ( 'NONE', #110379, #50928 ) ;
#121973 = ADVANCED_FACE ( 'NONE', ( #136455 ), #79988, .F. ) ;
#121974 = VECTOR ( 'NONE', #110733, 999.9999999999998863 ) ;
#121976 = CARTESIAN_POINT ( 'NONE',  ( -21.71757738642552127, -21.73023691814493574, 5.000000000000000888 ) ) ;
#121975 = VECTOR ( 'NONE', #104531, 1000.000000000000000 ) ;
#121977 = VERTEX_POINT ( 'NONE', #15362 ) ;
#121978 = CARTESIAN_POINT ( 'NONE',  ( -0.8062233626479216042, -1.049713688934361677, 3.918581274736450570 ) ) ;
#121979 = DIRECTION ( 'NONE',  ( -0.6830127018922180770, -0.6830127018922204085, -0.2588190451025213501 ) ) ;
#121980 = CARTESIAN_POINT ( 'NONE',  ( 37.33376352523143282, 6.110000000000001208, 1.122388791418549305E-15 ) ) ;
#121981 = EDGE_CURVE ( 'NONE', #22757, #137228, #12995, .T. ) ;
#121982 = ORIENTED_EDGE ( 'NONE', *, *, #125143, .T. ) ;
#121983 = DIRECTION ( 'NONE',  ( 0.5735764363510448272, -0.8191520442889927978, 1.003171929053526103E-16 ) ) ;
#121984 = VERTEX_POINT ( 'NONE', #71233 ) ;
#121985 = VERTEX_POINT ( 'NONE', #49500 ) ;
#121986 = PLANE ( 'NONE',  #95798 ) ;
#121987 = CARTESIAN_POINT ( 'NONE',  ( 184.1499999999998067, -49.14999999999999147, 34.92500000000001847 ) ) ;
#121988 = DIRECTION ( 'NONE',  ( -0.000000000000000000, -0.000000000000000000, -1.000000000000000000 ) ) ;
#121990 = EDGE_CURVE ( 'NONE', #55621, #60957, #27694, .T. ) ;
#121989 = ORIENTED_EDGE ( 'NONE', *, *, #18444, .F. ) ;
#121991 = DIRECTION ( 'NONE',  ( -0.7071067811865486830, -0.7071067811865464625, 0.000000000000000000 ) ) ;
#121992 = EDGE_LOOP ( 'NONE', ( #61294, #118421 ) ) ;
#121993 = CARTESIAN_POINT ( 'NONE',  ( 86.91709685856477563, 3.054999999999998828, 5.291415217122922066 ) ) ;
#121994 = EDGE_CURVE ( 'NONE', #57179, #124741, #38585, .T. ) ;
#121995 = DIRECTION ( 'NONE',  ( -1.000000000000000000, -0.000000000000000000, -0.000000000000000000 ) ) ;
#121996 = LINE ( 'NONE', #1626, #112577 ) ;
#121997 = CYLINDRICAL_SURFACE ( 'NONE', #109390, 6.094999999999989093 ) ;
#121998 = AXIS2_PLACEMENT_3D ( 'NONE', #99973, #91264, #26690 ) ;
#121999 = CARTESIAN_POINT ( 'NONE',  ( 57.18398860626899705, 28.73617430169827358, 5.000000000000000000 ) ) ;
#122000 = DIRECTION ( 'NONE',  ( -0.3543493200069163795, -9.265275131829747941E-33, -0.9351131265310288487 ) ) ;
#122001 = ORIENTED_EDGE ( 'NONE', *, *, #113496, .F. ) ;
#122002 = VECTOR ( 'NONE', #47454, 1000.000000000000000 ) ;
#122003 = DIRECTION ( 'NONE',  ( 0.6830127018922180770, -0.6830127018922204085, -0.2588190451025213501 ) ) ;
#122004 = CARTESIAN_POINT ( 'NONE',  ( 54.30793019189810167, -6.109999999999998543, 1.637169565754158063 ) ) ;
#122005 = CARTESIAN_POINT ( 'NONE',  ( -12.00548008471251293, 28.92564299267929684, 4.000000000000000000 ) ) ;
#122006 = DIRECTION ( 'NONE',  ( -0.7071067811865487940, 0.7071067811865463515, -0.000000000000000000 ) ) ;
#122007 = DIRECTION ( 'NONE',  ( -0.000000000000000000, 0.000000000000000000, 1.000000000000000000 ) ) ;
#122008 = ORIENTED_EDGE ( 'NONE', *, *, #132007, .F. ) ;
#122009 = MECHANICAL_DESIGN_GEOMETRIC_PRESENTATION_REPRESENTATION (  '', ( #84981 ), #89632 ) ;
#122010 = CARTESIAN_POINT ( 'NONE',  ( -31.49999999999977973, -13.53360074219760101, 5.000000000000000000 ) ) ;
#122011 = SURFACE_STYLE_FILL_AREA ( #111129 ) ;
#122012 = EDGE_LOOP ( 'NONE', ( #27908, #20219, #29558, #105588 ) ) ;
#122013 = EDGE_CURVE ( 'NONE', #79902, #108305, #135078, .T. ) ;
#122014 = CARTESIAN_POINT ( 'NONE',  ( 34.92500000000001137, 22.27000000000001023, -8.436784469852378621 ) ) ;
#122015 = VERTEX_POINT ( 'NONE', #91545 ) ;
#122016 = DIRECTION ( 'NONE',  ( -0.3543493200069162685, -0.000000000000000000, -0.9351131265310288487 ) ) ;
#122017 = FACE_OUTER_BOUND ( 'NONE', #14582, .T. ) ;
#122018 = VECTOR ( 'NONE', #33412, 1000.000000000000000 ) ;
#122019 = DIRECTION ( 'NONE',  ( -0.000000000000000000, 0.000000000000000000, 1.000000000000000000 ) ) ;
#122020 = LINE ( 'NONE', #22686, #48843 ) ;
#122021 = FACE_BOUND ( 'NONE', #21776, .T. ) ;
#122022 = DIRECTION ( 'NONE',  ( -0.7071067811865486830, -0.7071067811865464625, -0.000000000000000000 ) ) ;
#122023 = CARTESIAN_POINT ( 'NONE',  ( 0.000000000000000000, -0.3999999999999998002, -2.015694669338588429 ) ) ;
#122024 = CARTESIAN_POINT ( 'NONE',  ( 6.707106781186499056, -15.74070752338412049, 5.000000000000000000 ) ) ;
#122026 = ORIENTED_EDGE ( 'NONE', *, *, #120157, .F. ) ;
#122025 = LINE ( 'NONE', #112605, #110651 ) ;
#122027 = LINE ( 'NONE', #11838, #62629 ) ;
#122028 = ORIENTED_EDGE ( 'NONE', *, *, #38510, .F. ) ;
#122029 = EDGE_CURVE ( 'NONE', #54275, #67480, #69091, .T. ) ;
#122031 = VERTEX_POINT ( 'NONE', #8748 ) ;
#122030 = EDGE_CURVE ( 'NONE', #66308, #117459, #135761, .T. ) ;
#122032 = CARTESIAN_POINT ( 'NONE',  ( 73.12043019189812298, 3.055000000000001936, -5.291415217122916737 ) ) ;
#122033 = ORIENTED_EDGE ( 'NONE', *, *, #59892, .F. ) ;
#122034 = LINE ( 'NONE', #109751, #43059 ) ;
#122035 = AXIS2_PLACEMENT_3D ( 'NONE', #126324, #14712, #16095 ) ;
#122036 = LINE ( 'NONE', #8956, #109140 ) ;
#122037 = EDGE_CURVE ( 'NONE', #65337, #61284, #77142, .T. ) ;
#122038 = ORIENTED_EDGE ( 'NONE', *, *, #604, .F. ) ;
#122039 = FACE_OUTER_BOUND ( 'NONE', #8241, .T. ) ;
#122040 = EDGE_CURVE ( 'NONE', #64319, #104775, #142780, .T. ) ;
#122041 = EDGE_CURVE ( 'NONE', #4252, #9940, #138623, .T. ) ;
#122042 = LINE ( 'NONE', #35808, #123680 ) ;
#122043 = CARTESIAN_POINT ( 'NONE',  ( 23.78840764549667597, 3.061616997868385113E-16, -2.500000000000001332 ) ) ;
#122044 = PLANE ( 'NONE',  #124331 ) ;
#122045 = DIRECTION ( 'NONE',  ( -0.000000000000000000, 0.000000000000000000, 1.000000000000000000 ) ) ;
#122047 = DIRECTION ( 'NONE',  ( 0.6830127018922180770, -0.6830127018922204085, -0.2588190451025213501 ) ) ;
#122046 = DIRECTION ( 'NONE',  ( 0.7071067811865487940, 0.7071067811865463515, -0.000000000000000000 ) ) ;
#122048 = LINE ( 'NONE', #135807, #111811 ) ;
#122049 = DIRECTION ( 'NONE',  ( 0.6830127018922181881, 0.6830127018922202975, -0.2588190451025214056 ) ) ;
#122050 = ORIENTED_EDGE ( 'NONE', *, *, #108444, .T. ) ;
#122051 = CARTESIAN_POINT ( 'NONE',  ( 0.000000000000000000, 0.000000000000000000, 5.000000000000000000 ) ) ;
#122052 = VERTEX_POINT ( 'NONE', #63233 ) ;
#122053 = LINE ( 'NONE', #88024, #128284 ) ;
#122054 = DIRECTION ( 'NONE',  ( 0.5735764363510448272, -0.8191520442889927978, 1.003171929053526103E-16 ) ) ;
#122055 = ORIENTED_EDGE ( 'NONE', *, *, #85026, .F. ) ;
#122056 = ORIENTED_EDGE ( 'NONE', *, *, #30756, .T. ) ;
#122058 = EDGE_LOOP ( 'NONE', ( #33312, #15235, #81615 ) ) ;
#122057 = AXIS2_PLACEMENT_3D ( 'NONE', #57887, #15715, #4840 ) ;
#122059 = EDGE_CURVE ( 'NONE', #104096, #81350, #26989, .T. ) ;
#122060 = ADVANCED_FACE ( 'NONE', ( #30575 ), #61785, .T. ) ;
#122061 = CARTESIAN_POINT ( 'NONE',  ( 26.68793019189810423, 6.110000000000002984, -1.637169565754156730 ) ) ;
#122062 = EDGE_LOOP ( 'NONE', ( #87906, #76241, #100036 ) ) ;
#122063 = DIRECTION ( 'NONE',  ( 0.000000000000000000, 1.000000000000000000, -0.000000000000000000 ) ) ;
#122064 = VECTOR ( 'NONE', #94559, 1000.000000000000000 ) ;
#122065 = AXIS2_PLACEMENT_3D ( 'NONE', #57180, #102806, #57893 ) ;
#122066 = EDGE_CURVE ( 'NONE', #63283, #18713, #105703, .T. ) ;
#122067 = CARTESIAN_POINT ( 'NONE',  ( 8.994519915287490619, 28.92564299267944250, 4.000000000000000000 ) ) ;
#122068 = VECTOR ( 'NONE', #81200, 1000.000000000000000 ) ;
#122069 = CARTESIAN_POINT ( 'NONE',  ( 31.54580628287043709, 5.278424836066143655, -3.047499999999997655 ) ) ;
#122070 = CARTESIAN_POINT ( 'NONE',  ( -59.99451991528749772, 28.92564299267980132, 4.000000000000000000 ) ) ;
#122071 = ADVANCED_FACE ( 'NONE', ( #20371 ), #140732, .F. ) ;
#122072 = ORIENTED_EDGE ( 'NONE', *, *, #48887, .T. ) ;
#122073 = CARTESIAN_POINT ( 'NONE',  ( -45.48921356237309510, -27.52281430457087197, 5.000000000000000000 ) ) ;
#122074 = CARTESIAN_POINT ( 'NONE',  ( 6.489213562373093325, -27.52281430457059841, 5.000000000000000000 ) ) ;
#122075 = VECTOR ( 'NONE', #105586, 1000.000000000000000 ) ;
#122076 = CARTESIAN_POINT ( 'NONE',  ( -24.00548008471250938, 28.92564299267921513, 4.000000000000000000 ) ) ;
#122077 = EDGE_CURVE ( 'NONE', #9912, #60822, #130613, .T. ) ;
#122079 = VERTEX_POINT ( 'NONE', #51618 ) ;
#122078 = DIRECTION ( 'NONE',  ( -0.000000000000000000, 0.000000000000000000, 1.000000000000000000 ) ) ;
#122080 = EDGE_LOOP ( 'NONE', ( #123017, #89425, #110080, #127098, #26569 ) ) ;
#122081 = CARTESIAN_POINT ( 'NONE',  ( -8.018447346356650129, 18.75929247661552424, 20.33588619593444591 ) ) ;
#122082 = CARTESIAN_POINT ( 'NONE',  ( 25.00193056682080339, -22.22500000000000142, 4.500000000000000888 ) ) ;
#122083 = DIRECTION ( 'NONE',  ( 0.6830127018922181881, 0.6830127018922202975, -0.2588190451025214056 ) ) ;
#122084 = VERTEX_POINT ( 'NONE', #107399 ) ;
#122085 = CARTESIAN_POINT ( 'NONE',  ( 48.48921356237309510, -27.52281430457089328, 5.000000000000000000 ) ) ;
#122086 = CYLINDRICAL_SURFACE ( 'NONE', #117228, 0.5000000000000004441 ) ;
#122087 = EDGE_LOOP ( 'NONE', ( #106176, #124108, #30416, #57898 ) ) ;
#122088 = SPHERICAL_SURFACE ( 'NONE', #811, 9.500000000000000000 ) ;
#122089 = CARTESIAN_POINT ( 'NONE',  ( 23.99999999999984013, -10.44781430457072346, 5.000000000000000000 ) ) ;
#122090 = LINE ( 'NONE', #78609, #31065 ) ;
#122091 = ADVANCED_FACE ( 'NONE', ( #95810 ), #40734, .F. ) ;
#122092 = CARTESIAN_POINT ( 'NONE',  ( 66.48921356237309510, -27.52281430457101763, 5.000000000000000000 ) ) ;
#122093 = CARTESIAN_POINT ( 'NONE',  ( 34.17183060077623935, 3.759292476615688550, 4.000000000000000000 ) ) ;
#122094 = CARTESIAN_POINT ( 'NONE',  ( -51.18398860626899705, 28.73617430169823095, 5.000000000000000000 ) ) ;
#122095 = LINE ( 'NONE', #54039, #51742 ) ;
#122096 = LINE ( 'NONE', #56194, #85370 ) ;
#122097 = ORIENTED_EDGE ( 'NONE', *, *, #1162, .T. ) ;
#122098 = CARTESIAN_POINT ( 'NONE',  ( 5.510786437626906675, -27.52281430457051314, 5.000000000000000000 ) ) ;
#122099 = EDGE_CURVE ( 'NONE', #28445, #97682, #43253, .T. ) ;
#122100 = ORIENTED_EDGE ( 'NONE', *, *, #97359, .T. ) ;
#122102 = EDGE_CURVE ( 'NONE', #89832, #121130, #84940, .T. ) ;
#122101 = VECTOR ( 'NONE', #125090, 1000.000000000000000 ) ;
#122103 = DIRECTION ( 'NONE',  ( -0.7071067811865486830, 0.7071067811865464625, 0.000000000000000000 ) ) ;
#122104 = CARTESIAN_POINT ( 'NONE',  ( -13.36246187583893530, 22.22500000000000142, 4.000000000000000000 ) ) ;
#122105 = EDGE_CURVE ( 'NONE', #68584, #8173, #85636, .T. ) ;
#122106 = CARTESIAN_POINT ( 'NONE',  ( 2.301729841053981040, 2.500000000000000444, 3.061616997868383634E-16 ) ) ;
#122107 = VECTOR ( 'NONE', #134077, 1000.000000000000000 ) ;
#122108 = EDGE_LOOP ( 'NONE', ( #85029, #9319, #55782, #72611 ) ) ;
#122109 = PLANE ( 'NONE',  #99368 ) ;
#122110 = FACE_OUTER_BOUND ( 'NONE', #137767, .T. ) ;
#122111 = DIRECTION ( 'NONE',  ( -3.973028287378889149E-16, 1.000000000000000000, 0.000000000000000000 ) ) ;
#122112 = VERTEX_POINT ( 'NONE', #119671 ) ;
#122113 =( LENGTH_UNIT ( ) NAMED_UNIT ( * ) SI_UNIT ( .MILLI., .METRE. ) );
#122114 = LINE ( 'NONE', #22769, #76662 ) ;
#122115 = LINE ( 'NONE', #90954, #7592 ) ;
#122116 = VECTOR ( 'NONE', #9858, 1000.000000000000000 ) ;
#122117 = FILL_AREA_STYLE ('',( #77239 ) ) ;
#122118 = DIRECTION ( 'NONE',  ( 0.7071067811865487940, 0.7071067811865463515, 0.000000000000000000 ) ) ;
#122119 = CARTESIAN_POINT ( 'NONE',  ( 57.95376352523144448, -6.109999999999999432, -3.741295971395163529E-16 ) ) ;
#122120 = DIRECTION ( 'NONE',  ( -0.7071067811865486830, -0.7071067811865464625, 0.000000000000000000 ) ) ;
#122121 = CARTESIAN_POINT ( 'NONE',  ( 12.49289321881344783, -34.80096641561354431, 18.05156865852269732 ) ) ;
#122122 = CARTESIAN_POINT ( 'NONE',  ( 32.45419371712955581, 6.884901960086283523, 3.975000000000002753 ) ) ;
#122123 = CARTESIAN_POINT ( 'NONE',  ( -27.00548008471251293, 28.92564299267919381, 4.000000000000000000 ) ) ;
#122124 = ORIENTED_EDGE ( 'NONE', *, *, #29776, .T. ) ;
#122125 = CARTESIAN_POINT ( 'NONE',  ( -5.218373117075014278, 21.74787736706806385, 4.999607392498049308 ) ) ;
#122126 = VERTEX_POINT ( 'NONE', #18216 ) ;
#122127 = CARTESIAN_POINT ( 'NONE',  ( 8.994519915287490619, 28.92564299267944250, 4.000000000000000000 ) ) ;
#122128 = CARTESIAN_POINT ( 'NONE',  ( -33.18398860626899705, 28.73617430169810305, 5.000000000000000000 ) ) ;
#122129 = FACE_OUTER_BOUND ( 'NONE', #50981, .T. ) ;
#122130 = CARTESIAN_POINT ( 'NONE',  ( 11.99999999999992006, 2.342191155542461267, -5.001666872980111478 ) ) ;
#122131 = LINE ( 'NONE', #90226, #120318 ) ;
#122132 = CARTESIAN_POINT ( 'NONE',  ( -17.20003122016825614, 8.259292476615641476, 16.85664084051845180 ) ) ;
#122133 = EDGE_LOOP ( 'NONE', ( #33013, #30156, #116596, #86795, #107804, #114836 ) ) ;
#122134 = ORIENTED_EDGE ( 'NONE', *, *, #32894, .T. ) ;
#122135 = CARTESIAN_POINT ( 'NONE',  ( 8.000000000000007105, 0.000000000000000000, 0.000000000000000000 ) ) ;
#122136 = FACE_OUTER_BOUND ( 'NONE', #95638, .T. ) ;
#122137 = CARTESIAN_POINT ( 'NONE',  ( -22.49999999999984013, -20.53675388469232388, 2.352720554255840923 ) ) ;
#122138 = LINE ( 'NONE', #121435, #15634 ) ;
#122139 = CARTESIAN_POINT ( 'NONE',  ( 80.87086038379622721, 6.884901960086289741, -3.974999999999993427 ) ) ;
#122140 = PLANE ( 'NONE',  #30064 ) ;
#122141 = LINE ( 'NONE', #56243, #15875 ) ;
#122142 = VERTEX_POINT ( 'NONE', #72694 ) ;
#122143 = CONICAL_SURFACE ( 'NONE', #8681, 2.500000000000000444, 0.9599310885968830309 ) ;
#122144 = CARTESIAN_POINT ( 'NONE',  ( 69.25000000000000000, -9.735942053221458872E-16, 7.950000000000000178 ) ) ;
#122145 = PLANE ( 'NONE',  #79436 ) ;
#122146 = CARTESIAN_POINT ( 'NONE',  ( 32.99451991528749062, 28.92564299267960948, 4.000000000000000000 ) ) ;
#122147 = PLANE ( 'NONE',  #10414 ) ;
#122148 = ORIENTED_EDGE ( 'NONE', *, *, #37619, .F. ) ;
#122149 = DIRECTION ( 'NONE',  ( -0.6830127018922181881, 0.6830127018922202975, -0.2588190451025214056 ) ) ;
#122150 = VERTEX_POINT ( 'NONE', #129875 ) ;
#122151 = VECTOR ( 'NONE', #135890, 1000.000000000000227 ) ;
#122152 = DIRECTION ( 'NONE',  ( 1.000000000000000000, 0.000000000000000000, 0.000000000000000000 ) ) ;
#122153 = CARTESIAN_POINT ( 'NONE',  ( 62.41709685856476852, 3.054999999999998828, 5.291415217122922066 ) ) ;
#122154 = ORIENTED_EDGE ( 'NONE', *, *, #66100, .T. ) ;
#122155 = CARTESIAN_POINT ( 'NONE',  ( -25.39999999999996305, 0.000000000000000000, 2.500000000000000000 ) ) ;
#122156 = CARTESIAN_POINT ( 'NONE',  ( -34.49999999999976552, 0.05432934483094037370, 4.994342998332168548 ) ) ;
#122157 =( NAMED_UNIT ( * ) PLANE_ANGLE_UNIT ( ) SI_UNIT ( $, .RADIAN. ) );
#122158 = VECTOR ( 'NONE', #22869, 1000.000000000000000 ) ;
#122159 = DIRECTION ( 'NONE',  ( 0.7071067811865487940, 0.7071067811865463515, 0.000000000000000000 ) ) ;
#122160 = ADVANCED_FACE ( 'NONE', ( #74813 ), #19676, .F. ) ;
#122161 = FACE_OUTER_BOUND ( 'NONE', #14917, .T. ) ;
#122163 = ORIENTED_EDGE ( 'NONE', *, *, #92064, .T. ) ;
#122162 = FACE_OUTER_BOUND ( 'NONE', #54964, .T. ) ;
#122164 = EDGE_CURVE ( 'NONE', #92198, #109138, #135857, .T. ) ;
#122165 = CARTESIAN_POINT ( 'NONE',  ( -12.69999999999998153, 0.000000000000000000, 0.000000000000000000 ) ) ;
#122166 = LINE ( 'NONE', #77295, #56933 ) ;
#122167 = FACE_OUTER_BOUND ( 'NONE', #134194, .T. ) ;
#122168 = VECTOR ( 'NONE', #134018, 1000.000000000000000 ) ;
#122169 = DIRECTION ( 'NONE',  ( 0.7071067811865486830, -0.7071067811865464625, -0.000000000000000000 ) ) ;
#122170 = VECTOR ( 'NONE', #23999, 1000.000000000000000 ) ;
#122171 = ORIENTED_EDGE ( 'NONE', *, *, #26982, .T. ) ;
#122172 = ORIENTED_EDGE ( 'NONE', *, *, #45056, .T. ) ;
#122173 = CARTESIAN_POINT ( 'NONE',  ( 68.83376352523143282, 6.110000000000001208, 1.122388791418549305E-15 ) ) ;
#122174 = ORIENTED_EDGE ( 'NONE', *, *, #83308, .T. ) ;
#122175 = ADVANCED_FACE ( 'NONE', ( #29829 ), #74071, .F. ) ;
#122176 = CARTESIAN_POINT ( 'NONE',  ( -23.99999999999983302, 14.87792677143806230, -11.06722581663445482 ) ) ;
#122177 = LINE ( 'NONE', #91024, #118199 ) ;
#122178 = DIRECTION ( 'NONE',  ( -1.000000000000000000, -1.224606353822377258E-16, -0.000000000000000000 ) ) ;
#122179 = CARTESIAN_POINT ( 'NONE',  ( 0.000000000000000000, 0.000000000000000000, 5.000000000000000000 ) ) ;
#122180 = DIRECTION ( 'NONE',  ( -1.000000000000000000, -0.000000000000000000, -0.000000000000000000 ) ) ;
#122181 = ORIENTED_EDGE ( 'NONE', *, *, #67665, .T. ) ;
#122182 = ORIENTED_EDGE ( 'NONE', *, *, #62862, .F. ) ;
#122183 = CARTESIAN_POINT ( 'NONE',  ( -25.82816939922334498, -8.240707523384196875, 4.000000000000000000 ) ) ;
#122184 = CARTESIAN_POINT ( 'NONE',  ( -19.83193850628799737, -2.400066657216377575, -33.20899412005067575 ) ) ;
#122185 = EDGE_CURVE ( 'NONE', #61991, #130861, #42890, .T. ) ;
#122186 = ORIENTED_EDGE ( 'NONE', *, *, #60650, .F. ) ;
#122187 = DIRECTION ( 'NONE',  ( 0.6830127018922180770, -0.6830127018922204085, -0.2588190451025213501 ) ) ;
#122188 = DIRECTION ( 'NONE',  ( -0.6830127018922180770, -0.6830127018922204085, -0.2588190451025213501 ) ) ;
#122189 = DIRECTION ( 'NONE',  ( -0.6830127018922180770, -0.6830127018922204085, -0.2588190451025213501 ) ) ;
#122190 = EDGE_CURVE ( 'NONE', #33921, #82671, #99352, .T. ) ;
#122191 = ORIENTED_EDGE ( 'NONE', *, *, #43480, .T. ) ;
#122192 = FACE_BOUND ( 'NONE', #53793, .T. ) ;
#122193 = CARTESIAN_POINT ( 'NONE',  ( -29.99999999999978328, -12.03360074219761700, 5.000000000000000000 ) ) ;
#122194 = LINE ( 'NONE', #22867, #132335 ) ;
#122195 = DIRECTION ( 'NONE',  ( -0.000000000000000000, 0.000000000000000000, 1.000000000000000000 ) ) ;
#122196 = AXIS2_PLACEMENT_3D ( 'NONE', #93549, #92821, #37758 ) ;
#122197 = EDGE_CURVE ( 'NONE', #88988, #121666, #81038, .T. ) ;
#122198 = EDGE_CURVE ( 'NONE', #119727, #127658, #77654, .T. ) ;
#122199 = DIRECTION ( 'NONE',  ( -0.3543493200069162685, -0.000000000000000000, -0.9351131265310288487 ) ) ;
#122200 = CARTESIAN_POINT ( 'NONE',  ( 27.29974487139158512, -27.71228299555225405, 4.000000000000000000 ) ) ;
#122201 = DIRECTION ( 'NONE',  ( -7.198061428684097375E-18, 0.9982711593182352905, -0.05877663203541310527 ) ) ;
#122202 = ORIENTED_EDGE ( 'NONE', *, *, #119565, .T. ) ;
#122203 = ORIENTED_EDGE ( 'NONE', *, *, #115130, .F. ) ;
#122204 = CARTESIAN_POINT ( 'NONE',  ( 103.7454301918981230, -5.291415217122918513, -3.055000000000000160 ) ) ;
#122205 = VERTEX_POINT ( 'NONE', #32722 ) ;
#122206 =( NAMED_UNIT ( * ) SI_UNIT ( $, .STERADIAN. ) SOLID_ANGLE_UNIT ( ) );
#122207 = ORIENTED_EDGE ( 'NONE', *, *, #127816, .F. ) ;
#122208 = ADVANCED_FACE ( 'NONE', ( #69452 ), #120375, .F. ) ;
#122209 = LINE ( 'NONE', #43968, #102579 ) ;
#122210 = CARTESIAN_POINT ( 'NONE',  ( 6.770042794577893375, 21.73644205237997440, 5.000000000000000888 ) ) ;
#122211 = EDGE_CURVE ( 'NONE', #74950, #106339, #47518, .T. ) ;
#122212 = EDGE_CURVE ( 'NONE', #34178, #78214, #97964, .T. ) ;
#122213 = CARTESIAN_POINT ( 'NONE',  ( -6.183988606268994381, 28.73617430169791476, 5.000000000000000000 ) ) ;
#122214 = ORIENTED_EDGE ( 'NONE', *, *, #28782, .T. ) ;
#122215 = CARTESIAN_POINT ( 'NONE',  ( 71.00000000000000000, 0.000000000000000000, -7.950000000000000178 ) ) ;
#122217 = FACE_OUTER_BOUND ( 'NONE', #4464, .T. ) ;
#122216 = B_SPLINE_CURVE_WITH_KNOTS ( 'NONE', 3,
 ( #32366, #7729, #141860, #43255, #9121, #86756, #51983, #18594, #98342, #76610 ),
 .UNSPECIFIED., .F., .F.,
 ( 4, 2, 2, 2, 4 ),
 ( 0.001941010781631071457, 0.002456031491763875727, 0.002971052201896679998, 0.003486072912029485136, 0.004001093622162290274 ),
 .UNSPECIFIED. ) ;
#122218 = DIRECTION ( 'NONE',  ( 1.000000000000000000, 0.000000000000000000, 0.000000000000000000 ) ) ;
#122219 = FACE_OUTER_BOUND ( 'NONE', #109549, .T. ) ;
#122220 = CARTESIAN_POINT ( 'NONE',  ( 2.379139616203772789, -5.278424836066145431, -3.047499999999993658 ) ) ;
#122221 = DIRECTION ( 'NONE',  ( 0.000000000000000000, -1.000000000000000000, 0.000000000000000000 ) ) ;
#122222 = VERTEX_POINT ( 'NONE', #70197 ) ;
#122223 = EDGE_CURVE ( 'NONE', #3283, #52621, #21823, .T. ) ;
#122224 = LINE ( 'NONE', #102654, #112043 ) ;
#122225 = LINE ( 'NONE', #66459, #35055 ) ;
#122227 = EDGE_LOOP ( 'NONE', ( #71210, #41616, #63584, #49615 ) ) ;
#122226 = VECTOR ( 'NONE', #100502, 1000.000000000000000 ) ;
#122228 = VERTEX_POINT ( 'NONE', #76211 ) ;
#122229 = EDGE_CURVE ( 'NONE', #58779, #105272, #125239, .T. ) ;
#122231 = ORIENTED_EDGE ( 'NONE', *, *, #122884, .F. ) ;
#122230 = EDGE_CURVE ( 'NONE', #74252, #83338, #110229, .T. ) ;
#122232 = CARTESIAN_POINT ( 'NONE',  ( 57.60459685856476852, 1.637169565754164946, -6.109999999999999432 ) ) ;
#122233 = VERTEX_POINT ( 'NONE', #3431 ) ;
#122234 = DIRECTION ( 'NONE',  ( -0.6830127018922180770, -0.6830127018922204085, -0.2588190451025213501 ) ) ;
#122235 = CARTESIAN_POINT ( 'NONE',  ( 5.441639616203772789, -6.094999999999989093, 1.633150327867691765 ) ) ;
#122236 = VECTOR ( 'NONE', #67, 1000.000000000000000 ) ;
#122237 = CARTESIAN_POINT ( 'NONE',  ( 87.35459685856476142, -1.637169565754161615, 6.110000000000000320 ) ) ;
#122238 = FACE_OUTER_BOUND ( 'NONE', #79807, .T. ) ;
#122239 = EDGE_CURVE ( 'NONE', #30215, #140739, #25930, .T. ) ;
#122240 = ORIENTED_EDGE ( 'NONE', *, *, #103395, .T. ) ;
#122241 = LINE ( 'NONE', #88947, #60423 ) ;
#122242 = EDGE_CURVE ( 'NONE', #91297, #56327, #36790, .T. ) ;
#122243 = FACE_OUTER_BOUND ( 'NONE', #29826, .T. ) ;
#122244 = ORIENTED_EDGE ( 'NONE', *, *, #112141, .T. ) ;
#122245 = CARTESIAN_POINT ( 'NONE',  ( -2.510786437626908008, -27.52281430457053446, 5.000000000000000000 ) ) ;
#122246 = CARTESIAN_POINT ( 'NONE',  ( 12.48921356237309155, -27.52281430457064104, 5.000000000000000000 ) ) ;
#122247 = ORIENTED_EDGE ( 'NONE', *, *, #35835, .F. ) ;
#122248 = LINE ( 'NONE', #110645, #22587 ) ;
#122249 = VERTEX_POINT ( 'NONE', #31983 ) ;
#122250 = ORIENTED_EDGE ( 'NONE', *, *, #23566, .F. ) ;
#122251 = VERTEX_POINT ( 'NONE', #66764 ) ;
#122252 = CARTESIAN_POINT ( 'NONE',  ( 123.2870968585647944, 3.054999999999997495, 5.291415217122919401 ) ) ;
#122253 = AXIS2_PLACEMENT_3D ( 'NONE', #5649, #29553, #139792 ) ;
#122254 = DIRECTION ( 'NONE',  ( -0.7071067811865487940, 0.7071067811865463515, 0.000000000000000000 ) ) ;
#122255 = AXIS2_PLACEMENT_3D ( 'NONE', #105442, #6100, #106875 ) ;
#122256 = LINE ( 'NONE', #22929, #78708 ) ;
#122257 = LINE ( 'NONE', #67195, #106682 ) ;
#122258 = ORIENTED_EDGE ( 'NONE', *, *, #84777, .T. ) ;
#122259 = AXIS2_PLACEMENT_3D ( 'NONE', #139748, #107778, #77857 ) ;
#122260 = AXIS2_PLACEMENT_3D ( 'NONE', #59342, #14373, #68783 ) ;
#122261 = EDGE_CURVE ( 'NONE', #105963, #78350, #15455, .T. ) ;
#122262 = EDGE_CURVE ( 'NONE', #88988, #122835, #10910, .T. ) ;
#122263 = CARTESIAN_POINT ( 'NONE',  ( 13.39540314143521904, 2.126176841940962348, 7.934999999999989839 ) ) ;
#122264 = DIRECTION ( 'NONE',  ( 1.000000000000000000, 0.000000000000000000, 0.000000000000000000 ) ) ;
#122265 = LINE ( 'NONE', #133884, #71475 ) ;
#122266 = CARTESIAN_POINT ( 'NONE',  ( -32.26821726222483733, 22.27000000000000313, -14.68217205629616018 ) ) ;
#122267 = ORIENTED_EDGE ( 'NONE', *, *, #35191, .T. ) ;
#122268 = ORIENTED_EDGE ( 'NONE', *, *, #19864, .T. ) ;
#122269 = ORIENTED_EDGE ( 'NONE', *, *, #128352, .F. ) ;
#122270 = PLANE ( 'NONE',  #76495 ) ;
#122271 = DIRECTION ( 'NONE',  ( 0.3543493200069162685, -0.000000000000000000, -0.9351131265310288487 ) ) ;
#122272 = CARTESIAN_POINT ( 'NONE',  ( 1.199999999999999956, 0.000000000000000000, 0.000000000000000000 ) ) ;
#122273 = ADVANCED_FACE ( 'NONE', ( #55905 ), #13094, .F. ) ;
#122274 = DIRECTION ( 'NONE',  ( 0.7071067811865487940, 0.7071067811865463515, 0.000000000000000000 ) ) ;
#122275 = DIRECTION ( 'NONE',  ( -0.000000000000000000, -0.3543493200069152693, 0.9351131265310292928 ) ) ;
#122276 = DIRECTION ( 'NONE',  ( 0.7071067811865487940, 0.7071067811865463515, 0.000000000000000000 ) ) ;
#122277 = DIRECTION ( 'NONE',  ( -0.000000000000000000, -0.000000000000000000, 1.000000000000000000 ) ) ;
#122278 = DIRECTION ( 'NONE',  ( 1.000000000000000000, 0.000000000000000000, 0.000000000000000000 ) ) ;
#122279 = DIRECTION ( 'NONE',  ( -0.7071067811865487940, 0.7071067811865463515, 0.000000000000000000 ) ) ;
#122280 = EDGE_LOOP ( 'NONE', ( #76771, #108005, #92277, #135956, #65833 ) ) ;
#122281 = CARTESIAN_POINT ( 'NONE',  ( 23.99451991528749062, 28.92564299267954908, 4.000000000000000000 ) ) ;
#122282 = ORIENTED_EDGE ( 'NONE', *, *, #4013, .T. ) ;
#122283 = AXIS2_PLACEMENT_3D ( 'NONE', #20312, #99297, #41362 ) ;
#122284 = CARTESIAN_POINT ( 'NONE',  ( 16.90050536373548340, -0.4844931144635390985, -34.66719912185458696 ) ) ;
#122285 = ORIENTED_EDGE ( 'NONE', *, *, #94998, .T. ) ;
#122286 = VECTOR ( 'NONE', #90947, 1000.000000000000227 ) ;
#122287 = VECTOR ( 'NONE', #75375, 1000.000000000000000 ) ;
#122288 = CARTESIAN_POINT ( 'NONE',  ( 25.49999999999981526, -10.53360074219763121, 5.000000000000000000 ) ) ;
#122290 = ORIENTED_EDGE ( 'NONE', *, *, #4519, .F. ) ;
#122289 = CARTESIAN_POINT ( 'NONE',  ( 41.68749999999997868, -5.819803920172573974, 5.819803920172573086 ) ) ;
#122291 = DIRECTION ( 'NONE',  ( 1.000000000000000000, 0.000000000000000000, 0.000000000000000000 ) ) ;
#122292 = DIRECTION ( 'NONE',  ( -0.6830127018922180770, -0.6830127018922204085, -0.2588190451025213501 ) ) ;
#122293 = VERTEX_POINT ( 'NONE', #132765 ) ;
#122294 =( LENGTH_UNIT ( ) NAMED_UNIT ( * ) SI_UNIT ( .MILLI., .METRE. ) );
#122295 = VERTEX_POINT ( 'NONE', #33453 ) ;
#122296 = LINE ( 'NONE', #44817, #104664 ) ;
#122297 = VERTEX_POINT ( 'NONE', #89229 ) ;
#122298 = FACE_OUTER_BOUND ( 'NONE', #11877, .T. ) ;
#122299 = CARTESIAN_POINT ( 'NONE',  ( 110.4750270504628702, -5.819803920172572198, 5.819803920172572198 ) ) ;
#122300 = FACE_OUTER_BOUND ( 'NONE', #109493, .T. ) ;
#122301 = LINE ( 'NONE', #22974, #101819 ) ;
#122302 = DIRECTION ( 'NONE',  ( 0.3543493200069162685, -0.000000000000000000, -0.9351131265310288487 ) ) ;
#122303 = DIRECTION ( 'NONE',  ( 0.7071067811865487940, 0.7071067811865463515, 0.000000000000000000 ) ) ;
#122304 = CARTESIAN_POINT ( 'NONE',  ( 12.97916666666666607, 6.094999999999988205, -1.633150327867694651 ) ) ;
#122305 = CARTESIAN_POINT ( 'NONE',  ( 24.04123647476855652, 0.000000000000000000, 7.934999999999990727 ) ) ;
#122306 = AXIS2_PLACEMENT_3D ( 'NONE', #96358, #107261, #107948 ) ;
#122307 = CARTESIAN_POINT ( 'NONE',  ( -34.92500000000001137, 3.759292476615678336, 4.255531930566252008 ) ) ;
#122308 = CARTESIAN_POINT ( 'NONE',  ( -51.18398860626899705, 28.73617430169823095, 5.000000000000000000 ) ) ;
#122309 = ORIENTED_EDGE ( 'NONE', *, *, #36454, .F. ) ;
#122311 = EDGE_LOOP ( 'NONE', ( #32351, #62120, #100611, #128490, #87151, #58891 ) ) ;
#122310 = VECTOR ( 'NONE', #114949, 1000.000000000000000 ) ;
#122312 = CARTESIAN_POINT ( 'NONE',  ( 12.51280225271498736, 3.821174125832445049E-16, 0.000000000000000000 ) ) ;
#122313 = VERTEX_POINT ( 'NONE', #133453 ) ;
#122314 = CARTESIAN_POINT ( 'NONE',  ( 90.12543019189811844, 5.291415217122919401, 3.055000000000002824 ) ) ;
#122315 = DIRECTION ( 'NONE',  ( -0.7071067811865486830, 0.7071067811865464625, 0.000000000000000000 ) ) ;
#122316 = DIRECTION ( 'NONE',  ( 0.000000000000000000, 1.000000000000000000, 0.000000000000000000 ) ) ;
#122317 = DIRECTION ( 'NONE',  ( -0.7071067811865486830, 0.7071067811865464625, 0.000000000000000000 ) ) ;
#122318 = LINE ( 'NONE', #35377, #112672 ) ;
#122319 = EDGE_LOOP ( 'NONE', ( #121099, #43183, #32368, #123940 ) ) ;
#122320 = LINE ( 'NONE', #57129, #52113 ) ;
#122321 = DIRECTION ( 'NONE',  ( 0.000000000000000000, 0.000000000000000000, 1.000000000000000000 ) ) ;
#122322 = EDGE_CURVE ( 'NONE', #114028, #84504, #34140, .T. ) ;
#122323 = LINE ( 'NONE', #36078, #129837 ) ;
#122324 = CARTESIAN_POINT ( 'NONE',  ( 0.7700427945779364514, 21.73644205237998150, 5.000000000000000888 ) ) ;
#122325 = EDGE_CURVE ( 'NONE', #96698, #107938, #15029, .T. ) ;
#122326 = EDGE_CURVE ( 'NONE', #121813, #46067, #103462, .T. ) ;
#122327 = CARTESIAN_POINT ( 'NONE',  ( 20.51078643762690490, -27.52281430457041012, 5.000000000000000000 ) ) ;
#122329 = ORIENTED_EDGE ( 'NONE', *, *, #48426, .F. ) ;
#122328 = CARTESIAN_POINT ( 'NONE',  ( -34.92500000000001137, 22.22500000000000142, 4.000000000000000000 ) ) ;
#122330 = DIRECTION ( 'NONE',  ( -0.7071067811865486830, -0.7071067811865464625, -0.000000000000000000 ) ) ;
#122331 = CARTESIAN_POINT ( 'NONE',  ( 21.00548008471250938, 28.92564299267923644, 4.000000000000000000 ) ) ;
#122332 = LINE ( 'NONE', #101319, #3012 ) ;
#122333 = DIRECTION ( 'NONE',  ( 0.5735764363510453823, -0.8191520442889923537, 1.003171929053525486E-16 ) ) ;
#122334 = DIRECTION ( 'NONE',  ( -0.3543493200069162685, -0.000000000000000000, -0.9351131265310288487 ) ) ;
#122335 = EDGE_CURVE ( 'NONE', #135502, #98260, #115034, .T. ) ;
#122337 = VERTEX_POINT ( 'NONE', #116502 ) ;
#122336 = EDGE_CURVE ( 'NONE', #92907, #120201, #38236, .T. ) ;
#122338 = ORIENTED_EDGE ( 'NONE', *, *, #73508, .F. ) ;
#122339 = ORIENTED_EDGE ( 'NONE', *, *, #142876, .T. ) ;
#122340 = CARTESIAN_POINT ( 'NONE',  ( 89.68793019189810423, 6.110000000000002984, -1.637169565754156730 ) ) ;
#122341 = ORIENTED_EDGE ( 'NONE', *, *, #66799, .F. ) ;
#122342 = EDGE_CURVE ( 'NONE', #71721, #42777, #84600, .T. ) ;
#122343 = CARTESIAN_POINT ( 'NONE',  ( -36.48921356237310221, -27.52281430457080802, 5.000000000000000000 ) ) ;
#122344 = DIRECTION ( 'NONE',  ( 0.7071067811865487940, 0.7071067811865463515, -0.000000000000000000 ) ) ;
#122345 = CARTESIAN_POINT ( 'NONE',  ( 13.64840764549667540, 2.500000000000003553, 3.061616997868386099E-16 ) ) ;
#122346 = CARTESIAN_POINT ( 'NONE',  ( 85.24586038379622721, 3.974999999999996980, 6.884901960086287964 ) ) ;
#122347 = VERTEX_POINT ( 'NONE', #93321 ) ;
#122348 = CARTESIAN_POINT ( 'NONE',  ( 39.48921356237310221, -27.52281430457082934, 5.000000000000000000 ) ) ;
#122349 = CARTESIAN_POINT ( 'NONE',  ( -32.99999999999976552, -9.412538124160658271, 4.000000000000000000 ) ) ;
#122350 = EDGE_CURVE ( 'NONE', #126030, #118230, #94717, .T. ) ;
#122351 = CARTESIAN_POINT ( 'NONE',  ( 5.816011393731002066, 28.73617430169783304, 5.000000000000000000 ) ) ;
#122352 = CARTESIAN_POINT ( 'NONE',  ( 88.28709685856478018, 3.054999999999997495, 5.291415217122919401 ) ) ;
#122353 = ORIENTED_EDGE ( 'NONE', *, *, #12008, .F. ) ;
#122354 = VECTOR ( 'NONE', #57415, 1000.000000000000227 ) ;
#122355 = LINE ( 'NONE', #55715, #48948 ) ;
#122356 = CARTESIAN_POINT ( 'NONE',  ( -12.19999999999999929, -59.76999999999998892, -39.50000000000000000 ) ) ;
#122358 = EDGE_CURVE ( 'NONE', #61548, #87797, #40394, .T. ) ;
#122357 = VECTOR ( 'NONE', #14179, 1000.000000000000227 ) ;
#122359 = AXIS2_PLACEMENT_3D ( 'NONE', #126719, #115826, #74527 ) ;
#122360 = VECTOR ( 'NONE', #138637, 1000.000000000000000 ) ;
#122361 = VERTEX_POINT ( 'NONE', #59306 ) ;
#122362 = ORIENTED_EDGE ( 'NONE', *, *, #65154, .T. ) ;
#122363 = AXIS2_PLACEMENT_3D ( 'NONE', #38083, #126483, #115575 ) ;
#122364 = DIRECTION ( 'NONE',  ( -0.7071067811865486830, -0.7071067811865464625, -0.000000000000000000 ) ) ;
#122365 = AXIS2_PLACEMENT_3D ( 'NONE', #55628, #99088, #75944 ) ;
#122366 = CARTESIAN_POINT ( 'NONE',  ( 24.27540314143521982, -2.126176841940958351, -7.934999999999988951 ) ) ;
#122367 = DIRECTION ( 'NONE',  ( -0.000000000000000000, 0.000000000000000000, 1.000000000000000000 ) ) ;
#122368 = ADVANCED_FACE ( 'NONE', ( #82457 ), #4828, .T. ) ;
#122369 = AXIS2_PLACEMENT_3D ( 'NONE', #806, #86432, #68 ) ;
#122370 = VECTOR ( 'NONE', #40830, 999.9999999999998863 ) ;
#122371 = CARTESIAN_POINT ( 'NONE',  ( 166.3107925015840749, 26.96999999999993847, 33.18280220445518580 ) ) ;
#122372 = CARTESIAN_POINT ( 'NONE',  ( 72.18398860626899705, 28.73617430169837661, 5.000000000000000000 ) ) ;
#122373 = DIRECTION ( 'NONE',  ( -0.7071067811865486830, -0.7071067811865464625, 0.000000000000000000 ) ) ;
#122374 = EDGE_LOOP ( 'NONE', ( #18043, #128653, #30076, #119139 ) ) ;
#122375 = ORIENTED_EDGE ( 'NONE', *, *, #60900, .F. ) ;
#122376 = CARTESIAN_POINT ( 'NONE',  ( -36.18398860626899705, 28.73617430169812437, 5.000000000000000000 ) ) ;
#122377 = ORIENTED_EDGE ( 'NONE', *, *, #31678, .F. ) ;
#122378 = VERTEX_POINT ( 'NONE', #61452 ) ;
#122379 = EDGE_CURVE ( 'NONE', #66916, #46533, #23816, .T. ) ;
#122380 = MECHANICAL_DESIGN_GEOMETRIC_PRESENTATION_REPRESENTATION (  '', ( #52835 ), #15757 ) ;
#122381 =( BOUNDED_CURVE ( )  B_SPLINE_CURVE ( 3, ( #113321, #80736, #2404, #90901 ),
 .UNSPECIFIED., .F., .F. ) 
 B_SPLINE_CURVE_WITH_KNOTS ( ( 4, 4 ),
 ( 5.043186909253408956, 5.074607125596330093 ),
 .UNSPECIFIED. ) 
 CURVE ( )  GEOMETRIC_REPRESENTATION_ITEM ( )  RATIONAL_B_SPLINE_CURVE ( ( 1.000000000000000000, 0.9999177325257868620, 0.9999177325257868620, 1.000000000000000000 ) ) 
 REPRESENTATION_ITEM ( '' )  );
#122382 = ADVANCED_FACE ( 'NONE', ( #48385 ), #60743, .F. ) ;
#122383 = PRESENTATION_LAYER_ASSIGNMENT (  '', '', ( #32175 ) ) ;
#122384 = CARTESIAN_POINT ( 'NONE',  ( -29.99999999999979039, 16.93112307739200872, 4.000000000000000000 ) ) ;
#122385 = ORIENTED_EDGE ( 'NONE', *, *, #137726, .T. ) ;
#122386 = LINE ( 'NONE', #67332, #71474 ) ;
#122387 = CARTESIAN_POINT ( 'NONE',  ( -65.99451991528749772, 28.92564299267984396, 4.000000000000000000 ) ) ;
#122388 = ADVANCED_FACE ( 'NONE', ( #27329 ), #71578, .F. ) ;
#122389 = LINE ( 'NONE', #130449, #33990 ) ;
#122390 = CYLINDRICAL_SURFACE ( 'NONE', #101681, 7.950000000000000178 ) ;
#122391 = CIRCLE ( 'NONE', #22822, 2.999999999999999112 ) ;
#122392 = AXIS2_PLACEMENT_3D ( 'NONE', #54462, #25902, #99335 ) ;
#122393 =( BOUNDED_CURVE ( )  B_SPLINE_CURVE ( 3, ( #16543, #81866, #106385, #93417 ),
 .UNSPECIFIED., .F., .T. ) 
 B_SPLINE_CURVE_WITH_KNOTS ( ( 4, 4 ),
 ( 5.106027341939283204, 6.645403452391245303 ),
 .UNSPECIFIED. ) 
 CURVE ( )  GEOMETRIC_REPRESENTATION_ITEM ( )  RATIONAL_B_SPLINE_CURVE ( ( 1.000000000000000000, 0.8120851936182283959, 0.8120851936182283959, 1.000000000000000000 ) ) 
 REPRESENTATION_ITEM ( '' )  );
#122394 = ORIENTED_EDGE ( 'NONE', *, *, #74947, .F. ) ;
#122396 = EDGE_CURVE ( 'NONE', #65645, #106882, #28067, .T. ) ;
#122395 = VECTOR ( 'NONE', #39618, 1000.000000000000000 ) ;
#122397 = DIRECTION ( 'NONE',  ( -0.7071067811865486830, -0.7071067811865464625, -0.000000000000000000 ) ) ;
#122398 = COLOUR_RGB ( '', 0.31764706, 0.68627451, 0.89019608) ;
#122399 = ORIENTED_EDGE ( 'NONE', *, *, #133470, .F. ) ;
#122400 = DIRECTION ( 'NONE',  ( -0.7071067811865486830, 0.7071067811865464625, 0.000000000000000000 ) ) ;
#122401 = VERTEX_POINT ( 'NONE', #139714 ) ;
#122402 = LINE ( 'NONE', #78946, #79365 ) ;
#122403 = VERTEX_POINT ( 'NONE', #16441 ) ;
#122404 = PLANE ( 'NONE',  #138546 ) ;
#122405 = ORIENTED_EDGE ( 'NONE', *, *, #57438, .T. ) ;
#122406 = ORIENTED_EDGE ( 'NONE', *, *, #101607, .T. ) ;
#122407 = VECTOR ( 'NONE', #48158, 1000.000000000000000 ) ;
#122408 = VERTEX_POINT ( 'NONE', #29474 ) ;
#122409 = VECTOR ( 'NONE', #44924, 1000.000000000000000 ) ;
#122410 = DIRECTION ( 'NONE',  ( -0.000000000000000000, 0.000000000000000000, 1.000000000000000000 ) ) ;
#122411 = CARTESIAN_POINT ( 'NONE',  ( 17.99451991528748351, 28.92564299267950645, 4.000000000000000000 ) ) ;
#122412 = CARTESIAN_POINT ( 'NONE',  ( 117.1045968585647756, 1.637169565754164946, -6.109999999999999432 ) ) ;
#122413 = FACE_OUTER_BOUND ( 'NONE', #26624, .T. ) ;
#122414 = EDGE_CURVE ( 'NONE', #63944, #128763, #62301, .T. ) ;
#122415 = DIRECTION ( 'NONE',  ( 0.7071067811865487940, 0.7071067811865463515, 0.000000000000000000 ) ) ;
#122416 = LINE ( 'NONE', #46343, #117627 ) ;
#122417 = VECTOR ( 'NONE', #70784, 1000.000000000000000 ) ;
#122418 = ADVANCED_FACE ( 'NONE', ( #42541 ), #65000, .F. ) ;
#122419 = DIRECTION ( 'NONE',  ( -0.7071067811865487940, 0.7071067811865463515, 0.000000000000000000 ) ) ;
#122420 = LINE ( 'NONE', #46346, #101508 ) ;
#122421 = ORIENTED_EDGE ( 'NONE', *, *, #142931, .T. ) ;
#122422 = DIRECTION ( 'NONE',  ( 1.000000000000000000, 0.000000000000000000, 0.000000000000000000 ) ) ;
#122423 = CARTESIAN_POINT ( 'NONE',  ( -26.67183060077628198, -6.740707523384214639, 4.000000000000000000 ) ) ;
#122424 = FACE_OUTER_BOUND ( 'NONE', #29941, .T. ) ;
#122425 = ORIENTED_EDGE ( 'NONE', *, *, #18474, .T. ) ;
#122426 = ORIENTED_EDGE ( 'NONE', *, *, #41483, .F. ) ;
#122427 = ORIENTED_EDGE ( 'NONE', *, *, #132577, .T. ) ;
#122428 = DIRECTION ( 'NONE',  ( -0.3543493200069162685, -0.000000000000000000, -0.9351131265310288487 ) ) ;
#122429 = VERTEX_POINT ( 'NONE', #64267 ) ;
#122430 = ORIENTED_EDGE ( 'NONE', *, *, #48938, .F. ) ;
#122431 = DIRECTION ( 'NONE',  ( -1.000000000000000000, 0.000000000000000000, -0.000000000000000000 ) ) ;
#122432 = CARTESIAN_POINT ( 'NONE',  ( 106.5375270504628844, -9.735942053221456900E-16, 7.949999999999998401 ) ) ;
#122433 = CARTESIAN_POINT ( 'NONE',  ( 78.18398860626899705, 28.73617430169841924, 5.000000000000000000 ) ) ;
#122434 = EDGE_CURVE ( 'NONE', #96838, #61667, #141844, .T. ) ;
#122435 = DIRECTION ( 'NONE',  ( -0.000000000000000000, 0.3543493200069153248, 0.9351131265310292928 ) ) ;
#122436 = CARTESIAN_POINT ( 'NONE',  ( -11.57672154193639003, 11.25929247661560240, 17.85071094206587361 ) ) ;
#122437 = EDGE_LOOP ( 'NONE', ( #39845, #64605, #96224, #27356 ) ) ;
#122438 = DIRECTION ( 'NONE',  ( -0.000000000000000000, -0.000000000000000000, 1.000000000000000000 ) ) ;
#122439 = ORIENTED_EDGE ( 'NONE', *, *, #54470, .F. ) ;
#122440 = CARTESIAN_POINT ( 'NONE',  ( -53.99451991528749062, 28.92564299267975869, 4.000000000000000000 ) ) ;
#122441 = EDGE_CURVE ( 'NONE', #77873, #141023, #130253, .T. ) ;
#122442 = CARTESIAN_POINT ( 'NONE',  ( 14.65040314143522338, 7.934999999999989839, -2.126176841940961904 ) ) ;
#122443 = VERTEX_POINT ( 'NONE', #118634 ) ;
#122444 = CARTESIAN_POINT ( 'NONE',  ( 86.09959685856478018, -6.109999999999998543, -1.637169565754160727 ) ) ;
#122445 = CARTESIAN_POINT ( 'NONE',  ( -3.707106781186512823, -0.7407075233842770334, 5.000000000000000000 ) ) ;
#122446 = CARTESIAN_POINT ( 'NONE',  ( 98.07919371712955581, 3.975000000000002753, -6.884901960086283523 ) ) ;
#122447 = ORIENTED_EDGE ( 'NONE', *, *, #110579, .F. ) ;
#122448 = VERTEX_POINT ( 'NONE', #86744 ) ;
#122449 = ORIENTED_EDGE ( 'NONE', *, *, #42272, .F. ) ;
#122450 = LINE ( 'NONE', #55810, #75069 ) ;
#122451 = CARTESIAN_POINT ( 'NONE',  ( 32.99451991528749062, 28.92564299267960948, 4.000000000000000000 ) ) ;
#122452 = CARTESIAN_POINT ( 'NONE',  ( 34.92499999999998295, -1.298069433179003695, 4.500000000000000888 ) ) ;
#122453 = LINE ( 'NONE', #108700, #140032 ) ;
#122454 = DIRECTION ( 'NONE',  ( 0.6830127018922180770, -0.6830127018922204085, -0.2588190451025213501 ) ) ;
#122455 = ORIENTED_EDGE ( 'NONE', *, *, #80007, .T. ) ;
#122456 = CARTESIAN_POINT ( 'NONE',  ( 14.42840764549667476, 9.139736423841732040E-16, 0.000000000000000000 ) ) ;
#122457 = EDGE_CURVE ( 'NONE', #63324, #64204, #130966, .T. ) ;
#122458 = PLANE ( 'NONE',  #69841 ) ;
#122459 = LINE ( 'NONE', #142803, #60803 ) ;
#122460 = ORIENTED_EDGE ( 'NONE', *, *, #95661, .T. ) ;
#122461 = CARTESIAN_POINT ( 'NONE',  ( 28.00000000000002487, -52.14999999999999147, -34.92499999999976978 ) ) ;
#122462 = AXIS2_PLACEMENT_3D ( 'NONE', #71434, #48242, #37377 ) ;
#122463 = VECTOR ( 'NONE', #47628, 1000.000000000000227 ) ;
#122464 = VECTOR ( 'NONE', #14126, 1000.000000000000227 ) ;
#122465 = LINE ( 'NONE', #97883, #30898 ) ;
#122466 = ORIENTED_EDGE ( 'NONE', *, *, #17599, .F. ) ;
#122468 = ORIENTED_EDGE ( 'NONE', *, *, #12357, .T. ) ;
#122467 = CARTESIAN_POINT ( 'NONE',  ( -29.67183060077626067, 17.25929247661553845, 4.000000000000000000 ) ) ;
#122469 = ORIENTED_EDGE ( 'NONE', *, *, #13274, .T. ) ;
#122470 = EDGE_CURVE ( 'NONE', #28997, #75489, #143249, .T. ) ;
#122471 = DIRECTION ( 'NONE',  ( 0.7071067811865486830, -0.7071067811865464625, -0.000000000000000000 ) ) ;
#122472 = DIRECTION ( 'NONE',  ( 0.7071067811865486830, -0.7071067811865464625, -0.000000000000000000 ) ) ;
#122473 = ORIENTED_EDGE ( 'NONE', *, *, #40898, .T. ) ;
#122474 = DIRECTION ( 'NONE',  ( 0.7071067811865487940, 0.7071067811865463515, 0.000000000000000000 ) ) ;
#122475 = CARTESIAN_POINT ( 'NONE',  ( 15.48921356237309510, -27.52281430457066236, 5.000000000000000000 ) ) ;
#122476 = DIRECTION ( 'NONE',  ( -1.000000000000000000, -0.000000000000000000, -0.000000000000000000 ) ) ;
#122477 = LINE ( 'NONE', #78291, #117893 ) ;
#122478 = CARTESIAN_POINT ( 'NONE',  ( 47.62086038379622011, -6.884901960086286188, 3.974999999999997424 ) ) ;
#122479 = LINE ( 'NONE', #111630, #76702 ) ;
#122480 = LINE ( 'NONE', #21765, #5138 ) ;
#122481 = CARTESIAN_POINT ( 'NONE',  ( 33.79289321881321939, 15.75929247661555976, 5.000000000000000000 ) ) ;
#122482 = CARTESIAN_POINT ( 'NONE',  ( 30.18398860626900060, 28.73617430169808173, 5.000000000000000000 ) ) ;
#122483 = CARTESIAN_POINT ( 'NONE',  ( 19.81206980810188156, 7.934999999999993392, 2.126176841940951689 ) ) ;
#122485 = AXIS2_PLACEMENT_3D ( 'NONE', #137668, #115858, #49242 ) ;
#122484 = DIRECTION ( 'NONE',  ( 0.7071067811865486830, -0.7071067811865464625, -0.000000000000000000 ) ) ;
#122486 = PLANE ( 'NONE',  #138568 ) ;
#122487 = VECTOR ( 'NONE', #121276, 1000.000000000000114 ) ;
#122488 = DIRECTION ( 'NONE',  ( 0.7071067811865487940, -0.7071067811865463515, 0.000000000000000000 ) ) ;
#122489 = LINE ( 'NONE', #31933, #6055 ) ;
#122490 = EDGE_LOOP ( 'NONE', ( #78891, #24363, #18564 ) ) ;
#122491 = ORIENTED_EDGE ( 'NONE', *, *, #116592, .T. ) ;
#122492 = CARTESIAN_POINT ( 'NONE',  ( 102.7916666666666714, 3.975000000000003642, -6.884901960086285300 ) ) ;
#122493 = AXIS2_PLACEMENT_3D ( 'NONE', #123458, #56058, #22639 ) ;
#122494 = VERTEX_POINT ( 'NONE', #117878 ) ;
#122495 = VERTEX_POINT ( 'NONE', #18580 ) ;
#122496 = VERTEX_POINT ( 'NONE', #99011 ) ;
#122497 = DIRECTION ( 'NONE',  ( 0.7071067811865486830, -0.7071067811865464625, -0.000000000000000000 ) ) ;
#122498 = DIRECTION ( 'NONE',  ( 0.6830127018922181881, 0.6830127018922202975, -0.2588190451025214056 ) ) ;
#122499 = CARTESIAN_POINT ( 'NONE',  ( 13.79777835071270076, 9.118581059549645929, 2.675923548408995156 ) ) ;
#122500 = VERTEX_POINT ( 'NONE', #8404 ) ;
#122501 = AXIS2_PLACEMENT_3D ( 'NONE', #50513, #94698, #128091 ) ;
#122502 = FACE_OUTER_BOUND ( 'NONE', #69917, .T. ) ;
#122504 = EDGE_CURVE ( 'NONE', #88783, #69001, #68769, .T. ) ;
#122503 = CIRCLE ( 'NONE', #94754, 2.500000000000000444 ) ;
#122505 = CARTESIAN_POINT ( 'NONE',  ( -9.119999999999999218, 0.000000000000000000, -10.00000000000000000 ) ) ;
#122506 = AXIS2_PLACEMENT_3D ( 'NONE', #62071, #29407, #41724 ) ;
#122507 = CARTESIAN_POINT ( 'NONE',  ( -17.11087965568911073, 8.820243421702873121, 4.000000000000000000 ) ) ;
#122508 = CARTESIAN_POINT ( 'NONE',  ( -51.48921356237309510, -27.52281430457091460, 5.000000000000000000 ) ) ;
#122509 = EDGE_LOOP ( 'NONE', ( #66072, #112770, #91092, #139062 ) ) ;
#122510 = EDGE_CURVE ( 'NONE', #29342, #95787, #89486, .T. ) ;
#122511 = EDGE_CURVE ( 'NONE', #31472, #95905, #40959, .T. ) ;
#122512 = DIRECTION ( 'NONE',  ( 0.7071067811865487940, -0.7071067811865463515, 0.000000000000000000 ) ) ;
#122513 = DIRECTION ( 'NONE',  ( -0.000000000000000000, 0.000000000000000000, 1.000000000000000000 ) ) ;
#122514 = VECTOR ( 'NONE', #59260, 1000.000000000000000 ) ;
#122515 = CARTESIAN_POINT ( 'NONE',  ( -34.92499999999999716, 22.26999999999998181, -14.71147562388301822 ) ) ;
#122516 = CARTESIAN_POINT ( 'NONE',  ( 42.18398860626899705, 28.73617430169816700, 5.000000000000000000 ) ) ;
#122517 = CARTESIAN_POINT ( 'NONE',  ( -18.18398860626898994, 28.73617430169800002, 5.000000000000000000 ) ) ;
#122518 = VECTOR ( 'NONE', #32056, 999.9999999999998863 ) ;
#122519 = CARTESIAN_POINT ( 'NONE',  ( 85.53752705046288440, -9.735942053221456900E-16, 7.949999999999998401 ) ) ;
#122520 = CARTESIAN_POINT ( 'NONE',  ( 10.52840764549667618, 9.139736423841732040E-16, 0.000000000000000000 ) ) ;
#122521 = ADVANCED_FACE ( 'NONE', ( #141087 ), #41079, .F. ) ;
#122522 = EDGE_CURVE ( 'NONE', #25072, #93715, #51971, .T. ) ;
#122523 = EDGE_LOOP ( 'NONE', ( #45448, #36001, #5877, #74403 ) ) ;
#122524 = ORIENTED_EDGE ( 'NONE', *, *, #52236, .F. ) ;
#122525 = CARTESIAN_POINT ( 'NONE',  ( 116.2295968585647756, -6.110000000000000320, -1.637169565754161393 ) ) ;
#122526 = EDGE_CURVE ( 'NONE', #130061, #140080, #10567, .T. ) ;
#122527 = VERTEX_POINT ( 'NONE', #41801 ) ;
#122528 = EDGE_CURVE ( 'NONE', #123836, #50567, #120770, .T. ) ;
#122529 = DIRECTION ( 'NONE',  ( -0.7071067811865487940, 0.7071067811865463515, 0.000000000000000000 ) ) ;
#122530 = EDGE_CURVE ( 'NONE', #58012, #41530, #43241, .T. ) ;
#122531 = CARTESIAN_POINT ( 'NONE',  ( 24.39999999999999858, 1.126161369193133366, -16.41140641659140798 ) ) ;
#122532 = CARTESIAN_POINT ( 'NONE',  ( 0.000000000000000000, 4.931123077392136622, 4.000000000000000000 ) ) ;
#122533 = DIRECTION ( 'NONE',  ( 0.000000000000000000, 0.000000000000000000, 1.000000000000000000 ) ) ;
#122534 = ADVANCED_FACE ( 'NONE', ( #75172 ), #20019, .T. ) ;
#122535 = CARTESIAN_POINT ( 'NONE',  ( 116.1412635252314374, 4.472830434245836706, 4.472830434245840259 ) ) ;
#122536 = ORIENTED_EDGE ( 'NONE', *, *, #50931, .T. ) ;
#122537 = ORIENTED_EDGE ( 'NONE', *, *, #53861, .F. ) ;
#122538 = CARTESIAN_POINT ( 'NONE',  ( 0.2997448713915885632, -27.71228299555206220, 4.000000000000000000 ) ) ;
#122539 = CARTESIAN_POINT ( 'NONE',  ( 98.56250000000000000, -5.819803920172573086, -5.819803920172573974 ) ) ;
#122540 = EDGE_CURVE ( 'NONE', #74817, #88053, #53380, .T. ) ;
#122541 = VERTEX_POINT ( 'NONE', #9871 ) ;
#122542 = ORIENTED_EDGE ( 'NONE', *, *, #52776, .F. ) ;
#122543 = CARTESIAN_POINT ( 'NONE',  ( 38.64626352523144703, -4.472830434245840259, 4.472830434245839371 ) ) ;
#122544 = EDGE_LOOP ( 'NONE', ( #42098, #55199, #117189, #20380 ) ) ;
#122545 = DIRECTION ( 'NONE',  ( 0.000000000000000000, 1.000000000000000000, 0.000000000000000000 ) ) ;
#122546 = EDGE_CURVE ( 'NONE', #87653, #121, #98332, .T. ) ;
#122547 = CARTESIAN_POINT ( 'NONE',  ( 31.70376352523145158, 6.109999999999998543, 1.122388791418548911E-15 ) ) ;
#122548 = ORIENTED_EDGE ( 'NONE', *, *, #92956, .F. ) ;
#122549 = DIRECTION ( 'NONE',  ( -0.7071067811865486830, -0.7071067811865464625, -0.000000000000000000 ) ) ;
#122550 = ORIENTED_EDGE ( 'NONE', *, *, #30309, .F. ) ;
#122551 = ORIENTED_EDGE ( 'NONE', *, *, #119597, .T. ) ;
#122552 = ORIENTED_EDGE ( 'NONE', *, *, #42389, .T. ) ;
#122553 = ADVANCED_FACE ( 'NONE', ( #58439 ), #78711, .F. ) ;
#122554 = CARTESIAN_POINT ( 'NONE',  ( 7.139999999999985469, -40.06159979880239064, 18.96849477799998596 ) ) ;
#122555 = LINE ( 'NONE', #34875, #48830 ) ;
#122556 = EDGE_LOOP ( 'NONE', ( #129189, #102435, #128278, #123503 ) ) ;
#122557 = LINE ( 'NONE', #67516, #115400 ) ;
#122558 = EDGE_CURVE ( 'NONE', #117128, #13716, #80165, .T. ) ;
#122559 = AXIS2_PLACEMENT_3D ( 'NONE', #105602, #138265, #139722 ) ;
#122560 = DIRECTION ( 'NONE',  ( -0.7071067811865486830, -0.7071067811865464625, 0.000000000000000000 ) ) ;
#122561 = DIRECTION ( 'NONE',  ( 0.000000000000000000, 0.000000000000000000, 1.000000000000000000 ) ) ;
#122562 = VECTOR ( 'NONE', #135818, 999.9999999999998863 ) ;
#122563 = AXIS2_PLACEMENT_3D ( 'NONE', #44614, #135862, #78629 ) ;
#122564 = AXIS2_PLACEMENT_3D ( 'NONE', #120452, #30656, #42251 ) ;
#122565 = ADVANCED_FACE ( 'NONE', ( #23607 ), #22159, .F. ) ;
#122566 = CARTESIAN_POINT ( 'NONE',  ( -30.48921356237309510, -27.52281430457076894, 5.000000000000000000 ) ) ;
#122567 = CIRCLE ( 'NONE', #20640, 2.500000000000000444 ) ;
#122568 = FACE_BOUND ( 'NONE', #108518, .T. ) ;
#122569 = EDGE_LOOP ( 'NONE', ( #89255, #55807, #9762, #87627 ) ) ;
#122570 = CARTESIAN_POINT ( 'NONE',  ( -15.08491323193753075, -12.74070752338414891, 18.74364270924350606 ) ) ;
#122571 = CARTESIAN_POINT ( 'NONE',  ( -26.99999999999981171, -21.03360074219752462, 5.000000000000000000 ) ) ;
#122572 = CARTESIAN_POINT ( 'NONE',  ( -12.69999999999998153, -0.3999999999999997446, -2.467792535850613866 ) ) ;
#122573 = CARTESIAN_POINT ( 'NONE',  ( -12.48921356237309155, -27.52281430457064104, 5.000000000000000000 ) ) ;
#122574 = ORIENTED_EDGE ( 'NONE', *, *, #13671, .F. ) ;
#122575 = DIRECTION ( 'NONE',  ( -0.000000000000000000, 0.000000000000000000, 1.000000000000000000 ) ) ;
#122576 = ORIENTED_EDGE ( 'NONE', *, *, #64594, .T. ) ;
#122577 = ORIENTED_EDGE ( 'NONE', *, *, #125814, .F. ) ;
#122578 = VECTOR ( 'NONE', #112344, 1000.000000000000000 ) ;
#122579 = EDGE_CURVE ( 'NONE', #77421, #100584, #91039, .T. ) ;
#122580 = EDGE_LOOP ( 'NONE', ( #35028, #21164, #75658, #16851 ) ) ;
#122581 = CARTESIAN_POINT ( 'NONE',  ( 47.45376352523145158, -6.109999999999998543, -3.741295971395162543E-16 ) ) ;
#122582 = ORIENTED_EDGE ( 'NONE', *, *, #16201, .F. ) ;
#122583 = AXIS2_PLACEMENT_3D ( 'NONE', #41511, #42262, #96574 ) ;
#122584 = PLANE ( 'NONE',  #67259 ) ;
#122585 = FACE_OUTER_BOUND ( 'NONE', #52210, .T. ) ;
#122586 = EDGE_CURVE ( 'NONE', #28861, #126820, #91907, .T. ) ;
#122587 = ORIENTED_EDGE ( 'NONE', *, *, #66644, .F. ) ;
#122588 = LINE ( 'NONE', #110274, #12080 ) ;
#122589 = PLANE ( 'NONE',  #48140 ) ;
#122590 = CIRCLE ( 'NONE', #50793, 2.500000000000000888 ) ;
#122591 = VECTOR ( 'NONE', #20395, 1000.000000000000000 ) ;
#122592 = VECTOR ( 'NONE', #72308, 1000.000000000000000 ) ;
#122593 = DIRECTION ( 'NONE',  ( 0.000000000000000000, 0.000000000000000000, 1.000000000000000000 ) ) ;
#122594 = DIRECTION ( 'NONE',  ( -0.3543493200069162685, -0.000000000000000000, -0.9351131265310288487 ) ) ;
#122596 = EDGE_CURVE ( 'NONE', #4187, #78485, #1121, .T. ) ;
#122595 = CARTESIAN_POINT ( 'NONE',  ( -36.29974487139159578, -27.71228299555231445, 4.000000000000000000 ) ) ;
#122597 = LINE ( 'NONE', #13815, #7680 ) ;
#122598 = ORIENTED_EDGE ( 'NONE', *, *, #65967, .F. ) ;
#122599 = ORIENTED_EDGE ( 'NONE', *, *, #26163, .T. ) ;
#122600 = ORIENTED_EDGE ( 'NONE', *, *, #28466, .T. ) ;
#122601 = ORIENTED_EDGE ( 'NONE', *, *, #41684, .T. ) ;
#122602 = CIRCLE ( 'NONE', #34672, 2.500000000000000444 ) ;
#122603 = CARTESIAN_POINT ( 'NONE',  ( 16.49999999999988987, -4.533600742197687161, 5.000000000000000000 ) ) ;
#122604 = LINE ( 'NONE', #109595, #430 ) ;
#122605 = ORIENTED_EDGE ( 'NONE', *, *, #10947, .F. ) ;
#122606 = VECTOR ( 'NONE', #31404, 1000.000000000000000 ) ;
#122607 = AXIS2_PLACEMENT_3D ( 'NONE', #5131, #38519, #7283 ) ;
#122608 = EDGE_LOOP ( 'NONE', ( #4264, #54504, #99961, #100037 ) ) ;
#122609 = CARTESIAN_POINT ( 'NONE',  ( 161.1275701981784039, 26.96999999999993491, -34.89911187425553862 ) ) ;
#122610 = CARTESIAN_POINT ( 'NONE',  ( 31.49999999999978684, -19.53360074219753884, 5.000000000000000000 ) ) ;
#122611 = EDGE_CURVE ( 'NONE', #81705, #50033, #67124, .T. ) ;
#122612 = CARTESIAN_POINT ( 'NONE',  ( -34.92500000000001137, 22.22500000000000142, 4.000000000000000000 ) ) ;
#122613 = EDGE_LOOP ( 'NONE', ( #63892, #57117, #128900, #131732 ) ) ;
#122614 = AXIS2_PLACEMENT_3D ( 'NONE', #80125, #1076, #24284 ) ;
#122615 = CARTESIAN_POINT ( 'NONE',  ( -63.48921356237309510, -27.52281430457099631, 5.000000000000000000 ) ) ;
#122616 = FACE_OUTER_BOUND ( 'NONE', #16707, .T. ) ;
#122617 = EDGE_CURVE ( 'NONE', #100722, #131560, #79478, .T. ) ;
#122618 = CARTESIAN_POINT ( 'NONE',  ( 32.29623647476855552, 7.934999999999990727, -1.457635852685135314E-15 ) ) ;
#122619 = DIRECTION ( 'NONE',  ( 0.7071067811865486830, -0.7071067811865464625, -0.000000000000000000 ) ) ;
#122620 = ORIENTED_EDGE ( 'NONE', *, *, #83255, .T. ) ;
#122622 = CARTESIAN_POINT ( 'NONE',  ( 30.18398860626900060, 28.73617430169808173, 5.000000000000000000 ) ) ;
#122621 = CARTESIAN_POINT ( 'NONE',  ( 113.6620968585647944, -5.291415217122919401, 3.054999999999998384 ) ) ;
#122623 = LINE ( 'NONE', #58138, #18769 ) ;
#122624 = DIRECTION ( 'NONE',  ( 0.3543493200069162685, -0.000000000000000000, -0.9351131265310288487 ) ) ;
#122625 = DIRECTION ( 'NONE',  ( 0.7071067811865486830, -0.7071067811865464625, -0.000000000000000000 ) ) ;
#122626 = AXIS2_PLACEMENT_3D ( 'NONE', #131867, #53597, #87637 ) ;
#122628 = ORIENTED_EDGE ( 'NONE', *, *, #37304, .T. ) ;
#122627 = CARTESIAN_POINT ( 'NONE',  ( -8.671830600776411657, 14.25929247661557220, 4.000000000000000000 ) ) ;
#122629 = LINE ( 'NONE', #79901, #27682 ) ;
#122630 = VERTEX_POINT ( 'NONE', #123670 ) ;
#122631 = LINE ( 'NONE', #121202, #82188 ) ;
#122632 = DIRECTION ( 'NONE',  ( -0.000000000000000000, 0.000000000000000000, 1.000000000000000000 ) ) ;
#122633 = LINE ( 'NONE', #2254, #95796 ) ;
#122635 = EDGE_CURVE ( 'NONE', #39039, #90401, #110591, .T. ) ;
#122634 = ORIENTED_EDGE ( 'NONE', *, *, #78831, .F. ) ;
#122636 = CARTESIAN_POINT ( 'NONE',  ( 0.000000000000000000, 0.000000000000000000, 5.000000000000000000 ) ) ;
#122637 = EDGE_CURVE ( 'NONE', #121702, #49011, #121538, .T. ) ;
#122638 = ADVANCED_BREP_SHAPE_REPRESENTATION ( '', ( #46908, #127880 ), #114089 ) ;
#122639 = DIRECTION ( 'NONE',  ( -0.000000000000000000, 0.3543493200069153248, 0.9351131265310292928 ) ) ;
#122640 = DIRECTION ( 'NONE',  ( -0.000000000000000000, 0.3543493200069153248, 0.9351131265310292928 ) ) ;
#122641 = EDGE_LOOP ( 'NONE', ( #62292, #109858, #36976, #55022 ) ) ;
#122642 = LINE ( 'NONE', #111785, #107124 ) ;
#122643 = ORIENTED_EDGE ( 'NONE', *, *, #111613, .T. ) ;
#122644 = LINE ( 'NONE', #45837, #71637 ) ;
#122646 = ORIENTED_EDGE ( 'NONE', *, *, #118800, .T. ) ;
#122645 = DIRECTION ( 'NONE',  ( 0.7071067811865487940, 0.7071067811865463515, 0.000000000000000000 ) ) ;
#122647 = EDGE_CURVE ( 'NONE', #49545, #70705, #69276, .T. ) ;
#122648 = ORIENTED_EDGE ( 'NONE', *, *, #140154, .F. ) ;
#122649 = CARTESIAN_POINT ( 'NONE',  ( 10.87659042482644800, 10.89112078991403898, -26.37954615677881520 ) ) ;
#122650 = PRESENTATION_STYLE_ASSIGNMENT (( #35698 ) ) ;
#122651 = EDGE_LOOP ( 'NONE', ( #79428, #11520, #23848, #7991 ) ) ;
#122652 = CARTESIAN_POINT ( 'NONE',  ( 21.00548008471250938, 28.92564299267923644, 4.000000000000000000 ) ) ;
#122653 = LINE ( 'NONE', #105878, #29859 ) ;
#122654 = DIRECTION ( 'NONE',  ( 1.000000000000000000, 1.224606353822377258E-16, 0.000000000000000000 ) ) ;
#122655 = VERTEX_POINT ( 'NONE', #14148 ) ;
#122656 = CARTESIAN_POINT ( 'NONE',  ( 31.82816939922330235, 15.75929247661555799, 4.000000000000000000 ) ) ;
#122657 = CARTESIAN_POINT ( 'NONE',  ( 39.48921356237310221, -27.52281430457082934, 5.000000000000000000 ) ) ;
#122658 = CARTESIAN_POINT ( 'NONE',  ( 31.92500000000001492, -6.269999999999992468, -37.00000000000000000 ) ) ;
#122659 = DIRECTION ( 'NONE',  ( 0.6830127018922181881, 0.6830127018922202975, -0.2588190451025214056 ) ) ;
#122660 = CARTESIAN_POINT ( 'NONE',  ( 32.87043019189811588, -3.055000000000001936, 5.291415217122918513 ) ) ;
#122661 = CARTESIAN_POINT ( 'NONE',  ( -5.999999999999955591, 16.55218569542900298, 5.000000000000000000 ) ) ;
#122662 = ORIENTED_EDGE ( 'NONE', *, *, #3843, .F. ) ;
#122663 = EDGE_LOOP ( 'NONE', ( #135981, #36677, #87241, #16182, #8235, #142732 ) ) ;
#122664 = DIRECTION ( 'NONE',  ( -0.7071067811865487940, 0.7071067811865463515, -0.000000000000000000 ) ) ;
#122665 = AXIS2_PLACEMENT_3D ( 'NONE', #80935, #24392, #59208 ) ;
#122666 = ORIENTED_EDGE ( 'NONE', *, *, #135362, .F. ) ;
#122667 = ORIENTED_EDGE ( 'NONE', *, *, #107653, .F. ) ;
#122668 = ORIENTED_EDGE ( 'NONE', *, *, #8599, .F. ) ;
#122669 = CARTESIAN_POINT ( 'NONE',  ( 0.6598099656846050376, -7.271130854732376747, -1.582424676226277249 ) ) ;
#122670 = LINE ( 'NONE', #69776, #115729 ) ;
#122671 = VECTOR ( 'NONE', #79881, 1000.000000000000000 ) ;
#122672 = AXIS2_PLACEMENT_3D ( 'NONE', #114936, #104073, #4729 ) ;
#122673 = PRESENTATION_LAYER_ASSIGNMENT (  '', '', ( #108784 ) ) ;
#122674 = VERTEX_POINT ( 'NONE', #89575 ) ;
#122675 = LINE ( 'NONE', #90797, #67062 ) ;
#122676 = CARTESIAN_POINT ( 'NONE',  ( 18.48921356237309510, -27.52281430457068367, 5.000000000000000000 ) ) ;
#122677 = COLOUR_RGB ( '', 0.08235294, 0.09019608, 0.10196078) ;
#122678 = CARTESIAN_POINT ( 'NONE',  ( 2.999999999999978240, -13.06887692260767864, 4.000000000000000000 ) ) ;
#122679 = CARTESIAN_POINT ( 'NONE',  ( 0.005480084712502889671, 28.92564299267938210, 4.000000000000000000 ) ) ;
#122680 = CARTESIAN_POINT ( 'NONE',  ( 122.9379301918981042, -6.110000000000001208, 1.637169565754158951 ) ) ;
#122681 = ORIENTED_EDGE ( 'NONE', *, *, #48962, .F. ) ;
#122682 = CARTESIAN_POINT ( 'NONE',  ( -8.292893218813397027, 8.259292476615632594, 5.000000000000000000 ) ) ;
#122683 = DIRECTION ( 'NONE',  ( -0.7071067811865487940, 0.7071067811865463515, 0.000000000000000000 ) ) ;
#122684 = DIRECTION ( 'NONE',  ( -0.6830127018922180770, -0.6830127018922204085, -0.2588190451025213501 ) ) ;
#122685 = AXIS2_PLACEMENT_3D ( 'NONE', #100421, #46058, #1068 ) ;
#122686 = CARTESIAN_POINT ( 'NONE',  ( 0.5657828326232884342, 7.338134074686143649, -1.735840177847257859 ) ) ;
#122687 = DIRECTION ( 'NONE',  ( -0.7071067811865486830, -0.7071067811865464625, 0.000000000000000000 ) ) ;
#122688 = LINE ( 'NONE', #11043, #65364 ) ;
#122689 = CARTESIAN_POINT ( 'NONE',  ( 2.816011393730999401, 28.73617430169785436, 5.000000000000000000 ) ) ;
#122690 = CARTESIAN_POINT ( 'NONE',  ( 44.26669371712954870, -7.949999999999999289, 2.130196079827424427 ) ) ;
#122691 = CARTESIAN_POINT ( 'NONE',  ( 22.49999999999984368, 11.52377502935405040, -1.522421517564136906 ) ) ;
#122692 = EDGE_CURVE ( 'NONE', #21837, #103874, #99737, .T. ) ;
#122693 = CARTESIAN_POINT ( 'NONE',  ( -20.70822291016940397, -15.74070752338411694, 19.73771281079092788 ) ) ;
#122694 = EDGE_LOOP ( 'NONE', ( #127145, #109717, #32646, #102699 ) ) ;
#122695 = ORIENTED_EDGE ( 'NONE', *, *, #88593, .F. ) ;
#122696 = CARTESIAN_POINT ( 'NONE',  ( 43.29166666666665719, 3.975000000000003642, -6.884901960086285300 ) ) ;
#122697 = ADVANCED_FACE ( 'NONE', ( #406 ), #88896, .F. ) ;
#122698 = CARTESIAN_POINT ( 'NONE',  ( 20.20519093902540320, -2.500000000000000444, 3.061616997868384127E-16 ) ) ;
#122699 = ADVANCED_FACE ( 'NONE', ( #34492 ), #80868, .T. ) ;
#122700 = AXIS2_PLACEMENT_3D ( 'NONE', #121245, #141593, #96603 ) ;
#122701 = VECTOR ( 'NONE', #141492, 1000.000000000000000 ) ;
#122702 = CARTESIAN_POINT ( 'NONE',  ( -5.994519915287488843, 28.92564299267942118, 4.000000000000000000 ) ) ;
#122703 = ORIENTED_EDGE ( 'NONE', *, *, #98152, .F. ) ;
#122704 = ADVANCED_FACE ( 'NONE', ( #114866 ), #52637, .T. ) ;
#122705 = CARTESIAN_POINT ( 'NONE',  ( -0.6634328256669722590, -1.145317346870745823, 3.945267063586698875 ) ) ;
#122706 = CARTESIAN_POINT ( 'NONE',  ( 11.93159235450332112, 9.902892378096218942E-16, 0.000000000000000000 ) ) ;
#122707 = VECTOR ( 'NONE', #122899, 1000.000000000000227 ) ;
#122708 = CARTESIAN_POINT ( 'NONE',  ( 38.93793019189809002, -6.110000000000001208, 1.637169565754158951 ) ) ;
#122710 = EDGE_CURVE ( 'NONE', #23067, #93995, #49680, .T. ) ;
#122709 = ORIENTED_EDGE ( 'NONE', *, *, #70849, .F. ) ;
#122711 = VECTOR ( 'NONE', #95221, 1000.000000000000000 ) ;
#122712 = CARTESIAN_POINT ( 'NONE',  ( 41.99451991528749062, 28.92564299267967343, 4.000000000000000000 ) ) ;
#122713 = VERTEX_POINT ( 'NONE', #138816 ) ;
#122714 = ORIENTED_EDGE ( 'NONE', *, *, #118983, .T. ) ;
#122715 = CARTESIAN_POINT ( 'NONE',  ( 2.301729841053981485, 3.821174125832445049E-16, 0.000000000000000000 ) ) ;
#122716 = VECTOR ( 'NONE', #117325, 1000.000000000000000 ) ;
#122717 = CARTESIAN_POINT ( 'NONE',  ( 27.48921356237309155, -27.52281430457074762, 5.000000000000000000 ) ) ;
#122718 = DIRECTION ( 'NONE',  ( 0.7071067811865487940, 0.7071067811865463515, 0.000000000000000000 ) ) ;
#122719 = EDGE_CURVE ( 'NONE', #89577, #85868, #37354, .T. ) ;
#122720 = LINE ( 'NONE', #113263, #67149 ) ;
#122721 = ORIENTED_EDGE ( 'NONE', *, *, #5017, .T. ) ;
#122722 = ADVANCED_FACE ( 'NONE', ( #81590 ), #39506, .T. ) ;
#122723 = CARTESIAN_POINT ( 'NONE',  ( 2.139447441471316935, 2.500000000000000888, 0.000000000000000000 ) ) ;
#122724 = VERTEX_POINT ( 'NONE', #125057 ) ;
#122725 = VECTOR ( 'NONE', #60231, 1000.000000000000000 ) ;
#122726 = DIRECTION ( 'NONE',  ( -0.7071067811865486830, -0.7071067811865464625, 0.000000000000000000 ) ) ;
#122727 = DIRECTION ( 'NONE',  ( -0.7071067811865487940, 0.7071067811865463515, -0.000000000000000000 ) ) ;
#122728 = CARTESIAN_POINT ( 'NONE',  ( -9.489213562373095101, -27.52281430457062328, 5.000000000000000000 ) ) ;
#122729 = DIRECTION ( 'NONE',  ( -1.000000000000000000, -0.000000000000000000, -0.000000000000000000 ) ) ;
#122730 = VECTOR ( 'NONE', #136432, 1000.000000000000000 ) ;
#122731 = DIRECTION ( 'NONE',  ( -0.7071067811865487940, 0.7071067811865463515, -0.000000000000000000 ) ) ;
#122732 = EDGE_CURVE ( 'NONE', #116147, #7244, #105032, .T. ) ;
#122733 = ORIENTED_EDGE ( 'NONE', *, *, #18342, .F. ) ;
#122734 = VECTOR ( 'NONE', #70730, 1000.000000000000000 ) ;
#122735 = CARTESIAN_POINT ( 'NONE',  ( 0.09667064187405399744, -2.240707523384260824, 15.26439735382752616 ) ) ;
#122736 = CARTESIAN_POINT ( 'NONE',  ( 59.84959685856477307, 6.109999999999996767, 1.637169565754163836 ) ) ;
#122737 = DIRECTION ( 'NONE',  ( -0.7071067811865486830, -0.7071067811865464625, -0.000000000000000000 ) ) ;
#122738 = PLANE ( 'NONE',  #82563 ) ;
#122739 = DIRECTION ( 'NONE',  ( -1.000000000000000000, -0.000000000000000000, -0.000000000000000000 ) ) ;
#122740 = ORIENTED_EDGE ( 'NONE', *, *, #56358, .T. ) ;
#122741 = AXIS2_PLACEMENT_3D ( 'NONE', #43005, #12488, #98775 ) ;
#122742 = CARTESIAN_POINT ( 'NONE',  ( 1.516262732464673579, -0.3999999999999997446, -2.467792535850613866 ) ) ;
#122743 = ORIENTED_EDGE ( 'NONE', *, *, #101040, .F. ) ;
#122744 = CARTESIAN_POINT ( 'NONE',  ( 34.74723349734966149, 22.27000000000000313, -10.47243126915188860 ) ) ;
#122745 = ORIENTED_EDGE ( 'NONE', *, *, #67446, .T. ) ;
#122746 = DIRECTION ( 'NONE',  ( -1.000000000000000000, -0.000000000000000000, -0.000000000000000000 ) ) ;
#122747 = CARTESIAN_POINT ( 'NONE',  ( 24.48921356237309510, -27.52281430457072631, 5.000000000000000000 ) ) ;
#122748 = EDGE_CURVE ( 'NONE', #15589, #52339, #133684, .T. ) ;
#122749 = DIRECTION ( 'NONE',  ( -0.7071067811865486830, 0.7071067811865464625, 0.000000000000000000 ) ) ;
#122750 = VECTOR ( 'NONE', #51676, 1000.000000000000000 ) ;
#122751 = DIRECTION ( 'NONE',  ( -0.7071067811865486830, 0.7071067811865464625, 0.000000000000000000 ) ) ;
#122752 = FACE_BOUND ( 'NONE', #72538, .T. ) ;
#122753 = CARTESIAN_POINT ( 'NONE',  ( -1.446650576632166452, 2.259292476615694323, 14.86850063742354777 ) ) ;
#122754 = DIRECTION ( 'NONE',  ( 0.7071067811865487940, -0.7071067811865463515, 0.000000000000000000 ) ) ;
#122755 = DIRECTION ( 'NONE',  ( -0.7071067811865486830, 0.7071067811865464625, 0.000000000000000000 ) ) ;
#122757 = ORIENTED_EDGE ( 'NONE', *, *, #125500, .F. ) ;
#122756 = DIRECTION ( 'NONE',  ( 0.7071067811865486830, -0.7071067811865464625, -0.000000000000000000 ) ) ;
#122758 = VECTOR ( 'NONE', #54771, 1000.000000000000000 ) ;
#122759 = DIRECTION ( 'NONE',  ( -1.000000000000000000, -1.224606353822377258E-16, -0.000000000000000000 ) ) ;
#122760 = EDGE_LOOP ( 'NONE', ( #134989, #119365, #38941, #105144 ) ) ;
#122761 = EDGE_LOOP ( 'NONE', ( #71065, #81123, #130908, #139156 ) ) ;
#122762 = CARTESIAN_POINT ( 'NONE',  ( 71.22459685856478018, -1.637169565754160949, 6.109999999999997655 ) ) ;
#122763 = ORIENTED_EDGE ( 'NONE', *, *, #109675, .T. ) ;
#122764 = CARTESIAN_POINT ( 'NONE',  ( -8.510786437626906675, -27.52281430457049183, 5.000000000000000000 ) ) ;
#122765 = DIRECTION ( 'NONE',  ( 0.000000000000000000, -1.000000000000000000, 0.000000000000000000 ) ) ;
#122766 = ADVANCED_FACE ( 'NONE', ( #135937 ), #127195, .F. ) ;
#122767 = ORIENTED_EDGE ( 'NONE', *, *, #61997, .F. ) ;
#122768 = DIRECTION ( 'NONE',  ( -0.6830127018922180770, -0.6830127018922204085, -0.2588190451025213501 ) ) ;
#122769 = AXIS2_PLACEMENT_3D ( 'NONE', #142634, #31730, #89671 ) ;
#122770 = CARTESIAN_POINT ( 'NONE',  ( 123.2083333333333428, -3.974999999999999201, -6.884901960086287964 ) ) ;
#122771 = VECTOR ( 'NONE', #80579, 1000.000000000000000 ) ;
#122772 = AXIS2_PLACEMENT_3D ( 'NONE', #47620, #80235, #90360 ) ;
#122773 = CARTESIAN_POINT ( 'NONE',  ( 3.793339364578457662, 21.75929247661549937, 4.998822639870711626 ) ) ;
#122774 = ADVANCED_FACE ( 'NONE', ( #25747 ), #59825, .T. ) ;
#122775 = DIRECTION ( 'NONE',  ( -0.000000000000000000, -0.000000000000000000, -1.000000000000000000 ) ) ;
#122777 =( NAMED_UNIT ( * ) PLANE_ANGLE_UNIT ( ) SI_UNIT ( $, .RADIAN. ) );
#122776 = DIRECTION ( 'NONE',  ( 1.000000000000000000, 1.224606353822377258E-16, 0.000000000000000000 ) ) ;
#122778 = CARTESIAN_POINT ( 'NONE',  ( -12.69999999999998153, 0.000000000000000000, 0.000000000000000000 ) ) ;
#122779 = DIRECTION ( 'NONE',  ( 0.7071067811865487940, 0.7071067811865463515, 0.000000000000000000 ) ) ;
#122781 = EDGE_LOOP ( 'NONE', ( #21521, #20408, #43881, #3596 ) ) ;
#122780 = VECTOR ( 'NONE', #140734, 999.9999999999998863 ) ;
#122782 = VECTOR ( 'NONE', #67775, 1000.000000000000000 ) ;
#122783 = CIRCLE ( 'NONE', #4649, 2.055000000000001048 ) ;
#122784 = CIRCLE ( 'NONE', #58055, 2.500000000000000888 ) ;
#122785 = ORIENTED_EDGE ( 'NONE', *, *, #104489, .F. ) ;
#122786 = AXIS2_PLACEMENT_3D ( 'NONE', #97194, #61777, #95081 ) ;
#122787 = DIRECTION ( 'NONE',  ( 0.7071067811865487940, 0.7071067811865463515, -0.000000000000000000 ) ) ;
#122788 = CARTESIAN_POINT ( 'NONE',  ( -8.816011393731004731, 28.73617430169781173, 5.000000000000000000 ) ) ;
#122789 = ORIENTED_EDGE ( 'NONE', *, *, #98378, .T. ) ;
#122790 = VECTOR ( 'NONE', #52019, 1000.000000000000000 ) ;
#122791 = VERTEX_POINT ( 'NONE', #70015 ) ;
#122792 = ORIENTED_EDGE ( 'NONE', *, *, #48739, .T. ) ;
#122793 = EDGE_CURVE ( 'NONE', #131487, #122496, #114182, .T. ) ;
#122794 = EDGE_CURVE ( 'NONE', #79126, #112433, #48952, .T. ) ;
#122795 = CARTESIAN_POINT ( 'NONE',  ( 30.77126352523143638, 4.472830434245838482, 4.472830434245842035 ) ) ;
#122796 = ORIENTED_EDGE ( 'NONE', *, *, #1610, .T. ) ;
#122797 = VECTOR ( 'NONE', #91136, 999.9999999999998863 ) ;
#122798 = LINE ( 'NONE', #132282, #78787 ) ;
#122799 = SURFACE_STYLE_FILL_AREA ( #133686 ) ;
#122800 = CARTESIAN_POINT ( 'NONE',  ( 30.96247294953710494, -7.464222240803106570E-16, -6.094999999999989981 ) ) ;
#122801 = CARTESIAN_POINT ( 'NONE',  ( 16.15294014157827718, 1.820683936599848396, -33.22430742917087088 ) ) ;
#122802 = EDGE_LOOP ( 'NONE', ( #36678, #31198, #97630, #75360 ) ) ;
#122803 = DIRECTION ( 'NONE',  ( 1.000000000000000000, 1.224606353822377258E-16, 0.000000000000000000 ) ) ;
#122804 = CARTESIAN_POINT ( 'NONE',  ( -31.78678096696621580, 12.75929247661558641, 10.29404684609028209 ) ) ;
#122805 = VECTOR ( 'NONE', #131085, 999.9999999999998863 ) ;
#122806 = CARTESIAN_POINT ( 'NONE',  ( -60.18398860626900415, 28.73617430169829490, 5.000000000000000000 ) ) ;
#122808 = EDGE_LOOP ( 'NONE', ( #85462, #59196, #96604, #39051 ) ) ;
#122807 = DIRECTION ( 'NONE',  ( 0.000000000000000000, -0.3543493200069152138, 0.9351131265310292928 ) ) ;
#122809 = ORIENTED_EDGE ( 'NONE', *, *, #63226, .T. ) ;
#122810 = DIRECTION ( 'NONE',  ( 0.3543493200069162685, -0.000000000000000000, -0.9351131265310288487 ) ) ;
#122811 = CARTESIAN_POINT ( 'NONE',  ( -6.712309939660236147, -21.73547319004780576, 4.999917730833664642 ) ) ;
#122812 = PLANE ( 'NONE',  #14677 ) ;
#122813 = ORIENTED_EDGE ( 'NONE', *, *, #68373, .T. ) ;
#122814 = VECTOR ( 'NONE', #81052, 1000.000000000000227 ) ;
#122815 = PLANE ( 'NONE',  #94428 ) ;
#122816 = CARTESIAN_POINT ( 'NONE',  ( 21.48921356237309155, -27.52281430457070499, 5.000000000000000000 ) ) ;
#122817 = VECTOR ( 'NONE', #4490, 1000.000000000000227 ) ;
#122819 = ORIENTED_EDGE ( 'NONE', *, *, #7836, .F. ) ;
#122818 = ADVANCED_FACE ( 'NONE', ( #126475 ), #50370, .T. ) ;
#122820 = EDGE_CURVE ( 'NONE', #30495, #139670, #16261, .T. ) ;
#122822 = LINE ( 'NONE', #27783, #125867 ) ;
#122821 = VECTOR ( 'NONE', #102398, 1000.000000000000227 ) ;
#122823 = CARTESIAN_POINT ( 'NONE',  ( 20.99999999999985789, 20.70535890316563155, 1.956823837851868086 ) ) ;
#122824 = DIRECTION ( 'NONE',  ( 0.7071067811865486830, -0.7071067811865464625, -0.000000000000000000 ) ) ;
#122825 = CARTESIAN_POINT ( 'NONE',  ( 1.499999999999992673, 1.466399257802244893, 5.000000000000000000 ) ) ;
#122826 = AXIS2_PLACEMENT_3D ( 'NONE', #109103, #84534, #87377 ) ;
#122827 = LINE ( 'NONE', #56893, #30839 ) ;
#122828 = FACE_OUTER_BOUND ( 'NONE', #118439, .T. ) ;
#122830 = EDGE_CURVE ( 'NONE', #48693, #61439, #83741, .T. ) ;
#122829 = LINE ( 'NONE', #135166, #141988 ) ;
#122831 = CARTESIAN_POINT ( 'NONE',  ( 28.49999999999980815, -5.947814304570768762, 5.000000000000000000 ) ) ;
#122832 = ORIENTED_EDGE ( 'NONE', *, *, #102603, .T. ) ;
#122833 = VECTOR ( 'NONE', #78093, 1000.000000000000000 ) ;
#122834 = EDGE_CURVE ( 'NONE', #88432, #47660, #19861, .T. ) ;
#122835 = VERTEX_POINT ( 'NONE', #85833 ) ;
#122836 = CARTESIAN_POINT ( 'NONE',  ( 25.02392480454907187, -6.350000000000004974, -3.888253587292851012E-16 ) ) ;
#122837 = CARTESIAN_POINT ( 'NONE',  ( 4.190181675744454104, -18.74070752338408852, 7.910009926591497376 ) ) ;
#122838 =( NAMED_UNIT ( * ) SI_UNIT ( $, .STERADIAN. ) SOLID_ANGLE_UNIT ( ) );
#122839 = FACE_OUTER_BOUND ( 'NONE', #81846, .T. ) ;
#122840 = EDGE_LOOP ( 'NONE', ( #88044, #63746, #31719, #8211 ) ) ;
#122841 = STYLED_ITEM ( 'NONE', ( #138018 ), #41038 ) ;
#122842 = DIRECTION ( 'NONE',  ( -0.000000000000000000, 0.3543493200069153248, 0.9351131265310292928 ) ) ;
#122843 = DIRECTION ( 'NONE',  ( -0.7071067811865486830, 0.7071067811865464625, 0.000000000000000000 ) ) ;
#122844 = ORIENTED_EDGE ( 'NONE', *, *, #94771, .F. ) ;
#122845 = DIRECTION ( 'NONE',  ( 0.7071067811865486830, -0.7071067811865464625, -0.000000000000000000 ) ) ;
#122846 = PLANE ( 'NONE',  #118314 ) ;
#122847 = AXIS2_PLACEMENT_3D ( 'NONE', #141233, #64399, #86877 ) ;
#122848 = CARTESIAN_POINT ( 'NONE',  ( -0.005480084712502889671, 28.92564299267938210, 4.000000000000000000 ) ) ;
#122849 = DIRECTION ( 'NONE',  ( -1.000000000000000000, -1.224606353822377258E-16, -0.000000000000000000 ) ) ;
#122850 = CARTESIAN_POINT ( 'NONE',  ( 58.82876352523144448, 0.000000000000000000, -6.109999999999999432 ) ) ;
#122851 = ADVANCED_FACE ( 'NONE', ( #109734 ), #29311, .F. ) ;
#122852 = CARTESIAN_POINT ( 'NONE',  ( 6.489213562373093325, -27.52281430457059841, 5.000000000000000000 ) ) ;
#122853 = CARTESIAN_POINT ( 'NONE',  ( -34.92500000000001137, -8.240707523384193323, 4.255531930566235133 ) ) ;
#122854 = EDGE_LOOP ( 'NONE', ( #89776, #28520, #49110, #54283 ) ) ;
#122855 = CARTESIAN_POINT ( 'NONE',  ( -22.17183060077631751, 9.759292476615618384, 4.000000000000000000 ) ) ;
#122856 = EDGE_LOOP ( 'NONE', ( #105120, #95739, #74219, #59357 ) ) ;
#122857 = VECTOR ( 'NONE', #55976, 1000.000000000000227 ) ;
#122858 = CARTESIAN_POINT ( 'NONE',  ( 16.27785539607886633, 4.584330080086930965E-16, 0.000000000000000000 ) ) ;
#122859 = CARTESIAN_POINT ( 'NONE',  ( 22.22840764549667725, 9.139736423841732040E-16, 0.000000000000000000 ) ) ;
#122860 = CARTESIAN_POINT ( 'NONE',  ( 31.22674160717815184, -11.24070752338416490, 18.24660765846989818 ) ) ;
#122861 = DIRECTION ( 'NONE',  ( -1.000000000000000000, -0.000000000000000000, -0.000000000000000000 ) ) ;
#122862 = CARTESIAN_POINT ( 'NONE',  ( 0.000000000000000000, 0.000000000000000000, 0.000000000000000000 ) ) ;
#122863 = CARTESIAN_POINT ( 'NONE',  ( -28.82816939922331656, 0.7592924766157138627, 4.000000000000000000 ) ) ;
#122864 = ORIENTED_EDGE ( 'NONE', *, *, #68244, .T. ) ;
#122865 = VERTEX_POINT ( 'NONE', #117718 ) ;
#122866 = DIRECTION ( 'NONE',  ( 0.7071067811865487940, -0.7071067811865463515, 0.000000000000000000 ) ) ;
#122867 = UNCERTAINTY_MEASURE_WITH_UNIT (LENGTH_MEASURE( 1.000000000000000082E-05 ), #52406, 'distance_accuracy_value', 'NONE');
#122868 = AXIS2_PLACEMENT_3D ( 'NONE', #98777, #77078, #34261 ) ;
#122869 = PLANE ( 'NONE',  #109861 ) ;
#122870 = DIRECTION ( 'NONE',  ( 0.000000000000000000, -1.000000000000000000, 0.000000000000000000 ) ) ;
#122871 = CARTESIAN_POINT ( 'NONE',  ( 71.24586038379622721, 3.974999999999996980, 6.884901960086287964 ) ) ;
#122872 = CARTESIAN_POINT ( 'NONE',  ( 22.82816939922338051, -20.24070752338406720, 4.000000000000000000 ) ) ;
#122873 = EDGE_CURVE ( 'NONE', #36826, #97582, #73553, .T. ) ;
#122874 = DIRECTION ( 'NONE',  ( -0.000000000000000000, 0.000000000000000000, 1.000000000000000000 ) ) ;
#122875 = VERTEX_POINT ( 'NONE', #42366 ) ;
#122876 = CARTESIAN_POINT ( 'NONE',  ( 72.16666666666665719, 6.884901960086285300, 3.975000000000003642 ) ) ;
#122877 = CARTESIAN_POINT ( 'NONE',  ( 2.139447441471317379, 4.584330080086930965E-16, 0.000000000000000000 ) ) ;
#122878 = ADVANCED_FACE ( 'NONE', ( #40232 ), #52491, .F. ) ;
#122879 = FACE_OUTER_BOUND ( 'NONE', #93775, .T. ) ;
#122880 = PLANE ( 'NONE',  #42857 ) ;
#122881 = ORIENTED_EDGE ( 'NONE', *, *, #5537, .F. ) ;
#122882 = VECTOR ( 'NONE', #142480, 1000.000000000000000 ) ;
#122883 = EDGE_CURVE ( 'NONE', #87653, #104458, #43076, .T. ) ;
#122884 = EDGE_CURVE ( 'NONE', #42638, #48700, #8934, .T. ) ;
#122885 = CARTESIAN_POINT ( 'NONE',  ( 2.510786437626908008, -27.52281430457053446, 5.000000000000000000 ) ) ;
#122886 = AXIS2_PLACEMENT_3D ( 'NONE', #115065, #27358, #127399 ) ;
#122887 = VECTOR ( 'NONE', #27873, 1000.000000000000000 ) ;
#122888 = DIRECTION ( 'NONE',  ( -1.000000000000000000, -1.224606353822377258E-16, -0.000000000000000000 ) ) ;
#122889 = CARTESIAN_POINT ( 'NONE',  ( 63.29209685856476852, -5.291415217122921177, 3.054999999999999272 ) ) ;
#122890 = EDGE_LOOP ( 'NONE', ( #63384, #40786, #73283, #86761 ) ) ;
#122891 = VERTEX_POINT ( 'NONE', #65564 ) ;
#122892 = VECTOR ( 'NONE', #51363, 1000.000000000000227 ) ;
#122893 = VECTOR ( 'NONE', #84528, 1000.000000000000000 ) ;
#122894 = CARTESIAN_POINT ( 'NONE',  ( -33.70679250724053588, 20.25929247661551358, 20.83292124670822432 ) ) ;
#122896 = CARTESIAN_POINT ( 'NONE',  ( 27.71757738642548574, -21.73023691814493574, 5.000000000000000888 ) ) ;
#122895 =( GEOMETRIC_REPRESENTATION_CONTEXT ( 3 ) GLOBAL_UNCERTAINTY_ASSIGNED_CONTEXT ( ( #46203 ) ) GLOBAL_UNIT_ASSIGNED_CONTEXT ( ( #135310, #125850, #115621 ) ) REPRESENTATION_CONTEXT ( 'NONE', 'WORKASPACE' ) );
#122897 = FACE_OUTER_BOUND ( 'NONE', #26677, .T. ) ;
#122898 = EDGE_CURVE ( 'NONE', #61706, #20496, #117147, .T. ) ;
#122899 = DIRECTION ( 'NONE',  ( 0.3543493200069162685, -0.000000000000000000, -0.9351131265310288487 ) ) ;
#122900 = EDGE_CURVE ( 'NONE', #22203, #110486, #75694, .T. ) ;
#122901 = DIRECTION ( 'NONE',  ( 0.000000000000000000, -1.000000000000000000, 0.000000000000000000 ) ) ;
#122903 = VERTEX_POINT ( 'NONE', #98158 ) ;
#122902 = CARTESIAN_POINT ( 'NONE',  ( -5.999999999999956479, -15.03360074219758502, 5.000000000000000000 ) ) ;
#122904 = DIRECTION ( 'NONE',  ( 0.000000000000000000, -1.000000000000000000, 0.000000000000000000 ) ) ;
#122905 = LINE ( 'NONE', #12692, #49986 ) ;
#122906 = DIRECTION ( 'NONE',  ( 0.7071067811865487940, -0.7071067811865463515, 0.000000000000000000 ) ) ;
#122907 = VECTOR ( 'NONE', #115712, 1000.000000000000000 ) ;
#122908 = DIRECTION ( 'NONE',  ( 0.7071067811865486830, -0.7071067811865464625, -0.000000000000000000 ) ) ;
#122909 = ORIENTED_EDGE ( 'NONE', *, *, #58596, .T. ) ;
#122910 = EDGE_CURVE ( 'NONE', #121970, #12022, #7547, .T. ) ;
#122911 = VERTEX_POINT ( 'NONE', #142386 ) ;
#122912 = CARTESIAN_POINT ( 'NONE',  ( 56.43793019189809712, -6.110000000000001208, 1.637169565754158951 ) ) ;
#122913 = VERTEX_POINT ( 'NONE', #21307 ) ;
#122914 = AXIS2_PLACEMENT_3D ( 'NONE', #104562, #81422, #71972 ) ;
#122915 = CARTESIAN_POINT ( 'NONE',  ( 28.17183060077627843, -5.240707523384230626, 4.000000000000000000 ) ) ;
#122916 = CARTESIAN_POINT ( 'NONE',  ( 27.77004279457773350, 21.73644205237998150, 5.000000000000000888 ) ) ;
#122917 = LINE ( 'NONE', #112051, #112710 ) ;
#122918 = VECTOR ( 'NONE', #112847, 999.9999999999998863 ) ;
#122919 = CARTESIAN_POINT ( 'NONE',  ( 15.75860074219783513, 21.72499999999999432, 5.000000000000000000 ) ) ;
#122920 = CARTESIAN_POINT ( 'NONE',  ( -34.45011844616455221, 4.516280811637433779, 5.000000000000000888 ) ) ;
#122921 = ORIENTED_EDGE ( 'NONE', *, *, #120246, .T. ) ;
#122923 = EDGE_CURVE ( 'NONE', #121049, #87976, #95992, .T. ) ;
#122922 = VERTEX_POINT ( 'NONE', #87278 ) ;
#122924 = DIRECTION ( 'NONE',  ( 1.000000000000000000, 0.000000000000000000, 0.000000000000000000 ) ) ;
#122925 = CARTESIAN_POINT ( 'NONE',  ( -19.87087987052762372, -2.718579257641874580, -33.78996532117428586 ) ) ;
#122926 = VECTOR ( 'NONE', #18234, 999.9999999999998863 ) ;
#122927 = ORIENTED_EDGE ( 'NONE', *, *, #104007, .F. ) ;
#122928 = AXIS2_PLACEMENT_3D ( 'NONE', #12687, #1779, #35206 ) ;
#122929 = LINE ( 'NONE', #35231, #104592 ) ;
#122930 = DIRECTION ( 'NONE',  ( 0.7071067811865487940, 0.7071067811865463515, 0.000000000000000000 ) ) ;
#122931 = EDGE_CURVE ( 'NONE', #13309, #60163, #40920, .T. ) ;
#122932 = VECTOR ( 'NONE', #142143, 1000.000000000000000 ) ;
#122933 = ORIENTED_EDGE ( 'NONE', *, *, #18009, .F. ) ;
#122934 = FACE_BOUND ( 'NONE', #28735, .T. ) ;
#122935 = MECHANICAL_DESIGN_GEOMETRIC_PRESENTATION_REPRESENTATION (  '', ( #127479 ), #65007 ) ;
#122936 = DIRECTION ( 'NONE',  ( 0.7071067811865487940, 0.7071067811865463515, -0.000000000000000000 ) ) ;
#122937 = ADVANCED_FACE ( 'NONE', ( #96678 ), #85124, .F. ) ;
#122938 = DIRECTION ( 'NONE',  ( 0.6830127018922181881, 0.6830127018922202975, -0.2588190451025214056 ) ) ;
#122939 = LINE ( 'NONE', #70728, #126911 ) ;
#122940 = DIRECTION ( 'NONE',  ( -1.000000000000000000, -0.000000000000000000, -0.000000000000000000 ) ) ;
#122941 = CARTESIAN_POINT ( 'NONE',  ( -20.28769006033958533, -21.73547319004782352, 4.999917730833664642 ) ) ;
#122943 = ADVANCED_FACE ( 'NONE', ( #64095 ), #76415, .F. ) ;
#122942 = DIRECTION ( 'NONE',  ( 0.000000000000000000, 0.04509928337004090459, 0.9989825096764751722 ) ) ;
#122944 = EDGE_LOOP ( 'NONE', ( #63350, #123837, #33447, #121454 ) ) ;
#122945 = VECTOR ( 'NONE', #51273, 999.9999999999998863 ) ;
#122946 = ORIENTED_EDGE ( 'NONE', *, *, #110611, .F. ) ;
#122947 = CARTESIAN_POINT ( 'NONE',  ( 100.9745968585647660, 1.637169565754164280, -6.109999999999996767 ) ) ;
#122948 = ORIENTED_EDGE ( 'NONE', *, *, #73135, .F. ) ;
#122949 = LINE ( 'NONE', #23624, #111399 ) ;
#122950 = ORIENTED_EDGE ( 'NONE', *, *, #123429, .F. ) ;
#122951 = VECTOR ( 'NONE', #17838, 1000.000000000000227 ) ;
#122952 = DIRECTION ( 'NONE',  ( 1.000000000000000000, 0.000000000000000000, 0.000000000000000000 ) ) ;
#122953 = CIRCLE ( 'NONE', #90572, 2.500000000000000444 ) ;
#122954 = DIRECTION ( 'NONE',  ( 0.000000000000000000, -1.000000000000000000, 0.000000000000000000 ) ) ;
#122955 = CARTESIAN_POINT ( 'NONE',  ( -34.92500000000001137, 19.44114312045508441, 6.054907437694472705 ) ) ;
#122956 = ORIENTED_EDGE ( 'NONE', *, *, #80541, .T. ) ;
#122957 = DIRECTION ( 'NONE',  ( 0.7071067811865487940, 0.7071067811865463515, 0.000000000000000000 ) ) ;
#122958 = FACE_OUTER_BOUND ( 'NONE', #140706, .T. ) ;
#122959 = PLANE ( 'NONE',  #103303 ) ;
#122961 = LINE ( 'NONE', #23641, #1013 ) ;
#122960 = CARTESIAN_POINT ( 'NONE',  ( -14.99999999999990230, -13.39766691384885000, -10.96608748226462282 ) ) ;
#122962 = CARTESIAN_POINT ( 'NONE',  ( 26.99999999999998579, -7.850927237173508821, -1.251176053402193178 ) ) ;
#122963 = VECTOR ( 'NONE', #16340, 1000.000000000000000 ) ;
#122964 = CARTESIAN_POINT ( 'NONE',  ( 2.510786437626908008, -27.52281430457053446, 5.000000000000000000 ) ) ;
#122965 = ORIENTED_EDGE ( 'NONE', *, *, #27579, .F. ) ;
#122966 = CARTESIAN_POINT ( 'NONE',  ( 87.62500000000001421, -7.950000000000000178, -4.867971026610729436E-16 ) ) ;
#122967 = CARTESIAN_POINT ( 'NONE',  ( 20.26628700938065109, -22.22500000000000142, -15.91404180650398814 ) ) ;
#122968 = ORIENTED_EDGE ( 'NONE', *, *, #100476, .F. ) ;
#122969 = ORIENTED_EDGE ( 'NONE', *, *, #83350, .F. ) ;
#122970 = EDGE_CURVE ( 'NONE', #74632, #90138, #89413, .T. ) ;
#122971 = ORIENTED_EDGE ( 'NONE', *, *, #140154, .T. ) ;
#122972 = CARTESIAN_POINT ( 'NONE',  ( 56.87543019189809712, -5.291415217122920289, -3.055000000000001492 ) ) ;
#122973 = VECTOR ( 'NONE', #7858, 999.9999999999998863 ) ;
#122974 = ORIENTED_EDGE ( 'NONE', *, *, #44682, .F. ) ;
#122975 = CARTESIAN_POINT ( 'NONE',  ( 11.99999999999992006, 8.587461875839162317, 4.000000000000000000 ) ) ;
#122976 = CARTESIAN_POINT ( 'NONE',  ( 8.795806282870438864, -5.278424836066144543, 3.047499999999995879 ) ) ;
#122978 =( BOUNDED_CURVE ( )  B_SPLINE_CURVE ( 3, ( #20897, #7875, #65161, #109351 ),
 .UNSPECIFIED., .F., .T. ) 
 B_SPLINE_CURVE_WITH_KNOTS ( ( 4, 4 ),
 ( 2.001653308786155883, 3.503810798801451742 ),
 .UNSPECIFIED. ) 
 CURVE ( )  GEOMETRIC_REPRESENTATION_ITEM ( )  RATIONAL_B_SPLINE_CURVE ( ( 1.000000000000000000, 0.8206354192515208368, 0.8206354192515208368, 1.000000000000000000 ) ) 
 REPRESENTATION_ITEM ( '' )  );
#122977 = CARTESIAN_POINT ( 'NONE',  ( 94.20876352523144703, -7.482591942790329030E-16, 6.110000000000001208 ) ) ;
#122979 = DIRECTION ( 'NONE',  ( -0.7071067811865486830, -0.7071067811865464625, 0.000000000000000000 ) ) ;
#122980 = VERTEX_POINT ( 'NONE', #112597 ) ;
#122981 = EDGE_LOOP ( 'NONE', ( #59054, #42099, #105337, #34000 ) ) ;
#122982 = DIRECTION ( 'NONE',  ( -0.6830127018922180770, -0.6830127018922204085, -0.2588190451025213501 ) ) ;
#122983 = VECTOR ( 'NONE', #83428, 1000.000000000000000 ) ;
#122984 = CARTESIAN_POINT ( 'NONE',  ( -20.99999999999984723, 20.58746187583902909, 4.000000000000000000 ) ) ;
#122985 = ORIENTED_EDGE ( 'NONE', *, *, #81151, .T. ) ;
#122986 = DIRECTION ( 'NONE',  ( -0.6830127018922180770, -0.6830127018922204085, -0.2588190451025213501 ) ) ;
#122987 = DIRECTION ( 'NONE',  ( -1.000000000000000000, -0.000000000000000000, -0.000000000000000000 ) ) ;
#122989 = DIRECTION ( 'NONE',  ( -0.3543493200069163240, 4.681814790819596721E-17, -0.9351131265310288487 ) ) ;
#122988 = VECTOR ( 'NONE', #4865, 1000.000000000000227 ) ;
#122991 = ORIENTED_EDGE ( 'NONE', *, *, #65785, .F. ) ;
#122990 = VECTOR ( 'NONE', #115752, 1000.000000000000000 ) ;
#122992 = CARTESIAN_POINT ( 'NONE',  ( -81.48921356237309510, -27.52281430457112066, 5.000000000000000000 ) ) ;
#122993 = ORIENTED_EDGE ( 'NONE', *, *, #12202, .T. ) ;
#122994 = ORIENTED_EDGE ( 'NONE', *, *, #12647, .F. ) ;
#122995 = ORIENTED_EDGE ( 'NONE', *, *, #95589, .F. ) ;
#122996 = FACE_OUTER_BOUND ( 'NONE', #63549, .T. ) ;
#122997 =( GEOMETRIC_REPRESENTATION_CONTEXT ( 3 ) GLOBAL_UNCERTAINTY_ASSIGNED_CONTEXT ( ( #63533 ) ) GLOBAL_UNIT_ASSIGNED_CONTEXT ( ( #98576, #101432, #142802 ) ) REPRESENTATION_CONTEXT ( 'NONE', 'WORKASPACE' ) );
#122998 = VECTOR ( 'NONE', #77943, 1000.000000000000000 ) ;
#122999 = VECTOR ( 'NONE', #15129, 1000.000000000000000 ) ;
#123000 = VECTOR ( 'NONE', #100638, 999.9999999999998863 ) ;
#123001 = FACE_OUTER_BOUND ( 'NONE', #64565, .T. ) ;
#123003 = EDGE_CURVE ( 'NONE', #53919, #43072, #78546, .T. ) ;
#123002 = LINE ( 'NONE', #112134, #128427 ) ;
#123004 = PLANE ( 'NONE',  #41763 ) ;
#123005 = EDGE_CURVE ( 'NONE', #141849, #109521, #34319, .T. ) ;
#123006 = FACE_OUTER_BOUND ( 'NONE', #12919, .T. ) ;
#123008 = EDGE_LOOP ( 'NONE', ( #97454, #132674, #134659, #9353 ) ) ;
#123007 = TOROIDAL_SURFACE ( 'NONE', #16490, 6.000000000000000000, 3.000000000000000000 ) ;
#123009 = CARTESIAN_POINT ( 'NONE',  ( 34.49999999999975842, -15.29013452822851349, 0.3645803511611147019 ) ) ;
#123010 = CARTESIAN_POINT ( 'NONE',  ( 14.12456980810188689, -6.871911579029512218, 3.967499999999996252 ) ) ;
#123011 = CARTESIAN_POINT ( 'NONE',  ( -18.32816939922340538, 20.25929247661551003, 4.000000000000000000 ) ) ;
#123012 = PLANE ( 'NONE',  #59888 ) ;
#123013 = EDGE_CURVE ( 'NONE', #120532, #117668, #121319, .T. ) ;
#123014 = VECTOR ( 'NONE', #15210, 1000.000000000000000 ) ;
#123015 = DIRECTION ( 'NONE',  ( -0.3543493200069163240, -0.000000000000000000, -0.9351131265310288487 ) ) ;
#123016 = EDGE_LOOP ( 'NONE', ( #50731, #74303, #108500 ) ) ;
#123017 = ORIENTED_EDGE ( 'NONE', *, *, #21883, .F. ) ;
#123018 = EDGE_LOOP ( 'NONE', ( #25912, #53884, #62062, #120538 ) ) ;
#123019 = CARTESIAN_POINT ( 'NONE',  ( 0.000000000000000000, 0.000000000000000000, 5.000000000000000000 ) ) ;
#123020 = CARTESIAN_POINT ( 'NONE',  ( 9.489213562373095101, -27.52281430457062328, 5.000000000000000000 ) ) ;
#123021 = FACE_OUTER_BOUND ( 'NONE', #53311, .T. ) ;
#123022 = LINE ( 'NONE', #86830, #124666 ) ;
#123023 = CARTESIAN_POINT ( 'NONE',  ( 9.748310473850249736, 8.447540412293815137, -4.346633328725724610 ) ) ;
#123024 = EDGE_CURVE ( 'NONE', #87648, #128406, #134362, .T. ) ;
#123025 = AXIS2_PLACEMENT_3D ( 'NONE', #50736, #28984, #8596 ) ;
#123026 = VECTOR ( 'NONE', #12887, 999.9999999999998863 ) ;
#123027 = CARTESIAN_POINT ( 'NONE',  ( 21.48921356237309155, -27.52281430457070499, 5.000000000000000000 ) ) ;
#123028 = DIRECTION ( 'NONE',  ( 0.3543493200069162685, -0.000000000000000000, -0.9351131265310288487 ) ) ;
#123029 = CARTESIAN_POINT ( 'NONE',  ( 34.42499999999998295, 0.000000000000000000, 4.500000000000000888 ) ) ;
#123030 = VECTOR ( 'NONE', #54534, 1000.000000000000227 ) ;
#123031 = EDGE_LOOP ( 'NONE', ( #130463, #99242, #126099, #23747, #10421 ) ) ;
#123032 = DIRECTION ( 'NONE',  ( 0.000000000000000000, -1.000000000000000000, 0.000000000000000000 ) ) ;
#123033 = VERTEX_POINT ( 'NONE', #101710 ) ;
#123034 = EDGE_CURVE ( 'NONE', #123294, #2398, #54663, .T. ) ;
#123036 = CIRCLE ( 'NONE', #125309, 9.119999999999999218 ) ;
#123035 = CARTESIAN_POINT ( 'NONE',  ( 16.92059731686079971, -0.5630473312367980654, -34.80677428804649765 ) ) ;
#123037 = ORIENTED_EDGE ( 'NONE', *, *, #105580, .T. ) ;
#123038 = CARTESIAN_POINT ( 'NONE',  ( 18.27497294953710494, 4.461849672132300881, 4.461849672132299105 ) ) ;
#123040 = VERTEX_POINT ( 'NONE', #1648 ) ;
#123039 = DIRECTION ( 'NONE',  ( 1.000000000000000000, 0.000000000000000000, 0.000000000000000000 ) ) ;
#123041 = AXIS2_PLACEMENT_3D ( 'NONE', #120483, #21212, #64018 ) ;
#123042 = SURFACE_STYLE_FILL_AREA ( #12821 ) ;
#123043 = CARTESIAN_POINT ( 'NONE',  ( -14.29289321881335262, 14.25929247661556509, 5.000000000000000000 ) ) ;
#123044 = EDGE_LOOP ( 'NONE', ( #123917, #98220, #88333 ) ) ;
#123045 = DIRECTION ( 'NONE',  ( 0.7071067811865486830, -0.7071067811865464625, -0.000000000000000000 ) ) ;
#123046 = VERTEX_POINT ( 'NONE', #43771 ) ;
#123047 = DIRECTION ( 'NONE',  ( 0.000000000000000000, 1.000000000000000000, 0.000000000000000000 ) ) ;
#123048 = UNCERTAINTY_MEASURE_WITH_UNIT (LENGTH_MEASURE( 1.000000000000000082E-05 ), #57990, 'distance_accuracy_value', 'NONE');
#123049 = VERTEX_POINT ( 'NONE', #143079 ) ;
#123050 = LINE ( 'NONE', #134655, #3556 ) ;
#123051 = CARTESIAN_POINT ( 'NONE',  ( 106.9750270504628986, -5.819803920172572198, 5.819803920172572198 ) ) ;
#123052 = CARTESIAN_POINT ( 'NONE',  ( 152.4000000000000057, -17.48000000000005016, -12.70000000000043272 ) ) ;
#123053 = PLANE ( 'NONE',  #124690 ) ;
#123054 = VERTEX_POINT ( 'NONE', #33634 ) ;
#123055 = LINE ( 'NONE', #67243, #120963 ) ;
#123057 = EDGE_CURVE ( 'NONE', #8957, #13435, #94237, .T. ) ;
#123056 = DIRECTION ( 'NONE',  ( 0.6830127018922181881, 0.6830127018922202975, -0.2588190451025214056 ) ) ;
#123058 = DIRECTION ( 'NONE',  ( -0.7071067811865486830, -0.7071067811865464625, 0.000000000000000000 ) ) ;
#123060 = VECTOR ( 'NONE', #126983, 1000.000000000000000 ) ;
#123059 = CARTESIAN_POINT ( 'NONE',  ( 17.35416666666666075, 1.633150327867695095, 6.094999999999988205 ) ) ;
#123061 = CARTESIAN_POINT ( 'NONE',  ( 24.33290314143522437, -3.967499999999994476, 6.871911579029513106 ) ) ;
#123063 = VECTOR ( 'NONE', #71171, 1000.000000000000000 ) ;
#123062 = DIRECTION ( 'NONE',  ( 0.000000000000000000, -5.075120898959323014E-15, -1.000000000000000000 ) ) ;
#123064 = DIRECTION ( 'NONE',  ( 1.055184596092948005E-16, -1.000000000000000000, 0.000000000000000000 ) ) ;
#123065 = ORIENTED_EDGE ( 'NONE', *, *, #35382, .T. ) ;
#123067 = ORIENTED_EDGE ( 'NONE', *, *, #128520, .T. ) ;
#123066 = EDGE_CURVE ( 'NONE', #27137, #107840, #88723, .T. ) ;
#123068 = ADVANCED_FACE ( 'NONE', ( #23429 ), #22684, .T. ) ;
#123069 = LINE ( 'NONE', #36750, #139269 ) ;
#123070 = VERTEX_POINT ( 'NONE', #87985 ) ;
#123071 = CARTESIAN_POINT ( 'NONE',  ( 91.43793019189810423, -6.110000000000001208, 1.637169565754158951 ) ) ;
#123072 = CARTESIAN_POINT ( 'NONE',  ( 51.29974487139158867, -27.71228299555242103, 4.000000000000000000 ) ) ;
#123073 = DIRECTION ( 'NONE',  ( 0.000000000000000000, 0.000000000000000000, 1.000000000000000000 ) ) ;
#123075 = VECTOR ( 'NONE', #63138, 1000.000000000000000 ) ;
#123074 = CARTESIAN_POINT ( 'NONE',  ( -34.92500000000001137, -7.298069433178910437, 4.500000000000000888 ) ) ;
#123076 = CARTESIAN_POINT ( 'NONE',  ( 123.3803752239611384, -44.19516442797115019, -34.92499999999998295 ) ) ;
#123077 = EDGE_LOOP ( 'NONE', ( #112712, #106143, #1582, #50778 ) ) ;
#123078 = ADVANCED_FACE ( 'NONE', ( #122017 ), #132955, .F. ) ;
#123079 = CARTESIAN_POINT ( 'NONE',  ( 20.20519093902540320, 2.500000000000000888, 0.000000000000000000 ) ) ;
#123080 = SURFACE_STYLE_USAGE ( .BOTH. , #35380 ) ;
#123081 = PLANE ( 'NONE',  #60429 ) ;
#123082 = EDGE_CURVE ( 'NONE', #103031, #17161, #24158, .T. ) ;
#123083 = PLANE ( 'NONE',  #110986 ) ;
#123084 = ADVANCED_FACE ( 'NONE', ( #66954 ), #100300, .F. ) ;
#123086 = ORIENTED_EDGE ( 'NONE', *, *, #44222, .F. ) ;
#123085 = PLANE ( 'NONE',  #133160 ) ;
#123087 = FILL_AREA_STYLE_COLOUR ( '', #60881 ) ;
#123088 = CARTESIAN_POINT ( 'NONE',  ( -63.18398860626900415, 28.73617430169831621, 5.000000000000000000 ) ) ;
#123089 = AXIS2_PLACEMENT_3D ( 'NONE', #1770, #112722, #93116 ) ;
#123090 = FACE_OUTER_BOUND ( 'NONE', #77025, .T. ) ;
#123091 = CARTESIAN_POINT ( 'NONE',  ( 86.75000000000000000, -9.735942053221458872E-16, 7.950000000000000178 ) ) ;
#123092 = DIRECTION ( 'NONE',  ( -0.7071067811865486830, 0.7071067811865464625, 0.000000000000000000 ) ) ;
#123093 = ORIENTED_EDGE ( 'NONE', *, *, #31923, .F. ) ;
#123094 = VERTEX_POINT ( 'NONE', #110423 ) ;
#123095 = ORIENTED_EDGE ( 'NONE', *, *, #3903, .F. ) ;
#123097 = ADVANCED_FACE ( 'NONE', ( #11097 ), #55373, .F. ) ;
#123096 = CARTESIAN_POINT ( 'NONE',  ( 94.35459685856476142, -1.637169565754161615, 6.110000000000000320 ) ) ;
#123098 = VERTEX_POINT ( 'NONE', #108022 ) ;
#123099 = ADVANCED_FACE ( 'NONE', ( #142831 ), #99294, .F. ) ;
#123100 = CARTESIAN_POINT ( 'NONE',  ( 33.18398860626899705, 28.73617430169810305, 5.000000000000000000 ) ) ;
#123101 = CARTESIAN_POINT ( 'NONE',  ( 21.29159235450332233, 2.500000000000001332, 0.000000000000000000 ) ) ;
#123102 = LINE ( 'NONE', #123824, #17948 ) ;
#123103 = DIRECTION ( 'NONE',  ( -1.000000000000000000, -0.000000000000000000, -0.000000000000000000 ) ) ;
#123104 = ORIENTED_EDGE ( 'NONE', *, *, #124533, .T. ) ;
#123106 = EDGE_CURVE ( 'NONE', #101635, #64566, #96427, .T. ) ;
#123105 = VECTOR ( 'NONE', #78089, 1000.000000000000000 ) ;
#123107 = VECTOR ( 'NONE', #60992, 1000.000000000000000 ) ;
#123108 = CARTESIAN_POINT ( 'NONE',  ( 103.5208333333333428, 7.949999999999998401, 2.130196079827431532 ) ) ;
#123109 = DIRECTION ( 'NONE',  ( 0.7071067811865487940, -0.7071067811865463515, 0.000000000000000000 ) ) ;
#123110 = AXIS2_PLACEMENT_3D ( 'NONE', #10440, #121349, #142421 ) ;
#123112 = VECTOR ( 'NONE', #106873, 1000.000000000000000 ) ;
#123111 = CARTESIAN_POINT ( 'NONE',  ( 25.49999999999982947, 3.052185695429136647, 5.000000000000000000 ) ) ;
#123113 = CARTESIAN_POINT ( 'NONE',  ( 84.20376352523145158, 6.109999999999998543, 1.122388791418548911E-15 ) ) ;
#123114 = ORIENTED_EDGE ( 'NONE', *, *, #50937, .T. ) ;
#123115 = CARTESIAN_POINT ( 'NONE',  ( 15.56584921360887108, 8.021612662230191759, 4.000000000000000000 ) ) ;
#123116 = CIRCLE ( 'NONE', #16591, 2.055000000000000604 ) ;
#123117 = VECTOR ( 'NONE', #3039, 1000.000000000000000 ) ;
#123118 = EDGE_CURVE ( 'NONE', #5341, #31146, #76893, .T. ) ;
#123119 = CYLINDRICAL_SURFACE ( 'NONE', #9935, 2.500000000000000444 ) ;
#123120 = VECTOR ( 'NONE', #7667, 1000.000000000000000 ) ;
#123121 = TOROIDAL_SURFACE ( 'NONE', #9657, 3.113037248396092416, 1.500000000000000000 ) ;
#123122 = VECTOR ( 'NONE', #18853, 1000.000000000000000 ) ;
#123123 = EDGE_LOOP ( 'NONE', ( #22138, #59674, #93297, #22402 ) ) ;
#123124 = ORIENTED_EDGE ( 'NONE', *, *, #81815, .F. ) ;
#123125 = PLANE ( 'NONE',  #53772 ) ;
#123126 = CARTESIAN_POINT ( 'NONE',  ( -25.39999999999996305, 3.061616997868383141E-16, -2.500000000000000000 ) ) ;
#123127 = DIRECTION ( 'NONE',  ( -0.000000000000000000, -0.3543493200069152693, 0.9351131265310292928 ) ) ;
#123128 = VECTOR ( 'NONE', #27684, 1000.000000000000000 ) ;
#123129 = FILL_AREA_STYLE_COLOUR ( '', #38679 ) ;
#123130 = CARTESIAN_POINT ( 'NONE',  ( 42.18398860626899705, 28.73617430169816700, 5.000000000000000000 ) ) ;
#123131 = EDGE_CURVE ( 'NONE', #56643, #9187, #121065, .T. ) ;
#123132 = CARTESIAN_POINT ( 'NONE',  ( -18.70710678118640047, -15.74070752338412760, 5.000000000000000000 ) ) ;
#123134 = EDGE_CURVE ( 'NONE', #84461, #61441, #66015, .T. ) ;
#123133 = SURFACE_SIDE_STYLE ('',( #57890 ) ) ;
#123135 = ORIENTED_EDGE ( 'NONE', *, *, #98286, .T. ) ;
#123136 = VERTEX_POINT ( 'NONE', #31228 ) ;
#123137 = ORIENTED_EDGE ( 'NONE', *, *, #108259, .F. ) ;
#123138 = ORIENTED_EDGE ( 'NONE', *, *, #40430, .T. ) ;
#123139 = EDGE_CURVE ( 'NONE', #73074, #63455, #130023, .T. ) ;
#123140 = AXIS2_PLACEMENT_3D ( 'NONE', #99039, #76629, #142583 ) ;
#123141 = VECTOR ( 'NONE', #18406, 999.9999999999998863 ) ;
#123142 = CARTESIAN_POINT ( 'NONE',  ( 34.92499999999998295, -22.22500000000000142, 4.500000000000000888 ) ) ;
#123143 = ORIENTED_EDGE ( 'NONE', *, *, #87527, .F. ) ;
#123144 = CARTESIAN_POINT ( 'NONE',  ( 56.66252705046289151, 7.949999999999998401, 1.460391307983218338E-15 ) ) ;
#123145 = CARTESIAN_POINT ( 'NONE',  ( 60.18398860626900415, 28.73617430169829490, 5.000000000000000000 ) ) ;
#123146 = AXIS2_PLACEMENT_3D ( 'NONE', #16708, #83409, #5799 ) ;
#123147 = DIRECTION ( 'NONE',  ( -0.000000000000000000, 0.3543493200069153248, 0.9351131265310292928 ) ) ;
#123148 = VECTOR ( 'NONE', #2315, 1000.000000000000000 ) ;
#123149 = CARTESIAN_POINT ( 'NONE',  ( 27.48921356237309155, -27.52281430457074762, 5.000000000000000000 ) ) ;
#123150 = VERTEX_POINT ( 'NONE', #63861 ) ;
#123151 = CARTESIAN_POINT ( 'NONE',  ( -17.99999999999987566, 16.93112307739200872, 4.000000000000000000 ) ) ;
#123152 = ORIENTED_EDGE ( 'NONE', *, *, #28086, .F. ) ;
#123153 = DIRECTION ( 'NONE',  ( 1.000000000000000000, 0.000000000000000000, 0.000000000000000000 ) ) ;
#123154 = ORIENTED_EDGE ( 'NONE', *, *, #27763, .T. ) ;
#123155 = CARTESIAN_POINT ( 'NONE',  ( 115.8708603837962414, 6.884901960086289741, -3.974999999999993427 ) ) ;
#123156 = ORIENTED_EDGE ( 'NONE', *, *, #130123, .T. ) ;
#123157 = LINE ( 'NONE', #67348, #108380 ) ;
#123158 = ORIENTED_EDGE ( 'NONE', *, *, #48739, .F. ) ;
#123159 = ORIENTED_EDGE ( 'NONE', *, *, #97745, .T. ) ;
#123160 = VECTOR ( 'NONE', #21327, 999.9999999999998863 ) ;
#123161 = ORIENTED_EDGE ( 'NONE', *, *, #83216, .T. ) ;
#123162 = CARTESIAN_POINT ( 'NONE',  ( -57.29974487139158157, -27.71228299555246011, 4.000000000000000000 ) ) ;
#123163 = CARTESIAN_POINT ( 'NONE',  ( 31.82816939922330945, -2.240707523384262601, 4.000000000000000000 ) ) ;
#123164 = CARTESIAN_POINT ( 'NONE',  ( 114.4795968585647614, 6.109999999999999432, 1.637169565754164280 ) ) ;
#123165 = DIRECTION ( 'NONE',  ( -1.000000000000000000, -1.224606353822377258E-16, -0.000000000000000000 ) ) ;
#123166 = EDGE_CURVE ( 'NONE', #56146, #14203, #87024, .T. ) ;
#123167 = CARTESIAN_POINT ( 'NONE',  ( -54.18398860626899705, 28.73617430169825226, 5.000000000000000000 ) ) ;
#123170 = FACE_OUTER_BOUND ( 'NONE', #15089, .T. ) ;
#123169 = CARTESIAN_POINT ( 'NONE',  ( -16.49999999999988276, -4.533600742197690714, 5.000000000000000000 ) ) ;
#123168 = VECTOR ( 'NONE', #138422, 1000.000000000000000 ) ;
#123171 = VECTOR ( 'NONE', #88288, 1000.000000000000000 ) ;
#123172 = FACE_OUTER_BOUND ( 'NONE', #29438, .T. ) ;
#123173 = VERTEX_POINT ( 'NONE', #109486 ) ;
#123174 = DIRECTION ( 'NONE',  ( 0.000000000000000000, -1.000000000000000000, 0.000000000000000000 ) ) ;
#123175 = DIRECTION ( 'NONE',  ( -0.6830127018922180770, -0.6830127018922204085, -0.2588190451025213501 ) ) ;
#123176 = LINE ( 'NONE', #23851, #35683 ) ;
#123177 = ORIENTED_EDGE ( 'NONE', *, *, #37492, .T. ) ;
#123178 = ORIENTED_EDGE ( 'NONE', *, *, #53910, .T. ) ;
#123179 = AXIS2_PLACEMENT_3D ( 'NONE', #112491, #13146, #2257 ) ;
#123180 = DIRECTION ( 'NONE',  ( 0.000000000000000000, 0.000000000000000000, 1.000000000000000000 ) ) ;
#123181 = EDGE_LOOP ( 'NONE', ( #128100, #22703, #133568, #101362 ) ) ;
#123183 = ORIENTED_EDGE ( 'NONE', *, *, #102114, .T. ) ;
#123182 = EDGE_CURVE ( 'NONE', #27059, #29014, #74010, .T. ) ;
#123184 = PLANE ( 'NONE',  #95385 ) ;
#123185 = DIRECTION ( 'NONE',  ( -0.7071067811865487940, 0.7071067811865463515, 0.000000000000000000 ) ) ;
#123186 = EDGE_CURVE ( 'NONE', #103613, #114421, #30511, .T. ) ;
#123187 = LINE ( 'NONE', #37598, #101875 ) ;
#123188 = DIRECTION ( 'NONE',  ( -0.7071067811865487940, 0.7071067811865463515, -0.000000000000000000 ) ) ;
#123189 = ORIENTED_EDGE ( 'NONE', *, *, #49320, .T. ) ;
#123190 = FACE_OUTER_BOUND ( 'NONE', #70573, .T. ) ;
#123191 = CIRCLE ( 'NONE', #74552, 2.055000000000001048 ) ;
#123192 = VERTEX_POINT ( 'NONE', #43516 ) ;
#123194 = EDGE_CURVE ( 'NONE', #137919, #32809, #131971, .T. ) ;
#123193 = DIRECTION ( 'NONE',  ( 1.000000000000000000, 0.000000000000000000, 0.000000000000000000 ) ) ;
#123195 = ADVANCED_FACE ( 'NONE', ( #54425 ), #142140, .F. ) ;
#123196 = CARTESIAN_POINT ( 'NONE',  ( 20.33790314143522338, -6.871911579029513106, -3.967499999999993587 ) ) ;
#123197 = ORIENTED_EDGE ( 'NONE', *, *, #130757, .T. ) ;
#123198 = CARTESIAN_POINT ( 'NONE',  ( 83.18293019189810877, -1.637169565754159173, -6.109999999999999432 ) ) ;
#123199 = CARTESIAN_POINT ( 'NONE',  ( -25.39999999999996305, 0.000000000000000000, 0.000000000000000000 ) ) ;
#123200 = ADVANCED_FACE ( 'NONE', ( #84877 ), #98601, .F. ) ;
#123201 = CARTESIAN_POINT ( 'NONE',  ( 131.8806778009766276, -49.14999999999999147, -40.92499999999998295 ) ) ;
#123202 = ORIENTED_EDGE ( 'NONE', *, *, #70082, .T. ) ;
#123203 = VERTEX_POINT ( 'NONE', #18898 ) ;
#123204 = ORIENTED_EDGE ( 'NONE', *, *, #128286, .F. ) ;
#123205 = DIRECTION ( 'NONE',  ( 0.7071067811865487940, -0.7071067811865463515, 0.000000000000000000 ) ) ;
#123206 = PLANE ( 'NONE',  #32458 ) ;
#123207 = FACE_OUTER_BOUND ( 'NONE', #94269, .T. ) ;
#123208 = VECTOR ( 'NONE', #45151, 1000.000000000000227 ) ;
#123210 = DIRECTION ( 'NONE',  ( 0.7071067811865487940, -0.7071067811865463515, 0.000000000000000000 ) ) ;
#123209 = VECTOR ( 'NONE', #4172, 1000.000000000000000 ) ;
#123211 = AXIS2_PLACEMENT_3D ( 'NONE', #130611, #142197, #755 ) ;
#123212 = CARTESIAN_POINT ( 'NONE',  ( -54.18398860626899705, 28.73617430169825226, 5.000000000000000000 ) ) ;
#123213 = ORIENTED_EDGE ( 'NONE', *, *, #69123, .T. ) ;
#123214 = VECTOR ( 'NONE', #1515, 999.9999999999998863 ) ;
#123215 = DIRECTION ( 'NONE',  ( -0.7071067811865486830, -0.7071067811865464625, 0.000000000000000000 ) ) ;
#123216 = EDGE_CURVE ( 'NONE', #114730, #23765, #11436, .T. ) ;
#123217 = VECTOR ( 'NONE', #15386, 1000.000000000000227 ) ;
#123218 = DIRECTION ( 'NONE',  ( -1.451651444332056451E-15, -1.000000000000000000, 0.000000000000000000 ) ) ;
#123219 = CARTESIAN_POINT ( 'NONE',  ( 20.99065804761471199, 4.584330080086930965E-16, 0.000000000000000000 ) ) ;
#123220 = VERTEX_POINT ( 'NONE', #97137 ) ;
#123221 = VECTOR ( 'NONE', #132914, 1000.000000000000114 ) ;
#123222 = VECTOR ( 'NONE', #111436, 999.9999999999998863 ) ;
#123223 = EDGE_CURVE ( 'NONE', #139365, #89715, #141397, .T. ) ;
#123224 = DIRECTION ( 'NONE',  ( -0.6830127018922180770, -0.6830127018922204085, -0.2588190451025213501 ) ) ;
#123225 = ORIENTED_EDGE ( 'NONE', *, *, #134896, .T. ) ;
#123227 = VERTEX_POINT ( 'NONE', #86324 ) ;
#123226 = CARTESIAN_POINT ( 'NONE',  ( 61.46640106136302961, -43.14999999999999147, -34.92499999999998295 ) ) ;
#123228 = EDGE_LOOP ( 'NONE', ( #42739, #46426, #61893, #51430 ) ) ;
#123229 = DIRECTION ( 'NONE',  ( -8.817971600062198362E-18, -0.3543493200069152693, 0.9351131265310292928 ) ) ;
#123230 = DIRECTION ( 'NONE',  ( -0.6830127018922181881, 0.6830127018922202975, -0.2588190451025214056 ) ) ;
#123231 = EDGE_CURVE ( 'NONE', #64995, #51758, #124465, .T. ) ;
#123232 = ORIENTED_EDGE ( 'NONE', *, *, #56140, .T. ) ;
#123233 = FILL_AREA_STYLE ('',( #79025 ) ) ;
#123234 = EDGE_LOOP ( 'NONE', ( #134643, #111521, #65017, #104962 ) ) ;
#123235 = CARTESIAN_POINT ( 'NONE',  ( -31.92499999999997584, -6.270000000000012008, -37.00000000000000000 ) ) ;
#123236 = DIRECTION ( 'NONE',  ( -0.7071067811865487940, 0.7071067811865463515, 0.000000000000000000 ) ) ;
#123237 = DIRECTION ( 'NONE',  ( 0.7071067811865487940, 0.7071067811865463515, -0.000000000000000000 ) ) ;
#123238 = PLANE ( 'NONE',  #60031 ) ;
#123239 = CARTESIAN_POINT ( 'NONE',  ( 0.000000000000000000, -2.375000000000000000, 4.319999999999998508 ) ) ;
#123240 = PLANE ( 'NONE',  #90783 ) ;
#123242 = EDGE_CURVE ( 'NONE', #37516, #42382, #71086, .T. ) ;
#123241 = LINE ( 'NONE', #23916, #77302 ) ;
#123243 = CARTESIAN_POINT ( 'NONE',  ( 9.489213562373095101, -27.52281430457062328, 5.000000000000000000 ) ) ;
#123244 = CARTESIAN_POINT ( 'NONE',  ( 19.95790314143522437, 6.871911579029515771, 3.967499999999989146 ) ) ;
#123245 = DIRECTION ( 'NONE',  ( -1.000000000000000000, -0.000000000000000000, -0.000000000000000000 ) ) ;
#123246 = CARTESIAN_POINT ( 'NONE',  ( 23.78840764549667597, 0.000000000000000000, 2.500000000000001332 ) ) ;
#123247 = DIRECTION ( 'NONE',  ( 0.7071067811865486830, -0.7071067811865464625, -0.000000000000000000 ) ) ;
#123248 = CARTESIAN_POINT ( 'NONE',  ( 48.18398860626899705, 28.73617430169820608, 5.000000000000000000 ) ) ;
#123249 = ORIENTED_EDGE ( 'NONE', *, *, #92070, .F. ) ;
#123250 = VECTOR ( 'NONE', #127222, 1000.000000000000114 ) ;
#123251 = VERTEX_POINT ( 'NONE', #126165 ) ;
#123252 = EDGE_CURVE ( 'NONE', #11459, #91750, #82664, .T. ) ;
#123253 = CARTESIAN_POINT ( 'NONE',  ( 88.93750000000000000, 5.819803920172573974, -5.819803920172572198 ) ) ;
#123254 = AXIS2_PLACEMENT_3D ( 'NONE', #21835, #31299, #84955 ) ;
#123255 = ORIENTED_EDGE ( 'NONE', *, *, #61781, .F. ) ;
#123256 = ORIENTED_EDGE ( 'NONE', *, *, #113890, .T. ) ;
#123257 = ADVANCED_FACE ( 'NONE', ( #115230 ), #15916, .T. ) ;
#123258 = EDGE_LOOP ( 'NONE', ( #124086, #96049, #2966, #143233 ) ) ;
#123259 = CARTESIAN_POINT ( 'NONE',  ( -30.18398860626900060, 28.73617430169808173, 5.000000000000000000 ) ) ;
#123260 = FACE_OUTER_BOUND ( 'NONE', #96001, .T. ) ;
#123261 = CIRCLE ( 'NONE', #56111, 2.500000000000000888 ) ;
#123262 = PLANE ( 'NONE',  #19938 ) ;
#123263 = ORIENTED_EDGE ( 'NONE', *, *, #64998, .T. ) ;
#123264 = DIRECTION ( 'NONE',  ( 0.7071067811865487940, 0.7071067811865463515, 0.000000000000000000 ) ) ;
#123265 = EDGE_CURVE ( 'NONE', #50158, #123707, #94230, .T. ) ;
#123266 = CARTESIAN_POINT ( 'NONE',  ( -6.516654386410399624, 22.22500000000000142, 4.500000000000000888 ) ) ;
#123267 = DIRECTION ( 'NONE',  ( -0.6830127018922180770, -0.6830127018922204085, -0.2588190451025213501 ) ) ;
#123268 = DIRECTION ( 'NONE',  ( -1.000000000000000000, -1.224606353822377258E-16, -0.000000000000000000 ) ) ;
#123269 = ORIENTED_EDGE ( 'NONE', *, *, #50421, .T. ) ;
#123270 = CARTESIAN_POINT ( 'NONE',  ( 20.20666063542138247, 21.75929247661549581, 4.998822639870702744 ) ) ;
#123271 = CARTESIAN_POINT ( 'NONE',  ( -32.18650864602341954, -15.74070752338412760, 8.904080028139013336 ) ) ;
#123272 = CARTESIAN_POINT ( 'NONE',  ( 5.510786437626906675, -27.52281430457051314, 5.000000000000000000 ) ) ;
#123273 = CARTESIAN_POINT ( 'NONE',  ( 19.49999999999985789, -19.53360074219754594, 5.000000000000000000 ) ) ;
#123274 = LINE ( 'NONE', #68203, #22111 ) ;
#123275 = CARTESIAN_POINT ( 'NONE',  ( -16.49999999999988631, -7.420205493532911589, -2.617629953481292127 ) ) ;
#123276 = CARTESIAN_POINT ( 'NONE',  ( 69.48921356237309510, -27.52281430457103895, 5.000000000000000000 ) ) ;
#123277 = LINE ( 'NONE', #45722, #17460 ) ;
#123278 = CARTESIAN_POINT ( 'NONE',  ( 42.18398860626899705, 28.73617430169816700, 5.000000000000000000 ) ) ;
#123279 = ORIENTED_EDGE ( 'NONE', *, *, #135330, .F. ) ;
#123280 = ORIENTED_EDGE ( 'NONE', *, *, #34181, .F. ) ;
#123281 = CARTESIAN_POINT ( 'NONE',  ( 118.5629301918981042, 1.637169565754157174, 6.110000000000002984 ) ) ;
#123282 = ORIENTED_EDGE ( 'NONE', *, *, #38117, .F. ) ;
#123283 = ADVANCED_FACE ( 'NONE', ( #105797 ), #116706, .F. ) ;
#123284 = VECTOR ( 'NONE', #56285, 1000.000000000000000 ) ;
#123285 = CARTESIAN_POINT ( 'NONE',  ( -2.510786437626908008, -27.52281430457053446, 5.000000000000000000 ) ) ;
#123286 = VECTOR ( 'NONE', #48508, 1000.000000000000000 ) ;
#123287 = CARTESIAN_POINT ( 'NONE',  ( 36.18398860626899705, 28.73617430169812437, 5.000000000000000000 ) ) ;
#123288 = EDGE_CURVE ( 'NONE', #101443, #19509, #99800, .T. ) ;
#123289 = CARTESIAN_POINT ( 'NONE',  ( 51.18398860626899705, 28.73617430169823095, 5.000000000000000000 ) ) ;
#123291 =( BOUNDED_CURVE ( )  B_SPLINE_CURVE ( 2, ( #77353, #120055, #133837, #20775, #122220, #43979, #65028, #67156, #88930 ),
 .UNSPECIFIED., .F., .F. ) 
 B_SPLINE_CURVE_WITH_KNOTS ( ( 3, 2, 2, 2, 3 ),
 ( 0.1224767841415644182, 0.1250000000000000000, 0.1333333333333333315, 0.1416666666666666907, 0.1500000000000000222 ),
 .UNSPECIFIED. ) 
 CURVE ( )  GEOMETRIC_REPRESENTATION_ITEM ( )  RATIONAL_B_SPLINE_CURVE ( ( 0.9856134340836057994, 0.9896828205435386216, 1.000000000000000000, 0.9659258262890683122, 1.000000000000000000, 0.9659258262890683122, 1.000000000000000000, 0.9659258262890682012, 1.000000000000000222 ) ) 
 REPRESENTATION_ITEM ( '' )  );
#123290 = FACE_OUTER_BOUND ( 'NONE', #88365, .T. ) ;
#123292 = CARTESIAN_POINT ( 'NONE',  ( 111.4745968585647944, 1.637169565754164058, -6.109999999999996767 ) ) ;
#123293 = ORIENTED_EDGE ( 'NONE', *, *, #109950, .F. ) ;
#123294 = VERTEX_POINT ( 'NONE', #129001 ) ;
#123295 = CONICAL_SURFACE ( 'NONE', #32960, 2.055000000000000604, 0.9599310885968764806 ) ;
#123296 = PRESENTATION_LAYER_ASSIGNMENT (  '', '', ( #100414 ) ) ;
#123297 = LINE ( 'NONE', #57328, #50083 ) ;
#123298 =( BOUNDED_CURVE ( )  B_SPLINE_CURVE ( 3, ( #44674, #19997, #45377, #109163 ),
 .UNSPECIFIED., .F., .T. ) 
 B_SPLINE_CURVE_WITH_KNOTS ( ( 4, 4 ),
 ( 1.208578181583235267, 1.359146454359472678 ),
 .UNSPECIFIED. ) 
 CURVE ( )  GEOMETRIC_REPRESENTATION_ITEM ( )  RATIONAL_B_SPLINE_CURVE ( ( 1.000000000000000000, 0.9981116584018945304, 0.9981116584018945304, 1.000000000000000000 ) ) 
 REPRESENTATION_ITEM ( '' )  );
#123299 = ORIENTED_EDGE ( 'NONE', *, *, #117140, .F. ) ;
#123300 = VERTEX_POINT ( 'NONE', #51465 ) ;
#123301 = ORIENTED_EDGE ( 'NONE', *, *, #114354, .T. ) ;
#123302 = CARTESIAN_POINT ( 'NONE',  ( 25.02392480454907187, -6.350000000000004974, -3.888253587292851012E-16 ) ) ;
#123303 = CARTESIAN_POINT ( 'NONE',  ( 45.18398860626900415, 28.73617430169818832, 5.000000000000000000 ) ) ;
#123304 = AXIS2_PLACEMENT_3D ( 'NONE', #127715, #72660, #40702 ) ;
#123305 = ADVANCED_FACE ( 'NONE', ( #5047 ), #7191, .F. ) ;
#123306 = CARTESIAN_POINT ( 'NONE',  ( 33.59959685856477307, -6.109999999999997655, -1.637169565754160283 ) ) ;
#123307 = ORIENTED_EDGE ( 'NONE', *, *, #46153, .T. ) ;
#123308 = FACE_OUTER_BOUND ( 'NONE', #9567, .T. ) ;
#123309 = EDGE_LOOP ( 'NONE', ( #98522, #31679, #133414, #17571 ) ) ;
#123310 = ORIENTED_EDGE ( 'NONE', *, *, #67901, .F. ) ;
#123311 = AXIS2_PLACEMENT_3D ( 'NONE', #63683, #54935, #129611 ) ;
#123312 = VECTOR ( 'NONE', #42263, 1000.000000000000000 ) ;
#123313 = ORIENTED_EDGE ( 'NONE', *, *, #117460, .T. ) ;
#123314 = AXIS2_PLACEMENT_3D ( 'NONE', #90115, #90865, #12552 ) ;
#123315 = VECTOR ( 'NONE', #126535, 1000.000000000000000 ) ;
#123316 = VECTOR ( 'NONE', #7193, 999.9999999999998863 ) ;
#123317 = CARTESIAN_POINT ( 'NONE',  ( 0.1161069444170879233, 0.4000000000000001332, -2.220360628129161462 ) ) ;
#123318 = CARTESIAN_POINT ( 'NONE',  ( -12.20000000000000284, -40.42999999999999261, 19.06900128115121973 ) ) ;
#123319 = ORIENTED_EDGE ( 'NONE', *, *, #133595, .F. ) ;
#123320 = CARTESIAN_POINT ( 'NONE',  ( -4.171830600776450737, -17.24070752338411694, 4.000000000000000000 ) ) ;
#123322 = FACE_OUTER_BOUND ( 'NONE', #99099, .T. ) ;
#123321 = VECTOR ( 'NONE', #97179, 1000.000000000000000 ) ;
#123323 = VECTOR ( 'NONE', #3046, 1000.000000000000227 ) ;
#123324 =( GEOMETRIC_REPRESENTATION_CONTEXT ( 3 ) GLOBAL_UNCERTAINTY_ASSIGNED_CONTEXT ( ( #8331 ) ) GLOBAL_UNIT_ASSIGNED_CONTEXT ( ( #50018, #19506, #84771 ) ) REPRESENTATION_CONTEXT ( 'NONE', 'WORKASPACE' ) );
#123325 = CYLINDRICAL_SURFACE ( 'NONE', #108574, 1.000000000000000888 ) ;
#123326 = CARTESIAN_POINT ( 'NONE',  ( -30.79289321881324071, 3.759292476615681888, 5.000000000000000000 ) ) ;
#123327 = FACE_BOUND ( 'NONE', #60337, .T. ) ;
#123328 = EDGE_LOOP ( 'NONE', ( #114879, #23775, #15288, #12090, #21320 ) ) ;
#123329 = DIRECTION ( 'NONE',  ( 0.7071067811865486830, -0.7071067811865464625, -0.000000000000000000 ) ) ;
#123330 = DIRECTION ( 'NONE',  ( 0.3543493200069163240, 0.000000000000000000, 0.9351131265310288487 ) ) ;
#123331 = LINE ( 'NONE', #55930, #118522 ) ;
#123332 = CARTESIAN_POINT ( 'NONE',  ( -19.83957586139685247, 9.091547215995101183, 4.000000000000000000 ) ) ;
#123333 = ORIENTED_EDGE ( 'NONE', *, *, #57901, .T. ) ;
#123334 = FACE_OUTER_BOUND ( 'NONE', #72274, .T. ) ;
#123335 = ORIENTED_EDGE ( 'NONE', *, *, #20847, .T. ) ;
#123336 = ORIENTED_EDGE ( 'NONE', *, *, #104208, .T. ) ;
#123337 = VERTEX_POINT ( 'NONE', #38442 ) ;
#123338 = CARTESIAN_POINT ( 'NONE',  ( 49.93293019189810167, 1.637169565754156508, 6.110000000000000320 ) ) ;
#123339 = ORIENTED_EDGE ( 'NONE', *, *, #107466, .T. ) ;
#123340 = AXIS2_PLACEMENT_3D ( 'NONE', #101802, #143167, #90208 ) ;
#123341 = LINE ( 'NONE', #45088, #92680 ) ;
#123342 = CARTESIAN_POINT ( 'NONE',  ( -25.82816939922335209, -14.24070752338413293, 4.000000000000000000 ) ) ;
#123343 = ORIENTED_EDGE ( 'NONE', *, *, #85761, .F. ) ;
#123344 = CARTESIAN_POINT ( 'NONE',  ( 34.92499999999998295, 18.94777415420114508, 3.758136617891463249 ) ) ;
#123345 = DIRECTION ( 'NONE',  ( -0.6830127018922181881, 0.6830127018922202975, -0.2588190451025214056 ) ) ;
#123346 = AXIS2_PLACEMENT_3D ( 'NONE', #42763, #76825, #110110 ) ;
#123347 = DIRECTION ( 'NONE',  ( -1.000000000000000000, 0.000000000000000000, 0.000000000000000000 ) ) ;
#123348 = LINE ( 'NONE', #805, #74095 ) ;
#123349 = LINE ( 'NONE', #68277, #8913 ) ;
#123350 = VECTOR ( 'NONE', #32427, 1000.000000000000000 ) ;
#123351 = FACE_OUTER_BOUND ( 'NONE', #101558, .T. ) ;
#123352 = ORIENTED_EDGE ( 'NONE', *, *, #30927, .F. ) ;
#123353 = EDGE_CURVE ( 'NONE', #72974, #139938, #84116, .T. ) ;
#123354 = ORIENTED_EDGE ( 'NONE', *, *, #122185, .F. ) ;
#123355 = ORIENTED_EDGE ( 'NONE', *, *, #83332, .T. ) ;
#123356 = VECTOR ( 'NONE', #122330, 1000.000000000000000 ) ;
#123357 = VERTEX_POINT ( 'NONE', #117388 ) ;
#123358 = CONICAL_SURFACE ( 'NONE', #132689, 2.500000000000000444, 0.9599310885968830309 ) ;
#123359 = LINE ( 'NONE', #34915, #130676 ) ;
#123360 = VERTEX_POINT ( 'NONE', #83377 ) ;
#123361 = ORIENTED_EDGE ( 'NONE', *, *, #46899, .F. ) ;
#123362 = CARTESIAN_POINT ( 'NONE',  ( 166.7103603248079651, 26.96999999999993491, -32.60912447188198371 ) ) ;
#123363 = CARTESIAN_POINT ( 'NONE',  ( 36.18398860626899705, 28.73617430169812437, 5.000000000000000000 ) ) ;
#123364 = EDGE_CURVE ( 'NONE', #118176, #18168, #49348, .T. ) ;
#123365 = EDGE_CURVE ( 'NONE', #91404, #1467, #27535, .T. ) ;
#123366 = CARTESIAN_POINT ( 'NONE',  ( 30.29974487139158867, -27.71228299555227537, 4.000000000000000000 ) ) ;
#123367 = VERTEX_POINT ( 'NONE', #115967 ) ;
#123368 = CARTESIAN_POINT ( 'NONE',  ( -8.999999999999939604, 16.93112307739201938, 4.000000000000000000 ) ) ;
#123370 = EDGE_CURVE ( 'NONE', #130889, #54158, #16671, .T. ) ;
#123369 = PLANE ( 'NONE',  #111595 ) ;
#123371 = EDGE_CURVE ( 'NONE', #79780, #57963, #127589, .T. ) ;
#123372 = CARTESIAN_POINT ( 'NONE',  ( 29.96290314143522338, -3.967499999999994476, 6.871911579029513106 ) ) ;
#123373 = FACE_OUTER_BOUND ( 'NONE', #36275, .T. ) ;
#123374 = VERTEX_POINT ( 'NONE', #50038 ) ;
#123376 = PLANE ( 'NONE',  #82374 ) ;
#123375 = CARTESIAN_POINT ( 'NONE',  ( 107.6829301918981088, -1.637169565754159173, -6.109999999999999432 ) ) ;
#123377 = EDGE_CURVE ( 'NONE', #49398, #135194, #84793, .T. ) ;
#123378 = FACE_OUTER_BOUND ( 'NONE', #104967, .T. ) ;
#123379 = CARTESIAN_POINT ( 'NONE',  ( 0.000000000000000000, 0.000000000000000000, 6.349999999999999645 ) ) ;
#123380 = CONICAL_SURFACE ( 'NONE', #63270, 2.055000000000001048, 0.9599310885968758145 ) ;
#123381 = ORIENTED_EDGE ( 'NONE', *, *, #37843, .F. ) ;
#123382 = DIRECTION ( 'NONE',  ( -0.7071067811865486830, -0.7071067811865464625, 0.000000000000000000 ) ) ;
#123384 = ORIENTED_EDGE ( 'NONE', *, *, #26724, .T. ) ;
#123383 = DIRECTION ( 'NONE',  ( -0.3543493200069162685, -0.000000000000000000, -0.9351131265310288487 ) ) ;
#123386 = VECTOR ( 'NONE', #137504, 1000.000000000000000 ) ;
#123385 = CARTESIAN_POINT ( 'NONE',  ( 0.000000000000000000, 0.000000000000000000, 5.000000000000000000 ) ) ;
#123387 = ORIENTED_EDGE ( 'NONE', *, *, #50584, .T. ) ;
#123388 = ADVANCED_FACE ( 'NONE', ( #73918 ), #106509, .T. ) ;
#123389 = FILL_AREA_STYLE_COLOUR ( '', #54353 ) ;
#123390 = CARTESIAN_POINT ( 'NONE',  ( 17.01299345042646749, -0.9444868035190615574, -36.07446264259789359 ) ) ;
#123391 = DIRECTION ( 'NONE',  ( -0.6830127018922180770, -0.6830127018922204085, -0.2588190451025213501 ) ) ;
#123392 = CARTESIAN_POINT ( 'NONE',  ( 18.00548008471250583, 28.92564299267925776, 4.000000000000000000 ) ) ;
#123393 = VERTEX_POINT ( 'NONE', #137034 ) ;
#123394 = DIRECTION ( 'NONE',  ( -0.000000000000000000, 0.000000000000000000, 1.000000000000000000 ) ) ;
#123395 = EDGE_CURVE ( 'NONE', #31572, #87975, #110570, .T. ) ;
#123396 = CARTESIAN_POINT ( 'NONE',  ( 9.183988606268997046, 28.73617430169793607, 5.000000000000000000 ) ) ;
#123397 = CARTESIAN_POINT ( 'NONE',  ( -21.32816939922337696, -12.74070752338415602, 4.000000000000000000 ) ) ;
#123398 = ORIENTED_EDGE ( 'NONE', *, *, #31558, .T. ) ;
#123399 = AXIS2_PLACEMENT_3D ( 'NONE', #31642, #122189, #33798 ) ;
#123400 = DIRECTION ( 'NONE',  ( -0.3543493200069162685, -0.000000000000000000, -0.9351131265310288487 ) ) ;
#123401 = VERTEX_POINT ( 'NONE', #37740 ) ;
#123402 = EDGE_CURVE ( 'NONE', #94958, #125587, #131152, .T. ) ;
#123403 = DIRECTION ( 'NONE',  ( 0.6830127018922180770, -0.6830127018922204085, -0.2588190451025213501 ) ) ;
#123405 = ORIENTED_EDGE ( 'NONE', *, *, #32992, .F. ) ;
#123404 = CARTESIAN_POINT ( 'NONE',  ( 0.5685132242927009028, 2.500000000000000888, 0.000000000000000000 ) ) ;
#123406 = ORIENTED_EDGE ( 'NONE', *, *, #105314, .F. ) ;
#123407 = AXIS2_PLACEMENT_3D ( 'NONE', #119471, #64407, #97751 ) ;
#123408 = CARTESIAN_POINT ( 'NONE',  ( 2.510786437626908008, -27.52281430457053446, 5.000000000000000000 ) ) ;
#123409 =( LENGTH_UNIT ( ) NAMED_UNIT ( * ) SI_UNIT ( .MILLI., .METRE. ) );
#123410 = EDGE_CURVE ( 'NONE', #57246, #112167, #8609, .T. ) ;
#123411 = ORIENTED_EDGE ( 'NONE', *, *, #119086, .T. ) ;
#123412 = LINE ( 'NONE', #127475, #4162 ) ;
#123413 = CARTESIAN_POINT ( 'NONE',  ( -34.92499999999999005, -3.270000000000012896, -40.00000000000000000 ) ) ;
#123414 = LINE ( 'NONE', #121927, #93171 ) ;
#123415 = ORIENTED_EDGE ( 'NONE', *, *, #92583, .F. ) ;
#123416 = CARTESIAN_POINT ( 'NONE',  ( -11.99999999999992006, -13.39766691384885000, -10.96608748226462993 ) ) ;
#123417 = CARTESIAN_POINT ( 'NONE',  ( 0.000000000000000000, 9.735942053221458872E-16, -7.950000000000000178 ) ) ;
#123419 = ADVANCED_FACE ( 'NONE', ( #42743 ), #97804, .F. ) ;
#123418 = CARTESIAN_POINT ( 'NONE',  ( 23.99999999999983302, 9.631307414974347836, -9.079085613539486843 ) ) ;
#123420 = VECTOR ( 'NONE', #16924, 1000.000000000000227 ) ;
#123421 = CARTESIAN_POINT ( 'NONE',  ( -51.29974487139158867, -27.71228299555242103, 4.000000000000000000 ) ) ;
#123422 = CARTESIAN_POINT ( 'NONE',  ( 125.7882715818462174, -5.693400499257576186, 5.136054288641274113 ) ) ;
#123423 = LINE ( 'NONE', #134275, #129864 ) ;
#123425 = ORIENTED_EDGE ( 'NONE', *, *, #7395, .T. ) ;
#123424 = VECTOR ( 'NONE', #127833, 1000.000000000000000 ) ;
#123426 = VECTOR ( 'NONE', #35091, 1000.000000000000000 ) ;
#123427 = VERTEX_POINT ( 'NONE', #53606 ) ;
#123428 = ORIENTED_EDGE ( 'NONE', *, *, #104362, .T. ) ;
#123429 = EDGE_CURVE ( 'NONE', #29014, #9981, #19531, .T. ) ;
#123430 = ORIENTED_EDGE ( 'NONE', *, *, #379, .F. ) ;
#123431 = ORIENTED_EDGE ( 'NONE', *, *, #78841, .F. ) ;
#123432 = ADVANCED_FACE ( 'NONE', ( #76063 ), #142743, .F. ) ;
#123433 = VERTEX_POINT ( 'NONE', #109395 ) ;
#123434 = VECTOR ( 'NONE', #100345, 1000.000000000000000 ) ;
#123435 = AXIS2_PLACEMENT_3D ( 'NONE', #67264, #46247, #2689 ) ;
#123436 = CARTESIAN_POINT ( 'NONE',  ( 1.032389698926723387, -5.330271677715373357, -4.643458396899380780 ) ) ;
#123437 = AXIS2_PLACEMENT_3D ( 'NONE', #56999, #69286, #1132 ) ;
#123438 = DIRECTION ( 'NONE',  ( -0.000000000000000000, -0.3543493200069153248, -0.9351131265310291818 ) ) ;
#123439 = ORIENTED_EDGE ( 'NONE', *, *, #75484, .F. ) ;
#123440 = ADVANCED_FACE ( 'NONE', ( #64468 ), #61986, .T. ) ;
#123441 = LINE ( 'NONE', #103762, #120298 ) ;
#123443 = EDGE_CURVE ( 'NONE', #117264, #79752, #111884, .T. ) ;
#123442 = LINE ( 'NONE', #133578, #95248 ) ;
#123444 = CARTESIAN_POINT ( 'NONE',  ( -25.39999999999996305, 0.000000000000000000, 2.500000000000000000 ) ) ;
#123445 = DIRECTION ( 'NONE',  ( 0.7071067811865487940, 0.7071067811865463515, 0.000000000000000000 ) ) ;
#123446 = CARTESIAN_POINT ( 'NONE',  ( 123.5212635252314470, -4.472830434245839371, -4.472830434245840259 ) ) ;
#123447 = EDGE_LOOP ( 'NONE', ( #25404, #39532, #52684, #29198 ) ) ;
#123448 = DIRECTION ( 'NONE',  ( -0.000000000000000000, -0.000000000000000000, 1.000000000000000000 ) ) ;
#123449 = LINE ( 'NONE', #87216, #28312 ) ;
#123450 = CARTESIAN_POINT ( 'NONE',  ( 78.29166666666665719, 3.975000000000003642, -6.884901960086285300 ) ) ;
#123451 = CARTESIAN_POINT ( 'NONE',  ( 1.260906555256695372, 1.651889767224451688, 6.634712388435225705 ) ) ;
#123452 =( LENGTH_UNIT ( ) NAMED_UNIT ( * ) SI_UNIT ( .MILLI., .METRE. ) );
#123453 = DIRECTION ( 'NONE',  ( 2.110369192185896011E-16, -1.000000000000000000, 0.000000000000000000 ) ) ;
#123454 = DIRECTION ( 'NONE',  ( 0.7071067811865486830, -0.7071067811865464625, -0.000000000000000000 ) ) ;
#123455 = CARTESIAN_POINT ( 'NONE',  ( 44.99586038379622721, -3.974999999999998312, -6.884901960086286188 ) ) ;
#123456 = DIRECTION ( 'NONE',  ( -0.7071067811865486830, -0.7071067811865464625, -0.000000000000000000 ) ) ;
#123458 = CARTESIAN_POINT ( 'NONE',  ( 48.48921356237309510, -27.52281430457089328, 5.000000000000000000 ) ) ;
#123457 = VECTOR ( 'NONE', #37828, 1000.000000000000227 ) ;
#123459 = ORIENTED_EDGE ( 'NONE', *, *, #18785, .T. ) ;
#123460 = VERTEX_POINT ( 'NONE', #21680 ) ;
#123461 = CARTESIAN_POINT ( 'NONE',  ( 49.99999999999998579, 0.000000000000000000, -7.950000000000000178 ) ) ;
#123462 = EDGE_CURVE ( 'NONE', #81589, #133341, #98519, .T. ) ;
#123463 = DIRECTION ( 'NONE',  ( -0.7071067811865486830, -0.7071067811865464625, 0.000000000000000000 ) ) ;
#123464 = ORIENTED_EDGE ( 'NONE', *, *, #73842, .F. ) ;
#123465 = CARTESIAN_POINT ( 'NONE',  ( 127.0000000000000568, -4.172191364199829167, -4.786994800550450790 ) ) ;
#123466 = AXIS2_PLACEMENT_3D ( 'NONE', #54361, #65230, #111555 ) ;
#123467 = CARTESIAN_POINT ( 'NONE',  ( 0.000000000000000000, 0.000000000000000000, 5.000000000000000000 ) ) ;
#123468 = CARTESIAN_POINT ( 'NONE',  ( 33.83376352523143282, 6.110000000000001208, 1.122388791418549305E-15 ) ) ;
#123469 = EDGE_CURVE ( 'NONE', #110421, #137557, #131874, .T. ) ;
#123470 = VECTOR ( 'NONE', #72784, 1000.000000000000000 ) ;
#123471 = EDGE_LOOP ( 'NONE', ( #103704, #68982, #120095, #69336 ) ) ;
#123472 = LINE ( 'NONE', #79976, #17754 ) ;
#123473 = ORIENTED_EDGE ( 'NONE', *, *, #9604, .F. ) ;
#123474 = CARTESIAN_POINT ( 'NONE',  ( 17.01299345043647193, -0.9444868035624202074, 500000.0000000000582 ) ) ;
#123475 = DIRECTION ( 'NONE',  ( -0.7071067811865487940, 0.7071067811865463515, -0.000000000000000000 ) ) ;
#123476 = DIRECTION ( 'NONE',  ( 0.000000000000000000, -1.000000000000000000, 0.000000000000000000 ) ) ;
#123477 = AXIS2_PLACEMENT_3D ( 'NONE', #133022, #33701, #90939 ) ;
#123478 = PLANE ( 'NONE',  #99614 ) ;
#123479 = VERTEX_POINT ( 'NONE', #30418 ) ;
#123480 = EDGE_CURVE ( 'NONE', #98048, #77315, #6330, .T. ) ;
#123481 = CARTESIAN_POINT ( 'NONE',  ( -4.637538124160927921, 22.22499999999999432, 4.000000000000000000 ) ) ;
#123482 = VERTEX_POINT ( 'NONE', #32568 ) ;
#123483 = DIRECTION ( 'NONE',  ( 0.000000000000000000, 0.000000000000000000, 1.000000000000000000 ) ) ;
#123484 = LINE ( 'NONE', #2346, #29988 ) ;
#123485 = SPHERICAL_SURFACE ( 'NONE', #33838, 9.500000000000000000 ) ;
#123486 = DIRECTION ( 'NONE',  ( -0.7071067811865487940, 0.7071067811865463515, -0.000000000000000000 ) ) ;
#123487 =( BOUNDED_CURVE ( )  B_SPLINE_CURVE ( 3, ( #1975, #2732, #13589, #49127 ),
 .UNSPECIFIED., .F., .T. ) 
 B_SPLINE_CURVE_WITH_KNOTS ( ( 4, 4 ),
 ( 2.001653308786160768, 3.503810798801450854 ),
 .UNSPECIFIED. ) 
 CURVE ( )  GEOMETRIC_REPRESENTATION_ITEM ( )  RATIONAL_B_SPLINE_CURVE ( ( 1.000000000000000000, 0.8206354192515221690, 0.8206354192515221690, 1.000000000000000000 ) ) 
 REPRESENTATION_ITEM ( '' )  );
#123488 = AXIS2_PLACEMENT_3D ( 'NONE', #54411, #30498, #120305 ) ;
#123489 = ORIENTED_EDGE ( 'NONE', *, *, #13694, .F. ) ;
#123490 = VECTOR ( 'NONE', #130158, 1000.000000000000000 ) ;
#123491 = CARTESIAN_POINT ( 'NONE',  ( 27.29974487139158512, -27.71228299555225405, 4.000000000000000000 ) ) ;
#123492 = CARTESIAN_POINT ( 'NONE',  ( 55.47459685856478018, 1.637169565754164058, -6.109999999999996767 ) ) ;
#123493 = DIRECTION ( 'NONE',  ( -0.6830127018922180770, -0.6830127018922204085, -0.2588190451025213501 ) ) ;
#123494 = CARTESIAN_POINT ( 'NONE',  ( -20.99999999999985789, 9.631307414974306980, -9.079085613539588095 ) ) ;
#123495 = ORIENTED_EDGE ( 'NONE', *, *, #7869, .F. ) ;
#123496 = VERTEX_POINT ( 'NONE', #140585 ) ;
#123497 = AXIS2_PLACEMENT_3D ( 'NONE', #90989, #48178, #46806 ) ;
#123498 = LINE ( 'NONE', #24152, #116420 ) ;
#123499 = ORIENTED_EDGE ( 'NONE', *, *, #31678, .T. ) ;
#123500 = EDGE_CURVE ( 'NONE', #38910, #18784, #110094, .T. ) ;
#123501 = EDGE_CURVE ( 'NONE', #137039, #60934, #31145, .T. ) ;
#123502 = FACE_OUTER_BOUND ( 'NONE', #47558, .T. ) ;
#123503 = ORIENTED_EDGE ( 'NONE', *, *, #107182, .T. ) ;
#123504 = LINE ( 'NONE', #25570, #141837 ) ;
#123505 = CARTESIAN_POINT ( 'NONE',  ( 34.92499999999998295, 22.22500000000000142, 5.000000000000000000 ) ) ;
#123506 = CARTESIAN_POINT ( 'NONE',  ( -22.42819999999999681, 3.174999999999997602, 5.000000000000000000 ) ) ;
#123507 = VECTOR ( 'NONE', #78712, 1000.000000000000000 ) ;
#123508 = PLANE ( 'NONE',  #104370 ) ;
#123509 = FACE_BOUND ( 'NONE', #709, .T. ) ;
#123510 = EDGE_CURVE ( 'NONE', #60942, #64740, #108644, .T. ) ;
#123511 = DIRECTION ( 'NONE',  ( 0.7071067811865487940, 0.7071067811865463515, 0.000000000000000000 ) ) ;
#123512 = LINE ( 'NONE', #45937, #134716 ) ;
#123513 = AXIS2_PLACEMENT_3D ( 'NONE', #131652, #129482, #65719 ) ;
#123514 = DIRECTION ( 'NONE',  ( -0.000000000000000000, -0.3543493200069152693, 0.9351131265310292928 ) ) ;
#123516 = VERTEX_POINT ( 'NONE', #99204 ) ;
#123515 = LINE ( 'NONE', #89419, #69010 ) ;
#123517 = CARTESIAN_POINT ( 'NONE',  ( 0.000000000000000000, 0.000000000000000000, 5.000000000000000000 ) ) ;
#123518 = ORIENTED_EDGE ( 'NONE', *, *, #29273, .F. ) ;
#123519 = ORIENTED_EDGE ( 'NONE', *, *, #54539, .F. ) ;
#123520 = CARTESIAN_POINT ( 'NONE',  ( 76.03709685856478018, -3.054999999999998828, -5.291415217122919401 ) ) ;
#123521 = VERTEX_POINT ( 'NONE', #47753 ) ;
#123522 = CARTESIAN_POINT ( 'NONE',  ( -20.25795612380215971, -2.670494247963030698, 4.000000000000000000 ) ) ;
#123523 = ORIENTED_EDGE ( 'NONE', *, *, #86084, .F. ) ;
#123524 = CARTESIAN_POINT ( 'NONE',  ( -18.18398860626898994, 28.73617430169800002, 5.000000000000000000 ) ) ;
#123525 = AXIS2_PLACEMENT_3D ( 'NONE', #83445, #116766, #73989 ) ;
#123526 = VECTOR ( 'NONE', #105822, 1000.000000000000000 ) ;
#123527 = DIRECTION ( 'NONE',  ( 0.7071067811865486830, -0.7071067811865464625, -0.000000000000000000 ) ) ;
#123528 = LINE ( 'NONE', #124208, #84801 ) ;
#123529 = CARTESIAN_POINT ( 'NONE',  ( 7.060677813783885703, -39.92999999999999261, 19.30339710675712794 ) ) ;
#123531 = LINE ( 'NONE', #34351, #19456 ) ;
#123530 = LINE ( 'NONE', #136501, #66730 ) ;
#123532 = DIRECTION ( 'NONE',  ( 0.6830127018922180770, -0.6830127018922204085, -0.2588190451025213501 ) ) ;
#123533 = CARTESIAN_POINT ( 'NONE',  ( 5.999999999999963585, 17.96639925780208458, 5.000000000000000000 ) ) ;
#123534 = VERTEX_POINT ( 'NONE', #124560 ) ;
#123535 = AXIS2_PLACEMENT_3D ( 'NONE', #82125, #5208, #4448 ) ;
#123536 = EDGE_LOOP ( 'NONE', ( #87709, #138355, #104796, #125961 ) ) ;
#123537 = DIRECTION ( 'NONE',  ( 1.000000000000000000, 0.000000000000000000, 0.000000000000000000 ) ) ;
#123538 = DIRECTION ( 'NONE',  ( 0.000000000000000000, 0.000000000000000000, 1.000000000000000000 ) ) ;
#123539 = VERTEX_POINT ( 'NONE', #111535 ) ;
#123540 = ORIENTED_EDGE ( 'NONE', *, *, #1137, .F. ) ;
#123541 = EDGE_LOOP ( 'NONE', ( #12157, #63497, #135885, #81738, #112413, #108240, #124006, #9481 ) ) ;
#123542 = EDGE_CURVE ( 'NONE', #143110, #66688, #89093, .T. ) ;
#123543 = FACE_OUTER_BOUND ( 'NONE', #35378, .T. ) ;
#123544 = ORIENTED_EDGE ( 'NONE', *, *, #52456, .F. ) ;
#123545 = PLANE ( 'NONE',  #9182 ) ;
#123546 = AXIS2_PLACEMENT_3D ( 'NONE', #117564, #50930, #18246 ) ;
#123548 = EDGE_CURVE ( 'NONE', #133840, #100802, #91921, .T. ) ;
#123547 = CARTESIAN_POINT ( 'NONE',  ( 42.66252705046289151, 7.949999999999998401, 1.460391307983218338E-15 ) ) ;
#123549 = EDGE_CURVE ( 'NONE', #3030, #93111, #115208, .T. ) ;
#123550 = VECTOR ( 'NONE', #117307, 1000.000000000000000 ) ;
#123551 = CARTESIAN_POINT ( 'NONE',  ( 1.962903141435219601, -3.967499999999994476, 6.871911579029513106 ) ) ;
#123552 = CARTESIAN_POINT ( 'NONE',  ( -28.82816939922332011, -8.240707523384200428, 4.000000000000000000 ) ) ;
#123553 = ADVANCED_FACE ( 'NONE', ( #66622 ), #36141, .T. ) ;
#123554 = VERTEX_POINT ( 'NONE', #77515 ) ;
#123555 = LINE ( 'NONE', #114065, #6362 ) ;
#123556 = EDGE_CURVE ( 'NONE', #134614, #86498, #113674, .T. ) ;
#123557 = DIRECTION ( 'NONE',  ( -0.7071067811865486830, 0.7071067811865464625, 0.000000000000000000 ) ) ;
#123558 = DIRECTION ( 'NONE',  ( -0.7071067811865487940, 0.7071067811865463515, -0.000000000000000000 ) ) ;
#123560 = EDGE_LOOP ( 'NONE', ( #99559, #134498, #40380, #90515 ) ) ;
#123559 = CARTESIAN_POINT ( 'NONE',  ( 14.39532882439692862, 4.202752102959690472E-16, 0.000000000000000000 ) ) ;
#123561 = ORIENTED_EDGE ( 'NONE', *, *, #73514, .F. ) ;
#123562 = EDGE_CURVE ( 'NONE', #87598, #122913, #56500, .T. ) ;
#123563 = LINE ( 'NONE', #112649, #33457 ) ;
#123564 = CARTESIAN_POINT ( 'NONE',  ( 45.29974487139158867, -27.71228299555237840, 4.000000000000000000 ) ) ;
#123565 = VECTOR ( 'NONE', #57752, 1000.000000000000000 ) ;
#123566 = CARTESIAN_POINT ( 'NONE',  ( 19.49999999999986500, -13.91253812416061386, 4.000000000000000000 ) ) ;
#123567 = VERTEX_POINT ( 'NONE', #22355 ) ;
#123568 =( LENGTH_UNIT ( ) NAMED_UNIT ( * ) SI_UNIT ( .MILLI., .METRE. ) );
#123569 = DIRECTION ( 'NONE',  ( -1.000000000000000000, -0.000000000000000000, -0.000000000000000000 ) ) ;
#123570 = EDGE_CURVE ( 'NONE', #84117, #66120, #44912, .T. ) ;
#123571 = AXIS2_PLACEMENT_3D ( 'NONE', #134421, #2430, #113344 ) ;
#123572 = EDGE_CURVE ( 'NONE', #4279, #42711, #134757, .T. ) ;
#123573 = DIRECTION ( 'NONE',  ( -1.000000000000000000, -1.224606353822377258E-16, -0.000000000000000000 ) ) ;
#123574 = DIRECTION ( 'NONE',  ( -0.000000000000000000, -0.3543493200069152693, 0.9351131265310292928 ) ) ;
#123575 = DIRECTION ( 'NONE',  ( -0.6830127018922181881, 0.6830127018922202975, -0.2588190451025214056 ) ) ;
#123576 = DIRECTION ( 'NONE',  ( 0.000000000000000000, 0.000000000000000000, 1.000000000000000000 ) ) ;
#123577 = CARTESIAN_POINT ( 'NONE',  ( 39.48921356237310221, -27.52281430457082934, 5.000000000000000000 ) ) ;
#123579 = VECTOR ( 'NONE', #9584, 1000.000000000000227 ) ;
#123578 = DIRECTION ( 'NONE',  ( -0.5735764363510507113, 0.8191520442889885789, 1.003171929053520926E-16 ) ) ;
#123580 = ADVANCED_FACE ( 'NONE', ( #80370 ), #14370, .F. ) ;
#123581 = DIRECTION ( 'NONE',  ( -0.7071067811865486830, -0.7071067811865464625, -0.000000000000000000 ) ) ;
#123582 = DIRECTION ( 'NONE',  ( 0.7071067811865486830, -0.7071067811865464625, -0.000000000000000000 ) ) ;
#123583 = EDGE_CURVE ( 'NONE', #58706, #98679, #110793, .T. ) ;
#123584 = ORIENTED_EDGE ( 'NONE', *, *, #10585, .T. ) ;
#123585 = ORIENTED_EDGE ( 'NONE', *, *, #111619, .T. ) ;
#123586 = PRESENTATION_STYLE_ASSIGNMENT (( #88799 ) ) ;
#123587 = DIRECTION ( 'NONE',  ( 0.000000000000000000, -1.000000000000000000, 0.000000000000000000 ) ) ;
#123588 = ADVANCED_FACE ( 'NONE', ( #11476 ), #67344, .F. ) ;
#123589 = VECTOR ( 'NONE', #129522, 1000.000000000000000 ) ;
#123590 = DIRECTION ( 'NONE',  ( -1.000000000000000000, 0.000000000000000000, -0.000000000000000000 ) ) ;
#123591 = ORIENTED_EDGE ( 'NONE', *, *, #66907, .T. ) ;
#123592 = CARTESIAN_POINT ( 'NONE',  ( 1.180000000000000826, -9.043340090917734386, 10.00000000000000000 ) ) ;
#123593 = CARTESIAN_POINT ( 'NONE',  ( 63.29974487139158867, -27.71228299555250274, 4.000000000000000000 ) ) ;
#123594 = CARTESIAN_POINT ( 'NONE',  ( -6.489213562373093325, -27.52281430457059841, 5.000000000000000000 ) ) ;
#123595 = ORIENTED_EDGE ( 'NONE', *, *, #140447, .F. ) ;
#123596 = CARTESIAN_POINT ( 'NONE',  ( -8.999999999999937828, -7.068876922607741697, 4.000000000000000000 ) ) ;
#123597 = DIRECTION ( 'NONE',  ( -0.000000000000000000, -0.3543493200069152693, 0.9351131265310292928 ) ) ;
#123598 = PRESENTATION_STYLE_ASSIGNMENT (( #111991 ) ) ;
#123599 = CARTESIAN_POINT ( 'NONE',  ( 55.47459685856478018, 1.637169565754164280, -6.109999999999997655 ) ) ;
#123600 = FACE_OUTER_BOUND ( 'NONE', #121461, .T. ) ;
#123601 = DIRECTION ( 'NONE',  ( 0.000000000000000000, 0.000000000000000000, -1.000000000000000000 ) ) ;
#123602 = DIRECTION ( 'NONE',  ( 0.000000000000000000, -1.000000000000000000, 0.000000000000000000 ) ) ;
#123603 = ORIENTED_EDGE ( 'NONE', *, *, #5206, .T. ) ;
#123604 = DIRECTION ( 'NONE',  ( 0.000000000000000000, -1.000000000000000000, 0.000000000000000000 ) ) ;
#123605 = ADVANCED_FACE ( 'NONE', ( #79684 ), #123867, .T. ) ;
#123606 = ORIENTED_EDGE ( 'NONE', *, *, #139122, .T. ) ;
#123607 = AXIS2_PLACEMENT_3D ( 'NONE', #34387, #123573, #58336 ) ;
#123608 = DIRECTION ( 'NONE',  ( -1.000000000000000000, -1.224606353822377258E-16, -0.000000000000000000 ) ) ;
#123609 = PLANE ( 'NONE',  #9044 ) ;
#123610 = PLANE ( 'NONE',  #32673 ) ;
#123611 = CARTESIAN_POINT ( 'NONE',  ( 1.353980332882009252, 0.4000000000000001887, -2.467792535850613866 ) ) ;
#123612 = CYLINDRICAL_SURFACE ( 'NONE', #20918, 7.950000000000000178 ) ;
#123613 = CARTESIAN_POINT ( 'NONE',  ( 26.29298673570676215, -21.74070752338406365, 4.999753212805220670 ) ) ;
#123614 = ORIENTED_EDGE ( 'NONE', *, *, #103162, .T. ) ;
#123616 = ORIENTED_EDGE ( 'NONE', *, *, #53156, .F. ) ;
#123615 = CIRCLE ( 'NONE', #19369, 2.500000000000000444 ) ;
#123617 = DIRECTION ( 'NONE',  ( 0.7071067811865487940, 0.7071067811865463515, 0.000000000000000000 ) ) ;
#123618 = FACE_OUTER_BOUND ( 'NONE', #78284, .T. ) ;
#123619 = LINE ( 'NONE', #56932, #135339 ) ;
#123620 = ADVANCED_FACE ( 'NONE', ( #2769 ), #617, .F. ) ;
#123621 = CARTESIAN_POINT ( 'NONE',  ( -36.29974487139159578, -27.71228299555231445, 4.000000000000000000 ) ) ;
#123622 = CARTESIAN_POINT ( 'NONE',  ( 74.01669371712955581, 7.950000000000001066, -2.130196079827421318 ) ) ;
#123623 = CARTESIAN_POINT ( 'NONE',  ( 24.18398860626899705, 28.73617430169804265, 5.000000000000000000 ) ) ;
#123624 = AXIS2_PLACEMENT_3D ( 'NONE', #127820, #138696, #61173 ) ;
#123625 = CARTESIAN_POINT ( 'NONE',  ( -57.48921356237308800, -27.52281430457095368, 5.000000000000000000 ) ) ;
#123626 = ORIENTED_EDGE ( 'NONE', *, *, #136295, .F. ) ;
#123627 = CARTESIAN_POINT ( 'NONE',  ( 75.66666666666665719, 6.884901960086285300, 3.975000000000003642 ) ) ;
#123628 = DIRECTION ( 'NONE',  ( -0.6830127018922180770, -0.6830127018922204085, -0.2588190451025213501 ) ) ;
#123629 = EDGE_CURVE ( 'NONE', #71528, #24671, #57336, .T. ) ;
#123630 = CARTESIAN_POINT ( 'NONE',  ( -34.92500000000001137, 9.006123077391837484, 4.000000000000000000 ) ) ;
#123631 = DIRECTION ( 'NONE',  ( -0.6830127018922181881, 0.6830127018922202975, -0.2588190451025214056 ) ) ;
#123632 = ORIENTED_EDGE ( 'NONE', *, *, #64921, .F. ) ;
#123633 = VECTOR ( 'NONE', #70908, 1000.000000000000000 ) ;
#123634 = DIRECTION ( 'NONE',  ( 1.000000000000000000, 0.000000000000000000, 0.000000000000000000 ) ) ;
#123635 = EDGE_CURVE ( 'NONE', #86443, #124077, #112865, .T. ) ;
#123636 = CARTESIAN_POINT ( 'NONE',  ( 25.34840764549667469, 9.139736423841732040E-16, 0.000000000000000000 ) ) ;
#123637 = CARTESIAN_POINT ( 'NONE',  ( 63.58376352523143993, -6.110000000000001208, -3.741295971395164515E-16 ) ) ;
#123638 = VERTEX_POINT ( 'NONE', #68087 ) ;
#123639 = ORIENTED_EDGE ( 'NONE', *, *, #41833, .T. ) ;
#123640 = LINE ( 'NONE', #24987, #130923 ) ;
#123641 = CARTESIAN_POINT ( 'NONE',  ( -42.48921356237308800, -27.52281430457085065, 5.000000000000000000 ) ) ;
#123642 = CARTESIAN_POINT ( 'NONE',  ( 44.75000000000000000, -9.735942053221458872E-16, 7.950000000000000178 ) ) ;
#123643 = EDGE_CURVE ( 'NONE', #88783, #93815, #43440, .T. ) ;
#123644 = LINE ( 'NONE', #59116, #138882 ) ;
#123646 = VERTEX_POINT ( 'NONE', #127402 ) ;
#123645 = DIRECTION ( 'NONE',  ( 0.7071067811865487940, 0.7071067811865463515, -0.000000000000000000 ) ) ;
#123647 = LINE ( 'NONE', #59119, #99311 ) ;
#123648 = FACE_OUTER_BOUND ( 'NONE', #67221, .T. ) ;
#123649 = CARTESIAN_POINT ( 'NONE',  ( -24.21271579574130683, 0.1791150535437372460, 5.000000000000000000 ) ) ;
#123650 = VECTOR ( 'NONE', #113491, 1000.000000000000000 ) ;
#123651 = ORIENTED_EDGE ( 'NONE', *, *, #126008, .F. ) ;
#123652 = ORIENTED_EDGE ( 'NONE', *, *, #112562, .T. ) ;
#123653 = CARTESIAN_POINT ( 'NONE',  ( 58.33376352523143993, 6.110000000000001208, 1.122388791418549305E-15 ) ) ;
#123654 = AXIS2_PLACEMENT_3D ( 'NONE', #79243, #90805, #113962 ) ;
#123655 = ORIENTED_EDGE ( 'NONE', *, *, #66422, .F. ) ;
#123656 = CARTESIAN_POINT ( 'NONE',  ( 19.89359858452208130, 4.202752102959690472E-16, 0.000000000000000000 ) ) ;
#123657 = CARTESIAN_POINT ( 'NONE',  ( 24.48921356237309510, -27.52281430457072631, 5.000000000000000000 ) ) ;
#123658 = DIRECTION ( 'NONE',  ( -0.7071067811865486830, -0.7071067811865464625, 0.000000000000000000 ) ) ;
#123659 = DIRECTION ( 'NONE',  ( -1.000000000000000000, -0.000000000000000000, -0.000000000000000000 ) ) ;
#123660 = CARTESIAN_POINT ( 'NONE',  ( -34.42500000000001137, 4.541399257801965739, 5.000000000000000000 ) ) ;
#123661 = ORIENTED_EDGE ( 'NONE', *, *, #142991, .T. ) ;
#123662 = ORIENTED_EDGE ( 'NONE', *, *, #57914, .F. ) ;
#123663 = CARTESIAN_POINT ( 'NONE',  ( -20.25795612380215971, -2.670494247963030698, 4.000000000000000000 ) ) ;
#123664 = CIRCLE ( 'NONE', #121235, 2.500000000000000444 ) ;
#123665 = EDGE_CURVE ( 'NONE', #118195, #131632, #26672, .T. ) ;
#123666 = ORIENTED_EDGE ( 'NONE', *, *, #124207, .F. ) ;
#123667 = EDGE_CURVE ( 'NONE', #61349, #60272, #95486, .T. ) ;
#123668 = VECTOR ( 'NONE', #63129, 1000.000000000000227 ) ;
#123669 = PRESENTATION_STYLE_ASSIGNMENT (( #59140 ) ) ;
#123670 = CARTESIAN_POINT ( 'NONE',  ( -10.49999999999992362, -4.533600742197692490, 5.000000000000000000 ) ) ;
#123671 = CARTESIAN_POINT ( 'NONE',  ( -66.29974487139159578, -27.71228299555252406, 4.000000000000000000 ) ) ;
#123672 = ORIENTED_EDGE ( 'NONE', *, *, #6442, .F. ) ;
#123673 = CIRCLE ( 'NONE', #116700, 4.999999999999998224 ) ;
#123674 = FACE_BOUND ( 'NONE', #54994, .T. ) ;
#123675 = ADVANCED_FACE ( 'NONE', ( #7010 ), #28104, .F. ) ;
#123676 = LINE ( 'NONE', #68576, #77994 ) ;
#123677 = DIRECTION ( 'NONE',  ( -0.7071067811865487940, 0.7071067811865463515, 0.000000000000000000 ) ) ;
#123678 = DIRECTION ( 'NONE',  ( 1.000000000000000000, 0.000000000000000000, 0.000000000000000000 ) ) ;
#123679 = LINE ( 'NONE', #80876, #57332 ) ;
#123680 = VECTOR ( 'NONE', #22709, 1000.000000000000000 ) ;
#123681 = CARTESIAN_POINT ( 'NONE',  ( -28.49999999999980460, 21.05218569542895324, 5.000000000000000000 ) ) ;
#123682 = CARTESIAN_POINT ( 'NONE',  ( 104.8685099229812465, 4.789999999999941416, -1.954035193718730588E-12 ) ) ;
#123683 = ORIENTED_EDGE ( 'NONE', *, *, #117021, .F. ) ;
#123684 = ORIENTED_EDGE ( 'NONE', *, *, #73732, .F. ) ;
#123685 = CARTESIAN_POINT ( 'NONE',  ( 99.22459685856478018, -1.637169565754160949, 6.109999999999997655 ) ) ;
#123686 = ORIENTED_EDGE ( 'NONE', *, *, #67957, .T. ) ;
#123687 = CARTESIAN_POINT ( 'NONE',  ( -2.510786437626908008, -27.52281430457053446, 5.000000000000000000 ) ) ;
#123688 = EDGE_LOOP ( 'NONE', ( #95784, #29572, #114559, #9781 ) ) ;
#123689 = CARTESIAN_POINT ( 'NONE',  ( 31.92500000000002203, -21.76999999999999247, -37.00000000000000000 ) ) ;
#123690 = CARTESIAN_POINT ( 'NONE',  ( 10.49999999999993250, 10.94296225409028089, -9.576120664313233277 ) ) ;
#123691 = PRESENTATION_LAYER_ASSIGNMENT (  '', '', ( #7941 ) ) ;
#123692 = FACE_OUTER_BOUND ( 'NONE', #9664, .T. ) ;
#123693 = ORIENTED_EDGE ( 'NONE', *, *, #137874, .T. ) ;
#123694 = DIRECTION ( 'NONE',  ( -1.000000000000000000, -0.000000000000000000, 0.000000000000000000 ) ) ;
#123695 = DIRECTION ( 'NONE',  ( 0.6830127018922181881, 0.6830127018922202975, -0.2588190451025214056 ) ) ;
#123696 = DIRECTION ( 'NONE',  ( 1.000000000000000000, 1.224606353822377258E-16, 0.000000000000000000 ) ) ;
#123698 = DIRECTION ( 'NONE',  ( 0.7071067811865487940, -0.7071067811865463515, 0.000000000000000000 ) ) ;
#123697 = DIRECTION ( 'NONE',  ( -0.000000000000000000, -0.3543493200069152693, 0.9351131265310292928 ) ) ;
#123699 = CARTESIAN_POINT ( 'NONE',  ( 36.48921356237310221, -27.52281430457080802, 5.000000000000000000 ) ) ;
#123700 = VECTOR ( 'NONE', #62224, 999.9999999999998863 ) ;
#123701 = LINE ( 'NONE', #124385, #51424 ) ;
#123702 = ORIENTED_EDGE ( 'NONE', *, *, #48085, .F. ) ;
#123703 = DIRECTION ( 'NONE',  ( -0.6830127018922181881, 0.6830127018922202975, -0.2588190451025214056 ) ) ;
#123704 = LINE ( 'NONE', #54870, #95130 ) ;
#123705 = ORIENTED_EDGE ( 'NONE', *, *, #79035, .F. ) ;
#123706 = ORIENTED_EDGE ( 'NONE', *, *, #126456, .T. ) ;
#123707 = VERTEX_POINT ( 'NONE', #72369 ) ;
#123708 = CARTESIAN_POINT ( 'NONE',  ( 57.45876352523143993, 0.000000000000000000, -6.110000000000001208 ) ) ;
#123709 = VERTEX_POINT ( 'NONE', #5605 ) ;
#123710 = CYLINDRICAL_SURFACE ( 'NONE', #16513, 2.500000000000000444 ) ;
#123711 = EDGE_CURVE ( 'NONE', #13955, #49848, #49163, .T. ) ;
#123712 = CARTESIAN_POINT ( 'NONE',  ( 7.920806282870441528, 3.047499999999997655, 5.278424836066143655 ) ) ;
#123713 = CARTESIAN_POINT ( 'NONE',  ( 93.62543019189811844, 5.291415217122919401, 3.055000000000002824 ) ) ;
#123714 = CARTESIAN_POINT ( 'NONE',  ( 38.99451991528749062, 28.92564299267965211, 4.000000000000000000 ) ) ;
#123715 = ORIENTED_EDGE ( 'NONE', *, *, #61866, .F. ) ;
#123716 = ADVANCED_FACE ( 'NONE', ( #92621 ), #48424, .F. ) ;
#123717 = CARTESIAN_POINT ( 'NONE',  ( -42.48921356237308800, -27.52281430457085065, 5.000000000000000000 ) ) ;
#123719 = VERTEX_POINT ( 'NONE', #38270 ) ;
#123718 = EDGE_CURVE ( 'NONE', #47033, #29497, #104939, .T. ) ;
#123720 = DIRECTION ( 'NONE',  ( 0.7071067811865487940, 0.7071067811865463515, 0.000000000000000000 ) ) ;
#123721 = ORIENTED_EDGE ( 'NONE', *, *, #68903, .F. ) ;
#123722 = EDGE_CURVE ( 'NONE', #57991, #55512, #6289, .T. ) ;
#123723 = AXIS2_PLACEMENT_3D ( 'NONE', #127040, #127789, #19710 ) ;
#123724 = LINE ( 'NONE', #24381, #85459 ) ;
#123725 = LINE ( 'NONE', #102678, #33647 ) ;
#123726 = EDGE_LOOP ( 'NONE', ( #52029, #27274, #106677 ) ) ;
#123727 = CARTESIAN_POINT ( 'NONE',  ( 27.29974487139158512, -27.71228299555225405, 4.000000000000000000 ) ) ;
#123728 = ORIENTED_EDGE ( 'NONE', *, *, #82804, .F. ) ;
#123729 = VERTEX_POINT ( 'NONE', #25964 ) ;
#123730 = ORIENTED_EDGE ( 'NONE', *, *, #120519, .F. ) ;
#123731 = FILL_AREA_STYLE_COLOUR ( '', #7651 ) ;
#123732 = EDGE_CURVE ( 'NONE', #34094, #26993, #4132, .T. ) ;
#123733 = LINE ( 'NONE', #136007, #72576 ) ;
#123734 = CARTESIAN_POINT ( 'NONE',  ( 30.18398860626900060, 28.73617430169808173, 5.000000000000000000 ) ) ;
#123735 = ADVANCED_FACE ( 'NONE', ( #39719 ), #106338, .F. ) ;
#123736 = CARTESIAN_POINT ( 'NONE',  ( -27.48921356237309155, -27.52281430457074762, 5.000000000000000000 ) ) ;
#123737 = VERTEX_POINT ( 'NONE', #17222 ) ;
#123738 = AXIS2_PLACEMENT_3D ( 'NONE', #141523, #118317, #6666 ) ;
#123739 = FACE_OUTER_BOUND ( 'NONE', #68602, .T. ) ;
#123740 = EDGE_CURVE ( 'NONE', #142010, #136110, #95720, .T. ) ;
#123741 = VECTOR ( 'NONE', #61068, 1000.000000000000114 ) ;
#123742 = CARTESIAN_POINT ( 'NONE',  ( 26.08290314143522082, 3.967499999999992699, -6.871911579029513994 ) ) ;
#123743 = DIRECTION ( 'NONE',  ( 0.7071067811865486830, -0.7071067811865464625, -0.000000000000000000 ) ) ;
#123744 = FACE_OUTER_BOUND ( 'NONE', #63607, .T. ) ;
#123745 = DIRECTION ( 'NONE',  ( -0.7071067811865486830, -0.7071067811865464625, 0.000000000000000000 ) ) ;
#123746 = ORIENTED_EDGE ( 'NONE', *, *, #50327, .F. ) ;
#123747 = AXIS2_PLACEMENT_3D ( 'NONE', #120516, #58933, #13912 ) ;
#123748 = VERTEX_POINT ( 'NONE', #103494 ) ;
#123749 = EDGE_LOOP ( 'NONE', ( #134249, #77460, #90454, #129545 ) ) ;
#123750 = DIRECTION ( 'NONE',  ( 0.6830127018922180770, -0.6830127018922204085, -0.2588190451025213501 ) ) ;
#123751 = EDGE_CURVE ( 'NONE', #79833, #43058, #136858, .T. ) ;
#123752 = LINE ( 'NONE', #22945, #21810 ) ;
#123753 = CARTESIAN_POINT ( 'NONE',  ( 94.28752705046289861, 0.000000000000000000, -7.949999999999998401 ) ) ;
#123754 = PLANE ( 'NONE',  #103334 ) ;
#123755 = FACE_OUTER_BOUND ( 'NONE', #99359, .T. ) ;
#123756 = AXIS2_PLACEMENT_3D ( 'NONE', #122272, #90378, #78096 ) ;
#123757 = DIRECTION ( 'NONE',  ( -0.7071067811865487940, 0.7071067811865463515, -0.000000000000000000 ) ) ;
#123758 = DIRECTION ( 'NONE',  ( 0.6830127018922181881, 0.6830127018922202975, -0.2588190451025214056 ) ) ;
#123759 = DIRECTION ( 'NONE',  ( 0.000000000000000000, -1.000000000000000000, 0.000000000000000000 ) ) ;
#123760 = CARTESIAN_POINT ( 'NONE',  ( 0.000000000000000000, 5.817072295949924468E-16, -4.749999999999997335 ) ) ;
#123761 = EDGE_CURVE ( 'NONE', #60930, #43567, #115068, .T. ) ;
#123762 = VERTEX_POINT ( 'NONE', #27360 ) ;
#123763 = CARTESIAN_POINT ( 'NONE',  ( 17.20358538138344429, -1.503029704422955248, -32.09388084135276387 ) ) ;
#123764 = ORIENTED_EDGE ( 'NONE', *, *, #111713, .T. ) ;
#123765 = DIRECTION ( 'NONE',  ( -0.000000000000000000, 0.3543493200069153248, 0.9351131265310292928 ) ) ;
#123767 = EDGE_LOOP ( 'NONE', ( #38768, #104338, #65960, #33007 ) ) ;
#123766 = LINE ( 'NONE', #136040, #69634 ) ;
#123768 = CARTESIAN_POINT ( 'NONE',  ( 1.603431928946415175, -14.24070752338413648, 19.24067776001726671 ) ) ;
#123769 = CARTESIAN_POINT ( 'NONE',  ( -2.994519915287485734, 28.92564299267940342, 4.000000000000000000 ) ) ;
#123770 = VERTEX_POINT ( 'NONE', #105628 ) ;
#123771 = CARTESIAN_POINT ( 'NONE',  ( 6.489213562373093325, -27.52281430457059841, 5.000000000000000000 ) ) ;
#123772 = ORIENTED_EDGE ( 'NONE', *, *, #80178, .F. ) ;
#123773 = CARTESIAN_POINT ( 'NONE',  ( -38.99451991528749062, 28.92564299267965211, 4.000000000000000000 ) ) ;
#123774 = VERTEX_POINT ( 'NONE', #60033 ) ;
#123775 = VECTOR ( 'NONE', #26878, 1000.000000000000000 ) ;
#123776 = LINE ( 'NONE', #24435, #38060 ) ;
#123777 = ADVANCED_FACE ( 'NONE', ( #50568 ), #4867, .F. ) ;
#123778 = CARTESIAN_POINT ( 'NONE',  ( 104.7875270504628986, 0.000000000000000000, -7.949999999999998401 ) ) ;
#123780 = VECTOR ( 'NONE', #34216, 1000.000000000000000 ) ;
#123779 = DIRECTION ( 'NONE',  ( 0.000000000000000000, 0.000000000000000000, 1.000000000000000000 ) ) ;
#123781 = AXIS2_PLACEMENT_3D ( 'NONE', #40480, #41161, #126727 ) ;
#123782 = FACE_OUTER_BOUND ( 'NONE', #122012, .T. ) ;
#123783 = ORIENTED_EDGE ( 'NONE', *, *, #32951, .F. ) ;
#123784 = VECTOR ( 'NONE', #11466, 1000.000000000000000 ) ;
#123785 = CARTESIAN_POINT ( 'NONE',  ( 71.99451991528749772, 28.92564299267988304, 4.000000000000000000 ) ) ;
#123786 = CARTESIAN_POINT ( 'NONE',  ( 62.99451991528749772, 28.92564299267982264, 4.000000000000000000 ) ) ;
#123787 = CARTESIAN_POINT ( 'NONE',  ( -39.29974487139159578, -27.71228299555233576, 4.000000000000000000 ) ) ;
#123788 = CARTESIAN_POINT ( 'NONE',  ( 12.25000000000000000, -7.464222240803106570E-16, -6.094999999999989981 ) ) ;
#123789 = CARTESIAN_POINT ( 'NONE',  ( -17.99999999999987210, -9.033600742197645417, 5.000000000000000000 ) ) ;
#123790 = PLANE ( 'NONE',  #130075 ) ;
#123791 = DIRECTION ( 'NONE',  ( 0.7071067811865487940, 0.7071067811865463515, 0.000000000000000000 ) ) ;
#123792 = ORIENTED_EDGE ( 'NONE', *, *, #50725, .T. ) ;
#123793 = DIRECTION ( 'NONE',  ( 0.7071067811865487940, -0.7071067811865463515, 0.000000000000000000 ) ) ;
#123794 = ORIENTED_EDGE ( 'NONE', *, *, #28551, .F. ) ;
#123795 = EDGE_CURVE ( 'NONE', #138233, #29394, #73066, .T. ) ;
#123796 = CARTESIAN_POINT ( 'NONE',  ( 91.72959685856477563, -6.110000000000000320, -1.637169565754161393 ) ) ;
#123797 = DIRECTION ( 'NONE',  ( -0.7071067811865486830, -0.7071067811865464625, -0.000000000000000000 ) ) ;
#123798 = DIRECTION ( 'NONE',  ( -1.000000000000000000, 0.000000000000000000, -0.000000000000000000 ) ) ;
#123799 = CARTESIAN_POINT ( 'NONE',  ( -22.49999999999984013, -16.91253812416058366, 4.000000000000000000 ) ) ;
#123800 = CARTESIAN_POINT ( 'NONE',  ( 122.6835989386368055, -43.15000000000001279, -34.92499999999998295 ) ) ;
#123801 = VERTEX_POINT ( 'NONE', #117219 ) ;
#123802 = LINE ( 'NONE', #24457, #109949 ) ;
#123803 =( LENGTH_UNIT ( ) NAMED_UNIT ( * ) SI_UNIT ( .MILLI., .METRE. ) );
#123804 = DIRECTION ( 'NONE',  ( -0.000000000000000000, 0.3543493200069153248, 0.9351131265310292928 ) ) ;
#123805 = EDGE_LOOP ( 'NONE', ( #8243, #65845, #90016, #15805 ) ) ;
#123806 = CARTESIAN_POINT ( 'NONE',  ( -30.48921356237309510, -27.52281430457076894, 5.000000000000000000 ) ) ;
#123807 = EDGE_CURVE ( 'NONE', #76459, #133583, #16982, .T. ) ;
#123808 = DIRECTION ( 'NONE',  ( 0.000000000000000000, 0.000000000000000000, 1.000000000000000000 ) ) ;
#123810 = ORIENTED_EDGE ( 'NONE', *, *, #100655, .T. ) ;
#123809 = DIRECTION ( 'NONE',  ( -1.000000000000000000, -0.000000000000000000, -0.000000000000000000 ) ) ;
#123811 = DIRECTION ( 'NONE',  ( -0.000000000000000000, -0.000000000000000000, -1.000000000000000000 ) ) ;
#123812 = LINE ( 'NONE', #77462, #19736 ) ;
#123813 = FACE_OUTER_BOUND ( 'NONE', #105865, .T. ) ;
#123814 = PLANE ( 'NONE',  #3871 ) ;
#123815 = ORIENTED_EDGE ( 'NONE', *, *, #81192, .T. ) ;
#123816 = ORIENTED_EDGE ( 'NONE', *, *, #30997, .F. ) ;
#123817 = EDGE_LOOP ( 'NONE', ( #79419, #77219, #141641, #93638 ) ) ;
#123818 = CARTESIAN_POINT ( 'NONE',  ( 87.64626352523141861, -4.472830434245840259, 4.472830434245839371 ) ) ;
#123819 = ORIENTED_EDGE ( 'NONE', *, *, #64953, .T. ) ;
#123820 = CARTESIAN_POINT ( 'NONE',  ( -36.29974487139159578, -27.71228299555231445, 4.000000000000000000 ) ) ;
#123821 = EDGE_CURVE ( 'NONE', #110390, #92829, #64305, .T. ) ;
#123822 = CARTESIAN_POINT ( 'NONE',  ( -8.563198967791651128, -12.74070752338415424, 9.898150129686394294 ) ) ;
#123823 = EDGE_CURVE ( 'NONE', #83942, #56788, #105858, .T. ) ;
#123824 = CARTESIAN_POINT ( 'NONE',  ( 26.99451991528749417, 28.92564299267956685, 4.000000000000000000 ) ) ;
#123825 = LINE ( 'NONE', #58606, #61673 ) ;
#123826 = ORIENTED_EDGE ( 'NONE', *, *, #83599, .F. ) ;
#123827 = DIRECTION ( 'NONE',  ( -0.7071067811865486830, -0.7071067811865464625, 0.000000000000000000 ) ) ;
#123829 = AXIS2_PLACEMENT_3D ( 'NONE', #13645, #78230, #113690 ) ;
#123828 = DIRECTION ( 'NONE',  ( -0.000000000000000000, 0.3543493200069153248, 0.9351131265310292928 ) ) ;
#123830 = CARTESIAN_POINT ( 'NONE',  ( -4.171830600776441855, 18.75929247661552424, 4.000000000000000000 ) ) ;
#123831 = CARTESIAN_POINT ( 'NONE',  ( 80.26626352523145158, 4.472830434245839371, -4.472830434245838482 ) ) ;
#123832 = ORIENTED_EDGE ( 'NONE', *, *, #63992, .T. ) ;
#123833 = EDGE_CURVE ( 'NONE', #7972, #100907, #23462, .T. ) ;
#123834 = LINE ( 'NONE', #112234, #123026 ) ;
#123835 = CARTESIAN_POINT ( 'NONE',  ( -10.25154412867569143, -11.24070752338416845, 10.39518518046011764 ) ) ;
#123836 = VERTEX_POINT ( 'NONE', #981 ) ;
#123837 = ORIENTED_EDGE ( 'NONE', *, *, #63335, .T. ) ;
#123838 = ADVANCED_FACE ( 'NONE', ( #45265 ), #131001, .F. ) ;
#123839 = DIRECTION ( 'NONE',  ( 0.6830127018922181881, 0.6830127018922202975, -0.2588190451025214056 ) ) ;
#123840 = EDGE_CURVE ( 'NONE', #16613, #94289, #111166, .T. ) ;
#123841 = SURFACE_STYLE_FILL_AREA ( #59312 ) ;
#123842 = CARTESIAN_POINT ( 'NONE',  ( 20.77540314143522338, -2.126176841940958351, -7.934999999999988951 ) ) ;
#123843 = DIRECTION ( 'NONE',  ( -1.000000000000000000, -1.224606353822377258E-16, -0.000000000000000000 ) ) ;
#123844 = CARTESIAN_POINT ( 'NONE',  ( 3.000000000000000444, -47.87246431468549446, -37.20487561447684755 ) ) ;
#123845 = DIRECTION ( 'NONE',  ( -0.000000000000000000, 0.000000000000000000, 1.000000000000000000 ) ) ;
#123846 = DIRECTION ( 'NONE',  ( 0.7071067811865487940, 0.7071067811865463515, -0.000000000000000000 ) ) ;
#123847 =( LENGTH_UNIT ( ) NAMED_UNIT ( * ) SI_UNIT ( .MILLI., .METRE. ) );
#123848 = VECTOR ( 'NONE', #36762, 1000.000000000000000 ) ;
#123849 = ORIENTED_EDGE ( 'NONE', *, *, #118916, .T. ) ;
#123850 = ORIENTED_EDGE ( 'NONE', *, *, #95436, .F. ) ;
#123851 = AXIS2_PLACEMENT_3D ( 'NONE', #39669, #126627, #6245 ) ;
#123852 = LINE ( 'NONE', #48403, #31750 ) ;
#123853 = ORIENTED_EDGE ( 'NONE', *, *, #13597, .T. ) ;
#123854 = ORIENTED_EDGE ( 'NONE', *, *, #101167, .T. ) ;
#123855 = ADVANCED_FACE ( 'NONE', ( #52694 ), #112968, .T. ) ;
#123856 = CARTESIAN_POINT ( 'NONE',  ( 45.18398860626900415, 28.73617430169818832, 5.000000000000000000 ) ) ;
#123857 = ORIENTED_EDGE ( 'NONE', *, *, #24566, .F. ) ;
#123858 = COLOUR_RGB ( '', 0.08235294, 0.09019608, 0.10196078) ;
#123859 = CARTESIAN_POINT ( 'NONE',  ( 10.83999999999999986, 9.521314400968980422E-16, 0.000000000000000000 ) ) ;
#123860 = CARTESIAN_POINT ( 'NONE',  ( -15.29974487139158867, -27.71228299555216879, 4.000000000000000000 ) ) ;
#123861 = CARTESIAN_POINT ( 'NONE',  ( 0.000000000000000000, 21.72500000000000142, 4.500000000000000888 ) ) ;
#123862 = LINE ( 'NONE', #24519, #62379 ) ;
#123863 = DIRECTION ( 'NONE',  ( 0.000000000000000000, -0.000000000000000000, -1.000000000000000000 ) ) ;
#123864 = ORIENTED_EDGE ( 'NONE', *, *, #23611, .F. ) ;
#123865 = CARTESIAN_POINT ( 'NONE',  ( 51.29974487139158867, -27.71228299555242103, 4.000000000000000000 ) ) ;
#123866 = EDGE_LOOP ( 'NONE', ( #105324, #28287, #66203, #69711 ) ) ;
#123867 = CYLINDRICAL_SURFACE ( 'NONE', #82779, 7.950000000000000178 ) ;
#123868 = ORIENTED_EDGE ( 'NONE', *, *, #21887, .F. ) ;
#123869 = CARTESIAN_POINT ( 'NONE',  ( 0.000000000000000000, 0.000000000000000000, 7.950000000000000178 ) ) ;
#123870 = ORIENTED_EDGE ( 'NONE', *, *, #120106, .T. ) ;
#123871 = ORIENTED_EDGE ( 'NONE', *, *, #119154, .F. ) ;
#123872 = ORIENTED_EDGE ( 'NONE', *, *, #40352, .F. ) ;
#123873 = EDGE_LOOP ( 'NONE', ( #19395, #46048, #134143, #31091 ) ) ;
#123874 = B_SPLINE_CURVE_WITH_KNOTS ( 'NONE', 1,
 ( #29573, #60840 ),
 .UNSPECIFIED., .F., .F.,
 ( 2, 2 ),
 ( 0.000000000000000000, 1.000000000000000000 ),
 .UNSPECIFIED. ) ;
#123875 = VECTOR ( 'NONE', #18928, 1000.000000000000000 ) ;
#123876 = CARTESIAN_POINT ( 'NONE',  ( 94.04166666666665719, -3.975000000000002753, 6.884901960086286188 ) ) ;
#123877 = CONICAL_SURFACE ( 'NONE', #54456, 2.500000000000000444, 0.9599310885968830309 ) ;
#123879 = ADVANCED_FACE ( 'NONE', ( #11854 ), #130293, .F. ) ;
#123878 = AXIS2_PLACEMENT_3D ( 'NONE', #126698, #13649, #47088 ) ;
#123880 = FACE_OUTER_BOUND ( 'NONE', #60655, .T. ) ;
#123881 = CARTESIAN_POINT ( 'NONE',  ( 122.5004301918981184, -3.055000000000002380, 5.291415217122920289 ) ) ;
#123882 = PLANE ( 'NONE',  #135424 ) ;
#123883 = VECTOR ( 'NONE', #23981, 1000.000000000000000 ) ;
#123884 = EDGE_CURVE ( 'NONE', #13822, #96941, #41835, .T. ) ;
#123885 = FACE_OUTER_BOUND ( 'NONE', #96598, .T. ) ;
#123887 = DIRECTION ( 'NONE',  ( -0.6830127018922181881, 0.6830127018922202975, -0.2588190451025214056 ) ) ;
#123886 = CARTESIAN_POINT ( 'NONE',  ( 60.48921356237309510, -27.52281430457097500, 5.000000000000000000 ) ) ;
#123888 = CARTESIAN_POINT ( 'NONE',  ( -17.58838509405156003, 22.22500000000000142, 4.777194822843815025 ) ) ;
#123889 = ADVANCED_FACE ( 'NONE', ( #33659 ), #86058, .F. ) ;
#123890 = EDGE_CURVE ( 'NONE', #96522, #116312, #118675, .T. ) ;
#123891 = DIRECTION ( 'NONE',  ( 1.000000000000000000, 0.000000000000000000, 0.000000000000000000 ) ) ;
#123892 = VERTEX_POINT ( 'NONE', #22713 ) ;
#123893 = CARTESIAN_POINT ( 'NONE',  ( -39.48921356237310221, -27.52281430457082934, 5.000000000000000000 ) ) ;
#123894 = ORIENTED_EDGE ( 'NONE', *, *, #21934, .T. ) ;
#123895 = VERTEX_POINT ( 'NONE', #84630 ) ;
#123896 = CARTESIAN_POINT ( 'NONE',  ( -20.51078643762690490, -27.52281430457041012, 5.000000000000000000 ) ) ;
#123897 = ORIENTED_EDGE ( 'NONE', *, *, #132872, .F. ) ;
#123898 = DIRECTION ( 'NONE',  ( -0.7071067811865486830, -0.7071067811865464625, 0.000000000000000000 ) ) ;
#123899 = DIRECTION ( 'NONE',  ( -0.6830127018922180770, -0.6830127018922204085, -0.2588190451025213501 ) ) ;
#123900 = LINE ( 'NONE', #69525, #29383 ) ;
#123901 = EDGE_CURVE ( 'NONE', #1535, #87168, #19366, .T. ) ;
#123902 = DIRECTION ( 'NONE',  ( -0.000000000000000000, -0.000000000000000000, 1.000000000000000000 ) ) ;
#123903 = ADVANCED_FACE ( 'NONE', ( #107080 ), #108276, .T. ) ;
#123904 = PLANE ( 'NONE',  #58053 ) ;
#123905 = ORIENTED_EDGE ( 'NONE', *, *, #29849, .T. ) ;
#123906 = CARTESIAN_POINT ( 'NONE',  ( 10.04515773336659556, -21.74070752338405654, 21.72585301388586743 ) ) ;
#123907 = ORIENTED_EDGE ( 'NONE', *, *, #140127, .F. ) ;
#123908 = DIRECTION ( 'NONE',  ( 0.3543493200069162685, -0.000000000000000000, -0.9351131265310288487 ) ) ;
#123909 =( BOUNDED_CURVE ( )  B_SPLINE_CURVE ( 3, ( #57972, #135512, #89834, #110844 ),
 .UNSPECIFIED., .F., .T. ) 
 B_SPLINE_CURVE_WITH_KNOTS ( ( 4, 4 ),
 ( 0.8834430019029044789, 0.8929338002999919199 ),
 .UNSPECIFIED. ) 
 CURVE ( )  GEOMETRIC_REPRESENTATION_ITEM ( )  RATIONAL_B_SPLINE_CURVE ( ( 1.000000000000000000, 0.9999924937429014449, 0.9999924937429014449, 1.000000000000000000 ) ) 
 REPRESENTATION_ITEM ( '' )  );
#123910 = CARTESIAN_POINT ( 'NONE',  ( 28.79623647476855197, 7.934999999999990727, -1.457635852685135314E-15 ) ) ;
#123911 = VERTEX_POINT ( 'NONE', #29509 ) ;
#123912 = CARTESIAN_POINT ( 'NONE',  ( 79.82876352523145158, 0.000000000000000000, -6.109999999999999432 ) ) ;
#123913 = EDGE_CURVE ( 'NONE', #39694, #127061, #117924, .T. ) ;
#123914 = PLANE ( 'NONE',  #8798 ) ;
#123915 = CARTESIAN_POINT ( 'NONE',  ( -33.48921356237309510, -27.52281430457078670, 5.000000000000000000 ) ) ;
#123916 = EDGE_LOOP ( 'NONE', ( #76272, #27431, #65394 ) ) ;
#123917 = ORIENTED_EDGE ( 'NONE', *, *, #36727, .T. ) ;
#123918 = VERTEX_POINT ( 'NONE', #30979 ) ;
#123919 = CARTESIAN_POINT ( 'NONE',  ( -51.48921356237309510, -27.52281430457091460, 5.000000000000000000 ) ) ;
#123920 = DIRECTION ( 'NONE',  ( 0.7071067811865487940, -0.7071067811865463515, 0.000000000000000000 ) ) ;
#123921 = EDGE_CURVE ( 'NONE', #138262, #103456, #74487, .T. ) ;
#123922 = LINE ( 'NONE', #24578, #8042 ) ;
#123923 = DIRECTION ( 'NONE',  ( 1.000000000000000000, 0.000000000000000000, 0.000000000000000000 ) ) ;
#123924 = ORIENTED_EDGE ( 'NONE', *, *, #76989, .F. ) ;
#123925 = SURFACE_SIDE_STYLE ('',( #112325 ) ) ;
#123926 = DIRECTION ( 'NONE',  ( 0.7071067811865487940, 0.7071067811865463515, 0.000000000000000000 ) ) ;
#123927 = LINE ( 'NONE', #10139, #18711 ) ;
#123928 = ORIENTED_EDGE ( 'NONE', *, *, #75569, .T. ) ;
#123929 = EDGE_CURVE ( 'NONE', #142002, #104583, #82882, .T. ) ;
#123930 = PLANE ( 'NONE',  #100321 ) ;
#123931 = ORIENTED_EDGE ( 'NONE', *, *, #127304, .T. ) ;
#123933 = ORIENTED_EDGE ( 'NONE', *, *, #53272, .T. ) ;
#123932 = DIRECTION ( 'NONE',  ( -0.000000000000000000, 0.3543493200069153248, 0.9351131265310292928 ) ) ;
#123934 = VERTEX_POINT ( 'NONE', #137238 ) ;
#123935 = ADVANCED_FACE ( 'NONE', ( #93011 ), #115427, .F. ) ;
#123936 = CARTESIAN_POINT ( 'NONE',  ( 24.48921356237309510, -27.52281430457072631, 5.000000000000000000 ) ) ;
#123938 = EDGE_CURVE ( 'NONE', #2974, #92499, #1669, .T. ) ;
#123937 = DIRECTION ( 'NONE',  ( -0.7071067811865486830, 0.7071067811865464625, 0.000000000000000000 ) ) ;
#123939 = ORIENTED_EDGE ( 'NONE', *, *, #38986, .T. ) ;
#123940 = ORIENTED_EDGE ( 'NONE', *, *, #126033, .F. ) ;
#123941 = CARTESIAN_POINT ( 'NONE',  ( -7.171830600776422315, -11.24070752338416668, 4.000000000000000000 ) ) ;
#123942 = DIRECTION ( 'NONE',  ( -0.7071067811865486830, -0.7071067811865464625, 0.000000000000000000 ) ) ;
#123943 = ADVANCED_FACE ( 'NONE', ( #57552 ), #81452, .F. ) ;
#123944 = VECTOR ( 'NONE', #113817, 1000.000000000000227 ) ;
#123945 = DIRECTION ( 'NONE',  ( -0.6830127018922180770, -0.6830127018922204085, -0.2588190451025213501 ) ) ;
#123946 = CARTESIAN_POINT ( 'NONE',  ( 48.05836038379622011, -7.949999999999996625, -2.130196079827426203 ) ) ;
#123948 = FACE_OUTER_BOUND ( 'NONE', #24197, .T. ) ;
#123947 = VECTOR ( 'NONE', #73699, 1000.000000000000000 ) ;
#123949 = FACE_OUTER_BOUND ( 'NONE', #15032, .T. ) ;
#123950 = FACE_OUTER_BOUND ( 'NONE', #9089, .T. ) ;
#123951 = CARTESIAN_POINT ( 'NONE',  ( 16.60373647476855297, 5.808823158059036373, 5.808823158059032821 ) ) ;
#123952 = CARTESIAN_POINT ( 'NONE',  ( -4.001930566820951718, -22.22500000000000142, 4.500000000000000888 ) ) ;
#123953 = DIRECTION ( 'NONE',  ( 1.000000000000000000, 0.000000000000000000, 0.000000000000000000 ) ) ;
#123954 = CARTESIAN_POINT ( 'NONE',  ( 32.99999999999977263, -16.60178936734445543, 0.8616154019348262194 ) ) ;
#123955 = DIRECTION ( 'NONE',  ( -0.7071067811865486830, -0.7071067811865464625, 0.000000000000000000 ) ) ;
#123956 = ORIENTED_EDGE ( 'NONE', *, *, #35984, .F. ) ;
#123957 = EDGE_LOOP ( 'NONE', ( #142113, #95059, #18382, #13353 ) ) ;
#123958 = CARTESIAN_POINT ( 'NONE',  ( 91.70833333333334281, -3.974999999999999201, -6.884901960086287964 ) ) ;
#123959 = ORIENTED_EDGE ( 'NONE', *, *, #103565, .F. ) ;
#123960 = VECTOR ( 'NONE', #47831, 1000.000000000000000 ) ;
#123961 = VERTEX_POINT ( 'NONE', #91584 ) ;
#123962 = ORIENTED_EDGE ( 'NONE', *, *, #112591, .F. ) ;
#123963 = CARTESIAN_POINT ( 'NONE',  ( -2.510786437626908008, -27.52281430457053446, 5.000000000000000000 ) ) ;
#123964 = FACE_OUTER_BOUND ( 'NONE', #131526, .T. ) ;
#123965 = DIRECTION ( 'NONE',  ( -0.6830127018922181881, 0.6830127018922202975, -0.2588190451025214056 ) ) ;
#123966 = VERTEX_POINT ( 'NONE', #14734 ) ;
#123967 = LINE ( 'NONE', #26074, #92587 ) ;
#123968 = CARTESIAN_POINT ( 'NONE',  ( 34.92499999999998295, -1.487538124160511899, 4.000000000000000000 ) ) ;
#123969 = DIRECTION ( 'NONE',  ( 1.000000000000000000, 0.000000000000000000, 0.000000000000000000 ) ) ;
#123970 = DIRECTION ( 'NONE',  ( 0.7071067811865487940, 0.7071067811865463515, 0.000000000000000000 ) ) ;
#123971 = DIRECTION ( 'NONE',  ( -0.6830127018922180770, -0.6830127018922204085, -0.2588190451025213501 ) ) ;
#123972 = DIRECTION ( 'NONE',  ( 0.7071067811865486830, -0.7071067811865464625, -0.000000000000000000 ) ) ;
#123973 = PLANE ( 'NONE',  #17232 ) ;
#123974 = CARTESIAN_POINT ( 'NONE',  ( 15.29974487139158867, -27.71228299555216879, 4.000000000000000000 ) ) ;
#123975 = DIRECTION ( 'NONE',  ( 0.3543493200069162685, -0.000000000000000000, -0.9351131265310288487 ) ) ;
#123976 = CARTESIAN_POINT ( 'NONE',  ( 15.18398860626900237, 28.73617430169797871, 5.000000000000000000 ) ) ;
#123977 = VECTOR ( 'NONE', #26780, 1000.000000000000000 ) ;
#123978 = LINE ( 'NONE', #26785, #35303 ) ;
#123979 = ORIENTED_EDGE ( 'NONE', *, *, #24186, .F. ) ;
#123980 = ORIENTED_EDGE ( 'NONE', *, *, #24165, .T. ) ;
#123981 = VECTOR ( 'NONE', #116645, 1000.000000000000000 ) ;
#123982 = CARTESIAN_POINT ( 'NONE',  ( 115.7920968585647756, -5.291415217122921177, 3.054999999999999272 ) ) ;
#123983 = VERTEX_POINT ( 'NONE', #25594 ) ;
#123984 = AXIS2_PLACEMENT_3D ( 'NONE', #25382, #102973, #69654 ) ;
#123985 = ADVANCED_FACE ( 'NONE', ( #103849 ), #58299, .T. ) ;
#123986 = CARTESIAN_POINT ( 'NONE',  ( 99.72916666666665719, 7.950000000000001954, -2.130196079827421762 ) ) ;
#123987 =( GEOMETRIC_REPRESENTATION_CONTEXT ( 3 ) GLOBAL_UNCERTAINTY_ASSIGNED_CONTEXT ( ( #137470 ) ) GLOBAL_UNIT_ASSIGNED_CONTEXT ( ( #57085, #2651, #1905 ) ) REPRESENTATION_CONTEXT ( 'NONE', 'WORKASPACE' ) );
#123988 = PLANE ( 'NONE',  #3956 ) ;
#123989 = DIRECTION ( 'NONE',  ( 0.7071067811865486830, -0.7071067811865464625, -0.000000000000000000 ) ) ;
#123990 = CARTESIAN_POINT ( 'NONE',  ( 8.999999999999959144, 17.58746187583906817, 4.000000000000000000 ) ) ;
#123991 = CARTESIAN_POINT ( 'NONE',  ( 113.0787635252314516, -7.482591942790325086E-16, 6.109999999999998543 ) ) ;
#123992 = VERTEX_POINT ( 'NONE', #45962 ) ;
#123993 = ORIENTED_EDGE ( 'NONE', *, *, #21627, .T. ) ;
#123994 = CARTESIAN_POINT ( 'NONE',  ( 60.48921356237309510, -27.52281430457097500, 5.000000000000000000 ) ) ;
#123995 = CARTESIAN_POINT ( 'NONE',  ( 27.29177708983031181, -15.74070752338412049, 19.73771281079103801 ) ) ;
#123996 = ORIENTED_EDGE ( 'NONE', *, *, #63333, .T. ) ;
#123997 = ORIENTED_EDGE ( 'NONE', *, *, #143285, .T. ) ;
#123998 = EDGE_CURVE ( 'NONE', #84085, #82511, #123530, .T. ) ;
#123999 = EDGE_LOOP ( 'NONE', ( #37403, #141848, #136262, #129332 ) ) ;
#124000 = DIRECTION ( 'NONE',  ( 0.6830127018922180770, 0.6830127018922202975, -0.2588190451025213501 ) ) ;
#124001 = EDGE_CURVE ( 'NONE', #3062, #22300, #85542, .T. ) ;
#124002 = EDGE_CURVE ( 'NONE', #58222, #73971, #13995, .T. ) ;
#124003 = CARTESIAN_POINT ( 'NONE',  ( 27.18293019189811588, -1.637169565754158951, -6.109999999999998543 ) ) ;
#124004 = ORIENTED_EDGE ( 'NONE', *, *, #83746, .T. ) ;
#124006 = ORIENTED_EDGE ( 'NONE', *, *, #9406, .T. ) ;
#124005 = ADVANCED_FACE ( 'NONE', ( #48806 ), #24193, .F. ) ;
#124007 = PLANE ( 'NONE',  #75641 ) ;
#124008 = VERTEX_POINT ( 'NONE', #27030 ) ;
#124009 = ORIENTED_EDGE ( 'NONE', *, *, #1223, .T. ) ;
#124010 = ORIENTED_EDGE ( 'NONE', *, *, #132450, .F. ) ;
#124011 = FACE_OUTER_BOUND ( 'NONE', #98450, .T. ) ;
#124012 = EDGE_CURVE ( 'NONE', #128576, #137465, #35811, .T. ) ;
#124013 = LINE ( 'NONE', #24680, #10423 ) ;
#124014 = CARTESIAN_POINT ( 'NONE',  ( 9.183988606268997046, 28.73617430169793607, 5.000000000000000000 ) ) ;
#124015 = EDGE_LOOP ( 'NONE', ( #13388, #70453, #116737, #46308 ) ) ;
#124016 = FACE_OUTER_BOUND ( 'NONE', #19001, .T. ) ;
#124017 = CARTESIAN_POINT ( 'NONE',  ( 0.4892135623730947680, -27.52281430457055578, 5.000000000000000000 ) ) ;
#124018 = EDGE_CURVE ( 'NONE', #120303, #55061, #69872, .T. ) ;
#124019 = PLANE ( 'NONE',  #28127 ) ;
#124020 = FACE_BOUND ( 'NONE', #130270, .T. ) ;
#124021 = ORIENTED_EDGE ( 'NONE', *, *, #105643, .F. ) ;
#124022 = DIRECTION ( 'NONE',  ( -0.000000000000000000, 0.3543493200069153248, 0.9351131265310292928 ) ) ;
#124023 = DIRECTION ( 'NONE',  ( 0.000000000000000000, -1.000000000000000000, 0.000000000000000000 ) ) ;
#124024 = DIRECTION ( 'NONE',  ( -0.000000000000000000, 0.000000000000000000, 1.000000000000000000 ) ) ;
#124025 = ORIENTED_EDGE ( 'NONE', *, *, #126486, .F. ) ;
#124026 = DIRECTION ( 'NONE',  ( -0.6830127018922180770, -0.6830127018922204085, -0.2588190451025213501 ) ) ;
#124027 = ORIENTED_EDGE ( 'NONE', *, *, #134623, .T. ) ;
#124029 = ORIENTED_EDGE ( 'NONE', *, *, #26664, .F. ) ;
#124028 = ADVANCED_FACE ( 'NONE', ( #3805 ), #134389, .T. ) ;
#124030 = ORIENTED_EDGE ( 'NONE', *, *, #66140, .F. ) ;
#124031 = VECTOR ( 'NONE', #80951, 999.9999999999998863 ) ;
#124032 = CARTESIAN_POINT ( 'NONE',  ( 41.76626352523145158, 4.472830434245838482, -4.472830434245837594 ) ) ;
#124033 = ORIENTED_EDGE ( 'NONE', *, *, #108480, .F. ) ;
#124034 = CARTESIAN_POINT ( 'NONE',  ( -27.32816939922333077, 17.25929247661554200, 4.000000000000000000 ) ) ;
#124035 = VECTOR ( 'NONE', #98832, 1000.000000000000227 ) ;
#124036 = LINE ( 'NONE', #56684, #70560 ) ;
#124037 = EDGE_CURVE ( 'NONE', #54748, #62201, #79331, .T. ) ;
#124038 = ORIENTED_EDGE ( 'NONE', *, *, #142710, .T. ) ;
#124039 = LINE ( 'NONE', #137780, #88496 ) ;
#124040 = DIRECTION ( 'NONE',  ( 0.3543493200069162685, -0.000000000000000000, -0.9351131265310288487 ) ) ;
#124041 = ADVANCED_FACE ( 'NONE', ( #13279 ), #101741, .T. ) ;
#124042 = EDGE_CURVE ( 'NONE', #42749, #143546, #102481, .T. ) ;
#124043 = LINE ( 'NONE', #100853, #16098 ) ;
#124044 = DIRECTION ( 'NONE',  ( 1.000000000000000000, 0.000000000000000000, 0.000000000000000000 ) ) ;
#124045 = LINE ( 'NONE', #33494, #58673 ) ;
#124046 = ORIENTED_EDGE ( 'NONE', *, *, #44796, .F. ) ;
#124047 = ORIENTED_EDGE ( 'NONE', *, *, #37100, .T. ) ;
#124048 = ORIENTED_EDGE ( 'NONE', *, *, #12699, .T. ) ;
#124049 = ORIENTED_EDGE ( 'NONE', *, *, #27226, .T. ) ;
#124050 = ORIENTED_EDGE ( 'NONE', *, *, #142895, .F. ) ;
#124051 = EDGE_CURVE ( 'NONE', #9764, #130424, #80094, .T. ) ;
#124052 = ORIENTED_EDGE ( 'NONE', *, *, #119137, .T. ) ;
#124053 = LINE ( 'NONE', #66122, #14256 ) ;
#124054 = EDGE_CURVE ( 'NONE', #17089, #14082, #114043, .T. ) ;
#124055 = CARTESIAN_POINT ( 'NONE',  ( 0.9815526536432959137, 18.75929247661553134, 20.33588619593442814 ) ) ;
#124056 = ORIENTED_EDGE ( 'NONE', *, *, #44980, .F. ) ;
#124057 = LINE ( 'NONE', #60250, #44121 ) ;
#124058 = EDGE_LOOP ( 'NONE', ( #112078, #51569, #57514, #136215 ) ) ;
#124059 = VECTOR ( 'NONE', #91860, 1000.000000000000227 ) ;
#124060 = PLANE ( 'NONE',  #93075 ) ;
#124061 = CARTESIAN_POINT ( 'NONE',  ( 25.58790314143521982, 6.871911579029515771, 3.967499999999989146 ) ) ;
#124062 = VECTOR ( 'NONE', #115373, 1000.000000000000000 ) ;
#124063 = CARTESIAN_POINT ( 'NONE',  ( -36.48921356237310221, -27.52281430457080802, 5.000000000000000000 ) ) ;
#124064 = ORIENTED_EDGE ( 'NONE', *, *, #101005, .T. ) ;
#124066 = CARTESIAN_POINT ( 'NONE',  ( 10.49999999999992362, -17.91344420646041513, 1.358650452708489054 ) ) ;
#124065 = CARTESIAN_POINT ( 'NONE',  ( 114.0995968585647660, -6.109999999999998543, -1.637169565754160727 ) ) ;
#124067 = AXIS2_PLACEMENT_3D ( 'NONE', #24549, #25260, #12239 ) ;
#124068 = EDGE_CURVE ( 'NONE', #129470, #119697, #129920, .T. ) ;
#124069 = VECTOR ( 'NONE', #43546, 999.9999999999998863 ) ;
#124070 = CARTESIAN_POINT ( 'NONE',  ( -34.42500000000001137, -22.22500000000000142, 5.000000000000000000 ) ) ;
#124071 = LINE ( 'NONE', #68303, #16462 ) ;
#124072 = VERTEX_POINT ( 'NONE', #94421 ) ;
#124073 = DIRECTION ( 'NONE',  ( 0.7071067811865487940, -0.7071067811865463515, 0.000000000000000000 ) ) ;
#124075 = ORIENTED_EDGE ( 'NONE', *, *, #139680, .F. ) ;
#124074 = FACE_OUTER_BOUND ( 'NONE', #32542, .T. ) ;
#124076 = DIRECTION ( 'NONE',  ( 0.3543493200069162685, -0.000000000000000000, -0.9351131265310288487 ) ) ;
#124077 = VERTEX_POINT ( 'NONE', #128505 ) ;
#124078 = VECTOR ( 'NONE', #84882, 1000.000000000000000 ) ;
#124079 = DIRECTION ( 'NONE',  ( 0.6830127018922180770, -0.6830127018922204085, -0.2588190451025213501 ) ) ;
#124080 = EDGE_CURVE ( 'NONE', #120007, #127365, #30627, .T. ) ;
#124081 = CARTESIAN_POINT ( 'NONE',  ( -34.92500000000001137, -15.15525166281330627, -9.164774702225015446 ) ) ;
#124082 = CARTESIAN_POINT ( 'NONE',  ( 60.48921356237309510, -27.52281430457097500, 5.000000000000000000 ) ) ;
#124083 = EDGE_LOOP ( 'NONE', ( #32035, #102587, #142671, #42885 ) ) ;
#124084 = CARTESIAN_POINT ( 'NONE',  ( -10.82816939922344979, -14.24070752338413293, 4.000000000000000000 ) ) ;
#124085 = LINE ( 'NONE', #121209, #35235 ) ;
#124086 = ORIENTED_EDGE ( 'NONE', *, *, #29923, .F. ) ;
#124087 = CARTESIAN_POINT ( 'NONE',  ( 51.18398860626899705, 28.73617430169823095, 5.000000000000000000 ) ) ;
#124088 = ORIENTED_EDGE ( 'NONE', *, *, #121556, .T. ) ;
#124089 = DIRECTION ( 'NONE',  ( -0.3543493200069162685, -0.000000000000000000, -0.9351131265310288487 ) ) ;
#124091 = ORIENTED_EDGE ( 'NONE', *, *, #46016, .F. ) ;
#124090 = CARTESIAN_POINT ( 'NONE',  ( 34.42499999999998295, 14.97718569542923994, 5.000000000000000000 ) ) ;
#124092 = ORIENTED_EDGE ( 'NONE', *, *, #101057, .F. ) ;
#124093 = DIRECTION ( 'NONE',  ( -0.3543493200069162685, -0.000000000000000000, -0.9351131265310288487 ) ) ;
#124094 = ORIENTED_EDGE ( 'NONE', *, *, #60290, .T. ) ;
#124095 = ADVANCED_FACE ( 'NONE', ( #51659 ), #60410, .F. ) ;
#124096 = EDGE_CURVE ( 'NONE', #54960, #98193, #104595, .T. ) ;
#124097 = CARTESIAN_POINT ( 'NONE',  ( -45.18398860626900415, 28.73617430169818832, 5.000000000000000000 ) ) ;
#124098 = EDGE_LOOP ( 'NONE', ( #135988, #126828, #64864, #140678, #266 ) ) ;
#124099 = CARTESIAN_POINT ( 'NONE',  ( -15.18398860626900237, 28.73617430169797871, 5.000000000000000000 ) ) ;
#124100 = DIRECTION ( 'NONE',  ( 0.7071067811865486830, -0.7071067811865464625, -0.000000000000000000 ) ) ;
#124101 = CARTESIAN_POINT ( 'NONE',  ( -55.65468426144000347, -40.29840020119755195, 19.55137198191481218 ) ) ;
#124103 = VECTOR ( 'NONE', #68700, 1000.000000000000000 ) ;
#124102 = FACE_OUTER_BOUND ( 'NONE', #60396, .T. ) ;
#124104 = CARTESIAN_POINT ( 'NONE',  ( 126.4306647761266049, -6.963203063247377145, -0.9358753878083012623 ) ) ;
#124105 = CARTESIAN_POINT ( 'NONE',  ( 17.99999999999987566, -8.731860332648819778, -2.120594902707497287 ) ) ;
#124106 = ORIENTED_EDGE ( 'NONE', *, *, #35087, .T. ) ;
#124107 = ORIENTED_EDGE ( 'NONE', *, *, #6436, .F. ) ;
#124108 = ORIENTED_EDGE ( 'NONE', *, *, #4687, .T. ) ;
#124109 = CARTESIAN_POINT ( 'NONE',  ( 122.3333333333333286, -6.884901960086287964, 3.974999999999998312 ) ) ;
#124110 = ORIENTED_EDGE ( 'NONE', *, *, #48156, .F. ) ;
#124111 = ORIENTED_EDGE ( 'NONE', *, *, #43091, .T. ) ;
#124112 = ORIENTED_EDGE ( 'NONE', *, *, #114876, .T. ) ;
#124113 = CARTESIAN_POINT ( 'NONE',  ( 0.3933287082456937700, -7.643270253734883113, 1.126925465033841833 ) ) ;
#124114 = CARTESIAN_POINT ( 'NONE',  ( -30.32816939922331656, 2.259292476615690770, 4.000000000000000000 ) ) ;
#124115 = VERTEX_POINT ( 'NONE', #118307 ) ;
#124116 =( BOUNDED_SURFACE ( )  B_SPLINE_SURFACE ( 3, 2, ( 
 ( #21398, #41715, #65660 ),
 ( #111230, #10492, #131586 ),
 ( #43867, #85927, #130166 ),
 ( #141761, #42462, #48150 ) ),
 .UNSPECIFIED., .F., .F., .T. ) 
 B_SPLINE_SURFACE_WITH_KNOTS ( ( 4, 4 ),
 ( 3, 3 ),
 ( 0.000000000000000000, 0.001630001914283318388 ),
 ( 0.000000000000000000, 1.000000000000000000 ),
 .UNSPECIFIED. ) 
 GEOMETRIC_REPRESENTATION_ITEM ( )  RATIONAL_B_SPLINE_SURFACE ( (
 ( 1.000000000000000000, 0.7071067811865475727, 1.000000000000000000),
 ( 1.000000000000000000, 0.7121002461815024720, 1.000000000000000000),
 ( 1.000000000000000000, 0.7157206429707747564, 1.000000000000000000),
 ( 1.000000000000000000, 0.7180326832784528213, 1.000000000000000000) ) ) 
 REPRESENTATION_ITEM ( '' )  SURFACE ( )  );
#124117 = LINE ( 'NONE', #92914, #92481 ) ;
#124118 = DIRECTION ( 'NONE',  ( 0.7071067811865487940, -0.7071067811865463515, 0.000000000000000000 ) ) ;
#124119 = CARTESIAN_POINT ( 'NONE',  ( 12.19999999999999574, -60.26999999999998892, -39.50000000000000000 ) ) ;
#124120 = CARTESIAN_POINT ( 'NONE',  ( -2.292893218813436995, -9.740707523384184441, 5.000000000000000000 ) ) ;
#124121 = CARTESIAN_POINT ( 'NONE',  ( 120.0212635252314328, -4.472830434245839371, -4.472830434245840259 ) ) ;
#124122 = VERTEX_POINT ( 'NONE', #107441 ) ;
#124123 = CARTESIAN_POINT ( 'NONE',  ( 23.60898926630779826, -0.6778661889157658882, 4.000000000000000000 ) ) ;
#124124 = DIRECTION ( 'NONE',  ( -0.000000000000000000, 0.3543493200069153248, 0.9351131265310292928 ) ) ;
#124125 = CARTESIAN_POINT ( 'NONE',  ( 78.00000000000000000, 0.000000000000000000, -7.950000000000000178 ) ) ;
#124126 = CARTESIAN_POINT ( 'NONE',  ( 12.65494483745374588, 5.259292476615665457, 12.77922209995896807 ) ) ;
#124127 = CARTESIAN_POINT ( 'NONE',  ( 23.29289321881329400, 11.25929247661560417, 5.000000000000000000 ) ) ;
#124128 = CARTESIAN_POINT ( 'NONE',  ( 41.99451991528749062, 28.92564299267967343, 4.000000000000000000 ) ) ;
#124129 = FACE_OUTER_BOUND ( 'NONE', #63370, .T. ) ;
#124130 = CARTESIAN_POINT ( 'NONE',  ( 44.41252705046289151, -7.949999999999998401, -4.867971026610728450E-16 ) ) ;
#124131 = AXIS2_PLACEMENT_3D ( 'NONE', #46883, #70049, #12035 ) ;
#124132 = DIRECTION ( 'NONE',  ( -1.000000000000000000, 0.000000000000000000, -0.000000000000000000 ) ) ;
#124133 = PLANE ( 'NONE',  #80923 ) ;
#124134 = ORIENTED_EDGE ( 'NONE', *, *, #43374, .F. ) ;
#124135 = EDGE_LOOP ( 'NONE', ( #82104, #15970, #12321, #89219 ) ) ;
#124136 = CARTESIAN_POINT ( 'NONE',  ( 43.87500000000000000, 7.950000000000000178, 1.460391307983218535E-15 ) ) ;
#124137 = ORIENTED_EDGE ( 'NONE', *, *, #21201, .T. ) ;
#124138 = VECTOR ( 'NONE', #66594, 1000.000000000000000 ) ;
#124139 = DIRECTION ( 'NONE',  ( -0.6830127018922181881, 0.6830127018922202975, -0.2588190451025214056 ) ) ;
#124140 = EDGE_CURVE ( 'NONE', #8796, #98543, #50233, .T. ) ;
#124141 = ORIENTED_EDGE ( 'NONE', *, *, #89242, .T. ) ;
#124142 = CARTESIAN_POINT ( 'NONE',  ( 10.83999999999999986, 9.521314400968980422E-16, 0.000000000000000000 ) ) ;
#124143 = CARTESIAN_POINT ( 'NONE',  ( 66.48921356237309510, -27.52281430457101763, 5.000000000000000000 ) ) ;
#124144 = CARTESIAN_POINT ( 'NONE',  ( 36.60459685856475431, 1.637169565754164946, -6.109999999999999432 ) ) ;
#124146 = ORIENTED_EDGE ( 'NONE', *, *, #79142, .T. ) ;
#124145 = CONICAL_SURFACE ( 'NONE', #45429, 2.055000000000001048, 0.9599310885968758145 ) ;
#124147 = LINE ( 'NONE', #49487, #45660 ) ;
#124148 = ORIENTED_EDGE ( 'NONE', *, *, #54364, .T. ) ;
#124149 = DIRECTION ( 'NONE',  ( 0.7071067811865487940, 0.7071067811865463515, 0.000000000000000000 ) ) ;
#124150 = DIRECTION ( 'NONE',  ( 0.6830127018922180770, -0.6830127018922204085, -0.2588190451025213501 ) ) ;
#124151 = CARTESIAN_POINT ( 'NONE',  ( -33.48921356237309510, -27.52281430457078670, 5.000000000000000000 ) ) ;
#124152 = EDGE_CURVE ( 'NONE', #68414, #89048, #96537, .T. ) ;
#124153 = CARTESIAN_POINT ( 'NONE',  ( 39.18398860626899705, 28.73617430169814568, 5.000000000000000000 ) ) ;
#124154 = VERTEX_POINT ( 'NONE', #139405 ) ;
#124155 = VECTOR ( 'NONE', #125231, 1000.000000000000227 ) ;
#124156 = CARTESIAN_POINT ( 'NONE',  ( -42.48921356237308800, -27.52281430457085065, 5.000000000000000000 ) ) ;
#124157 = EDGE_CURVE ( 'NONE', #113425, #1274, #95856, .T. ) ;
#124158 = EDGE_CURVE ( 'NONE', #87398, #34254, #16882, .T. ) ;
#124159 = ORIENTED_EDGE ( 'NONE', *, *, #103369, .F. ) ;
#124160 = DIRECTION ( 'NONE',  ( 0.7071067811865487940, -0.7071067811865463515, 0.000000000000000000 ) ) ;
#124161 = CARTESIAN_POINT ( 'NONE',  ( -14.51078643762690490, -27.52281430457045275, 5.000000000000000000 ) ) ;
#124162 = LINE ( 'NONE', #37894, #63943 ) ;
#124163 = CARTESIAN_POINT ( 'NONE',  ( 27.00548008471251293, 28.92564299267919381, 4.000000000000000000 ) ) ;
#124164 = DIRECTION ( 'NONE',  ( -0.7071067811865486830, 0.7071067811865464625, 0.000000000000000000 ) ) ;
#124165 = VECTOR ( 'NONE', #26449, 999.9999999999998863 ) ;
#124167 = ADVANCED_FACE ( 'NONE', ( #61155 ), #82865, .T. ) ;
#124166 = VECTOR ( 'NONE', #130059, 999.9999999999998863 ) ;
#124168 = EDGE_CURVE ( 'NONE', #82994, #11548, #95135, .T. ) ;
#124169 = PRESENTATION_LAYER_ASSIGNMENT (  '', '', ( #135656 ) ) ;
#124170 = FACE_OUTER_BOUND ( 'NONE', #121356, .T. ) ;
#124171 = CARTESIAN_POINT ( 'NONE',  ( 54.74543019189812298, -5.291415217122918513, -3.055000000000000160 ) ) ;
#124172 = CARTESIAN_POINT ( 'NONE',  ( -24.99941145866615244, 2.672864951410426126, 4.679979323531659574 ) ) ;
#124173 = EDGE_CURVE ( 'NONE', #47805, #46388, #8108, .T. ) ;
#124174 = CARTESIAN_POINT ( 'NONE',  ( 0.000000000000000000, -2.375000000000000000, 1.069999999999998508 ) ) ;
#124176 = ORIENTED_EDGE ( 'NONE', *, *, #6927, .T. ) ;
#124175 = DIRECTION ( 'NONE',  ( 0.000000000000000000, -1.000000000000000000, 0.000000000000000000 ) ) ;
#124177 = ORIENTED_EDGE ( 'NONE', *, *, #34017, .F. ) ;
#124178 = AXIS2_PLACEMENT_3D ( 'NONE', #5141, #22782, #115321 ) ;
#124179 = DIRECTION ( 'NONE',  ( -0.000000000000000000, 0.3543493200069153248, 0.9351131265310292928 ) ) ;
#124180 = ORIENTED_EDGE ( 'NONE', *, *, #89271, .F. ) ;
#124181 = EDGE_CURVE ( 'NONE', #91814, #70943, #105303, .T. ) ;
#124182 = CARTESIAN_POINT ( 'NONE',  ( 34.36534788329977630, 22.27000000000001378, -12.13892467737981740 ) ) ;
#124183 = ORIENTED_EDGE ( 'NONE', *, *, #21260, .F. ) ;
#124184 = SURFACE_SIDE_STYLE ('',( #81424 ) ) ;
#124185 = DIRECTION ( 'NONE',  ( -0.7071067811865487940, 0.7071067811865463515, -0.000000000000000000 ) ) ;
#124186 = FACE_BOUND ( 'NONE', #5502, .T. ) ;
#124187 = LINE ( 'NONE', #90871, #31715 ) ;
#124188 = CARTESIAN_POINT ( 'NONE',  ( 13.13598696172163116, -2.500000000000000444, 3.061616997868384127E-16 ) ) ;
#124189 = LINE ( 'NONE', #68421, #103473 ) ;
#124190 = CARTESIAN_POINT ( 'NONE',  ( 81.48921356237309510, -27.52281430457112066, 5.000000000000000000 ) ) ;
#124192 = ORIENTED_EDGE ( 'NONE', *, *, #98673, .F. ) ;
#124191 = CARTESIAN_POINT ( 'NONE',  ( -8.999999999999932498, -7.447814304570754551, 5.000000000000000000 ) ) ;
#124193 = ADVANCED_FACE ( 'NONE', ( #84308 ), #29873, .T. ) ;
#124194 = ORIENTED_EDGE ( 'NONE', *, *, #115277, .F. ) ;
#124195 = CARTESIAN_POINT ( 'NONE',  ( -7.140000000000000568, -35.07067781378390237, 17.84983973653577749 ) ) ;
#124196 = ITEM_DEFINED_TRANSFORMATION ( 'NONE', 'NONE', #72535,  #127880 ) ;
#124197 = ORIENTED_EDGE ( 'NONE', *, *, #126830, .F. ) ;
#124198 = VERTEX_POINT ( 'NONE', #63278 ) ;
#124199 = CARTESIAN_POINT ( 'NONE',  ( 73.41209685856478018, 5.291415217122921177, -3.054999999999994831 ) ) ;
#124200 = EDGE_LOOP ( 'NONE', ( #101700, #37525, #93960, #27346 ) ) ;
#124201 = CARTESIAN_POINT ( 'NONE',  ( -27.18398860626900060, 28.73617430169806042, 5.000000000000000000 ) ) ;
#124202 = ADVANCED_FACE ( 'NONE', ( #61832 ), #105992, .F. ) ;
#124203 = ORIENTED_EDGE ( 'NONE', *, *, #51739, .F. ) ;
#124204 = DIRECTION ( 'NONE',  ( 1.000000000000000000, 3.115803279706882722E-16, -0.000000000000000000 ) ) ;
#124205 = VECTOR ( 'NONE', #140712, 1000.000000000000227 ) ;
#124206 = CARTESIAN_POINT ( 'NONE',  ( 63.48921356237309510, -27.52281430457099631, 5.000000000000000000 ) ) ;
#124207 = EDGE_CURVE ( 'NONE', #74246, #108986, #18262, .T. ) ;
#124208 = CARTESIAN_POINT ( 'NONE',  ( -23.99451991528749062, 28.92564299267954908, 4.000000000000000000 ) ) ;
#124209 = CARTESIAN_POINT ( 'NONE',  ( 102.5000000000000142, 0.000000000000000000, -7.950000000000000178 ) ) ;
#124210 = DIRECTION ( 'NONE',  ( 0.000000000000000000, 0.000000000000000000, 1.000000000000000000 ) ) ;
#124211 = EDGE_CURVE ( 'NONE', #63098, #83424, #88577, .T. ) ;
#124212 = LINE ( 'NONE', #48093, #91035 ) ;
#124213 = CARTESIAN_POINT ( 'NONE',  ( 21.81246187583931473, -22.22500000000000142, 4.000000000000000000 ) ) ;
#124214 = EDGE_LOOP ( 'NONE', ( #91793, #43458, #31143, #54471 ) ) ;
#124215 = AXIS2_PLACEMENT_3D ( 'NONE', #35885, #90967, #133745 ) ;
#124216 = VERTEX_POINT ( 'NONE', #142247 ) ;
#124217 = CARTESIAN_POINT ( 'NONE',  ( -18.63311396761903538, -2.779424156541560276, 4.000000000000000000 ) ) ;
#124218 = DIRECTION ( 'NONE',  ( 0.6830127018922181881, 0.6830127018922202975, -0.2588190451025214056 ) ) ;
#124219 = VERTEX_POINT ( 'NONE', #63960 ) ;
#124220 = EDGE_CURVE ( 'NONE', #128218, #101990, #130658, .T. ) ;
#124221 = ORIENTED_EDGE ( 'NONE', *, *, #85086, .T. ) ;
#124222 = ORIENTED_EDGE ( 'NONE', *, *, #46410, .F. ) ;
#124223 = CARTESIAN_POINT ( 'NONE',  ( 26.25043019189810067, 3.055000000000002824, -5.291415217122919401 ) ) ;
#124224 = ORIENTED_EDGE ( 'NONE', *, *, #16668, .F. ) ;
#124225 = LINE ( 'NONE', #55414, #13859 ) ;
#124226 = VECTOR ( 'NONE', #48243, 1000.000000000000000 ) ;
#124227 = CARTESIAN_POINT ( 'NONE',  ( 43.53752705046289151, -9.735942053221456900E-16, 7.949999999999998401 ) ) ;
#124228 = CARTESIAN_POINT ( 'NONE',  ( -0.6620968585647807325, -6.871911579029513106, -3.967499999999993587 ) ) ;
#124229 = CARTESIAN_POINT ( 'NONE',  ( 1.828169399223519065, -14.24070752338414358, 4.000000000000000000 ) ) ;
#124230 = ORIENTED_EDGE ( 'NONE', *, *, #83000, .F. ) ;
#124231 = VECTOR ( 'NONE', #11450, 1000.000000000000114 ) ;
#124232 = ADVANCED_FACE ( 'NONE', ( #132810 ), #22546, .F. ) ;
#124233 = FACE_OUTER_BOUND ( 'NONE', #8130, .T. ) ;
#124234 = CARTESIAN_POINT ( 'NONE',  ( -17.57538274164440040, -2.608983483842240325, 5.000000000000000000 ) ) ;
#124235 = FACE_OUTER_BOUND ( 'NONE', #57918, .T. ) ;
#124237 = VERTEX_POINT ( 'NONE', #98703 ) ;
#124236 = LINE ( 'NONE', #24221, #91167 ) ;
#124238 = ORIENTED_EDGE ( 'NONE', *, *, #16352, .T. ) ;
#124239 = FACE_OUTER_BOUND ( 'NONE', #21421, .T. ) ;
#124240 = DIRECTION ( 'NONE',  ( 1.000000000000000000, 0.000000000000000000, 0.000000000000000000 ) ) ;
#124241 = FACE_OUTER_BOUND ( 'NONE', #102564, .T. ) ;
#124242 = ORIENTED_EDGE ( 'NONE', *, *, #78913, .T. ) ;
#124243 =( NAMED_UNIT ( * ) SI_UNIT ( $, .STERADIAN. ) SOLID_ANGLE_UNIT ( ) );
#124244 = CARTESIAN_POINT ( 'NONE',  ( -6.499999999999999112, 0.000000000000000000, -10.00000000000000000 ) ) ;
#124245 = EDGE_CURVE ( 'NONE', #67596, #128513, #87132, .T. ) ;
#124246 = VECTOR ( 'NONE', #4670, 1000.000000000000000 ) ;
#124247 = CARTESIAN_POINT ( 'NONE',  ( 28.27083333333332860, -7.949999999999998401, -2.130196079827426203 ) ) ;
#124248 = CARTESIAN_POINT ( 'NONE',  ( -11.67183060077638856, 20.25929247661551003, 4.000000000000000000 ) ) ;
#124249 = ORIENTED_EDGE ( 'NONE', *, *, #102605, .F. ) ;
#124250 = CARTESIAN_POINT ( 'NONE',  ( 26.99999999999981171, -11.35517001088070010, -1.126524801160046607 ) ) ;
#124251 = CARTESIAN_POINT ( 'NONE',  ( 52.26932219902325727, -52.14999999999999147, 40.92499999999998295 ) ) ;
#124252 = CARTESIAN_POINT ( 'NONE',  ( 22.21247294953710494, 0.000000000000000000, 6.094999999999989981 ) ) ;
#124253 = CARTESIAN_POINT ( 'NONE',  ( 17.70174076595082369, 22.22500000000000142, 24.94223936709560974 ) ) ;
#124254 = VECTOR ( 'NONE', #89569, 1000.000000000000000 ) ;
#124255 = LINE ( 'NONE', #134436, #110809 ) ;
#124256 = ORIENTED_EDGE ( 'NONE', *, *, #58413, .F. ) ;
#124257 = VERTEX_POINT ( 'NONE', #42219 ) ;
#124258 = LINE ( 'NONE', #13333, #60995 ) ;
#124259 = VECTOR ( 'NONE', #98658, 1000.000000000000000 ) ;
#124260 = AXIS2_PLACEMENT_3D ( 'NONE', #53010, #40742, #61119 ) ;
#124261 =( NAMED_UNIT ( * ) PLANE_ANGLE_UNIT ( ) SI_UNIT ( $, .RADIAN. ) );
#124262 = CARTESIAN_POINT ( 'NONE',  ( -31.49999999999977263, 13.56627193232213102, -10.57019076586075990 ) ) ;
#124263 = ADVANCED_FACE ( 'NONE', ( #89272 ), #9533, .F. ) ;
#124264 = AXIS2_PLACEMENT_3D ( 'NONE', #24123, #135743, #79970 ) ;
#124265 = CARTESIAN_POINT ( 'NONE',  ( -30.29974487139158867, -27.71228299555227537, 4.000000000000000000 ) ) ;
#124266 = PLANE ( 'NONE',  #1989 ) ;
#124267 = DIRECTION ( 'NONE',  ( -0.7071067811865487940, 0.7071067811865463515, 0.000000000000000000 ) ) ;
#124268 = EDGE_CURVE ( 'NONE', #86675, #60444, #32032, .T. ) ;
#124269 = ORIENTED_EDGE ( 'NONE', *, *, #126924, .F. ) ;
#124270 = CARTESIAN_POINT ( 'NONE',  ( -57.48921356237308800, -27.52281430457095368, 5.000000000000000000 ) ) ;
#124271 = UNCERTAINTY_MEASURE_WITH_UNIT (LENGTH_MEASURE( 1.000000000000000082E-05 ), #105053, 'distance_accuracy_value', 'NONE');
#124272 = CARTESIAN_POINT ( 'NONE',  ( 26.40000000000000568, -16.48000000000005016, 12.69999999999954454 ) ) ;
#124273 = AXIS2_PLACEMENT_3D ( 'NONE', #133931, #34618, #123064 ) ;
#124274 = DIRECTION ( 'NONE',  ( 0.6830127018922181881, 0.6830127018922202975, -0.2588190451025214056 ) ) ;
#124275 = CARTESIAN_POINT ( 'NONE',  ( 60.14126352523143737, 4.472830434245837594, 4.472830434245841147 ) ) ;
#124276 = EDGE_CURVE ( 'NONE', #43467, #90522, #121169, .T. ) ;
#124277 = LINE ( 'NONE', #110517, #67267 ) ;
#124278 = ADVANCED_FACE ( 'NONE', ( #8792 ), #66806, .F. ) ;
#124279 = DIRECTION ( 'NONE',  ( -0.000000000000000000, 0.3543493200069153248, 0.9351131265310292928 ) ) ;
#124280 = DIRECTION ( 'NONE',  ( -0.000000000000000000, -0.3543493200069152693, 0.9351131265310292928 ) ) ;
#124281 = ORIENTED_EDGE ( 'NONE', *, *, #8467, .F. ) ;
#124282 = DIRECTION ( 'NONE',  ( 0.5735764363510453823, -0.8191520442889923537, 1.003171929053525486E-16 ) ) ;
#124283 = ORIENTED_EDGE ( 'NONE', *, *, #130390, .T. ) ;
#124284 = LINE ( 'NONE', #91655, #19989 ) ;
#124285 = DIRECTION ( 'NONE',  ( 0.7071067811865487940, 0.7071067811865463515, -0.000000000000000000 ) ) ;
#124286 = CARTESIAN_POINT ( 'NONE',  ( 33.03752705046289151, -9.735942053221456900E-16, 7.949999999999998401 ) ) ;
#124287 = DIRECTION ( 'NONE',  ( -0.7071067811865486830, 0.7071067811865464625, 0.000000000000000000 ) ) ;
#124288 = EDGE_CURVE ( 'NONE', #99410, #114108, #132080, .T. ) ;
#124289 = DIRECTION ( 'NONE',  ( -0.3543493200069162685, -0.000000000000000000, -0.9351131265310288487 ) ) ;
#124290 = FACE_OUTER_BOUND ( 'NONE', #47872, .T. ) ;
#124291 = VERTEX_POINT ( 'NONE', #11667 ) ;
#124292 = VERTEX_POINT ( 'NONE', #20417 ) ;
#124293 = DIRECTION ( 'NONE',  ( 1.000000000000000000, -0.000000000000000000, -0.000000000000000000 ) ) ;
#124294 = LINE ( 'NONE', #69218, #32999 ) ;
#124295 = AXIS2_PLACEMENT_3D ( 'NONE', #130670, #141530, #77706 ) ;
#124296 = LINE ( 'NONE', #125008, #84432 ) ;
#124297 =( BOUNDED_CURVE ( )  B_SPLINE_CURVE ( 2, ( #81911, #38370, #47855, #48526, #71724, #28206, #139117, #15158, #49273, #60880, #116633, #115167, #59438 ),
 .UNSPECIFIED., .F., .T. ) 
 B_SPLINE_CURVE_WITH_KNOTS ( ( 3, 2, 2, 2, 2, 2, 3 ),
 ( 0.7000000000000000666, 0.7083333333333334814, 0.7166666666666667851, 0.7250000000000000888, 0.7333333333333333925, 0.7416666666666668073, 0.7500000000000001110 ),
 .UNSPECIFIED. ) 
 CURVE ( )  GEOMETRIC_REPRESENTATION_ITEM ( )  RATIONAL_B_SPLINE_CURVE ( ( 0.9999999999999995559, 0.9659258262890687563, 1.000000000000000000, 0.9659258262890683122, 1.000000000000000000, 0.9659258262890683122, 1.000000000000000000, 0.9659258262890683122, 1.000000000000000000, 0.9659258262890683122, 1.000000000000000000, 0.9659258262890678681, 1.000000000000000444 ) ) 
 REPRESENTATION_ITEM ( '' )  );
#124298 = CARTESIAN_POINT ( 'NONE',  ( -5.700255128608413102, -27.71228299555201957, 4.000000000000000000 ) ) ;
#124299 = CARTESIAN_POINT ( 'NONE',  ( 79.12086038379622721, -6.884901960086286188, 3.974999999999997424 ) ) ;
#124300 = DIRECTION ( 'NONE',  ( 1.000000000000000000, 0.000000000000000000, 0.000000000000000000 ) ) ;
#124301 = VECTOR ( 'NONE', #114081, 1000.000000000000000 ) ;
#124302 = LINE ( 'NONE', #46060, #73771 ) ;
#124303 = ORIENTED_EDGE ( 'NONE', *, *, #93232, .T. ) ;
#124304 = CARTESIAN_POINT ( 'NONE',  ( 76.25000000000000000, -9.735942053221458872E-16, 7.950000000000000178 ) ) ;
#124305 = PLANE ( 'NONE',  #142008 ) ;
#124306 = LINE ( 'NONE', #101840, #20787 ) ;
#124307 = LINE ( 'NONE', #46808, #70606 ) ;
#124308 = VECTOR ( 'NONE', #18944, 1000.000000000000000 ) ;
#124309 = ORIENTED_EDGE ( 'NONE', *, *, #101467, .T. ) ;
#124310 = DIRECTION ( 'NONE',  ( -0.3543493200069162685, -0.000000000000000000, -0.9351131265310288487 ) ) ;
#124311 = PLANE ( 'NONE',  #62872 ) ;
#124312 = CARTESIAN_POINT ( 'NONE',  ( 65.18793019189811844, 6.110000000000002984, -1.637169565754156730 ) ) ;
#124313 = VECTOR ( 'NONE', #21047, 1000.000000000000000 ) ;
#124314 = DIRECTION ( 'NONE',  ( 0.3543493200069162685, -0.000000000000000000, -0.9351131265310288487 ) ) ;
#124315 = ORIENTED_EDGE ( 'NONE', *, *, #42669, .F. ) ;
#124316 = ORIENTED_EDGE ( 'NONE', *, *, #106284, .F. ) ;
#124317 = ADVANCED_FACE ( 'NONE', ( #43614 ), #110279, .T. ) ;
#124318 = CARTESIAN_POINT ( 'NONE',  ( 26.99999999999981526, 12.83542986846999590, -1.025386466790432438 ) ) ;
#124319 = FACE_OUTER_BOUND ( 'NONE', #128999, .T. ) ;
#124320 = CARTESIAN_POINT ( 'NONE',  ( -17.99999999999986855, -8.151047557385087572, -8.977947279169756101 ) ) ;
#124321 = DIRECTION ( 'NONE',  ( 0.6830127018922180770, -0.6830127018922204085, -0.2588190451025213501 ) ) ;
#124322 = EDGE_CURVE ( 'NONE', #92341, #54868, #21151, .T. ) ;
#124324 = ORIENTED_EDGE ( 'NONE', *, *, #96467, .T. ) ;
#124323 = CARTESIAN_POINT ( 'NONE',  ( 66.18398860626901126, 28.73617430169833753, 5.000000000000000000 ) ) ;
#124325 = CARTESIAN_POINT ( 'NONE',  ( 14.67183060077636725, -9.740707523384175559, 4.000000000000000000 ) ) ;
#124326 = CARTESIAN_POINT ( 'NONE',  ( 72.18398860626899705, 28.73617430169837661, 5.000000000000000000 ) ) ;
#124327 = CARTESIAN_POINT ( 'NONE',  ( 127.0000000000000000, 7.776507174585694135E-16, -6.350000000000001421 ) ) ;
#124328 = CARTESIAN_POINT ( 'NONE',  ( 39.29974487139159578, -27.71228299555233576, 4.000000000000000000 ) ) ;
#124329 = ORIENTED_EDGE ( 'NONE', *, *, #40608, .F. ) ;
#124330 = EDGE_CURVE ( 'NONE', #101812, #140709, #65408, .T. ) ;
#124331 = AXIS2_PLACEMENT_3D ( 'NONE', #58297, #91582, #135803 ) ;
#124333 = EDGE_LOOP ( 'NONE', ( #11346, #25870, #92778, #63450, #77049, #1306 ) ) ;
#124332 = ADVANCED_FACE ( 'NONE', ( #100156 ), #131617, .T. ) ;
#124334 = ADVANCED_FACE ( 'NONE', ( #78399 ), #10263, .T. ) ;
#124335 = CARTESIAN_POINT ( 'NONE',  ( 57.16709685856477563, -3.055000000000000160, -5.291415217122921177 ) ) ;
#124336 = EDGE_LOOP ( 'NONE', ( #79670, #100000, #19654, #98711, #25179 ) ) ;
#124337 = ADVANCED_FACE ( 'NONE', ( #44368, #54523 ), #64667, .T. ) ;
#124338 = VECTOR ( 'NONE', #45405, 1000.000000000000227 ) ;
#124339 = LINE ( 'NONE', #122176, #10490 ) ;
#124340 = CARTESIAN_POINT ( 'NONE',  ( -17.99999999999987566, -5.527737879153209910, -7.983877177622330734 ) ) ;
#124341 = ADVANCED_FACE ( 'NONE', ( #111741 ), #80555, .T. ) ;
#124342 = CARTESIAN_POINT ( 'NONE',  ( 5.816011393731002066, 28.73617430169783304, 5.000000000000000000 ) ) ;
#124343 = LINE ( 'NONE', #69266, #91853 ) ;
#124344 = ORIENTED_EDGE ( 'NONE', *, *, #65304, .T. ) ;
#124345 = ORIENTED_EDGE ( 'NONE', *, *, #36098, .T. ) ;
#124346 = ADVANCED_FACE ( 'NONE', ( #15242 ), #3637, .F. ) ;
#124347 = CARTESIAN_POINT ( 'NONE',  ( -20.36090904532357015, -2.649219295539896990, 4.327832195654618630 ) ) ;
#124348 = CARTESIAN_POINT ( 'NONE',  ( -16.73819859380873609, 0.09982356673932113456, -33.96774470396684364 ) ) ;
#124349 = EDGE_CURVE ( 'NONE', #57164, #2746, #69691, .T. ) ;
#124350 = ORIENTED_EDGE ( 'NONE', *, *, #33227, .T. ) ;
#124351 = CARTESIAN_POINT ( 'NONE',  ( -29.29289321881324426, 2.259292476615688994, 5.000000000000000000 ) ) ;
#124352 = ORIENTED_EDGE ( 'NONE', *, *, #25896, .F. ) ;
#124353 = CARTESIAN_POINT ( 'NONE',  ( 17.99451991528748351, 28.92564299267950645, 4.000000000000000000 ) ) ;
#124354 = PLANE ( 'NONE',  #121173 ) ;
#124355 = ORIENTED_EDGE ( 'NONE', *, *, #142233, .F. ) ;
#124356 = ADVANCED_FACE ( 'NONE', ( #67545 ), #46531, .T. ) ;
#124357 = CIRCLE ( 'NONE', #17840, 2.500000000000000888 ) ;
#124358 = FACE_BOUND ( 'NONE', #64369, .T. ) ;
#124359 = CARTESIAN_POINT ( 'NONE',  ( 28.17183060077627843, -11.24070752338417201, 4.000000000000000000 ) ) ;
#124360 = FACE_OUTER_BOUND ( 'NONE', #45782, .T. ) ;
#124361 = DIRECTION ( 'NONE',  ( -0.000000000000000000, 0.000000000000000000, 1.000000000000000000 ) ) ;
#124362 = CARTESIAN_POINT ( 'NONE',  ( 9.489213562373095101, -27.52281430457062328, 5.000000000000000000 ) ) ;
#124363 = EDGE_CURVE ( 'NONE', #56202, #12987, #113870, .T. ) ;
#124364 = AXIS2_PLACEMENT_3D ( 'NONE', #123505, #67704, #21999 ) ;
#124365 = AXIS2_PLACEMENT_3D ( 'NONE', #142036, #12198, #67323 ) ;
#124366 = DIRECTION ( 'NONE',  ( -0.7071067811865486830, -0.7071067811865464625, -0.000000000000000000 ) ) ;
#124367 = CARTESIAN_POINT ( 'NONE',  ( -74.54871988794029392, 18.06436050938311411, -10.38815185181645973 ) ) ;
#124368 = ORIENTED_EDGE ( 'NONE', *, *, #72059, .T. ) ;
#124369 = AXIS2_PLACEMENT_3D ( 'NONE', #43556, #87778, #12343 ) ;
#124370 = ORIENTED_EDGE ( 'NONE', *, *, #16713, .T. ) ;
#124371 = CARTESIAN_POINT ( 'NONE',  ( 106.2245968585647802, -1.637169565754160949, 6.109999999999997655 ) ) ;
#124372 = ORIENTED_EDGE ( 'NONE', *, *, #41510, .F. ) ;
#124373 = DIRECTION ( 'NONE',  ( -0.7071067811865487940, 0.7071067811865463515, 0.000000000000000000 ) ) ;
#124374 = ORIENTED_EDGE ( 'NONE', *, *, #45865, .F. ) ;
#124375 = VECTOR ( 'NONE', #53160, 1000.000000000000000 ) ;
#124376 = DIRECTION ( 'NONE',  ( -0.7071067811865487940, 0.7071067811865463515, -0.000000000000000000 ) ) ;
#124377 = CARTESIAN_POINT ( 'NONE',  ( 0.000000000000000000, 7.776507174585692163E-16, -6.349999999999999645 ) ) ;
#124378 = DIRECTION ( 'NONE',  ( -0.3543493200069162685, -0.000000000000000000, -0.9351131265310288487 ) ) ;
#124379 = ORIENTED_EDGE ( 'NONE', *, *, #77335, .F. ) ;
#124380 = CARTESIAN_POINT ( 'NONE',  ( -6.349999999999999645, 0.000000000000000000, 0.000000000000000000 ) ) ;
#124381 = CARTESIAN_POINT ( 'NONE',  ( 2.999999999999975131, 10.93112307739207267, 4.000000000000000000 ) ) ;
#124382 = LINE ( 'NONE', #35268, #79836 ) ;
#124383 = EDGE_CURVE ( 'NONE', #22013, #68609, #110516, .T. ) ;
#124384 = CARTESIAN_POINT ( 'NONE',  ( 16.83455439249994612, 8.717631302929021331, 5.000000000000000000 ) ) ;
#124385 = CARTESIAN_POINT ( 'NONE',  ( 26.99999999999981526, -10.77435723561691994, -9.972017380717289825 ) ) ;
#124386 = EDGE_LOOP ( 'NONE', ( #72581, #109532, #100081, #89423 ) ) ;
#124387 = LINE ( 'NONE', #82328, #79692 ) ;
#124388 = EDGE_CURVE ( 'NONE', #116079, #98487, #47254, .T. ) ;
#124389 = DIRECTION ( 'NONE',  ( -0.7071067811865486830, 0.7071067811865464625, 0.000000000000000000 ) ) ;
#124390 = VERTEX_POINT ( 'NONE', #59521 ) ;
#124391 = ORIENTED_EDGE ( 'NONE', *, *, #30946, .F. ) ;
#124392 = ORIENTED_EDGE ( 'NONE', *, *, #135644, .T. ) ;
#124393 = CARTESIAN_POINT ( 'NONE',  ( 58.91709685856477563, 3.054999999999998828, 5.291415217122922066 ) ) ;
#124394 = VECTOR ( 'NONE', #80057, 1000.000000000000227 ) ;
#124395 = ORIENTED_EDGE ( 'NONE', *, *, #115823, .T. ) ;
#124396 = EDGE_CURVE ( 'NONE', #107388, #22970, #103677, .T. ) ;
#124397 = AXIS2_PLACEMENT_3D ( 'NONE', #1378, #80424, #25288 ) ;
#124398 = CARTESIAN_POINT ( 'NONE',  ( 6.754139616203771901, 3.047499999999993214, -5.278424836066146320 ) ) ;
#124399 = CARTESIAN_POINT ( 'NONE',  ( 88.95876352523143282, 0.000000000000000000, -6.110000000000001208 ) ) ;
#124400 = CARTESIAN_POINT ( 'NONE',  ( -1.499999999999990896, 19.39370406404967184, 1.459788787078205141 ) ) ;
#124401 = ORIENTED_EDGE ( 'NONE', *, *, #17851, .F. ) ;
#124402 = EDGE_CURVE ( 'NONE', #19621, #117948, #134213, .T. ) ;
#124403 = CARTESIAN_POINT ( 'NONE',  ( -17.51078643762690845, -27.52281430457043143, 5.000000000000000000 ) ) ;
#124404 = ORIENTED_EDGE ( 'NONE', *, *, #139180, .F. ) ;
#124405 = CIRCLE ( 'NONE', #128959, 9.119999999999999218 ) ;
#124406 = DIRECTION ( 'NONE',  ( 0.7071067811865487940, -0.7071067811865463515, 0.000000000000000000 ) ) ;
#124407 = ORIENTED_EDGE ( 'NONE', *, *, #133262, .F. ) ;
#124408 = DIRECTION ( 'NONE',  ( 0.7071067811865486830, -0.7071067811865464625, -0.000000000000000000 ) ) ;
#124409 = LINE ( 'NONE', #103348, #66868 ) ;
#124410 = CARTESIAN_POINT ( 'NONE',  ( 125.1829301918981372, -1.637169565754159173, -6.109999999999999432 ) ) ;
#124411 = ORIENTED_EDGE ( 'NONE', *, *, #105342, .T. ) ;
#124412 = LINE ( 'NONE', #44764, #75834 ) ;
#124413 = EDGE_LOOP ( 'NONE', ( #126987, #101999, #71913, #29183 ) ) ;
#124414 = ORIENTED_EDGE ( 'NONE', *, *, #49900, .T. ) ;
#124415 = EDGE_LOOP ( 'NONE', ( #31048, #112980, #14663, #142537 ) ) ;
#124417 = VECTOR ( 'NONE', #122497, 1000.000000000000000 ) ;
#124416 = LINE ( 'NONE', #48280, #132724 ) ;
#124418 = DIRECTION ( 'NONE',  ( 0.6830127018922180770, -0.6830127018922204085, -0.2588190451025213501 ) ) ;
#124419 = DIRECTION ( 'NONE',  ( 0.6830127018922181881, 0.6830127018922202975, -0.2588190451025214056 ) ) ;
#124420 = EDGE_CURVE ( 'NONE', #44265, #45274, #123349, .T. ) ;
#124421 = CARTESIAN_POINT ( 'NONE',  ( -34.92500000000001137, 22.22500000000000142, 0.4999999999999995559 ) ) ;
#124422 = EDGE_CURVE ( 'NONE', #13073, #89747, #4320, .T. ) ;
#124423 = FACE_OUTER_BOUND ( 'NONE', #140565, .T. ) ;
#124424 = EDGE_LOOP ( 'NONE', ( #49947, #12066, #40375, #22299 ) ) ;
#124425 = CARTESIAN_POINT ( 'NONE',  ( 20.97873647476855652, -5.808823158059033709, 5.808823158059035485 ) ) ;
#124426 = DIRECTION ( 'NONE',  ( 0.6830127018922180770, -0.6830127018922204085, -0.2588190451025213501 ) ) ;
#124427 = CARTESIAN_POINT ( 'NONE',  ( -78.18398860626899705, 28.73617430169841924, 5.000000000000000000 ) ) ;
#124428 = CIRCLE ( 'NONE', #122035, 2.500000000000000888 ) ;
#124429 = CARTESIAN_POINT ( 'NONE',  ( 2.384059369432880882, 22.22500000000000142, -9.137797280955542334 ) ) ;
#124430 = VERTEX_POINT ( 'NONE', #2956 ) ;
#124431 = EDGE_LOOP ( 'NONE', ( #135051, #92603, #57289, #31677 ) ) ;
#124432 = ORIENTED_EDGE ( 'NONE', *, *, #120353, .F. ) ;
#124433 = DIRECTION ( 'NONE',  ( 0.000000000000000000, -1.000000000000000000, 0.000000000000000000 ) ) ;
#124434 = DIRECTION ( 'NONE',  ( 0.000000000000000000, -1.000000000000000000, 0.000000000000000000 ) ) ;
#124435 = UNCERTAINTY_MEASURE_WITH_UNIT (LENGTH_MEASURE( 1.000000000000000082E-05 ), #114529, 'distance_accuracy_value', 'NONE');
#124436 = DIRECTION ( 'NONE',  ( -1.000000000000000000, 0.000000000000000000, 0.000000000000000000 ) ) ;
#124438 = EDGE_CURVE ( 'NONE', #68957, #115494, #135637, .T. ) ;
#124437 = DIRECTION ( 'NONE',  ( 0.7071067811865487940, -0.7071067811865463515, 0.000000000000000000 ) ) ;
#124439 = CARTESIAN_POINT ( 'NONE',  ( 33.32816939922330590, 14.25929247661557397, 4.000000000000000000 ) ) ;
#124440 = ADVANCED_FACE ( 'NONE', ( #94953 ), #94252, .F. ) ;
#124442 = VECTOR ( 'NONE', #41558, 1000.000000000000000 ) ;
#124441 = LINE ( 'NONE', #44795, #15886 ) ;
#124443 = EDGE_CURVE ( 'NONE', #128263, #3015, #20766, .T. ) ;
#124444 = CARTESIAN_POINT ( 'NONE',  ( 21.16809626817622103, 8.755558144015518351, 4.000000000000000000 ) ) ;
#124445 = DIRECTION ( 'NONE',  ( -0.6830127018922180770, -0.6830127018922204085, -0.2588190451025213501 ) ) ;
#124446 = LINE ( 'NONE', #40157, #134561 ) ;
#124447 = CARTESIAN_POINT ( 'NONE',  ( 1.499999999999990896, -14.56887692260766443, 4.000000000000000000 ) ) ;
#124448 = ORIENTED_EDGE ( 'NONE', *, *, #18437, .F. ) ;
#124449 = CARTESIAN_POINT ( 'NONE',  ( 19.82791644288525390, -2.376042199413920475, -33.22268429432537573 ) ) ;
#124450 = ORIENTED_EDGE ( 'NONE', *, *, #83488, .F. ) ;
#124451 = AXIS2_PLACEMENT_3D ( 'NONE', #38296, #29529, #73772 ) ;
#124452 = CARTESIAN_POINT ( 'NONE',  ( -34.49999999999975842, 5.696342897626469615, -7.587980461218476691 ) ) ;
#124454 = EDGE_LOOP ( 'NONE', ( #52533, #132719, #31881, #86061 ) ) ;
#124453 = DIRECTION ( 'NONE',  ( -0.000000000000000000, -0.3543493200069152693, 0.9351131265310292928 ) ) ;
#124455 =( GEOMETRIC_REPRESENTATION_CONTEXT ( 3 ) GLOBAL_UNCERTAINTY_ASSIGNED_CONTEXT ( ( #83678 ) ) GLOBAL_UNIT_ASSIGNED_CONTEXT ( ( #33804, #97597, #109912 ) ) REPRESENTATION_CONTEXT ( 'NONE', 'WORKASPACE' ) );
#124456 = ADVANCED_FACE ( 'NONE', ( #39174 ), #127615, .F. ) ;
#124457 =( NAMED_UNIT ( * ) PLANE_ANGLE_UNIT ( ) SI_UNIT ( $, .RADIAN. ) );
#124458 = CARTESIAN_POINT ( 'NONE',  ( 20.99999999999985434, 10.55218569542906160, 5.000000000000000000 ) ) ;
#124459 =( REPRESENTATION_RELATIONSHIP ('NONE','NONE', #69070, #64389 ) REPRESENTATION_RELATIONSHIP_WITH_TRANSFORMATION ( #130817 )SHAPE_REPRESENTATION_RELATIONSHIP( ) );
#124460 = ORIENTED_EDGE ( 'NONE', *, *, #117277, .F. ) ;
#124461 = CARTESIAN_POINT ( 'NONE',  ( -15.29974487139158867, -27.71228299555216879, 4.000000000000000000 ) ) ;
#124462 = ORIENTED_EDGE ( 'NONE', *, *, #61428, .T. ) ;
#124463 = LINE ( 'NONE', #67993, #35165 ) ;
#124464 = ORIENTED_EDGE ( 'NONE', *, *, #89231, .F. ) ;
#124465 = CIRCLE ( 'NONE', #52730, 2.500000000000000888 ) ;
#124466 = PRESENTATION_LAYER_ASSIGNMENT (  '', '', ( #131410 ) ) ;
#124467 = LINE ( 'NONE', #71531, #7900 ) ;
#124469 = CARTESIAN_POINT ( 'NONE',  ( 99.97502705046289861, -5.819803920172572198, 5.819803920172572198 ) ) ;
#124468 = VECTOR ( 'NONE', #47189, 1000.000000000000227 ) ;
#124470 = CARTESIAN_POINT ( 'NONE',  ( 26.99999999999981881, 13.55218569542903317, 5.000000000000000000 ) ) ;
#124471 = ORIENTED_EDGE ( 'NONE', *, *, #54560, .T. ) ;
#124472 = CARTESIAN_POINT ( 'NONE',  ( -41.99451991528749062, 28.92564299267967343, 4.000000000000000000 ) ) ;
#124473 = DIRECTION ( 'NONE',  ( -0.3543493200069162685, -0.000000000000000000, -0.9351131265310288487 ) ) ;
#124474 = LINE ( 'NONE', #12834, #18280 ) ;
#124475 = CARTESIAN_POINT ( 'NONE',  ( 21.43750000000000000, -4.461849672132299105, 4.461849672132299993 ) ) ;
#124476 = CARTESIAN_POINT ( 'NONE',  ( 23.31206980810188512, 7.934999999999992504, 2.126176841940951689 ) ) ;
#124477 = AXIS2_PLACEMENT_3D ( 'NONE', #52651, #67866, #111307 ) ;
#124478 = DIRECTION ( 'NONE',  ( 0.000000000000000000, -1.000000000000000000, 5.075120898959323014E-15 ) ) ;
#124479 = CARTESIAN_POINT ( 'NONE',  ( 18.63425672184678916, 4.584330080086930965E-16, 0.000000000000000000 ) ) ;
#124480 = EDGE_LOOP ( 'NONE', ( #107960, #99277, #55451, #27959 ) ) ;
#124481 = CARTESIAN_POINT ( 'NONE',  ( -19.95484226663321436, -21.74070752338405299, 21.72585301388579992 ) ) ;
#124482 = ORIENTED_EDGE ( 'NONE', *, *, #62977, .T. ) ;
#124483 = CARTESIAN_POINT ( 'NONE',  ( 97.27126352523143282, 4.472830434245839371, 4.472830434245842035 ) ) ;
#124484 = CARTESIAN_POINT ( 'NONE',  ( 23.78840764549667597, 2.499999999999998224, 3.061616997868380183E-16 ) ) ;
#124485 = LINE ( 'NONE', #14293, #55564 ) ;
#124486 = EDGE_CURVE ( 'NONE', #141655, #100403, #118119, .T. ) ;
#124487 = DIRECTION ( 'NONE',  ( -0.7071067811865486830, 0.7071067811865464625, 0.000000000000000000 ) ) ;
#124488 = CARTESIAN_POINT ( 'NONE',  ( 123.7287633666124265, -43.84677628532222116, -34.92499999999998295 ) ) ;
#124489 = VERTEX_POINT ( 'NONE', #18827 ) ;
#124490 = CARTESIAN_POINT ( 'NONE',  ( -34.82816939922328459, -14.24070752338413826, 4.000000000000000000 ) ) ;
#124491 = LINE ( 'NONE', #111469, #76670 ) ;
#124492 = ORIENTED_EDGE ( 'NONE', *, *, #109132, .F. ) ;
#124493 = CARTESIAN_POINT ( 'NONE',  ( -30.18398860626900060, 28.73617430169808173, 5.000000000000000000 ) ) ;
#124494 = CARTESIAN_POINT ( 'NONE',  ( -17.51078643762690845, -27.52281430457043143, 5.000000000000000000 ) ) ;
#124496 = ORIENTED_EDGE ( 'NONE', *, *, #137597, .F. ) ;
#124495 = PLANE ( 'NONE',  #121529 ) ;
#124498 = VECTOR ( 'NONE', #77351, 1000.000000000000000 ) ;
#124497 = FACE_OUTER_BOUND ( 'NONE', #105702, .T. ) ;
#124499 = CARTESIAN_POINT ( 'NONE',  ( 103.0375270504628986, -9.735942053221456900E-16, 7.949999999999998401 ) ) ;
#124500 = CARTESIAN_POINT ( 'NONE',  ( 0.2416945842518697374, 0.7592924766157104211, 14.37146558664982621 ) ) ;
#124501 = LINE ( 'NONE', #12161, #121974 ) ;
#124502 = DIRECTION ( 'NONE',  ( -0.6830127018922180770, -0.6830127018922204085, -0.2588190451025213501 ) ) ;
#124503 = ORIENTED_EDGE ( 'NONE', *, *, #35943, .T. ) ;
#124504 = ORIENTED_EDGE ( 'NONE', *, *, #100842, .F. ) ;
#124505 = ORIENTED_EDGE ( 'NONE', *, *, #92507, .T. ) ;
#124506 = EDGE_CURVE ( 'NONE', #127352, #17335, #7214, .T. ) ;
#124507 = CARTESIAN_POINT ( 'NONE',  ( 82.68793019189809002, 6.110000000000002984, -1.637169565754156730 ) ) ;
#124508 = PRESENTATION_LAYER_ASSIGNMENT (  '', '', ( #36542 ) ) ;
#124509 = VERTEX_POINT ( 'NONE', #63096 ) ;
#124510 = ADVANCED_FACE ( 'NONE', ( #7943 ), #107266, .F. ) ;
#124511 = EDGE_CURVE ( 'NONE', #54378, #33777, #39917, .T. ) ;
#124512 = CARTESIAN_POINT ( 'NONE',  ( -11.99999999999991651, 8.966399257802171618, 5.000000000000000000 ) ) ;
#124513 = CARTESIAN_POINT ( 'NONE',  ( -11.39513766812472184, 21.75929247661549937, 21.32995629748188904 ) ) ;
#124514 = EDGE_CURVE ( 'NONE', #3029, #53162, #61661, .T. ) ;
#124515 = CARTESIAN_POINT ( 'NONE',  ( 20.99999999999985789, -12.03360074219761344, 5.000000000000000000 ) ) ;
#124516 = DIRECTION ( 'NONE',  ( -0.7071067811865487940, 0.7071067811865463515, 0.000000000000000000 ) ) ;
#124517 = EDGE_LOOP ( 'NONE', ( #22096, #90264, #125109, #92113 ) ) ;
#124518 = EDGE_CURVE ( 'NONE', #12215, #68587, #26857, .T. ) ;
#124519 = CARTESIAN_POINT ( 'NONE',  ( 14.24715658456393541, 6.719242673238161601, 5.000000000000000000 ) ) ;
#124521 =( BOUNDED_CURVE ( )  B_SPLINE_CURVE ( 2, ( #64165, #97477, #143139, #19221, #8997, #118524, #8304, #31532, #63480, #130866, #75063, #86642, #9761 ),
 .UNSPECIFIED., .F., .F. ) 
 B_SPLINE_CURVE_WITH_KNOTS ( ( 3, 2, 2, 2, 2, 2, 3 ),
 ( 0.1833333333333333204, 0.1861111111111111160, 0.1888888888888888840, 0.1916666666666666796, 0.1944444444444444475, 0.1972222222222222154, 0.2000000000000000111 ),
 .UNSPECIFIED. ) 
 CURVE ( )  GEOMETRIC_REPRESENTATION_ITEM ( )  RATIONAL_B_SPLINE_CURVE ( ( 1.000000000000000000, 0.9659258262890683122, 1.000000000000000000, 0.9659258262890683122, 1.000000000000000000, 0.9659258262890683122, 1.000000000000000000, 0.9659258262890683122, 1.000000000000000000, 0.9659258262890683122, 1.000000000000000000, 0.9659258262890683122, 1.000000000000000000 ) ) 
 REPRESENTATION_ITEM ( '' )  );
#124520 = DIRECTION ( 'NONE',  ( -0.000000000000000000, 0.3543493200069153248, 0.9351131265310292928 ) ) ;
#124522 = CARTESIAN_POINT ( 'NONE',  ( 27.98911971346032246, -22.02621442084248216, 4.990779571109221990 ) ) ;
#124523 = CARTESIAN_POINT ( 'NONE',  ( 79.82876352523145158, 0.000000000000000000, -6.109999999999998543 ) ) ;
#124524 = VERTEX_POINT ( 'NONE', #95679 ) ;
#124525 = EDGE_CURVE ( 'NONE', #16309, #99319, #60232, .T. ) ;
#124526 = FACE_OUTER_BOUND ( 'NONE', #50198, .T. ) ;
#124527 = CARTESIAN_POINT ( 'NONE',  ( -10.73248902172657360, 22.22500000000000142, -4.167446773218399514 ) ) ;
#124528 = LINE ( 'NONE', #46290, #53962 ) ;
#124529 = EDGE_LOOP ( 'NONE', ( #61024, #100462, #62903, #34506 ) ) ;
#124530 = VERTEX_POINT ( 'NONE', #84136 ) ;
#124531 = EDGE_CURVE ( 'NONE', #70558, #129671, #138492, .T. ) ;
#124532 = DIRECTION ( 'NONE',  ( 0.7071067811865486830, -0.7071067811865464625, -0.000000000000000000 ) ) ;
#124533 = EDGE_CURVE ( 'NONE', #18734, #7814, #16696, .T. ) ;
#124534 = DIRECTION ( 'NONE',  ( 0.7071067811865487940, 0.7071067811865463515, -0.000000000000000000 ) ) ;
#124535 = CARTESIAN_POINT ( 'NONE',  ( 23.25456980810188767, -6.871911579029512218, 3.967499999999996252 ) ) ;
#124536 = CARTESIAN_POINT ( 'NONE',  ( 56.99451991528749062, 28.92564299267978001, 4.000000000000000000 ) ) ;
#124537 = DIRECTION ( 'NONE',  ( 0.000000000000000000, -1.000000000000000000, 0.000000000000000000 ) ) ;
#124538 = ADVANCED_FACE ( 'NONE', ( #60975 ), #38460, .F. ) ;
#124539 = CARTESIAN_POINT ( 'NONE',  ( 1.500000000000000000, 0.000000000000000000, -8.000000000000001776 ) ) ;
#124540 = CARTESIAN_POINT ( 'NONE',  ( -3.299744871391591339, -27.71228299555208352, 4.000000000000000000 ) ) ;
#124541 = ORIENTED_EDGE ( 'NONE', *, *, #129548, .F. ) ;
#124542 = AXIS2_PLACEMENT_3D ( 'NONE', #89605, #133145, #34518 ) ;
#124543 = EDGE_LOOP ( 'NONE', ( #20703, #3508, #63500, #19083 ) ) ;
#124544 = CARTESIAN_POINT ( 'NONE',  ( 9.770833333333333925, 6.094999999999991758, 1.633150327867686880 ) ) ;
#124545 = ORIENTED_EDGE ( 'NONE', *, *, #127048, .F. ) ;
#124546 = ORIENTED_EDGE ( 'NONE', *, *, #106448, .F. ) ;
#124547 = AXIS2_PLACEMENT_3D ( 'NONE', #26255, #70518, #15331 ) ;
#124548 = DIRECTION ( 'NONE',  ( 1.000000000000000000, 0.000000000000000000, 0.000000000000000000 ) ) ;
#124549 = ORIENTED_EDGE ( 'NONE', *, *, #133702, .F. ) ;
#124550 = DIRECTION ( 'NONE',  ( -7.447409204830965619E-33, 6.123233995736750012E-17, -1.000000000000000000 ) ) ;
#124551 = CARTESIAN_POINT ( 'NONE',  ( -4.001930566820951718, -22.22500000000000142, 4.500000000000000888 ) ) ;
#124552 = EDGE_CURVE ( 'NONE', #136197, #88472, #50060, .T. ) ;
#124553 = CARTESIAN_POINT ( 'NONE',  ( 7.499999999999951150, 7.466399257802184053, 5.000000000000000000 ) ) ;
#124554 = AXIS2_PLACEMENT_3D ( 'NONE', #64885, #109066, #98219 ) ;
#124555 = DIRECTION ( 'NONE',  ( 0.7071067811865486830, -0.7071067811865464625, -0.000000000000000000 ) ) ;
#124556 = ORIENTED_EDGE ( 'NONE', *, *, #135676, .T. ) ;
#124557 = CARTESIAN_POINT ( 'NONE',  ( -34.92500000000001137, 15.66246187583883831, 4.000000000000000000 ) ) ;
#124558 = VECTOR ( 'NONE', #48786, 1000.000000000000000 ) ;
#124559 = VERTEX_POINT ( 'NONE', #73243 ) ;
#124560 = CARTESIAN_POINT ( 'NONE',  ( -5.207106781186503497, 12.75929247661559351, 5.000000000000000000 ) ) ;
#124561 = ORIENTED_EDGE ( 'NONE', *, *, #63935, .F. ) ;
#124562 = ORIENTED_EDGE ( 'NONE', *, *, #62969, .T. ) ;
#124563 = DIRECTION ( 'NONE',  ( -0.000000000000000000, 0.3543493200069153248, 0.9351131265310292928 ) ) ;
#124564 = ORIENTED_EDGE ( 'NONE', *, *, #67762, .F. ) ;
#124565 = ORIENTED_EDGE ( 'NONE', *, *, #90436, .T. ) ;
#124566 = FACE_OUTER_BOUND ( 'NONE', #19497, .T. ) ;
#124567 = VECTOR ( 'NONE', #129186, 999.9999999999998863 ) ;
#124568 = VERTEX_POINT ( 'NONE', #116727 ) ;
#124569 = VECTOR ( 'NONE', #62176, 1000.000000000000000 ) ;
#124570 = EDGE_CURVE ( 'NONE', #120201, #110351, #105821, .T. ) ;
#124571 = LINE ( 'NONE', #114400, #25746 ) ;
#124572 = PLANE ( 'NONE',  #40277 ) ;
#124573 = CARTESIAN_POINT ( 'NONE',  ( 121.7712635252314328, 4.472830434245838482, 4.472830434245842035 ) ) ;
#124574 = DIRECTION ( 'NONE',  ( 1.000000000000000000, 0.000000000000000000, 0.000000000000000000 ) ) ;
#124575 = EDGE_CURVE ( 'NONE', #44742, #81070, #106531, .T. ) ;
#124576 = DIRECTION ( 'NONE',  ( -0.000000000000000000, -1.000000000000000000, -0.000000000000000000 ) ) ;
#124577 = LINE ( 'NONE', #57931, #21224 ) ;
#124578 = DIRECTION ( 'NONE',  ( -0.000000000000000000, 0.000000000000000000, 1.000000000000000000 ) ) ;
#124579 = LINE ( 'NONE', #4151, #42430 ) ;
#124580 = PRESENTATION_STYLE_ASSIGNMENT (( #48446 ) ) ;
#124581 = ORIENTED_EDGE ( 'NONE', *, *, #10478, .F. ) ;
#124582 = CARTESIAN_POINT ( 'NONE',  ( 0.000000000000000000, 0.000000000000000000, 5.000000000000000000 ) ) ;
#124583 = CARTESIAN_POINT ( 'NONE',  ( -39.48921356237310221, -27.52281430457082934, 5.000000000000000000 ) ) ;
#124584 = ADVANCED_FACE ( 'NONE', ( #66643 ), #97064, .F. ) ;
#124585 = ORIENTED_EDGE ( 'NONE', *, *, #82055, .F. ) ;
#124586 = ORIENTED_EDGE ( 'NONE', *, *, #31781, .F. ) ;
#124587 = CARTESIAN_POINT ( 'NONE',  ( -26.29289321881326913, -12.74070752338415602, 5.000000000000000000 ) ) ;
#124588 = ORIENTED_EDGE ( 'NONE', *, *, #43739, .F. ) ;
#124589 = VECTOR ( 'NONE', #82223, 1000.000000000000227 ) ;
#124590 = DIRECTION ( 'NONE',  ( -0.000000000000000000, 0.000000000000000000, 1.000000000000000000 ) ) ;
#124591 = CARTESIAN_POINT ( 'NONE',  ( 1.179999999999999272, 10.00000000000000178, 10.00000000000000000 ) ) ;
#124592 = EDGE_CURVE ( 'NONE', #105871, #92747, #9349, .T. ) ;
#124593 = LINE ( 'NONE', #81110, #54187 ) ;
#124594 = CARTESIAN_POINT ( 'NONE',  ( -22.55363393633058067, -22.22500000000000142, 0.3120269325270338401 ) ) ;
#124595 = EDGE_LOOP ( 'NONE', ( #17971, #107862, #18188, #137570 ) ) ;
#124596 = AXIS2_PLACEMENT_3D ( 'NONE', #75544, #94588, #20413 ) ;
#124597 = LINE ( 'NONE', #134793, #74340 ) ;
#124598 = EDGE_LOOP ( 'NONE', ( #5063, #2572, #15726, #45949 ) ) ;
#124599 = LINE ( 'NONE', #2061, #2818 ) ;
#124600 = CARTESIAN_POINT ( 'NONE',  ( 25.87956980810188767, 3.967499999999998916, 6.871911579029510442 ) ) ;
#124601 = VERTEX_POINT ( 'NONE', #99226 ) ;
#124602 = CARTESIAN_POINT ( 'NONE',  ( -2.000000000000000000, 2.375000000000000000, 0.000000000000000000 ) ) ;
#124603 = DIRECTION ( 'NONE',  ( -0.7071067811865486830, 0.7071067811865464625, 0.000000000000000000 ) ) ;
#124604 = EDGE_LOOP ( 'NONE', ( #107730, #124391, #82586, #11495 ) ) ;
#124605 = VERTEX_POINT ( 'NONE', #141329 ) ;
#124606 = ORIENTED_EDGE ( 'NONE', *, *, #95271, .F. ) ;
#124607 = PLANE ( 'NONE',  #31075 ) ;
#124608 = DIRECTION ( 'NONE',  ( 0.6830127018922180770, -0.6830127018922204085, -0.2588190451025213501 ) ) ;
#124610 = VECTOR ( 'NONE', #47083, 1000.000000000000000 ) ;
#124609 = CARTESIAN_POINT ( 'NONE',  ( -2.207106781186527922, 15.75929247661555443, 5.000000000000000000 ) ) ;
#124611 = PLANE ( 'NONE',  #26467 ) ;
#124612 = ORIENTED_EDGE ( 'NONE', *, *, #101761, .F. ) ;
#124613 = CARTESIAN_POINT ( 'NONE',  ( 8.999999999999925393, -10.77435723561694836, -9.972017380717252522 ) ) ;
#124614 = AXIS2_PLACEMENT_3D ( 'NONE', #114111, #135869, #36549 ) ;
#124615 = EDGE_CURVE ( 'NONE', #39763, #135646, #31166, .T. ) ;
#124617 = EDGE_CURVE ( 'NONE', #77841, #29516, #54365, .T. ) ;
#124616 = DIRECTION ( 'NONE',  ( 0.7071067811865487940, 0.7071067811865463515, -0.000000000000000000 ) ) ;
#124618 = LINE ( 'NONE', #5666, #139449 ) ;
#124619 = ORIENTED_EDGE ( 'NONE', *, *, #88689, .F. ) ;
#124620 = CARTESIAN_POINT ( 'NONE',  ( 1.180000000000001270, -9.043340090917736163, 10.00000000000000000 ) ) ;
#124621 = VERTEX_POINT ( 'NONE', #43454 ) ;
#124622 = EDGE_CURVE ( 'NONE', #10035, #7970, #20437, .T. ) ;
#124624 = ORIENTED_EDGE ( 'NONE', *, *, #38903, .T. ) ;
#124623 = CARTESIAN_POINT ( 'NONE',  ( 57.88343899890125499, -48.52444309369082731, -36.09967824800666136 ) ) ;
#124625 = ORIENTED_EDGE ( 'NONE', *, *, #68172, .F. ) ;
#124626 = EDGE_CURVE ( 'NONE', #78422, #98176, #53628, .T. ) ;
#124627 = CARTESIAN_POINT ( 'NONE',  ( -4.499999999999968914, -10.04351517176479014, -1.623559851933833453 ) ) ;
#124628 = DIRECTION ( 'NONE',  ( -0.000000000000000000, 0.3543493200069153248, 0.9351131265310292928 ) ) ;
#124629 = VERTEX_POINT ( 'NONE', #32593 ) ;
#124630 = DIRECTION ( 'NONE',  ( -0.7071067811865487940, 0.7071067811865463515, 0.000000000000000000 ) ) ;
#124631 = UNCERTAINTY_MEASURE_WITH_UNIT (LENGTH_MEASURE( 1.000000000000000082E-05 ), #79181, 'distance_accuracy_value', 'NONE');
#124632 = VERTEX_POINT ( 'NONE', #120249 ) ;
#124633 = CARTESIAN_POINT ( 'NONE',  ( -20.29289321881331531, 11.25929247661560062, 5.000000000000000000 ) ) ;
#124634 = CARTESIAN_POINT ( 'NONE',  ( 1.499999999999989120, 21.43112307739196964, 4.000000000000000000 ) ) ;
#124635 = CARTESIAN_POINT ( 'NONE',  ( 25.19018167574432709, -18.74070752338409562, 7.910009926591448526 ) ) ;
#124636 = VECTOR ( 'NONE', #125654, 1000.000000000000000 ) ;
#124637 = CARTESIAN_POINT ( 'NONE',  ( -28.17183060077627843, -5.240707523384232402, 4.000000000000000000 ) ) ;
#124638 = CARTESIAN_POINT ( 'NONE',  ( -16.17183060077634948, -17.24070752338410273, 4.000000000000000000 ) ) ;
#124639 = CARTESIAN_POINT ( 'NONE',  ( 20.20519093902540320, 4.584330080086930965E-16, 0.000000000000000000 ) ) ;
#124640 = LINE ( 'NONE', #102193, #44923 ) ;
#124641 = DIRECTION ( 'NONE',  ( -1.000000000000000000, -1.224606353822377258E-16, -0.000000000000000000 ) ) ;
#124642 = CARTESIAN_POINT ( 'NONE',  ( 25.49956980810189222, -3.967499999999998028, -6.871911579029511330 ) ) ;
#124643 = LINE ( 'NONE', #113768, #132527 ) ;
#124644 = DIRECTION ( 'NONE',  ( -0.7071067811865487940, 0.7071067811865463515, -0.000000000000000000 ) ) ;
#124645 = DIRECTION ( 'NONE',  ( 0.3543493200069164351, -0.000000000000000000, -0.9351131265310288487 ) ) ;
#124646 = LINE ( 'NONE', #70322, #59428 ) ;
#124647 = ORIENTED_EDGE ( 'NONE', *, *, #3341, .F. ) ;
#124648 = ADVANCED_FACE ( 'NONE', ( #75376 ), #142076, .F. ) ;
#124649 = VERTEX_POINT ( 'NONE', #129736 ) ;
#124650 = CARTESIAN_POINT ( 'NONE',  ( 95.06250000000000000, -5.819803920172572198, -5.819803920172573086 ) ) ;
#124651 = ORIENTED_EDGE ( 'NONE', *, *, #9452, .F. ) ;
#124652 = ORIENTED_EDGE ( 'NONE', *, *, #142496, .T. ) ;
#124653 = VECTOR ( 'NONE', #139261, 1000.000000000000000 ) ;
#124654 = ORIENTED_EDGE ( 'NONE', *, *, #37954, .F. ) ;
#124655 = DIRECTION ( 'NONE',  ( -0.7071067811865487940, 0.7071067811865463515, 0.000000000000000000 ) ) ;
#124656 = DIRECTION ( 'NONE',  ( -0.000000000000000000, 0.000000000000000000, 1.000000000000000000 ) ) ;
#124657 = CARTESIAN_POINT ( 'NONE',  ( 12.52989244501176813, 8.713222490859248381, -3.789296364347416901 ) ) ;
#124658 = ORIENTED_EDGE ( 'NONE', *, *, #10873, .T. ) ;
#124659 =( GEOMETRIC_REPRESENTATION_CONTEXT ( 3 ) GLOBAL_UNCERTAINTY_ASSIGNED_CONTEXT ( ( #85229 ) ) GLOBAL_UNIT_ASSIGNED_CONTEXT ( ( #73057, #49864, #82481 ) ) REPRESENTATION_CONTEXT ( 'NONE', 'WORKASPACE' ) );
#124660 = VECTOR ( 'NONE', #91618, 1000.000000000000114 ) ;
#124661 = PLANE ( 'NONE',  #118022 ) ;
#124662 = PLANE ( 'NONE',  #46527 ) ;
#124663 = AXIS2_PLACEMENT_3D ( 'NONE', #140748, #137390, #118279 ) ;
#124664 = DIRECTION ( 'NONE',  ( 1.000000000000000000, 0.000000000000000000, 0.000000000000000000 ) ) ;
#124665 = CARTESIAN_POINT ( 'NONE',  ( 126.1498859171888114, 5.910167777758539742, -4.315024036782260985 ) ) ;
#124666 = VECTOR ( 'NONE', #31724, 1000.000000000000000 ) ;
#124667 = CARTESIAN_POINT ( 'NONE',  ( 126.7870968585647944, 3.054999999999997495, 5.291415217122919401 ) ) ;
#124668 = LINE ( 'NONE', #64766, #114143 ) ;
#124669 = LINE ( 'NONE', #113065, #98280 ) ;
#124671 = DIRECTION ( 'NONE',  ( -1.000000000000000000, -0.000000000000000000, -0.000000000000000000 ) ) ;
#124670 = VECTOR ( 'NONE', #72566, 1000.000000000000227 ) ;
#124672 = CARTESIAN_POINT ( 'NONE',  ( 24.98358986394466186, 3.827854121229848694, 4.315828149752546139 ) ) ;
#124673 = LINE ( 'NONE', #123276, #87019 ) ;
#124674 = AXIS2_PLACEMENT_3D ( 'NONE', #31381, #110333, #65464 ) ;
#124675 = LINE ( 'NONE', #10879, #10521 ) ;
#124676 = VERTEX_POINT ( 'NONE', #109418 ) ;
#124677 = ORIENTED_EDGE ( 'NONE', *, *, #131863, .T. ) ;
#124678 = EDGE_CURVE ( 'NONE', #68424, #86982, #131171, .T. ) ;
#124679 = CARTESIAN_POINT ( 'NONE',  ( 106.8962635252314328, 4.472830434245840259, -4.472830434245839371 ) ) ;
#124680 =( BOUNDED_CURVE ( )  B_SPLINE_CURVE ( 2, ( #33139, #440, #120800, #65027, #30226, #130283, #96872, #88199, #41825, #141878, #118666, #86045, #109930 ),
 .UNSPECIFIED., .F., .T. ) 
 B_SPLINE_CURVE_WITH_KNOTS ( ( 3, 2, 2, 2, 2, 2, 3 ),
 ( 0.6666666666666666297, 0.6694444444444443976, 0.6722222222222222765, 0.6750000000000000444, 0.6777777777777778123, 0.6805555555555555802, 0.6833333333333333481 ),
 .UNSPECIFIED. ) 
 CURVE ( )  GEOMETRIC_REPRESENTATION_ITEM ( )  RATIONAL_B_SPLINE_CURVE ( ( 1.000000000000000000, 0.9659258262890683122, 1.000000000000000000, 0.9659258262890683122, 1.000000000000000000, 0.9659258262890683122, 1.000000000000000000, 0.9659258262890683122, 1.000000000000000000, 0.9659258262890683122, 1.000000000000000000, 0.9659258262890683122, 1.000000000000000000 ) ) 
 REPRESENTATION_ITEM ( '' )  );
#124681 = ORIENTED_EDGE ( 'NONE', *, *, #89484, .F. ) ;
#124682 = ADVANCED_FACE ( 'NONE', ( #42765 ), #76085, .F. ) ;
#124683 = DIRECTION ( 'NONE',  ( -1.000000000000000000, -0.000000000000000000, -0.000000000000000000 ) ) ;
#124684 = VECTOR ( 'NONE', #62588, 1000.000000000000000 ) ;
#124685 = CARTESIAN_POINT ( 'NONE',  ( 29.99451991528749417, 28.92564299267958816, 4.000000000000000000 ) ) ;
#124686 = EDGE_CURVE ( 'NONE', #71456, #68931, #65957, .T. ) ;
#124687 = EDGE_CURVE ( 'NONE', #117948, #40407, #121703, .T. ) ;
#124688 = DIRECTION ( 'NONE',  ( 0.000000000000000000, -1.000000000000000000, 0.000000000000000000 ) ) ;
#124689 = CARTESIAN_POINT ( 'NONE',  ( -19.82816939922339117, 15.75929247661555799, 4.000000000000000000 ) ) ;
#124690 = AXIS2_PLACEMENT_3D ( 'NONE', #47670, #113578, #67242 ) ;
#124691 = CARTESIAN_POINT ( 'NONE',  ( 103.0162635252314374, -4.472830434245839371, 4.472830434245839371 ) ) ;
#124692 = EDGE_LOOP ( 'NONE', ( #78403, #77579, #41367, #120576 ) ) ;
#124693 = ORIENTED_EDGE ( 'NONE', *, *, #107591, .T. ) ;
#124694 = DIRECTION ( 'NONE',  ( 0.7071067811865486830, -0.7071067811865464625, -0.000000000000000000 ) ) ;
#124695 = CARTESIAN_POINT ( 'NONE',  ( -34.11017322888186953, -22.22500000000000497, 4.785647885939355639 ) ) ;
#124696 = CONICAL_SURFACE ( 'NONE', #13521, 2.500000000000000444, 0.9599310885968830309 ) ;
#124697 = ORIENTED_EDGE ( 'NONE', *, *, #101078, .T. ) ;
#124698 = ORIENTED_EDGE ( 'NONE', *, *, #1564, .F. ) ;
#124699 = ADVANCED_FACE ( 'NONE', ( #130480 ), #55058, .F. ) ;
#124700 = VERTEX_POINT ( 'NONE', #52869 ) ;
#124701 = PLANE ( 'NONE',  #120895 ) ;
#124702 = EDGE_CURVE ( 'NONE', #71690, #114228, #132643, .T. ) ;
#124703 = CARTESIAN_POINT ( 'NONE',  ( 2.108736474768552860, -5.808823158059033709, 5.808823158059035485 ) ) ;
#124704 = VECTOR ( 'NONE', #49257, 999.9999999999998863 ) ;
#124705 = EDGE_CURVE ( 'NONE', #139177, #67571, #32052, .T. ) ;
#124706 = EDGE_LOOP ( 'NONE', ( #28146, #114542, #63069, #94470 ) ) ;
#124707 = ORIENTED_EDGE ( 'NONE', *, *, #95185, .F. ) ;
#124708 = DIRECTION ( 'NONE',  ( -0.6830127018922180770, -0.6830127018922204085, -0.2588190451025213501 ) ) ;
#124709 = EDGE_LOOP ( 'NONE', ( #621, #96009, #73385, #4305 ) ) ;
#124710 = EDGE_LOOP ( 'NONE', ( #39349, #43067, #65414, #94342 ) ) ;
#124711 = EDGE_CURVE ( 'NONE', #29397, #113191, #19550, .T. ) ;
#124712 = CIRCLE ( 'NONE', #94580, 3.999999999999989786 ) ;
#124713 = VECTOR ( 'NONE', #95921, 999.9999999999998863 ) ;
#124714 = CARTESIAN_POINT ( 'NONE',  ( -59.99451991528749772, 28.92564299267980132, 4.000000000000000000 ) ) ;
#124715 = FACE_OUTER_BOUND ( 'NONE', #21849, .T. ) ;
#124716 = LINE ( 'NONE', #90685, #37552 ) ;
#124717 = EDGE_LOOP ( 'NONE', ( #46922, #25587, #24198, #8839 ) ) ;
#124718 = LINE ( 'NONE', #23237, #32146 ) ;
#124719 = CARTESIAN_POINT ( 'NONE',  ( -20.20710678118640402, -8.240707523384189770, 5.000000000000000000 ) ) ;
#124720 = ADVANCED_FACE ( 'NONE', ( #20247 ), #78968, .F. ) ;
#124721 = DIRECTION ( 'NONE',  ( -0.000000000000000000, 0.000000000000000000, 1.000000000000000000 ) ) ;
#124722 = DIRECTION ( 'NONE',  ( 0.000000000000000000, 0.000000000000000000, 1.000000000000000000 ) ) ;
#124723 = FACE_BOUND ( 'NONE', #119675, .T. ) ;
#124724 = VERTEX_POINT ( 'NONE', #68802 ) ;
#124725 = CARTESIAN_POINT ( 'NONE',  ( 62.93336038379622721, 2.130196079827431532, -7.949999999999996625 ) ) ;
#124726 = DIRECTION ( 'NONE',  ( -0.000000000000000000, 0.000000000000000000, 1.000000000000000000 ) ) ;
#124727 = CARTESIAN_POINT ( 'NONE',  ( -25.39999999999996305, 3.061616997868383141E-16, -2.500000000000000000 ) ) ;
#124728 = ORIENTED_EDGE ( 'NONE', *, *, #58641, .F. ) ;
#124729 = EDGE_CURVE ( 'NONE', #98397, #119455, #20540, .T. ) ;
#124730 = DIRECTION ( 'NONE',  ( 0.6830127018922180770, -0.6830127018922204085, -0.2588190451025213501 ) ) ;
#124731 = ORIENTED_EDGE ( 'NONE', *, *, #123371, .F. ) ;
#124732 = EDGE_CURVE ( 'NONE', #126893, #10073, #14394, .T. ) ;
#124733 = ORIENTED_EDGE ( 'NONE', *, *, #83908, .T. ) ;
#124734 = ORIENTED_EDGE ( 'NONE', *, *, #6001, .T. ) ;
#124735 = EDGE_CURVE ( 'NONE', #69740, #113816, #58675, .T. ) ;
#124736 = CARTESIAN_POINT ( 'NONE',  ( 41.32876352523144448, 0.000000000000000000, -6.109999999999998543 ) ) ;
#124737 = ORIENTED_EDGE ( 'NONE', *, *, #65546, .F. ) ;
#124738 = DIRECTION ( 'NONE',  ( 0.6830127018922180770, -0.6830127018922204085, -0.2588190451025213501 ) ) ;
#124739 = PLANE ( 'NONE',  #99269 ) ;
#124740 = FACE_OUTER_BOUND ( 'NONE', #108435, .T. ) ;
#124741 = VERTEX_POINT ( 'NONE', #25991 ) ;
#124742 = FACE_OUTER_BOUND ( 'NONE', #14966, .T. ) ;
#124743 = SURFACE_SIDE_STYLE ('',( #69686 ) ) ;
#124744 = CARTESIAN_POINT ( 'NONE',  ( 34.92499999999998295, -6.048682586364314773, 15.71395525773010604 ) ) ;
#124745 =( NAMED_UNIT ( * ) PLANE_ANGLE_UNIT ( ) SI_UNIT ( $, .RADIAN. ) );
#124746 = CARTESIAN_POINT ( 'NONE',  ( 45.48921356237309510, -27.52281430457087197, 5.000000000000000000 ) ) ;
#124747 = DIRECTION ( 'NONE',  ( -0.000000000000000000, 0.000000000000000000, 1.000000000000000000 ) ) ;
#124748 = CARTESIAN_POINT ( 'NONE',  ( -10.17183060077639389, 18.75929247661552424, 4.000000000000000000 ) ) ;
#124749 = EDGE_LOOP ( 'NONE', ( #11006, #67735, #5820, #101271, #27386, #129394 ) ) ;
#124750 = ORIENTED_EDGE ( 'NONE', *, *, #72823, .F. ) ;
#124751 = ORIENTED_EDGE ( 'NONE', *, *, #31045, .F. ) ;
#124752 = ORIENTED_EDGE ( 'NONE', *, *, #50119, .F. ) ;
#124753 = LINE ( 'NONE', #48631, #51851 ) ;
#124754 = VECTOR ( 'NONE', #56139, 1000.000000000000000 ) ;
#124755 = CIRCLE ( 'NONE', #29845, 2.500000000000000444 ) ;
#124756 = ORIENTED_EDGE ( 'NONE', *, *, #37600, .F. ) ;
#124757 = VECTOR ( 'NONE', #52839, 1000.000000000000000 ) ;
#124759 = ORIENTED_EDGE ( 'NONE', *, *, #38108, .F. ) ;
#124758 = AXIS2_PLACEMENT_3D ( 'NONE', #56494, #12915, #78934 ) ;
#124760 = DIRECTION ( 'NONE',  ( -1.000000000000000000, -0.000000000000000000, -0.000000000000000000 ) ) ;
#124761 = LINE ( 'NONE', #124055, #2293 ) ;
#124762 = ORIENTED_EDGE ( 'NONE', *, *, #63591, .F. ) ;
#124763 = CARTESIAN_POINT ( 'NONE',  ( 69.18398860626899705, 28.73617430169835529, 5.000000000000000000 ) ) ;
#124764 = VECTOR ( 'NONE', #43295, 1000.000000000000000 ) ;
#124766 = EDGE_LOOP ( 'NONE', ( #8401, #56534, #58242 ) ) ;
#124765 = VECTOR ( 'NONE', #77051, 1000.000000000000000 ) ;
#124767 = DIRECTION ( 'NONE',  ( 1.000000000000000000, 0.000000000000000000, 0.000000000000000000 ) ) ;
#124768 = DIRECTION ( 'NONE',  ( 0.6830127018922181881, 0.6830127018922202975, -0.2588190451025214056 ) ) ;
#124769 = CARTESIAN_POINT ( 'NONE',  ( -1.682930191898113881, -2.126176841940956130, 7.934999999999991616 ) ) ;
#124770 = ORIENTED_EDGE ( 'NONE', *, *, #8257, .F. ) ;
#124772 = CARTESIAN_POINT ( 'NONE',  ( 11.99451991528749417, 28.92564299267946382, 4.000000000000000000 ) ) ;
#124771 = CARTESIAN_POINT ( 'NONE',  ( 112.4954301918981230, 5.291415217122917625, 3.055000000000002380 ) ) ;
#124773 = FACE_OUTER_BOUND ( 'NONE', #113087, .T. ) ;
#124774 = LINE ( 'NONE', #47964, #83577 ) ;
#124775 = VERTEX_POINT ( 'NONE', #13651 ) ;
#124776 = LINE ( 'NONE', #15971, #47337 ) ;
#124777 = EDGE_LOOP ( 'NONE', ( #69049, #64228, #4432 ) ) ;
#124778 = DIRECTION ( 'NONE',  ( 1.000000000000000000, 0.000000000000000000, 0.000000000000000000 ) ) ;
#124779 = CARTESIAN_POINT ( 'NONE',  ( -78.18398860626899705, 28.73617430169841924, 5.000000000000000000 ) ) ;
#124780 =( NAMED_UNIT ( * ) PLANE_ANGLE_UNIT ( ) SI_UNIT ( $, .RADIAN. ) );
#124781 = DIRECTION ( 'NONE',  ( 1.000000000000000000, 0.000000000000000000, 0.000000000000000000 ) ) ;
#124782 = CARTESIAN_POINT ( 'NONE',  ( 48.18398860626899705, 28.73617430169820608, 5.000000000000000000 ) ) ;
#124783 = CARTESIAN_POINT ( 'NONE',  ( 180.9285571751891837, -48.88296141031964481, -39.14553452061820593 ) ) ;
#124784 = ORIENTED_EDGE ( 'NONE', *, *, #12360, .T. ) ;
#124785 = PLANE ( 'NONE',  #11190 ) ;
#124786 = VECTOR ( 'NONE', #69226, 1000.000000000000227 ) ;
#124787 = CYLINDRICAL_SURFACE ( 'NONE', #48917, 2.552699999999994418 ) ;
#124788 = LINE ( 'NONE', #69732, #120866 ) ;
#124789 = ORIENTED_EDGE ( 'NONE', *, *, #142510, .F. ) ;
#124790 = CARTESIAN_POINT ( 'NONE',  ( -4.499999999999968914, 7.087461875839175640, 4.000000000000000000 ) ) ;
#124791 = VECTOR ( 'NONE', #62114, 1000.000000000000000 ) ;
#124793 = AXIS2_PLACEMENT_3D ( 'NONE', #96605, #74195, #140169 ) ;
#124792 = CARTESIAN_POINT ( 'NONE',  ( -15.79333936457836707, 21.75929247661549937, 4.998822639870700080 ) ) ;
#124794 = ORIENTED_EDGE ( 'NONE', *, *, #132212, .T. ) ;
#124795 = VECTOR ( 'NONE', #14252, 999.9999999999998863 ) ;
#124796 = EDGE_CURVE ( 'NONE', #45028, #5277, #110559, .T. ) ;
#124798 = ORIENTED_EDGE ( 'NONE', *, *, #33220, .F. ) ;
#124797 = PLANE ( 'NONE',  #34736 ) ;
#124800 = ORIENTED_EDGE ( 'NONE', *, *, #83462, .F. ) ;
#124799 = EDGE_CURVE ( 'NONE', #27842, #17414, #87423, .T. ) ;
#124801 = CARTESIAN_POINT ( 'NONE',  ( -4.199658430161101741, 13.35074831326553024, -24.67186739689545050 ) ) ;
#124802 = AXIS2_PLACEMENT_3D ( 'NONE', #19980, #20700, #43907 ) ;
#124803 = CARTESIAN_POINT ( 'NONE',  ( 28.00000000000002487, -49.14999999999999147, 34.92500000000003268 ) ) ;
#124804 = ORIENTED_EDGE ( 'NONE', *, *, #39157, .T. ) ;
#124805 = VECTOR ( 'NONE', #130469, 1000.000000000000000 ) ;
#124806 = DIRECTION ( 'NONE',  ( 0.7071067811865487940, 0.7071067811865463515, 0.000000000000000000 ) ) ;
#124807 = ORIENTED_EDGE ( 'NONE', *, *, #22315, .T. ) ;
#124808 = EDGE_CURVE ( 'NONE', #119425, #136749, #24548, .T. ) ;
#124809 = CARTESIAN_POINT ( 'NONE',  ( 12.69999999999999574, -35.13237070076361590, 17.62370837922860645 ) ) ;
#124810 = DIRECTION ( 'NONE',  ( -0.000000000000000000, 0.3543493200069153248, 0.9351131265310292928 ) ) ;
#124811 = CARTESIAN_POINT ( 'NONE',  ( -34.92500000000001137, -0.1586646689214904482, -3.482007288379085796 ) ) ;
#124812 = CARTESIAN_POINT ( 'NONE',  ( 53.99451991528749062, 28.92564299267975869, 4.000000000000000000 ) ) ;
#124813 = AXIS2_PLACEMENT_3D ( 'NONE', #60461, #6707, #50990 ) ;
#124814 = CARTESIAN_POINT ( 'NONE',  ( 152.4000000000000057, 7.919999999999947526, -21.52769999999997808 ) ) ;
#124815 = DIRECTION ( 'NONE',  ( 0.7071067811865487940, 0.7071067811865463515, 0.000000000000000000 ) ) ;
#124816 = PLANE ( 'NONE',  #18688 ) ;
#124817 = CARTESIAN_POINT ( 'NONE',  ( 53.99451991528749062, 28.92564299267975869, 4.000000000000000000 ) ) ;
#124818 = ORIENTED_EDGE ( 'NONE', *, *, #79983, .F. ) ;
#124819 = EDGE_CURVE ( 'NONE', #25787, #37639, #44934, .T. ) ;
#124820 = VERTEX_POINT ( 'NONE', #56523 ) ;
#124821 = VERTEX_POINT ( 'NONE', #57938 ) ;
#124822 = CARTESIAN_POINT ( 'NONE',  ( 116.5000000000000000, 0.000000000000000000, -7.950000000000000178 ) ) ;
#124823 = ORIENTED_EDGE ( 'NONE', *, *, #139487, .F. ) ;
#124824 = VERTEX_POINT ( 'NONE', #70255 ) ;
#124825 = ORIENTED_EDGE ( 'NONE', *, *, #122230, .F. ) ;
#124826 = CYLINDRICAL_SURFACE ( 'NONE', #112724, 3.378199999999994319 ) ;
#124827 = CARTESIAN_POINT ( 'NONE',  ( 34.92499999999998295, 18.00612307739178064, 4.000000000000000000 ) ) ;
#124828 = EDGE_CURVE ( 'NONE', #135494, #87458, #113704, .T. ) ;
#124829 = ORIENTED_EDGE ( 'NONE', *, *, #132062, .T. ) ;
#124830 = LINE ( 'NONE', #136409, #25337 ) ;
#124831 = DIRECTION ( 'NONE',  ( -1.000000000000000000, -1.224606353822377258E-16, -0.000000000000000000 ) ) ;
#124832 = CARTESIAN_POINT ( 'NONE',  ( 7.408407645496676963, 3.061616997868381169E-16, -2.500000000000001332 ) ) ;
#124833 = CARTESIAN_POINT ( 'NONE',  ( 111.4170968585647614, 3.054999999999998828, 5.291415217122922066 ) ) ;
#124834 = ORIENTED_EDGE ( 'NONE', *, *, #106639, .F. ) ;
#124835 = FACE_OUTER_BOUND ( 'NONE', #97707, .T. ) ;
#124836 = FACE_OUTER_BOUND ( 'NONE', #73483, .T. ) ;
#124837 = DIRECTION ( 'NONE',  ( 0.7071067811865486830, -0.7071067811865464625, -0.000000000000000000 ) ) ;
#124838 = CARTESIAN_POINT ( 'NONE',  ( 1.021278265688378539, 4.989057771970841770, 5.031783612235352088 ) ) ;
#124839 = DIRECTION ( 'NONE',  ( -0.7071067811865486830, -0.7071067811865464625, 0.000000000000000000 ) ) ;
#124840 = PLANE ( 'NONE',  #44567 ) ;
#124841 = CARTESIAN_POINT ( 'NONE',  ( -57.18398860626899705, 28.73617430169827358, 5.000000000000000000 ) ) ;
#124842 = CARTESIAN_POINT ( 'NONE',  ( 42.95419371712954870, 6.884901960086283523, 3.975000000000002753 ) ) ;
#124843 = PLANE ( 'NONE',  #106975 ) ;
#124844 = LINE ( 'NONE', #127721, #29870 ) ;
#124845 = ORIENTED_EDGE ( 'NONE', *, *, #100972, .T. ) ;
#124846 = ORIENTED_EDGE ( 'NONE', *, *, #141959, .T. ) ;
#124847 = CARTESIAN_POINT ( 'NONE',  ( 35.27083333333330728, -7.949999999999999289, -2.130196079827426203 ) ) ;
#124848 = ORIENTED_EDGE ( 'NONE', *, *, #11465, .T. ) ;
#124849 = ORIENTED_EDGE ( 'NONE', *, *, #85006, .F. ) ;
#124850 = LINE ( 'NONE', #72671, #4586 ) ;
#124851 = ADVANCED_FACE ( 'NONE', ( #102845 ), #47776, .F. ) ;
#124852 = DIRECTION ( 'NONE',  ( 0.6830127018922181881, 0.6830127018922202975, -0.2588190451025214056 ) ) ;
#124853 = VERTEX_POINT ( 'NONE', #1345 ) ;
#124854 = FACE_OUTER_BOUND ( 'NONE', #28609, .T. ) ;
#124856 = ADVANCED_FACE ( 'NONE', ( #59358 ), #131709, .T. ) ;
#124855 = CARTESIAN_POINT ( 'NONE',  ( 4.499999999999983125, 19.08746187583904330, 4.000000000000000000 ) ) ;
#124857 = EDGE_CURVE ( 'NONE', #3513, #8091, #133333, .T. ) ;
#124858 = CARTESIAN_POINT ( 'NONE',  ( 128.2454301918981230, -5.291415217122918513, -3.055000000000000160 ) ) ;
#124859 = ORIENTED_EDGE ( 'NONE', *, *, #39565, .T. ) ;
#124860 = CARTESIAN_POINT ( 'NONE',  ( 183.3316408629057435, -52.14999999999999147, -41.64500000000001023 ) ) ;
#124862 = ORIENTED_EDGE ( 'NONE', *, *, #103834, .F. ) ;
#124861 =( GEOMETRIC_REPRESENTATION_CONTEXT ( 3 ) GLOBAL_UNCERTAINTY_ASSIGNED_CONTEXT ( ( #116055 ) ) GLOBAL_UNIT_ASSIGNED_CONTEXT ( ( #44317, #42891, #130614 ) ) REPRESENTATION_CONTEXT ( 'NONE', 'WORKASPACE' ) );
#124863 = CARTESIAN_POINT ( 'NONE',  ( 23.99999999999985079, 17.58746187583907172, 4.000000000000000000 ) ) ;
#124864 = AXIS2_PLACEMENT_3D ( 'NONE', #117589, #61846, #7415 ) ;
#124865 = VECTOR ( 'NONE', #113845, 1000.000000000000000 ) ;
#124866 = CIRCLE ( 'NONE', #103926, 5.968999999999998529 ) ;
#124867 = ADVANCED_FACE ( 'NONE', ( #2791 ), #80391, .T. ) ;
#124868 = CARTESIAN_POINT ( 'NONE',  ( 12.32816939922345334, -0.7407075233842701500, 4.000000000000000000 ) ) ;
#124869 = CIRCLE ( 'NONE', #94725, 2.500000000000000888 ) ;
#124870 = DIRECTION ( 'NONE',  ( 0.7071067811865487940, 0.7071067811865463515, -0.000000000000000000 ) ) ;
#124871 = VERTEX_POINT ( 'NONE', #23085 ) ;
#124872 = EDGE_CURVE ( 'NONE', #13885, #99232, #67367, .T. ) ;
#124873 = ORIENTED_EDGE ( 'NONE', *, *, #120766, .F. ) ;
#124874 = CARTESIAN_POINT ( 'NONE',  ( 2.999999999999999112, -43.14999999999999147, -40.92499999999998295 ) ) ;
#124875 = EDGE_CURVE ( 'NONE', #135574, #52853, #111559, .T. ) ;
#124876 = CARTESIAN_POINT ( 'NONE',  ( -30.98911971346031180, -22.02621442084248216, 4.990779571109225543 ) ) ;
#124877 = LINE ( 'NONE', #81407, #6042 ) ;
#124878 = DIRECTION ( 'NONE',  ( 0.6830127018922181881, 0.6830127018922202975, -0.2588190451025214056 ) ) ;
#124879 = PLANE ( 'NONE',  #69417 ) ;
#124880 = AXIS2_PLACEMENT_3D ( 'NONE', #100044, #69578, #89854 ) ;
#124881 = ADVANCED_FACE ( 'NONE', ( #100699 ), #138324, .T. ) ;
#124882 = CARTESIAN_POINT ( 'NONE',  ( 57.66209685856478728, -5.291415217122919401, 3.054999999999997939 ) ) ;
#124883 = CARTESIAN_POINT ( 'NONE',  ( 39.29974487139159578, -27.71228299555233576, 4.000000000000000000 ) ) ;
#124884 = CARTESIAN_POINT ( 'NONE',  ( 2.139447441471316935, 2.500000000000000888, 0.000000000000000000 ) ) ;
#124885 = EDGE_LOOP ( 'NONE', ( #79587, #137920, #121350, #69395 ) ) ;
#124886 = EDGE_LOOP ( 'NONE', ( #94412, #12390, #117027 ) ) ;
#124887 = VECTOR ( 'NONE', #99474, 1000.000000000000000 ) ;
#124888 = VECTOR ( 'NONE', #54730, 1000.000000000000000 ) ;
#124889 = CARTESIAN_POINT ( 'NONE',  ( 34.92499999999998295, -22.22500000000000142, 4.500000000000000888 ) ) ;
#124890 = ADVANCED_FACE ( 'NONE', ( #2044 ), #17245, .T. ) ;
#124891 = VERTEX_POINT ( 'NONE', #7036 ) ;
#124892 = AXIS2_PLACEMENT_3D ( 'NONE', #11048, #101659, #1602 ) ;
#124893 = LINE ( 'NONE', #112593, #28021 ) ;
#124894 = EDGE_LOOP ( 'NONE', ( #52252, #69234, #125820, #133457 ) ) ;
#124895 = CARTESIAN_POINT ( 'NONE',  ( -32.67183060077624646, -0.7407075233842805861, 4.000000000000000000 ) ) ;
#124896 = VECTOR ( 'NONE', #35769, 1000.000000000000114 ) ;
#124897 = AXIS2_PLACEMENT_3D ( 'NONE', #12485, #15319, #13183 ) ;
#124898 = VECTOR ( 'NONE', #106586, 1000.000000000000000 ) ;
#124899 = FACE_BOUND ( 'NONE', #62630, .T. ) ;
#124900 = CARTESIAN_POINT ( 'NONE',  ( -29.99451991528749417, 28.92564299267958816, 4.000000000000000000 ) ) ;
#124901 = DIRECTION ( 'NONE',  ( -0.000000000000000000, 0.000000000000000000, 1.000000000000000000 ) ) ;
#124902 = DIRECTION ( 'NONE',  ( 0.6830127018922180770, -0.6830127018922204085, -0.2588190451025213501 ) ) ;
#124903 = FACE_BOUND ( 'NONE', #59323, .T. ) ;
#124905 = EDGE_LOOP ( 'NONE', ( #139957, #132566, #86929, #132064 ) ) ;
#124904 = DIRECTION ( 'NONE',  ( 0.000000000000000000, 0.000000000000000000, 1.000000000000000000 ) ) ;
#124906 = VECTOR ( 'NONE', #3064, 999.9999999999998863 ) ;
#124907 = AXIS2_PLACEMENT_3D ( 'NONE', #124063, #89985, #34927 ) ;
#124908 = DIRECTION ( 'NONE',  ( -0.000000000000000000, -0.3543493200069152693, 0.9351131265310292928 ) ) ;
#124909 = ORIENTED_EDGE ( 'NONE', *, *, #82817, .T. ) ;
#124910 = EDGE_CURVE ( 'NONE', #16142, #51777, #18644, .T. ) ;
#124911 = EDGE_CURVE ( 'NONE', #31681, #64729, #103516, .T. ) ;
#124912 = EDGE_LOOP ( 'NONE', ( #14924, #11287, #65891, #121242 ) ) ;
#124913 = CARTESIAN_POINT ( 'NONE',  ( 62.03709685856478728, -3.054999999999998828, -5.291415217122919401 ) ) ;
#124914 = ORIENTED_EDGE ( 'NONE', *, *, #91991, .F. ) ;
#124915 = DIRECTION ( 'NONE',  ( -1.000000000000000000, -0.000000000000000000, -0.000000000000000000 ) ) ;
#124916 = VERTEX_POINT ( 'NONE', #6311 ) ;
#124917 = DIRECTION ( 'NONE',  ( -0.7071067811865487940, 0.7071067811865463515, 0.000000000000000000 ) ) ;
#124918 = VECTOR ( 'NONE', #71349, 1000.000000000000000 ) ;
#124919 = ADVANCED_FACE ( 'NONE', ( #73088 ), #71644, .F. ) ;
#124920 = DIRECTION ( 'NONE',  ( 0.7071067811865486830, -0.7071067811865464625, -0.000000000000000000 ) ) ;
#124921 = CARTESIAN_POINT ( 'NONE',  ( 5.510786437626906675, -27.52281430457051314, 5.000000000000000000 ) ) ;
#124922 = PLANE ( 'NONE',  #104867 ) ;
#124923 = CARTESIAN_POINT ( 'NONE',  ( 15.65467068707222076, 0.000000000000000000, 2.500000000000000444 ) ) ;
#124924 = ORIENTED_EDGE ( 'NONE', *, *, #52200, .F. ) ;
#124925 = ORIENTED_EDGE ( 'NONE', *, *, #96809, .F. ) ;
#124926 = CARTESIAN_POINT ( 'NONE',  ( 14.24890464969599968, -0.3792994071806725653, 4.162343009174986896 ) ) ;
#124927 = DIRECTION ( 'NONE',  ( 0.7071067811865487940, 0.7071067811865463515, -0.000000000000000000 ) ) ;
#124928 = ORIENTED_EDGE ( 'NONE', *, *, #61724, .F. ) ;
#124929 = ORIENTED_EDGE ( 'NONE', *, *, #89872, .F. ) ;
#124930 = ORIENTED_EDGE ( 'NONE', *, *, #47309, .F. ) ;
#124931 = CARTESIAN_POINT ( 'NONE',  ( -4.499999999999962697, -7.912538124160678699, 4.000000000000000000 ) ) ;
#124932 = ORIENTED_EDGE ( 'NONE', *, *, #140245, .F. ) ;
#124933 = DIRECTION ( 'NONE',  ( -0.000000000000000000, 0.000000000000000000, 1.000000000000000000 ) ) ;
#124934 = CARTESIAN_POINT ( 'NONE',  ( 41.78752705046289151, 0.000000000000000000, -7.949999999999998401 ) ) ;
#124935 = CARTESIAN_POINT ( 'NONE',  ( 2.837903141435219379, -6.871911579029513106, -3.967499999999993587 ) ) ;
#124936 = CARTESIAN_POINT ( 'NONE',  ( 8.671830600776406328, -0.7407075233842701500, 4.000000000000000000 ) ) ;
#124937 = VERTEX_POINT ( 'NONE', #128855 ) ;
#124938 = LINE ( 'NONE', #111946, #45781 ) ;
#124940 = EDGE_CURVE ( 'NONE', #52654, #28957, #49902, .T. ) ;
#124939 = CARTESIAN_POINT ( 'NONE',  ( -34.92500000000001137, 21.72500000000000142, 5.000000000000000000 ) ) ;
#124941 = CARTESIAN_POINT ( 'NONE',  ( -10.82816939922345156, 6.759292476615645917, 4.000000000000000000 ) ) ;
#124943 = ORIENTED_EDGE ( 'NONE', *, *, #16223, .F. ) ;
#124942 = CARTESIAN_POINT ( 'NONE',  ( 57.18398860626899705, 28.73617430169827358, 5.000000000000000000 ) ) ;
#124944 = EDGE_LOOP ( 'NONE', ( #71384, #109190, #66871, #134299 ) ) ;
#124945 = DIRECTION ( 'NONE',  ( -0.000000000000000000, 1.000000000000000000, -0.000000000000000000 ) ) ;
#124946 = CARTESIAN_POINT ( 'NONE',  ( -17.39513766812467921, 21.75929247661549937, 21.32995629748190325 ) ) ;
#124947 = CARTESIAN_POINT ( 'NONE',  ( 156.1500000000000057, -49.14999999999999147, 49.92499999999997584 ) ) ;
#124948 = ORIENTED_EDGE ( 'NONE', *, *, #85662, .F. ) ;
#124949 = LINE ( 'NONE', #118145, #78313 ) ;
#124950 = PRESENTATION_STYLE_ASSIGNMENT (( #111207 ) ) ;
#124951 = DIRECTION ( 'NONE',  ( -0.6830127018922181881, 0.6830127018922202975, -0.2588190451025214056 ) ) ;
#124952 = VECTOR ( 'NONE', #99550, 999.9999999999998863 ) ;
#124953 = VERTEX_POINT ( 'NONE', #115090 ) ;
#124954 = VECTOR ( 'NONE', #30642, 1000.000000000000000 ) ;
#124955 = AXIS2_PLACEMENT_3D ( 'NONE', #65455, #110324, #87173 ) ;
#124956 = VECTOR ( 'NONE', #7887, 999.9999999999998863 ) ;
#124957 = DIRECTION ( 'NONE',  ( 0.000000000000000000, 1.000000000000000000, 0.000000000000000000 ) ) ;
#124958 = PLANE ( 'NONE',  #118764 ) ;
#124959 =( BOUNDED_CURVE ( )  B_SPLINE_CURVE ( 3, ( #52584, #119258, #17793, #28719 ),
 .UNSPECIFIED., .F., .T. ) 
 B_SPLINE_CURVE_WITH_KNOTS ( ( 4, 4 ),
 ( 4.350170835173033268, 4.500739107949210727 ),
 .UNSPECIFIED. ) 
 CURVE ( )  GEOMETRIC_REPRESENTATION_ITEM ( )  RATIONAL_B_SPLINE_CURVE ( ( 1.000000000000000000, 0.9981116584018959736, 0.9981116584018959736, 1.000000000000000000 ) ) 
 REPRESENTATION_ITEM ( '' )  );
#124960 = CARTESIAN_POINT ( 'NONE',  ( 6.608306282870438864, 1.633150327867687324, -6.094999999999991758 ) ) ;
#124962 = EDGE_CURVE ( 'NONE', #43532, #113219, #128171, .T. ) ;
#124961 = AXIS2_PLACEMENT_3D ( 'NONE', #45965, #48094, #102484 ) ;
#124963 = CARTESIAN_POINT ( 'NONE',  ( 78.00000000000000000, 0.000000000000000000, -7.950000000000000178 ) ) ;
#124964 = CARTESIAN_POINT ( 'NONE',  ( -11.70025512860841133, -27.71228299555198049, 4.000000000000000000 ) ) ;
#124965 = ADVANCED_FACE ( 'NONE', ( #60060 ), #16510, .T. ) ;
#124966 = VERTEX_POINT ( 'NONE', #81833 ) ;
#124967 = ORIENTED_EDGE ( 'NONE', *, *, #73669, .F. ) ;
#124968 = CARTESIAN_POINT ( 'NONE',  ( -12.69999999999998153, 3.061616997868383634E-16, -2.500000000000000444 ) ) ;
#124969 = VECTOR ( 'NONE', #16781, 1000.000000000000227 ) ;
#124970 = DIRECTION ( 'NONE',  ( -0.000000000000000000, 0.3543493200069153248, 0.9351131265310292928 ) ) ;
#124971 = ADVANCED_FACE ( 'NONE', ( #94080 ), #82512, .F. ) ;
#124972 = EDGE_CURVE ( 'NONE', #16103, #71793, #32165, .T. ) ;
#124973 = CARTESIAN_POINT ( 'NONE',  ( 6.978736474768552966, -5.808823158059033709, 5.808823158059035485 ) ) ;
#124974 = CARTESIAN_POINT ( 'NONE',  ( 54.29974487139159578, -27.71228299555243879, 4.000000000000000000 ) ) ;
#124975 = VECTOR ( 'NONE', #24924, 1000.000000000000114 ) ;
#124976 = CARTESIAN_POINT ( 'NONE',  ( 34.92499999999998295, 22.22500000000000142, 4.000000000000000000 ) ) ;
#124977 = PLANE ( 'NONE',  #27480 ) ;
#124978 = CARTESIAN_POINT ( 'NONE',  ( -32.99451991528749062, 28.92564299267960948, 4.000000000000000000 ) ) ;
#124979 = EDGE_LOOP ( 'NONE', ( #85958, #1440, #42019, #6727 ) ) ;
#124980 = ADVANCED_FACE ( 'NONE', ( #39003 ), #142970, .T. ) ;
#124981 = SURFACE_SIDE_STYLE ('',( #101801 ) ) ;
#124982 = CARTESIAN_POINT ( 'NONE',  ( -3.656710001662112131, 3.759292476615685441, 13.27625715073264523 ) ) ;
#124983 = VECTOR ( 'NONE', #59599, 1000.000000000000000 ) ;
#124984 = VECTOR ( 'NONE', #25159, 1000.000000000000000 ) ;
#124985 = FACE_OUTER_BOUND ( 'NONE', #14138, .T. ) ;
#124986 = CARTESIAN_POINT ( 'NONE',  ( 57.07876352523144448, -7.482591942790327058E-16, 6.109999999999999432 ) ) ;
#124987 = DIRECTION ( 'NONE',  ( 0.7071067811865487940, -0.7071067811865463515, 0.000000000000000000 ) ) ;
#124988 = EDGE_CURVE ( 'NONE', #56522, #64090, #94848, .T. ) ;
#124989 = VECTOR ( 'NONE', #136080, 1000.000000000000000 ) ;
#124990 = DIRECTION ( 'NONE',  ( 0.000000000000000000, -1.000000000000000000, 0.000000000000000000 ) ) ;
#124991 = EDGE_LOOP ( 'NONE', ( #4905, #125212, #54853, #44465, #125432 ) ) ;
#124992 = LINE ( 'NONE', #25672, #80744 ) ;
#124993 = ORIENTED_EDGE ( 'NONE', *, *, #122504, .T. ) ;
#124994 = CARTESIAN_POINT ( 'NONE',  ( -33.18398860626899705, 28.73617430169810305, 5.000000000000000000 ) ) ;
#124995 = AXIS2_PLACEMENT_3D ( 'NONE', #66393, #99708, #64973 ) ;
#124996 = EDGE_CURVE ( 'NONE', #37520, #130798, #60622, .T. ) ;
#124997 = VECTOR ( 'NONE', #100068, 1000.000000000000227 ) ;
#124998 = LINE ( 'NONE', #93090, #78549 ) ;
#124999 = DIRECTION ( 'NONE',  ( 0.7071067811865487940, 0.7071067811865463515, 0.000000000000000000 ) ) ;
#125000 = CARTESIAN_POINT ( 'NONE',  ( -30.18398860626900060, 28.73617430169808173, 5.000000000000000000 ) ) ;
#125001 = CARTESIAN_POINT ( 'NONE',  ( -0.4892135623730947680, -27.52281430457055578, 5.000000000000000000 ) ) ;
#125002 = VECTOR ( 'NONE', #91205, 1000.000000000000000 ) ;
#125003 = ORIENTED_EDGE ( 'NONE', *, *, #15228, .F. ) ;
#125004 = ORIENTED_EDGE ( 'NONE', *, *, #136620, .F. ) ;
#125005 = LINE ( 'NONE', #114128, #94956 ) ;
#125006 = DIRECTION ( 'NONE',  ( -1.000000000000000000, -1.224606353822377258E-16, -0.000000000000000000 ) ) ;
#125007 = EDGE_CURVE ( 'NONE', #22876, #141378, #54202, .T. ) ;
#125008 = CARTESIAN_POINT ( 'NONE',  ( 33.18398860626899705, 28.73617430169810305, 5.000000000000000000 ) ) ;
#125009 = CARTESIAN_POINT ( 'NONE',  ( 117.2291666666666572, 7.950000000000001954, -2.130196079827421762 ) ) ;
#125010 = CARTESIAN_POINT ( 'NONE',  ( 73.72502705046288440, 5.819803920172573086, -5.819803920172572198 ) ) ;
#125011 = LINE ( 'NONE', #39456, #15983 ) ;
#125012 = ORIENTED_EDGE ( 'NONE', *, *, #123166, .T. ) ;
#125013 = CARTESIAN_POINT ( 'NONE',  ( 63.85416666666665719, -2.130196079827425315, -7.950000000000001066 ) ) ;
#125014 = CARTESIAN_POINT ( 'NONE',  ( -0.7933393645784717618, 21.75929247661549581, 4.998822639870701856 ) ) ;
#125015 = FACE_OUTER_BOUND ( 'NONE', #119906, .T. ) ;
#125016 = LINE ( 'NONE', #114140, #98400 ) ;
#125017 = ADVANCED_FACE ( 'NONE', ( #65060 ), #63641, .T. ) ;
#125018 = VECTOR ( 'NONE', #115338, 1000.000000000000000 ) ;
#125019 = ORIENTED_EDGE ( 'NONE', *, *, #137864, .T. ) ;
#125020 = PLANE ( 'NONE',  #2733 ) ;
#125021 = EDGE_CURVE ( 'NONE', #133299, #49766, #141912, .T. ) ;
#125022 = DIRECTION ( 'NONE',  ( 0.6830127018922181881, 0.6830127018922202975, -0.2588190451025214056 ) ) ;
#125023 = CARTESIAN_POINT ( 'NONE',  ( 63.72959685856477563, -6.110000000000000320, -1.637169565754161393 ) ) ;
#125024 = EDGE_CURVE ( 'NONE', #135734, #105207, #131730, .T. ) ;
#125025 = PLANE ( 'NONE',  #66829 ) ;
#125026 = EDGE_LOOP ( 'NONE', ( #110212, #123993, #78801, #35714 ) ) ;
#125027 = ORIENTED_EDGE ( 'NONE', *, *, #27618, .F. ) ;
#125028 = VECTOR ( 'NONE', #8123, 1000.000000000000000 ) ;
#125029 = ADVANCED_FACE ( 'NONE', ( #107803 ), #86082, .F. ) ;
#125030 = CARTESIAN_POINT ( 'NONE',  ( 12.71159235450332048, -2.500000000000000000, 3.061616997868384127E-16 ) ) ;
#125031 = DIRECTION ( 'NONE',  ( 0.7071067811865487940, 0.7071067811865463515, 0.000000000000000000 ) ) ;
#125032 = PLANE ( 'NONE',  #41686 ) ;
#125033 = CARTESIAN_POINT ( 'NONE',  ( 60.18398860626900415, 28.73617430169829490, 5.000000000000000000 ) ) ;
#125035 = ORIENTED_EDGE ( 'NONE', *, *, #64607, .F. ) ;
#125034 = DIRECTION ( 'NONE',  ( 0.000000000000000000, 0.000000000000000000, 1.000000000000000000 ) ) ;
#125036 = DIRECTION ( 'NONE',  ( 0.6830127018922180770, -0.6830127018922204085, -0.2588190451025213501 ) ) ;
#125037 = PLANE ( 'NONE',  #77914 ) ;
#125038 = DIRECTION ( 'NONE',  ( -0.7071067811865486830, -0.7071067811865464625, 0.000000000000000000 ) ) ;
#125039 = AXIS2_PLACEMENT_3D ( 'NONE', #26575, #38182, #116444 ) ;
#125040 = FACE_OUTER_BOUND ( 'NONE', #30485, .T. ) ;
#125041 = VECTOR ( 'NONE', #37797, 1000.000000000000000 ) ;
#125042 = ORIENTED_EDGE ( 'NONE', *, *, #124686, .T. ) ;
#125043 = EDGE_LOOP ( 'NONE', ( #43931, #53791, #67302, #55152 ) ) ;
#125044 = EDGE_CURVE ( 'NONE', #133299, #63176, #57642, .T. ) ;
#125045 =( NAMED_UNIT ( * ) PLANE_ANGLE_UNIT ( ) SI_UNIT ( $, .RADIAN. ) );
#125046 = CARTESIAN_POINT ( 'NONE',  ( 10.60343192894636033, -14.24070752338413648, 19.24067776001728447 ) ) ;
#125047 = CARTESIAN_POINT ( 'NONE',  ( 111.0583603837962130, -7.949999999999996625, -2.130196079827426203 ) ) ;
#125048 = CARTESIAN_POINT ( 'NONE',  ( 20.99451991528748707, 28.92564299267952777, 4.000000000000000000 ) ) ;
#125049 = VERTEX_POINT ( 'NONE', #64327 ) ;
#125050 = VERTEX_POINT ( 'NONE', #21535 ) ;
#125051 = PLANE ( 'NONE',  #14492 ) ;
#125053 = EDGE_CURVE ( 'NONE', #36381, #141411, #108493, .T. ) ;
#125052 = CARTESIAN_POINT ( 'NONE',  ( 11.29289321881337926, -12.74070752338415602, 5.000000000000000000 ) ) ;
#125055 = EDGE_LOOP ( 'NONE', ( #11424, #107083, #70362, #98245 ) ) ;
#125054 = VECTOR ( 'NONE', #24558, 1000.000000000000000 ) ;
#125056 = ORIENTED_EDGE ( 'NONE', *, *, #129314, .T. ) ;
#125057 = CARTESIAN_POINT ( 'NONE',  ( 15.51665438641034633, 22.22500000000000142, 4.500000000000000888 ) ) ;
#125058 = CARTESIAN_POINT ( 'NONE',  ( 36.18398860626899705, 28.73617430169812437, 5.000000000000000000 ) ) ;
#125059 = VECTOR ( 'NONE', #64891, 1000.000000000000227 ) ;
#125060 = AXIS2_PLACEMENT_3D ( 'NONE', #55271, #34229, #850 ) ;
#125061 = AXIS2_PLACEMENT_3D ( 'NONE', #23879, #101423, #110145 ) ;
#125062 = ORIENTED_EDGE ( 'NONE', *, *, #109471, .T. ) ;
#125063 = AXIS2_PLACEMENT_3D ( 'NONE', #81824, #104215, #4885 ) ;
#125064 = FACE_BOUND ( 'NONE', #56390, .T. ) ;
#125065 = CARTESIAN_POINT ( 'NONE',  ( 27.18398860626900060, 28.73617430169806042, 5.000000000000000000 ) ) ;
#125066 = EDGE_CURVE ( 'NONE', #68801, #19998, #87507, .T. ) ;
#125067 = DIRECTION ( 'NONE',  ( 0.6830127018922180770, -0.6830127018922204085, -0.2588190451025213501 ) ) ;
#125068 = FACE_OUTER_BOUND ( 'NONE', #87720, .T. ) ;
#125069 = AXIS2_PLACEMENT_3D ( 'NONE', #119289, #76541, #52612 ) ;
#125070 = LINE ( 'NONE', #68579, #138327 ) ;
#125071 = FILL_AREA_STYLE ('',( #38087 ) ) ;
#125072 = DIRECTION ( 'NONE',  ( 1.000000000000000000, 0.000000000000000000, 0.000000000000000000 ) ) ;
#125073 = VERTEX_POINT ( 'NONE', #97657 ) ;
#125074 = EDGE_CURVE ( 'NONE', #113821, #6521, #32419, .T. ) ;
#125075 = EDGE_LOOP ( 'NONE', ( #53636, #25901, #8499, #122536 ) ) ;
#125076 = CARTESIAN_POINT ( 'NONE',  ( 94.84959685856476597, 6.109999999999996767, 1.637169565754163836 ) ) ;
#125077 = ORIENTED_EDGE ( 'NONE', *, *, #120874, .T. ) ;
#125078 = CARTESIAN_POINT ( 'NONE',  ( 19.25000000000000355, -7.464222240803106570E-16, -6.094999999999989981 ) ) ;
#125079 = AXIS2_PLACEMENT_3D ( 'NONE', #40520, #95588, #139848 ) ;
#125080 = DIRECTION ( 'NONE',  ( 0.7071067811865486830, -0.7071067811865464625, -0.000000000000000000 ) ) ;
#125081 = EDGE_CURVE ( 'NONE', #18455, #73811, #76654, .T. ) ;
#125082 = CARTESIAN_POINT ( 'NONE',  ( 6.781626882924904898, 21.74787736706805674, 4.999607392498049308 ) ) ;
#125083 =( GEOMETRIC_REPRESENTATION_CONTEXT ( 3 ) GLOBAL_UNCERTAINTY_ASSIGNED_CONTEXT ( ( #14086 ) ) GLOBAL_UNIT_ASSIGNED_CONTEXT ( ( #43043, #40890, #63389 ) ) REPRESENTATION_CONTEXT ( 'NONE', 'WORKASPACE' ) );
#125085 = ADVANCED_FACE ( 'NONE', ( #89640 ), #80228, .F. ) ;
#125084 = DIRECTION ( 'NONE',  ( 0.3543493200069162685, -0.000000000000000000, -0.9351131265310288487 ) ) ;
#125086 = ORIENTED_EDGE ( 'NONE', *, *, #63333, .F. ) ;
#125087 = LINE ( 'NONE', #115587, #129400 ) ;
#125088 = AXIS2_PLACEMENT_3D ( 'NONE', #3629, #13804, #55941 ) ;
#125089 = CARTESIAN_POINT ( 'NONE',  ( 0.000000000000000000, -16.60178936734448740, 0.8616154019347507242 ) ) ;
#125090 = DIRECTION ( 'NONE',  ( -0.7071067811865486830, -0.7071067811865464625, 0.000000000000000000 ) ) ;
#125091 = VECTOR ( 'NONE', #113403, 1000.000000000000000 ) ;
#125092 = DIRECTION ( 'NONE',  ( -0.7071067811865486830, -0.7071067811865464625, -0.000000000000000000 ) ) ;
#125093 = CARTESIAN_POINT ( 'NONE',  ( -5.999999999999963585, 4.965500833774324718, -4.007596771432642591 ) ) ;
#125094 = ORIENTED_EDGE ( 'NONE', *, *, #59762, .F. ) ;
#125095 = AXIS2_PLACEMENT_3D ( 'NONE', #6022, #104655, #82929 ) ;
#125096 = CARTESIAN_POINT ( 'NONE',  ( 34.47516574401890210, -1.509482387884363064, 4.998110765256833510 ) ) ;
#125097 = DIRECTION ( 'NONE',  ( -0.7071067811865486830, -0.7071067811865464625, 0.000000000000000000 ) ) ;
#125098 = ORIENTED_EDGE ( 'NONE', *, *, #85241, .T. ) ;
#125099 = EDGE_LOOP ( 'NONE', ( #113874, #114899, #129218, #89256 ) ) ;
#125100 = CIRCLE ( 'NONE', #25549, 2.055000000000000604 ) ;
#125101 = ORIENTED_EDGE ( 'NONE', *, *, #63667, .F. ) ;
#125102 = CARTESIAN_POINT ( 'NONE',  ( 49.72959685856476852, -6.110000000000000320, -1.637169565754161393 ) ) ;
#125103 = VERTEX_POINT ( 'NONE', #58504 ) ;
#125104 = AXIS2_PLACEMENT_3D ( 'NONE', #131512, #88735, #964 ) ;
#125105 = CARTESIAN_POINT ( 'NONE',  ( 3.399972949537105826, 4.461849672132297329, -4.461849672132302658 ) ) ;
#125106 = DIRECTION ( 'NONE',  ( 1.000000000000000000, 0.000000000000000000, 0.000000000000000000 ) ) ;
#125107 = ORIENTED_EDGE ( 'NONE', *, *, #88492, .T. ) ;
#125108 = DIRECTION ( 'NONE',  ( 0.7071067811865487940, 0.7071067811865463515, 0.000000000000000000 ) ) ;
#125109 = ORIENTED_EDGE ( 'NONE', *, *, #129371, .F. ) ;
#125110 = PLANE ( 'NONE',  #141421 ) ;
#125111 = AXIS2_PLACEMENT_3D ( 'NONE', #57301, #60144, #92025 ) ;
#125113 = ORIENTED_EDGE ( 'NONE', *, *, #98585, .T. ) ;
#125112 = CARTESIAN_POINT ( 'NONE',  ( 32.99999999999976552, -3.412538124160717778, 4.000000000000000000 ) ) ;
#125114 = VERTEX_POINT ( 'NONE', #56354 ) ;
#125115 = DIRECTION ( 'NONE',  ( -1.000000000000000000, -1.224606353822377258E-16, -0.000000000000000000 ) ) ;
#125116 = CARTESIAN_POINT ( 'NONE',  ( 34.42499999999998295, -0.02281430457060432127, 5.000000000000000000 ) ) ;
#125117 = CARTESIAN_POINT ( 'NONE',  ( -25.39999999999996305, 0.000000000000000000, 0.000000000000000000 ) ) ;
#125118 = VERTEX_POINT ( 'NONE', #68633 ) ;
#125119 = LINE ( 'NONE', #25808, #87513 ) ;
#125120 = EDGE_LOOP ( 'NONE', ( #21183, #129568, #94426, #134376 ) ) ;
#125121 = ORIENTED_EDGE ( 'NONE', *, *, #27769, .T. ) ;
#125122 = EDGE_LOOP ( 'NONE', ( #53261, #100084, #122491 ) ) ;
#125123 = EDGE_CURVE ( 'NONE', #135646, #54723, #13473, .T. ) ;
#125124 = DIRECTION ( 'NONE',  ( -0.7071067811865486830, 0.7071067811865464625, 0.000000000000000000 ) ) ;
#125125 = VECTOR ( 'NONE', #113888, 1000.000000000000000 ) ;
#125126 = CARTESIAN_POINT ( 'NONE',  ( 12.49289321881344605, -22.06289321881344634, -40.00000000000000000 ) ) ;
#125127 = FACE_OUTER_BOUND ( 'NONE', #38135, .T. ) ;
#125128 = EDGE_CURVE ( 'NONE', #23467, #15784, #124412, .T. ) ;
#125129 = ADVANCED_FACE ( 'NONE', ( #78072 ), #78782, .F. ) ;
#125130 = DIRECTION ( 'NONE',  ( -0.000000000000000000, 0.3543493200069153248, 0.9351131265310292928 ) ) ;
#125131 = ORIENTED_EDGE ( 'NONE', *, *, #129699, .F. ) ;
#125132 = CIRCLE ( 'NONE', #134476, 0.5000000000000004441 ) ;
#125133 = CARTESIAN_POINT ( 'NONE',  ( 0.000000000000000000, 0.000000000000000000, 7.950000000000000178 ) ) ;
#125134 = EDGE_CURVE ( 'NONE', #70009, #104583, #100532, .T. ) ;
#125135 = EDGE_CURVE ( 'NONE', #139751, #83228, #122248, .T. ) ;
#125136 = CARTESIAN_POINT ( 'NONE',  ( 25.79123647476855652, -9.717572351234235426E-16, -7.934999999999990727 ) ) ;
#125137 = DIRECTION ( 'NONE',  ( -1.000000000000000000, 0.000000000000000000, 0.000000000000000000 ) ) ;
#125138 = EDGE_CURVE ( 'NONE', #19533, #39593, #119825, .T. ) ;
#125139 = FACE_OUTER_BOUND ( 'NONE', #62151, .T. ) ;
#125140 = DIRECTION ( 'NONE',  ( -0.000000000000000000, 0.000000000000000000, 1.000000000000000000 ) ) ;
#125141 = ORIENTED_EDGE ( 'NONE', *, *, #78190, .T. ) ;
#125142 = ORIENTED_EDGE ( 'NONE', *, *, #33653, .T. ) ;
#125143 = EDGE_CURVE ( 'NONE', #77572, #97669, #102680, .T. ) ;
#125144 = VERTEX_POINT ( 'NONE', #11324 ) ;
#125145 = SURFACE_STYLE_USAGE ( .BOTH. , #23696 ) ;
#125146 = DIRECTION ( 'NONE',  ( -1.000000000000000000, -1.224606353822377258E-16, -0.000000000000000000 ) ) ;
#125147 = LINE ( 'NONE', #4025, #22172 ) ;
#125148 = EDGE_CURVE ( 'NONE', #35574, #114247, #112817, .T. ) ;
#125149 = DIRECTION ( 'NONE',  ( -0.7071067811865487940, 0.7071067811865463515, 0.000000000000000000 ) ) ;
#125150 = AXIS2_PLACEMENT_3D ( 'NONE', #77688, #100146, #11660 ) ;
#125151 = DIRECTION ( 'NONE',  ( -0.000000000000000000, 0.000000000000000000, 1.000000000000000000 ) ) ;
#125152 = CARTESIAN_POINT ( 'NONE',  ( 10.32500000000000107, 8.432637487761466488, -4.375000000000001776 ) ) ;
#125153 = CARTESIAN_POINT ( 'NONE',  ( 29.99999999999979039, -21.41253812416053748, 4.000000000000000000 ) ) ;
#125154 = CIRCLE ( 'NONE', #65055, 5.968999999999998529 ) ;
#125155 = ADVANCED_FACE ( 'NONE', ( #57053 ), #3322, .F. ) ;
#125156 = VECTOR ( 'NONE', #136627, 1000.000000000000227 ) ;
#125157 = CYLINDRICAL_SURFACE ( 'NONE', #8940, 2.500000000000000000 ) ;
#125158 = CARTESIAN_POINT ( 'NONE',  ( -36.29974487139159578, -27.71228299555231445, 4.000000000000000000 ) ) ;
#125159 = CARTESIAN_POINT ( 'NONE',  ( -33.29974487139158867, -27.71228299555229313, 4.000000000000000000 ) ) ;
#125160 = CARTESIAN_POINT ( 'NONE',  ( 8.700255128608413102, -27.71228299555199825, 4.000000000000000000 ) ) ;
#125161 = LINE ( 'NONE', #16367, #18672 ) ;
#125162 = ORIENTED_EDGE ( 'NONE', *, *, #21081, .F. ) ;
#125163 = VECTOR ( 'NONE', #108164, 999.9999999999998863 ) ;
#125164 = CONICAL_SURFACE ( 'NONE', #48811, 2.500000000000000444, 0.9599310885968830309 ) ;
#125165 = VECTOR ( 'NONE', #36703, 1000.000000000000000 ) ;
#125167 = PRESENTATION_STYLE_ASSIGNMENT (( #67982 ) ) ;
#125166 = VECTOR ( 'NONE', #112924, 999.9999999999998863 ) ;
#125168 = EDGE_LOOP ( 'NONE', ( #134603, #65309, #129388, #12087 ) ) ;
#125169 = VECTOR ( 'NONE', #45451, 1000.000000000000000 ) ;
#125170 = EDGE_CURVE ( 'NONE', #122142, #13717, #101223, .T. ) ;
#125171 = LINE ( 'NONE', #49785, #55267 ) ;
#125173 = ORIENTED_EDGE ( 'NONE', *, *, #92777, .T. ) ;
#125172 = DIRECTION ( 'NONE',  ( 0.7071067811865487940, 0.7071067811865463515, 0.000000000000000000 ) ) ;
#125174 = DIRECTION ( 'NONE',  ( -1.000000000000000000, -0.000000000000000000, 0.000000000000000000 ) ) ;
#125175 = DIRECTION ( 'NONE',  ( -0.000000000000000000, -0.3543493200069152693, 0.9351131265310292928 ) ) ;
#125176 = VERTEX_POINT ( 'NONE', #14216 ) ;
#125177 = CARTESIAN_POINT ( 'NONE',  ( -34.82816939922327748, -5.240707523384225297, 4.000000000000000000 ) ) ;
#125178 = ORIENTED_EDGE ( 'NONE', *, *, #122342, .F. ) ;
#125179 = DIRECTION ( 'NONE',  ( 0.7071067811865487940, 0.7071067811865463515, 0.000000000000000000 ) ) ;
#125180 = CIRCLE ( 'NONE', #134406, 2.500000000000000444 ) ;
#125181 = EDGE_LOOP ( 'NONE', ( #14469, #44019, #91422, #131357 ) ) ;
#125182 = ADVANCED_FACE ( 'NONE', ( #35297 ), #136000, .F. ) ;
#125183 = FACE_OUTER_BOUND ( 'NONE', #30667, .T. ) ;
#125184 = CARTESIAN_POINT ( 'NONE',  ( 106.2458603837962272, 3.974999999999996980, 6.884901960086287964 ) ) ;
#125185 = DIRECTION ( 'NONE',  ( -0.7071067811865486830, 0.7071067811865464625, 0.000000000000000000 ) ) ;
#125186 = DIRECTION ( 'NONE',  ( 0.6830127018922180770, -0.6830127018922204085, -0.2588190451025213501 ) ) ;
#125187 = EDGE_LOOP ( 'NONE', ( #81575, #103920, #121465, #95177 ) ) ;
#125188 = CARTESIAN_POINT ( 'NONE',  ( -23.51078643762690490, -27.52281430457038880, 5.000000000000000000 ) ) ;
#125189 = DIRECTION ( 'NONE',  ( 0.000000000000000000, 0.000000000000000000, 1.000000000000000000 ) ) ;
#125190 = DIRECTION ( 'NONE',  ( -0.3543493200069162685, -0.000000000000000000, -0.9351131265310288487 ) ) ;
#125191 = CARTESIAN_POINT ( 'NONE',  ( 26.25000000000000355, -7.464222240803106570E-16, -6.094999999999989981 ) ) ;
#125193 = CIRCLE ( 'NONE', #64988, 0.5000000000000004441 ) ;
#125192 = LINE ( 'NONE', #133237, #23616 ) ;
#125194 = DIRECTION ( 'NONE',  ( -0.6830127018922181881, 0.6830127018922202975, -0.2588190451025214056 ) ) ;
#125195 = CARTESIAN_POINT ( 'NONE',  ( 26.99999999999981526, 19.55218569542896390, 5.000000000000000000 ) ) ;
#125196 = EDGE_LOOP ( 'NONE', ( #42148, #143451, #2057, #5942 ) ) ;
#125197 = AXIS2_PLACEMENT_3D ( 'NONE', #26979, #104538, #92954 ) ;
#125198 = CARTESIAN_POINT ( 'NONE',  ( 33.48921356237309510, -27.52281430457078670, 5.000000000000000000 ) ) ;
#125199 = EDGE_CURVE ( 'NONE', #103729, #120153, #90352, .T. ) ;
#125200 = ORIENTED_EDGE ( 'NONE', *, *, #4694, .F. ) ;
#125201 = VECTOR ( 'NONE', #67678, 1000.000000000000000 ) ;
#125202 = CARTESIAN_POINT ( 'NONE',  ( 91.29209685856477563, -5.291415217122921177, 3.054999999999999272 ) ) ;
#125203 = ADVANCED_FACE ( 'NONE', ( #46918 ), #55604, .T. ) ;
#125204 = VECTOR ( 'NONE', #119806, 1000.000000000000000 ) ;
#125205 = CARTESIAN_POINT ( 'NONE',  ( -6.792893218813404133, 12.75929247661558996, 5.000000000000000000 ) ) ;
#125206 = DIRECTION ( 'NONE',  ( -0.7071067811865487940, 0.7071067811865463515, -0.000000000000000000 ) ) ;
#125207 = PLANE ( 'NONE',  #82673 ) ;
#125208 = ORIENTED_EDGE ( 'NONE', *, *, #102202, .F. ) ;
#125209 = LINE ( 'NONE', #68705, #21109 ) ;
#125210 = EDGE_CURVE ( 'NONE', #81380, #135817, #33857, .T. ) ;
#125211 = CARTESIAN_POINT ( 'NONE',  ( 12.29974487139158512, -27.71228299555214747, 4.000000000000000000 ) ) ;
#125212 = ORIENTED_EDGE ( 'NONE', *, *, #114262, .F. ) ;
#125213 = PLANE ( 'NONE',  #81033 ) ;
#125214 = VECTOR ( 'NONE', #37268, 1000.000000000000000 ) ;
#125215 = DIRECTION ( 'NONE',  ( 0.000000000000000000, 0.000000000000000000, 1.000000000000000000 ) ) ;
#125217 = ORIENTED_EDGE ( 'NONE', *, *, #118964, .T. ) ;
#125216 = DIRECTION ( 'NONE',  ( -1.000000000000000000, -0.000000000000000000, -0.000000000000000000 ) ) ;
#125218 = DIRECTION ( 'NONE',  ( 0.000000000000000000, 0.000000000000000000, -1.000000000000000000 ) ) ;
#125219 = CARTESIAN_POINT ( 'NONE',  ( -39.29974487139159578, -27.71228299555233576, 4.000000000000000000 ) ) ;
#125220 = CARTESIAN_POINT ( 'NONE',  ( -30.18398860626900060, 28.73617430169808173, 5.000000000000000000 ) ) ;
#125221 = ORIENTED_EDGE ( 'NONE', *, *, #94398, .F. ) ;
#125222 = ORIENTED_EDGE ( 'NONE', *, *, #143042, .T. ) ;
#125223 = ORIENTED_EDGE ( 'NONE', *, *, #100410, .T. ) ;
#125224 = CARTESIAN_POINT ( 'NONE',  ( 83.85459685856478984, -1.637169565754161615, 6.110000000000000320 ) ) ;
#125225 = MECHANICAL_DESIGN_GEOMETRIC_PRESENTATION_REPRESENTATION (  '', ( #122841 ), #141349 ) ;
#125226 = ORIENTED_EDGE ( 'NONE', *, *, #18379, .F. ) ;
#125227 = EDGE_CURVE ( 'NONE', #116279, #2318, #111379, .T. ) ;
#125228 = CARTESIAN_POINT ( 'NONE',  ( -36.48921356237310221, -27.52281430457080802, 5.000000000000000000 ) ) ;
#125229 = CIRCLE ( 'NONE', #18708, 3.999999999999989786 ) ;
#125230 = CARTESIAN_POINT ( 'NONE',  ( -29.99999999999979039, -13.97847968911263017, -0.1324546996127494158 ) ) ;
#125231 = DIRECTION ( 'NONE',  ( 0.3543493200069162685, -0.000000000000000000, -0.9351131265310288487 ) ) ;
#125232 = ORIENTED_EDGE ( 'NONE', *, *, #117760, .T. ) ;
#125233 = CARTESIAN_POINT ( 'NONE',  ( 103.6666666666666714, 6.884901960086285300, 3.975000000000003642 ) ) ;
#125234 = DIRECTION ( 'NONE',  ( -0.7071067811865486830, -0.7071067811865464625, 0.000000000000000000 ) ) ;
#125235 = CARTESIAN_POINT ( 'NONE',  ( 73.84959685856480860, 6.109999999999996767, 1.637169565754163836 ) ) ;
#125236 = EDGE_LOOP ( 'NONE', ( #141962, #72375, #56678, #41961 ) ) ;
#125237 = EDGE_CURVE ( 'NONE', #12885, #10266, #59880, .T. ) ;
#125238 = CARTESIAN_POINT ( 'NONE',  ( -66.48921356237309510, -27.52281430457101763, 5.000000000000000000 ) ) ;
#125239 = LINE ( 'NONE', #142199, #78019 ) ;
#125240 = DIRECTION ( 'NONE',  ( 0.3543493200069162685, -0.000000000000000000, -0.9351131265310288487 ) ) ;
#125241 = VECTOR ( 'NONE', #42612, 999.9999999999998863 ) ;
#125242 = VERTEX_POINT ( 'NONE', #94618 ) ;
#125243 = VERTEX_POINT ( 'NONE', #83053 ) ;
#125244 = ADVANCED_FACE ( 'NONE', ( #81655 ), #137444, .F. ) ;
#125245 = CARTESIAN_POINT ( 'NONE',  ( 45.28752705046289151, 0.000000000000000000, -7.949999999999998401 ) ) ;
#125246 = CARTESIAN_POINT ( 'NONE',  ( 24.12956980810188767, -3.967499999999998028, -6.871911579029511330 ) ) ;
#125247 = CARTESIAN_POINT ( 'NONE',  ( -34.82816939922328459, 0.7592924766157104211, 4.000000000000000000 ) ) ;
#125248 = VECTOR ( 'NONE', #117328, 1000.000000000000000 ) ;
#125249 = FACE_OUTER_BOUND ( 'NONE', #65554, .T. ) ;
#125250 = PLANE ( 'NONE',  #141326 ) ;
#125251 = CARTESIAN_POINT ( 'NONE',  ( -27.29974487139158512, -27.71228299555225405, 4.000000000000000000 ) ) ;
#125252 =( NAMED_UNIT ( * ) PLANE_ANGLE_UNIT ( ) SI_UNIT ( $, .RADIAN. ) );
#125253 = ORIENTED_EDGE ( 'NONE', *, *, #53585, .F. ) ;
#125254 = ORIENTED_EDGE ( 'NONE', *, *, #54701, .F. ) ;
#125255 = CARTESIAN_POINT ( 'NONE',  ( 8.750000000000000000, -7.464222240803106570E-16, -6.094999999999989981 ) ) ;
#125256 = ORIENTED_EDGE ( 'NONE', *, *, #95204, .T. ) ;
#125257 = VECTOR ( 'NONE', #85529, 1000.000000000000114 ) ;
#125258 = EDGE_CURVE ( 'NONE', #29217, #123150, #104054, .T. ) ;
#125259 = VECTOR ( 'NONE', #75894, 1000.000000000000000 ) ;
#125260 = CIRCLE ( 'NONE', #213, 2.500000000000000888 ) ;
#125262 = EDGE_CURVE ( 'NONE', #108299, #15522, #82355, .T. ) ;
#125261 = CARTESIAN_POINT ( 'NONE',  ( -69.48921356237309510, -27.52281430457103895, 5.000000000000000000 ) ) ;
#125263 = ORIENTED_EDGE ( 'NONE', *, *, #103825, .F. ) ;
#125264 = CARTESIAN_POINT ( 'NONE',  ( -35.99451991528749772, 28.92564299267963079, 4.000000000000000000 ) ) ;
#125265 = CARTESIAN_POINT ( 'NONE',  ( 57.48921356237308800, -27.52281430457095368, 5.000000000000000000 ) ) ;
#125266 = LINE ( 'NONE', #4858, #108673 ) ;
#125267 = VECTOR ( 'NONE', #114446, 1000.000000000000000 ) ;
#125268 = VECTOR ( 'NONE', #81532, 1000.000000000000000 ) ;
#125269 = VECTOR ( 'NONE', #63151, 1000.000000000000227 ) ;
#125270 = AXIS2_PLACEMENT_3D ( 'NONE', #70358, #25363, #126126 ) ;
#125271 = FACE_OUTER_BOUND ( 'NONE', #103241, .T. ) ;
#125272 = ORIENTED_EDGE ( 'NONE', *, *, #62698, .T. ) ;
#125273 = VECTOR ( 'NONE', #14586, 999.9999999999998863 ) ;
#125274 = DIRECTION ( 'NONE',  ( 1.000000000000000000, 0.000000000000000000, 0.000000000000000000 ) ) ;
#125275 = CARTESIAN_POINT ( 'NONE',  ( -18.88837638105230710, 9.759292476615614831, 17.35367589129216981 ) ) ;
#125276 = EDGE_LOOP ( 'NONE', ( #33865, #36353, #67868, #132673 ) ) ;
#125277 = CARTESIAN_POINT ( 'NONE',  ( -26.99999999999981526, 15.45873954670183181, -0.03131636524287845919 ) ) ;
#125278 = EDGE_LOOP ( 'NONE', ( #50241, #140705, #47945, #86514 ) ) ;
#125279 = EDGE_CURVE ( 'NONE', #43782, #49277, #95345, .T. ) ;
#125280 = EDGE_LOOP ( 'NONE', ( #108693, #31180, #45990, #143406 ) ) ;
#125281 = DIRECTION ( 'NONE',  ( -0.000000000000000000, -0.3543493200069152693, 0.9351131265310292928 ) ) ;
#125282 = VERTEX_POINT ( 'NONE', #92473 ) ;
#125283 = EDGE_LOOP ( 'NONE', ( #59467, #24323, #128375, #3621 ) ) ;
#125284 = AXIS2_PLACEMENT_3D ( 'NONE', #60711, #125934, #82426 ) ;
#125285 = PLANE ( 'NONE',  #81202 ) ;
#125286 = ORIENTED_EDGE ( 'NONE', *, *, #32704, .T. ) ;
#125287 = LINE ( 'NONE', #25976, #136889 ) ;
#125288 = DIRECTION ( 'NONE',  ( -0.7071067811865487940, 0.7071067811865463515, -0.000000000000000000 ) ) ;
#125289 = CARTESIAN_POINT ( 'NONE',  ( 114.9170968585647756, 3.054999999999998828, 5.291415217122922066 ) ) ;
#125290 = DIRECTION ( 'NONE',  ( -0.6830127018922180770, -0.6830127018922204085, -0.2588190451025213501 ) ) ;
#125291 = PRESENTATION_LAYER_ASSIGNMENT (  '', '', ( #83723 ) ) ;
#125292 = DIRECTION ( 'NONE',  ( 2.781805975412905274E-17, -0.3543493200069152138, 0.9351131265310292928 ) ) ;
#125293 = CARTESIAN_POINT ( 'NONE',  ( 66.18398860626901126, 28.73617430169833753, 5.000000000000000000 ) ) ;
#125294 = VECTOR ( 'NONE', #91652, 1000.000000000000000 ) ;
#125295 = CARTESIAN_POINT ( 'NONE',  ( 19.49999999999986855, -7.533600742197656963, 5.000000000000000000 ) ) ;
#125296 = DIRECTION ( 'NONE',  ( -0.000000000000000000, 0.000000000000000000, 1.000000000000000000 ) ) ;
#125297 = CARTESIAN_POINT ( 'NONE',  ( -42.48921356237308800, -27.52281430457085065, 5.000000000000000000 ) ) ;
#125298 = VECTOR ( 'NONE', #110426, 1000.000000000000000 ) ;
#125299 = FACE_OUTER_BOUND ( 'NONE', #76316, .T. ) ;
#125300 = ORIENTED_EDGE ( 'NONE', *, *, #79457, .T. ) ;
#125301 = AXIS2_PLACEMENT_3D ( 'NONE', #64265, #122187, #44702 ) ;
#125302 = CARTESIAN_POINT ( 'NONE',  ( -25.39999999999996305, 0.000000000000000000, 2.500000000000000000 ) ) ;
#125303 = CARTESIAN_POINT ( 'NONE',  ( 36.18398860626899705, 28.73617430169812437, 5.000000000000000000 ) ) ;
#125304 = EDGE_LOOP ( 'NONE', ( #59384, #139378, #142992, #21749 ) ) ;
#125305 = MECHANICAL_DESIGN_GEOMETRIC_PRESENTATION_REPRESENTATION (  '', ( #72049 ), #95173 ) ;
#125306 = ORIENTED_EDGE ( 'NONE', *, *, #17745, .T. ) ;
#125307 = LINE ( 'NONE', #114420, #47243 ) ;
#125308 = ORIENTED_EDGE ( 'NONE', *, *, #80877, .F. ) ;
#125309 = AXIS2_PLACEMENT_3D ( 'NONE', #4959, #38360, #59429 ) ;
#125310 = DIRECTION ( 'NONE',  ( 0.6830127018922181881, 0.6830127018922202975, -0.2588190451025214056 ) ) ;
#125311 = LINE ( 'NONE', #58685, #36257 ) ;
#125312 = AXIS2_PLACEMENT_3D ( 'NONE', #101622, #111045, #58903 ) ;
#125313 = DIRECTION ( 'NONE',  ( 0.000000000000000000, 1.000000000000000000, 0.000000000000000000 ) ) ;
#125314 = CARTESIAN_POINT ( 'NONE',  ( 24.18398860626899705, 28.73617430169804265, 5.000000000000000000 ) ) ;
#125315 = EDGE_CURVE ( 'NONE', #11548, #23039, #40292, .T. ) ;
#125316 = VERTEX_POINT ( 'NONE', #93917 ) ;
#125317 = EDGE_LOOP ( 'NONE', ( #56454, #54932, #80460, #46921 ) ) ;
#125318 = PLANE ( 'NONE',  #14424 ) ;
#125319 = EDGE_CURVE ( 'NONE', #138876, #141554, #125119, .T. ) ;
#125320 = COLOUR_RGB ( '', 0.66274510, 0.83137255, 0.94901961) ;
#125321 = CARTESIAN_POINT ( 'NONE',  ( 27.62956980810189123, -3.967499999999998028, -6.871911579029511330 ) ) ;
#125322 = ADVANCED_FACE ( 'NONE', ( #106193 ), #105494, .F. ) ;
#125323 = CARTESIAN_POINT ( 'NONE',  ( -33.32816939922329169, -3.740707523384244837, 4.000000000000000000 ) ) ;
#125324 = CARTESIAN_POINT ( 'NONE',  ( 11.75018676184482835, -8.548269360537348760, 4.146342017647454803 ) ) ;
#125325 = ORIENTED_EDGE ( 'NONE', *, *, #35334, .F. ) ;
#125326 = ORIENTED_EDGE ( 'NONE', *, *, #80188, .F. ) ;
#125327 = EDGE_CURVE ( 'NONE', #22361, #60511, #27956, .T. ) ;
#125328 = CONICAL_SURFACE ( 'NONE', #74434, 2.055000000000000604, 0.9599310885968764806 ) ;
#125329 = ORIENTED_EDGE ( 'NONE', *, *, #123370, .F. ) ;
#125330 = DIRECTION ( 'NONE',  ( 0.3543493200069162685, -0.000000000000000000, -0.9351131265310288487 ) ) ;
#125331 = DIRECTION ( 'NONE',  ( -1.000000000000000000, -1.224606353822377258E-16, -0.000000000000000000 ) ) ;
#125332 = CARTESIAN_POINT ( 'NONE',  ( -26.99451991528749417, 28.92564299267956685, 4.000000000000000000 ) ) ;
#125333 = CIRCLE ( 'NONE', #62851, 2.500000000000000444 ) ;
#125334 = ADVANCED_FACE ( 'NONE', ( #14923 ), #27224, .F. ) ;
#125335 = SURFACE_SIDE_STYLE ('',( #59389 ) ) ;
#125336 = ORIENTED_EDGE ( 'NONE', *, *, #12283, .F. ) ;
#125337 = CARTESIAN_POINT ( 'NONE',  ( 34.49999999999976552, -7.912538124160671593, 4.000000000000000000 ) ) ;
#125338 = LINE ( 'NONE', #70290, #126757 ) ;
#125339 = ADVANCED_FACE ( 'NONE', ( #83801 ), #126817, .F. ) ;
#125340 = LINE ( 'NONE', #49932, #125267 ) ;
#125341 = FACE_OUTER_BOUND ( 'NONE', #12445, .T. ) ;
#125342 = ORIENTED_EDGE ( 'NONE', *, *, #4033, .F. ) ;
#125343 = VECTOR ( 'NONE', #77910, 999.9999999999998863 ) ;
#125344 = CARTESIAN_POINT ( 'NONE',  ( -51.48921356237309510, -27.52281430457091460, 5.000000000000000000 ) ) ;
#125345 = ORIENTED_EDGE ( 'NONE', *, *, #126376, .T. ) ;
#125346 = EDGE_CURVE ( 'NONE', #16274, #5541, #5457, .T. ) ;
#125348 = ORIENTED_EDGE ( 'NONE', *, *, #10697, .F. ) ;
#125347 = FACE_OUTER_BOUND ( 'NONE', #77117, .T. ) ;
#125349 = ORIENTED_EDGE ( 'NONE', *, *, #12296, .T. ) ;
#125350 = EDGE_CURVE ( 'NONE', #80177, #21499, #116392, .T. ) ;
#125351 = FACE_OUTER_BOUND ( 'NONE', #97262, .T. ) ;
#125352 = FACE_OUTER_BOUND ( 'NONE', #64778, .T. ) ;
#125354 = ORIENTED_EDGE ( 'NONE', *, *, #73037, .F. ) ;
#125353 = VECTOR ( 'NONE', #71371, 1000.000000000000000 ) ;
#125355 = DIRECTION ( 'NONE',  ( -0.7071067811865486830, -0.7071067811865464625, 0.000000000000000000 ) ) ;
#125356 = ORIENTED_EDGE ( 'NONE', *, *, #13336, .F. ) ;
#125357 = ADVANCED_FACE ( 'NONE', ( #17085 ), #72937, .F. ) ;
#125358 = CARTESIAN_POINT ( 'NONE',  ( -13.49999999999988631, 22.08746187583901843, 4.000000000000000000 ) ) ;
#125359 = PLANE ( 'NONE',  #64811 ) ;
#125360 = CARTESIAN_POINT ( 'NONE',  ( 28.93293019189811943, 1.637169565754156730, 6.110000000000001208 ) ) ;
#125361 = LINE ( 'NONE', #126083, #43957 ) ;
#125362 = LINE ( 'NONE', #136942, #15994 ) ;
#125363 = CARTESIAN_POINT ( 'NONE',  ( -17.99999999999988276, -13.39766691384885711, -10.96608748226462282 ) ) ;
#125364 = PLANE ( 'NONE',  #88879 ) ;
#125365 = CARTESIAN_POINT ( 'NONE',  ( 23.21837311707488638, 21.74787736706806029, 4.999607392498050196 ) ) ;
#125366 = CARTESIAN_POINT ( 'NONE',  ( 31.91623647476855297, -7.934999999999990727, 4.858786175617117713E-16 ) ) ;
#125367 = CARTESIAN_POINT ( 'NONE',  ( 2.457903141435219485, 6.871911579029515771, 3.967499999999989146 ) ) ;
#125368 = DIRECTION ( 'NONE',  ( -0.7071067811865486830, -0.7071067811865464625, -0.000000000000000000 ) ) ;
#125369 = CIRCLE ( 'NONE', #62881, 3.999999999999996447 ) ;
#125370 = DIRECTION ( 'NONE',  ( -1.000000000000000000, -1.224606353822377258E-16, -0.000000000000000000 ) ) ;
#125371 = DIRECTION ( 'NONE',  ( -0.3543493200069162685, -0.000000000000000000, -0.9351131265310288487 ) ) ;
#125372 = EDGE_LOOP ( 'NONE', ( #37004, #143490, #77387, #69594 ) ) ;
#125373 =( BOUNDED_CURVE ( )  B_SPLINE_CURVE ( 3, ( #24425, #12110, #79581, #58548 ),
 .UNSPECIFIED., .F., .F. ) 
 B_SPLINE_CURVE_WITH_KNOTS ( ( 4, 4 ),
 ( 1.901594255663627608, 1.933014472006554740 ),
 .UNSPECIFIED. ) 
 CURVE ( )  GEOMETRIC_REPRESENTATION_ITEM ( )  RATIONAL_B_SPLINE_CURVE ( ( 1.000000000000000000, 0.9999177325257868620, 0.9999177325257868620, 1.000000000000000000 ) ) 
 REPRESENTATION_ITEM ( '' )  );
#125374 = ORIENTED_EDGE ( 'NONE', *, *, #138942, .F. ) ;
#125375 = CONICAL_SURFACE ( 'NONE', #81420, 2.055000000000001048, 0.9599310885968758145 ) ;
#125376 = CARTESIAN_POINT ( 'NONE',  ( 90.97916666666667140, -7.950000000000001066, 2.130196079827424427 ) ) ;
#125377 = VECTOR ( 'NONE', #61981, 1000.000000000000227 ) ;
#125378 = ORIENTED_EDGE ( 'NONE', *, *, #76982, .T. ) ;
#125379 = ORIENTED_EDGE ( 'NONE', *, *, #40579, .F. ) ;
#125380 = ADVANCED_FACE ( 'NONE', ( #117084 ), #6159, .F. ) ;
#125381 = CARTESIAN_POINT ( 'NONE',  ( 11.29289321881337393, 20.25929247661551713, 5.000000000000000000 ) ) ;
#125382 = CARTESIAN_POINT ( 'NONE',  ( -34.92500000000001137, 22.06445279868695408, 5.060837336147055332 ) ) ;
#125383 = AXIS2_PLACEMENT_3D ( 'NONE', #30298, #52747, #141186 ) ;
#125384 = AXIS2_PLACEMENT_3D ( 'NONE', #7111, #83299, #128929 ) ;
#125385 = VECTOR ( 'NONE', #57811, 999.9999999999998863 ) ;
#125386 = VECTOR ( 'NONE', #86739, 1000.000000000000000 ) ;
#125387 = CARTESIAN_POINT ( 'NONE',  ( 11.74803111135162226, 8.547913778412416619, -4.147067623587493479 ) ) ;
#125388 = ORIENTED_EDGE ( 'NONE', *, *, #46982, .T. ) ;
#125389 = CARTESIAN_POINT ( 'NONE',  ( -6.489213562373093325, -27.52281430457059841, 5.000000000000000000 ) ) ;
#125390 = VECTOR ( 'NONE', #139961, 999.9999999999998863 ) ;
#125391 = LINE ( 'NONE', #80470, #9381 ) ;
#125392 = CARTESIAN_POINT ( 'NONE',  ( -13.49999999999990408, -14.56887692260766087, 4.000000000000000000 ) ) ;
#125393 = CARTESIAN_POINT ( 'NONE',  ( 125.5279775329496630, -3.465570510557019812, -7.141980925050981810 ) ) ;
#125394 = CARTESIAN_POINT ( 'NONE',  ( 5.218373117075015166, 21.74787736706806029, 4.999607392498049308 ) ) ;
#125395 = CARTESIAN_POINT ( 'NONE',  ( 9.489213562373095101, -27.52281430457062328, 5.000000000000000000 ) ) ;
#125396 = VECTOR ( 'NONE', #50340, 999.9999999999998863 ) ;
#125397 = CARTESIAN_POINT ( 'NONE',  ( 13.49999999999990763, -17.91344420646041158, 1.358650452708495493 ) ) ;
#125398 = DIRECTION ( 'NONE',  ( 0.3543493200069162685, -0.000000000000000000, -0.9351131265310288487 ) ) ;
#125399 = CARTESIAN_POINT ( 'NONE',  ( 53.99451991528749062, 28.92564299267975869, 4.000000000000000000 ) ) ;
#125400 = DIRECTION ( 'NONE',  ( 0.000000000000000000, 0.000000000000000000, 1.000000000000000000 ) ) ;
#125401 = CARTESIAN_POINT ( 'NONE',  ( -4.499999999999960920, 12.05218569542904739, 5.000000000000000000 ) ) ;
#125402 = ORIENTED_EDGE ( 'NONE', *, *, #48969, .T. ) ;
#125403 = VERTEX_POINT ( 'NONE', #70775 ) ;
#125404 = CARTESIAN_POINT ( 'NONE',  ( 109.2295968585647614, -6.110000000000000320, -1.637169565754161393 ) ) ;
#125405 = VERTEX_POINT ( 'NONE', #114921 ) ;
#125406 = AXIS2_PLACEMENT_3D ( 'NONE', #98862, #22705, #77849 ) ;
#125407 = EDGE_CURVE ( 'NONE', #92088, #122112, #124521, .T. ) ;
#125408 = CARTESIAN_POINT ( 'NONE',  ( 34.92499999999998295, 22.22500000000000142, 4.000000000000000000 ) ) ;
#125409 = CARTESIAN_POINT ( 'NONE',  ( 31.49999999999979039, -20.94781430457059912, 5.000000000000000000 ) ) ;
#125410 = ORIENTED_EDGE ( 'NONE', *, *, #136456, .F. ) ;
#125411 = DIRECTION ( 'NONE',  ( 0.6830127018922180770, -0.6830127018922202975, -0.2588190451025213501 ) ) ;
#125412 = DIRECTION ( 'NONE',  ( -0.6830127018922180770, -0.6830127018922204085, -0.2588190451025213501 ) ) ;
#125413 = VECTOR ( 'NONE', #97041, 1000.000000000000000 ) ;
#125414 = VECTOR ( 'NONE', #12002, 1000.000000000000000 ) ;
#125415 = CARTESIAN_POINT ( 'NONE',  ( 104.4745968585647802, 1.637169565754164058, -6.109999999999996767 ) ) ;
#125416 = EDGE_LOOP ( 'NONE', ( #38832, #89132, #67129 ) ) ;
#125417 = ADVANCED_FACE ( 'NONE', ( #74334 ), #96050, .F. ) ;
#125418 = VECTOR ( 'NONE', #124760, 1000.000000000000000 ) ;
#125419 = ORIENTED_EDGE ( 'NONE', *, *, #15457, .F. ) ;
#125420 = CARTESIAN_POINT ( 'NONE',  ( 8.229957205422008926, 21.73644205237998150, 5.000000000000000888 ) ) ;
#125421 = CARTESIAN_POINT ( 'NONE',  ( 5.691592354503320905, 9.902892378096218942E-16, 0.000000000000000000 ) ) ;
#125422 = PRESENTATION_LAYER_ASSIGNMENT (  '', '', ( #106868 ) ) ;
#125423 = PLANE ( 'NONE',  #135765 ) ;
#125424 = ORIENTED_EDGE ( 'NONE', *, *, #109914, .T. ) ;
#125425 = VERTEX_POINT ( 'NONE', #40980 ) ;
#125426 = EDGE_CURVE ( 'NONE', #95280, #122630, #84499, .T. ) ;
#125427 = ORIENTED_EDGE ( 'NONE', *, *, #132683, .F. ) ;
#125428 = DIRECTION ( 'NONE',  ( -0.000000000000000000, -0.3543493200069152693, 0.9351131265310292928 ) ) ;
#125429 = VECTOR ( 'NONE', #14173, 999.9999999999998863 ) ;
#125430 = SURFACE_STYLE_FILL_AREA ( #136285 ) ;
#125431 = LINE ( 'NONE', #14515, #43136 ) ;
#125432 = ORIENTED_EDGE ( 'NONE', *, *, #98797, .T. ) ;
#125433 = ORIENTED_EDGE ( 'NONE', *, *, #142457, .T. ) ;
#125434 = DIRECTION ( 'NONE',  ( 0.000000000000000000, 1.000000000000000000, 0.000000000000000000 ) ) ;
#125435 = VERTEX_POINT ( 'NONE', #53259 ) ;
#125436 = ORIENTED_EDGE ( 'NONE', *, *, #81017, .F. ) ;
#125437 = AXIS2_PLACEMENT_3D ( 'NONE', #105589, #117873, #60735 ) ;
#125438 = AXIS2_PLACEMENT_3D ( 'NONE', #60298, #39980, #15299 ) ;
#125439 = EDGE_CURVE ( 'NONE', #39694, #4634, #140289, .T. ) ;
#125440 = DIRECTION ( 'NONE',  ( -0.000000000000000000, -0.3543493200069152693, 0.9351131265310292928 ) ) ;
#125441 = DIRECTION ( 'NONE',  ( 0.6830127018922180770, -0.6830127018922204085, -0.2588190451025213501 ) ) ;
#125442 = ADVANCED_FACE ( 'NONE', ( #10465 ), #129393, .F. ) ;
#125443 = ORIENTED_EDGE ( 'NONE', *, *, #58747, .T. ) ;
#125444 = DIRECTION ( 'NONE',  ( -0.3543493200069163240, 0.000000000000000000, -0.9351131265310288487 ) ) ;
#125445 = CARTESIAN_POINT ( 'NONE',  ( -23.22995720542189346, 21.73644205237998150, 5.000000000000000888 ) ) ;
#125446 = AXIS2_PLACEMENT_3D ( 'NONE', #140141, #53088, #130701 ) ;
#125447 = DIRECTION ( 'NONE',  ( -0.000000000000000000, -0.3543493200069152693, 0.9351131265310292928 ) ) ;
#125448 = DIRECTION ( 'NONE',  ( 0.6830127018922181881, 0.6830127018922202975, -0.2588190451025214056 ) ) ;
#125449 = CARTESIAN_POINT ( 'NONE',  ( -34.92500000000001137, 14.19452376399130600, 8.043047640789321662 ) ) ;
#125450 = FACE_BOUND ( 'NONE', #119853, .T. ) ;
#125451 = ORIENTED_EDGE ( 'NONE', *, *, #137906, .T. ) ;
#125452 = FACE_OUTER_BOUND ( 'NONE', #80371, .T. ) ;
#125453 = DIRECTION ( 'NONE',  ( -0.3543493200069162685, -0.000000000000000000, -0.9351131265310288487 ) ) ;
#125454 = CARTESIAN_POINT ( 'NONE',  ( 26.99999999999980105, 8.587461875839165870, 4.000000000000000000 ) ) ;
#125455 = EDGE_CURVE ( 'NONE', #87892, #34731, #73609, .T. ) ;
#125456 = EDGE_LOOP ( 'NONE', ( #119983, #58493, #118817, #68965 ) ) ;
#125457 = CARTESIAN_POINT ( 'NONE',  ( -27.88837638105224315, 9.759292476615614831, 17.35367589129219112 ) ) ;
#125458 = ORIENTED_EDGE ( 'NONE', *, *, #38651, .F. ) ;
#125459 = ORIENTED_EDGE ( 'NONE', *, *, #95599, .F. ) ;
#125460 = AXIS2_PLACEMENT_3D ( 'NONE', #91331, #59426, #15145 ) ;
#125461 = ORIENTED_EDGE ( 'NONE', *, *, #117887, .F. ) ;
#125462 = CARTESIAN_POINT ( 'NONE',  ( 37.97459685856477307, 1.637169565754164280, -6.109999999999996767 ) ) ;
#125463 = VERTEX_POINT ( 'NONE', #119923 ) ;
#125464 = CARTESIAN_POINT ( 'NONE',  ( 11.99999999999992006, 7.007997736742456851, -8.085015511992084569 ) ) ;
#125465 = FACE_OUTER_BOUND ( 'NONE', #74244, .T. ) ;
#125466 = LINE ( 'NONE', #67537, #135314 ) ;
#125467 = VERTEX_POINT ( 'NONE', #20629 ) ;
#125468 = DIRECTION ( 'NONE',  ( 0.000000000000000000, 0.000000000000000000, 1.000000000000000000 ) ) ;
#125469 = CONICAL_SURFACE ( 'NONE', #67657, 2.500000000000000888, 0.9599310885968822538 ) ;
#125470 = VECTOR ( 'NONE', #46549, 1000.000000000000227 ) ;
#125471 = EDGE_CURVE ( 'NONE', #71989, #56823, #31945, .T. ) ;
#125472 = DIRECTION ( 'NONE',  ( -0.7071067811865486830, -0.7071067811865464625, 0.000000000000000000 ) ) ;
#125473 = CIRCLE ( 'NONE', #62993, 2.500000000000000444 ) ;
#125474 = AXIS2_PLACEMENT_3D ( 'NONE', #12558, #33639, #100306 ) ;
#125475 = CARTESIAN_POINT ( 'NONE',  ( 0.1161069444170877152, -0.3999999999999998002, -2.220360628129161906 ) ) ;
#125476 = PLANE ( 'NONE',  #62520 ) ;
#125477 = SURFACE_STYLE_USAGE ( .BOTH. , #134949 ) ;
#125478 = DIRECTION ( 'NONE',  ( -0.7071067811865487940, 0.7071067811865463515, -0.000000000000000000 ) ) ;
#125479 = ORIENTED_EDGE ( 'NONE', *, *, #99244, .T. ) ;
#125480 = ORIENTED_EDGE ( 'NONE', *, *, #118996, .T. ) ;
#125481 = VECTOR ( 'NONE', #98972, 1000.000000000000000 ) ;
#125482 = ORIENTED_EDGE ( 'NONE', *, *, #421, .T. ) ;
#125483 = VECTOR ( 'NONE', #136049, 999.9999999999998863 ) ;
#125484 = ORIENTED_EDGE ( 'NONE', *, *, #81284, .F. ) ;
#125485 = SURFACE_SIDE_STYLE ('',( #114578 ) ) ;
#125486 = ORIENTED_EDGE ( 'NONE', *, *, #115627, .F. ) ;
#125487 = ORIENTED_EDGE ( 'NONE', *, *, #79927, .T. ) ;
#125488 = DIRECTION ( 'NONE',  ( 0.000000000000000000, -1.000000000000000000, 0.000000000000000000 ) ) ;
#125489 = DIRECTION ( 'NONE',  ( -0.3543493200069163240, -0.000000000000000000, 0.9351131265310288487 ) ) ;
#125490 = EDGE_LOOP ( 'NONE', ( #85171, #115369, #39284 ) ) ;
#125491 = FACE_OUTER_BOUND ( 'NONE', #57810, .T. ) ;
#125492 = ORIENTED_EDGE ( 'NONE', *, *, #138788, .T. ) ;
#125493 = CARTESIAN_POINT ( 'NONE',  ( -15.71230993966017309, -21.73547319004781642, 4.999917730833664642 ) ) ;
#125494 = CARTESIAN_POINT ( 'NONE',  ( 0.000000000000000000, 0.000000000000000000, 5.000000000000000000 ) ) ;
#125495 = ADVANCED_FACE ( 'NONE', ( #107645 ), #52555, .F. ) ;
#125496 = CARTESIAN_POINT ( 'NONE',  ( 5.025403141435220711, 2.126176841940962348, 7.934999999999989839 ) ) ;
#125497 = ORIENTED_EDGE ( 'NONE', *, *, #83237, .F. ) ;
#125499 = CARTESIAN_POINT ( 'NONE',  ( 25.49999999999982236, 6.431123077392117082, 4.000000000000000000 ) ) ;
#125498 = CARTESIAN_POINT ( 'NONE',  ( 97.76626352523143737, 4.472830434245839371, -4.472830434245839371 ) ) ;
#125500 = EDGE_CURVE ( 'NONE', #128811, #120024, #54724, .T. ) ;
#125501 = PLANE ( 'NONE',  #83708 ) ;
#125502 = CARTESIAN_POINT ( 'NONE',  ( 12.19999999999999574, -40.43000000000000682, 19.06900128115122683 ) ) ;
#125503 = VERTEX_POINT ( 'NONE', #96737 ) ;
#125504 = ORIENTED_EDGE ( 'NONE', *, *, #73652, .T. ) ;
#125505 = PRESENTATION_STYLE_ASSIGNMENT (( #14591 ) ) ;
#125506 = ORIENTED_EDGE ( 'NONE', *, *, #24180, .F. ) ;
#125507 = SURFACE_STYLE_FILL_AREA ( #60265 ) ;
#125508 = DIRECTION ( 'NONE',  ( 0.7071067811865487940, 0.7071067811865463515, 0.000000000000000000 ) ) ;
#125509 = DIRECTION ( 'NONE',  ( -0.3543493200069162685, -0.000000000000000000, -0.9351131265310288487 ) ) ;
#125510 = CARTESIAN_POINT ( 'NONE',  ( 18.70710678118641468, -15.74070752338412049, 5.000000000000000000 ) ) ;
#125511 = EDGE_CURVE ( 'NONE', #87888, #32541, #142444, .T. ) ;
#125512 = EDGE_CURVE ( 'NONE', #114222, #99443, #32243, .T. ) ;
#125513 = LINE ( 'NONE', #5825, #84247 ) ;
#125514 = ORIENTED_EDGE ( 'NONE', *, *, #25805, .F. ) ;
#125515 = VECTOR ( 'NONE', #7581, 1000.000000000000000 ) ;
#125516 = CARTESIAN_POINT ( 'NONE',  ( 12.29974487139158512, -27.71228299555214747, 4.000000000000000000 ) ) ;
#125517 = VECTOR ( 'NONE', #32734, 1000.000000000000000 ) ;
#125518 = VECTOR ( 'NONE', #20257, 1000.000000000000000 ) ;
#125519 = LINE ( 'NONE', #15275, #88132 ) ;
#125520 = LINE ( 'NONE', #105862, #11784 ) ;
#125521 = ORIENTED_EDGE ( 'NONE', *, *, #87812, .T. ) ;
#125522 = DIRECTION ( 'NONE',  ( -0.7071067811865486830, 0.7071067811865464625, 0.000000000000000000 ) ) ;
#125523 = VECTOR ( 'NONE', #70521, 999.9999999999998863 ) ;
#125524 = DIRECTION ( 'NONE',  ( -0.000000000000000000, 0.3543493200069153248, 0.9351131265310292928 ) ) ;
#125525 = EDGE_LOOP ( 'NONE', ( #120783, #126312, #77631, #133297, #71906, #9949 ) ) ;
#125526 = EDGE_CURVE ( 'NONE', #138987, #24260, #85125, .T. ) ;
#125528 = ORIENTED_EDGE ( 'NONE', *, *, #99659, .F. ) ;
#125527 = CARTESIAN_POINT ( 'NONE',  ( -27.18398860626900060, 28.73617430169806042, 5.000000000000000000 ) ) ;
#125529 = ADVANCED_FACE ( 'NONE', ( #65630 ), #117777, .F. ) ;
#125530 = EDGE_LOOP ( 'NONE', ( #129203, #27768, #28014, #40597 ) ) ;
#125531 = LINE ( 'NONE', #15286, #42453 ) ;
#125532 = DIRECTION ( 'NONE',  ( -0.000000000000000000, 0.000000000000000000, 1.000000000000000000 ) ) ;
#125533 = VECTOR ( 'NONE', #35633, 1000.000000000000000 ) ;
#125534 = EDGE_LOOP ( 'NONE', ( #94798, #114166, #99540, #116379 ) ) ;
#125535 = CARTESIAN_POINT ( 'NONE',  ( 112.2708333333333144, -7.949999999999998401, -2.130196079827426203 ) ) ;
#125536 = EDGE_CURVE ( 'NONE', #62317, #85316, #7607, .T. ) ;
#125537 = FACE_OUTER_BOUND ( 'NONE', #27807, .T. ) ;
#125538 = PLANE ( 'NONE',  #62288 ) ;
#125539 =( BOUNDED_CURVE ( )  B_SPLINE_CURVE ( 3, ( #128824, #70909, #61477, #116528 ),
 .UNSPECIFIED., .F., .T. ) 
 B_SPLINE_CURVE_WITH_KNOTS ( ( 4, 4 ),
 ( 2.779374508378133601, 4.199602562396796301 ),
 .UNSPECIFIED. ) 
 CURVE ( )  GEOMETRIC_REPRESENTATION_ITEM ( )  RATIONAL_B_SPLINE_CURVE ( ( 1.000000000000000000, 0.8388583629366717087, 0.8388583629366717087, 1.000000000000000000 ) ) 
 REPRESENTATION_ITEM ( '' )  );
#125540 = ORIENTED_EDGE ( 'NONE', *, *, #138411, .F. ) ;
#125541 = DIRECTION ( 'NONE',  ( 0.6830127018922180770, -0.6830127018922204085, -0.2588190451025213501 ) ) ;
#125542 = CARTESIAN_POINT ( 'NONE',  ( 4.288407645496676857, 9.139736423841732040E-16, 0.000000000000000000 ) ) ;
#125543 = LINE ( 'NONE', #72627, #9599 ) ;
#125544 = VECTOR ( 'NONE', #45394, 1000.000000000000000 ) ;
#125545 = PLANE ( 'NONE',  #40151 ) ;
#125546 = EDGE_CURVE ( 'NONE', #81589, #33976, #58333, .T. ) ;
#125547 = CARTESIAN_POINT ( 'NONE',  ( -0.3281693992235289459, -3.740707523384244837, 4.000000000000000000 ) ) ;
#125548 = AXIS2_PLACEMENT_3D ( 'NONE', #112348, #13004, #90598 ) ;
#125549 = CARTESIAN_POINT ( 'NONE',  ( -4.499999999999970690, 22.01701374228155217, 2.453858888625641832 ) ) ;
#125550 = CARTESIAN_POINT ( 'NONE',  ( 26.99451991528749417, 28.92564299267956685, 4.000000000000000000 ) ) ;
#125551 = CARTESIAN_POINT ( 'NONE',  ( 7.499999999999951150, 3.653845994658396545, -4.504631822206387248 ) ) ;
#125552 = ORIENTED_EDGE ( 'NONE', *, *, #33403, .T. ) ;
#125553 = ORIENTED_EDGE ( 'NONE', *, *, #5562, .T. ) ;
#125554 = VERTEX_POINT ( 'NONE', #90177 ) ;
#125555 = CARTESIAN_POINT ( 'NONE',  ( 123.0625000000000142, -5.819803920172572198, -5.819803920172573086 ) ) ;
#125556 = ORIENTED_EDGE ( 'NONE', *, *, #100344, .T. ) ;
#125557 = EDGE_LOOP ( 'NONE', ( #81167, #86677, #72573, #101226 ) ) ;
#125558 = ORIENTED_EDGE ( 'NONE', *, *, #21298, .T. ) ;
#125559 = ADVANCED_FACE ( 'NONE', ( #112653 ), #111201, .T. ) ;
#125560 = VECTOR ( 'NONE', #82726, 1000.000000000000000 ) ;
#125561 = PRESENTATION_STYLE_ASSIGNMENT (( #37845 ) ) ;
#125562 = DIRECTION ( 'NONE',  ( -1.000000000000000000, -0.000000000000000000, -0.000000000000000000 ) ) ;
#125563 = ORIENTED_EDGE ( 'NONE', *, *, #118683, .F. ) ;
#125564 = CARTESIAN_POINT ( 'NONE',  ( 12.19999999999999574, -59.76999999999998892, -39.50000000000000000 ) ) ;
#125565 = LINE ( 'NONE', #123444, #113417 ) ;
#125566 = CARTESIAN_POINT ( 'NONE',  ( -26.39513766812463658, 21.75929247661549226, 21.32995629748192457 ) ) ;
#125567 = CARTESIAN_POINT ( 'NONE',  ( 111.5629301918981184, 1.637169565754157174, 6.110000000000002984 ) ) ;
#125568 = ORIENTED_EDGE ( 'NONE', *, *, #103649, .T. ) ;
#125569 = DIRECTION ( 'NONE',  ( 0.7071067811865487940, -0.7071067811865463515, 0.000000000000000000 ) ) ;
#125570 = PLANE ( 'NONE',  #130255 ) ;
#125571 = ADVANCED_FACE ( 'NONE', ( #32993 ), #2433, .F. ) ;
#125573 = AXIS2_PLACEMENT_3D ( 'NONE', #48721, #92923, #18182 ) ;
#125572 = CARTESIAN_POINT ( 'NONE',  ( 0.000000000000000000, 0.000000000000000000, 5.000000000000000000 ) ) ;
#125574 = CARTESIAN_POINT ( 'NONE',  ( 0.3964375652403131500, 6.305472576662640272, -4.436123002877206289 ) ) ;
#125575 = DIRECTION ( 'NONE',  ( 0.7071067811865487940, -0.7071067811865463515, 0.000000000000000000 ) ) ;
#125576 =( BOUNDED_CURVE ( )  B_SPLINE_CURVE ( 2, ( #99621, #13318, #35855, #100368, #80071, #124247, #24921, #1018, #47456, #91622, #34388, #78608, #11159 ),
 .UNSPECIFIED., .F., .F. ) 
 B_SPLINE_CURVE_WITH_KNOTS ( ( 3, 2, 2, 2, 2, 2, 3 ),
 ( 0.9333333333333333481, 0.9361111111111111160, 0.9388888888888888840, 0.9416666666666666519, 0.9444444444444444198, 0.9472222222222221877, 0.9499999999999999556 ),
 .UNSPECIFIED. ) 
 CURVE ( )  GEOMETRIC_REPRESENTATION_ITEM ( )  RATIONAL_B_SPLINE_CURVE ( ( 1.000000000000000000, 0.9659258262890683122, 1.000000000000000000, 0.9659258262890683122, 1.000000000000000000, 0.9659258262890683122, 1.000000000000000000, 0.9659258262890683122, 1.000000000000000000, 0.9659258262890683122, 1.000000000000000000, 0.9659258262890683122, 1.000000000000000000 ) ) 
 REPRESENTATION_ITEM ( '' )  );
#125577 = LINE ( 'NONE', #124128, #100106 ) ;
#125578 = DIRECTION ( 'NONE',  ( 0.000000000000000000, -1.000000000000000000, 0.000000000000000000 ) ) ;
#125579 = CARTESIAN_POINT ( 'NONE',  ( 35.22502705046287730, 5.819803920172573086, -5.819803920172572198 ) ) ;
#125580 = ADVANCED_FACE ( 'NONE', ( #11155 ), #46746, .F. ) ;
#125581 = DIRECTION ( 'NONE',  ( -1.000000000000000000, -1.224606353822377258E-16, -0.000000000000000000 ) ) ;
#125582 = CARTESIAN_POINT ( 'NONE',  ( -33.29974487139158867, -27.71228299555229313, 4.000000000000000000 ) ) ;
#125583 = VERTEX_POINT ( 'NONE', #78603 ) ;
#125584 = ORIENTED_EDGE ( 'NONE', *, *, #11504, .T. ) ;
#125585 = CARTESIAN_POINT ( 'NONE',  ( 39.49999999999999289, 0.000000000000000000, -7.950000000000000178 ) ) ;
#125586 = ORIENTED_EDGE ( 'NONE', *, *, #118629, .F. ) ;
#125587 = VERTEX_POINT ( 'NONE', #22747 ) ;
#125588 = CARTESIAN_POINT ( 'NONE',  ( -0.1839886062690032631, 28.73617430169787568, 5.000000000000000000 ) ) ;
#125589 = DIRECTION ( 'NONE',  ( -0.7071067811865487940, 0.7071067811865463515, 0.000000000000000000 ) ) ;
#125590 = ORIENTED_EDGE ( 'NONE', *, *, #116340, .F. ) ;
#125591 = VECTOR ( 'NONE', #115856, 1000.000000000000000 ) ;
#125592 = VECTOR ( 'NONE', #74342, 1000.000000000000000 ) ;
#125593 = VECTOR ( 'NONE', #139885, 999.9999999999998863 ) ;
#125594 = FACE_OUTER_BOUND ( 'NONE', #90150, .T. ) ;
#125595 = CARTESIAN_POINT ( 'NONE',  ( -18.48921356237309510, -27.52281430457068367, 5.000000000000000000 ) ) ;
#125596 = DIRECTION ( 'NONE',  ( -0.000000000000000000, 0.000000000000000000, 1.000000000000000000 ) ) ;
#125597 = MECHANICAL_DESIGN_GEOMETRIC_PRESENTATION_REPRESENTATION (  '', ( #113985 ), #70045 ) ;
#125598 = CARTESIAN_POINT ( 'NONE',  ( 31.79209685856476852, -5.291415217122921177, 3.054999999999999272 ) ) ;
#125599 = ORIENTED_EDGE ( 'NONE', *, *, #142025, .F. ) ;
#125600 = EDGE_CURVE ( 'NONE', #106721, #56418, #100362, .T. ) ;
#125601 = LINE ( 'NONE', #137183, #126632 ) ;
#125602 = EDGE_LOOP ( 'NONE', ( #106799, #76925, #28056, #43866 ) ) ;
#125603 = STYLED_ITEM ( 'NONE', ( #16051 ), #130635 ) ;
#125604 = VECTOR ( 'NONE', #88661, 1000.000000000000227 ) ;
#125605 = CARTESIAN_POINT ( 'NONE',  ( -12.29974487139158512, -27.71228299555214747, 4.000000000000000000 ) ) ;
#125606 = DIRECTION ( 'NONE',  ( -0.7071067811865487940, 0.7071067811865463515, -0.000000000000000000 ) ) ;
#125607 = DIRECTION ( 'NONE',  ( -0.7071067811865486830, -0.7071067811865464625, -0.000000000000000000 ) ) ;
#125608 = EDGE_LOOP ( 'NONE', ( #59751, #21156, #28647, #94356, #141007 ) ) ;
#125609 = ADVANCED_FACE ( 'NONE', ( #68474 ), #88051, .T. ) ;
#125610 = ORIENTED_EDGE ( 'NONE', *, *, #52701, .F. ) ;
#125611 = FACE_OUTER_BOUND ( 'NONE', #132621, .T. ) ;
#125612 = DIRECTION ( 'NONE',  ( -0.000000000000000000, 0.000000000000000000, 1.000000000000000000 ) ) ;
#125613 = DIRECTION ( 'NONE',  ( 0.6830127018922181881, 0.6830127018922202975, -0.2588190451025214056 ) ) ;
#125614 = CARTESIAN_POINT ( 'NONE',  ( -11.99999999999991651, -11.35517001088073563, -1.126524801160135869 ) ) ;
#125615 = CARTESIAN_POINT ( 'NONE',  ( 44.82876352523145158, 0.000000000000000000, -6.109999999999998543 ) ) ;
#125616 = CARTESIAN_POINT ( 'NONE',  ( 124.5208333333333286, 7.949999999999998401, 2.130196079827431532 ) ) ;
#125617 = CARTESIAN_POINT ( 'NONE',  ( -8.510786437626906675, -27.52281430457049183, 5.000000000000000000 ) ) ;
#125618 = ORIENTED_EDGE ( 'NONE', *, *, #100434, .T. ) ;
#125619 = ORIENTED_EDGE ( 'NONE', *, *, #46354, .F. ) ;
#125620 = FACE_OUTER_BOUND ( 'NONE', #23975, .T. ) ;
#125621 = ORIENTED_EDGE ( 'NONE', *, *, #99812, .F. ) ;
#125622 = VECTOR ( 'NONE', #103000, 1000.000000000000000 ) ;
#125623 = CARTESIAN_POINT ( 'NONE',  ( 30.48921356237309510, -27.52281430457076894, 5.000000000000000000 ) ) ;
#125624 = PRODUCT_DEFINITION_CONTEXT ( 'detailed design', #112406, 'design' ) ;
#125625 = ADVANCED_FACE ( 'NONE', ( #110485 ), #122815, .F. ) ;
#125626 = ORIENTED_EDGE ( 'NONE', *, *, #55880, .F. ) ;
#125627 = AXIS2_PLACEMENT_3D ( 'NONE', #74517, #62207, #19391 ) ;
#125628 = DIRECTION ( 'NONE',  ( 1.000000000000000000, 0.000000000000000000, 0.000000000000000000 ) ) ;
#125629 = AXIS2_PLACEMENT_3D ( 'NONE', #133949, #59110, #44851 ) ;
#125630 = DIRECTION ( 'NONE',  ( -0.000000000000000000, -0.000000000000000000, 1.000000000000000000 ) ) ;
#125631 = ADVANCED_FACE ( 'NONE', ( #66314 ), #48191, .T. ) ;
#125632 = FACE_BOUND ( 'NONE', #67162, .T. ) ;
#125633 = DIRECTION ( 'NONE',  ( 0.000000000000000000, 0.000000000000000000, 1.000000000000000000 ) ) ;
#125634 = FILL_AREA_STYLE_COLOUR ( '', #109211 ) ;
#125635 = EDGE_CURVE ( 'NONE', #10662, #61952, #77893, .T. ) ;
#125636 = CARTESIAN_POINT ( 'NONE',  ( -13.31312592467349454, 1.515602562757560223, 4.636692559446319528 ) ) ;
#125638 = ORIENTED_EDGE ( 'NONE', *, *, #19635, .T. ) ;
#125637 = LINE ( 'NONE', #82846, #131502 ) ;
#125639 = CARTESIAN_POINT ( 'NONE',  ( -24.85181644961839709, 17.25929247661554200, 8.802941693769145814 ) ) ;
#125640 = VERTEX_POINT ( 'NONE', #89469 ) ;
#125641 = VERTEX_POINT ( 'NONE', #67769 ) ;
#125642 = CARTESIAN_POINT ( 'NONE',  ( 64.80793019189812298, -6.109999999999998543, 1.637169565754158507 ) ) ;
#125643 = ADVANCED_FACE ( 'NONE', ( #12615 ), #136241, .F. ) ;
#125644 = EDGE_LOOP ( 'NONE', ( #97462, #66995 ) ) ;
#125645 = EDGE_CURVE ( 'NONE', #95099, #142404, #118886, .T. ) ;
#125646 = DIRECTION ( 'NONE',  ( -0.3543493200069162685, -0.000000000000000000, -0.9351131265310288487 ) ) ;
#125647 = CARTESIAN_POINT ( 'NONE',  ( 56.09683561313696032, -51.20434817233908831, -36.87500513592858198 ) ) ;
#125648 = CIRCLE ( 'NONE', #141803, 2.500000000000000444 ) ;
#125649 = VERTEX_POINT ( 'NONE', #62393 ) ;
#125650 = CARTESIAN_POINT ( 'NONE',  ( -18.48921356237309510, -27.52281430457068367, 5.000000000000000000 ) ) ;
#125651 = VECTOR ( 'NONE', #102008, 999.9999999999998863 ) ;
#125652 = EDGE_CURVE ( 'NONE', #22237, #65842, #103195, .T. ) ;
#125653 = CARTESIAN_POINT ( 'NONE',  ( -4.773258392821638552, -11.24070752338417556, 18.24660765846982002 ) ) ;
#125654 = DIRECTION ( 'NONE',  ( 0.7071067811865486830, -0.7071067811865464625, -0.000000000000000000 ) ) ;
#125655 = CARTESIAN_POINT ( 'NONE',  ( -25.39999999999996305, 0.000000000000000000, 0.000000000000000000 ) ) ;
#125656 = CARTESIAN_POINT ( 'NONE',  ( 0.000000000000000000, 0.000000000000000000, 5.000000000000000000 ) ) ;
#125657 = DIRECTION ( 'NONE',  ( -0.7071067811865486830, 0.7071067811865464625, 0.000000000000000000 ) ) ;
#125658 = ORIENTED_EDGE ( 'NONE', *, *, #54035, .F. ) ;
#125659 = AXIS2_PLACEMENT_3D ( 'NONE', #58619, #59308, #103463 ) ;
#125660 = EDGE_LOOP ( 'NONE', ( #142611, #100174, #125086, #51918 ) ) ;
#125661 = LINE ( 'NONE', #80735, #109850 ) ;
#125662 = LINE ( 'NONE', #15413, #109104 ) ;
#125663 = EDGE_LOOP ( 'NONE', ( #87007, #46963, #122203, #75965 ) ) ;
#125664 = ORIENTED_EDGE ( 'NONE', *, *, #8250, .T. ) ;
#125665 = ORIENTED_EDGE ( 'NONE', *, *, #30590, .T. ) ;
#125666 = CARTESIAN_POINT ( 'NONE',  ( 19.58200623001875940, 3.821174125832445049E-16, 0.000000000000000000 ) ) ;
#125667 = LINE ( 'NONE', #93023, #13685 ) ;
#125668 = CIRCLE ( 'NONE', #65571, 4.000000000000000000 ) ;
#125669 = ORIENTED_EDGE ( 'NONE', *, *, #61866, .T. ) ;
#125670 = DIRECTION ( 'NONE',  ( 0.7071067811865487940, 0.7071067811865463515, 0.000000000000000000 ) ) ;
#125671 = CARTESIAN_POINT ( 'NONE',  ( 10.12956980810188767, -3.967499999999998028, -6.871911579029511330 ) ) ;
#125672 = EDGE_CURVE ( 'NONE', #80245, #65242, #7240, .T. ) ;
#125673 = CARTESIAN_POINT ( 'NONE',  ( 11.29289321881338637, -0.7407075233842718154, 5.000000000000000000 ) ) ;
#125674 = ORIENTED_EDGE ( 'NONE', *, *, #46108, .F. ) ;
#125675 = CARTESIAN_POINT ( 'NONE',  ( 11.81601139373100651, 28.73617430169779041, 5.000000000000000000 ) ) ;
#125676 = EDGE_CURVE ( 'NONE', #467, #10314, #107294, .T. ) ;
#125677 = LINE ( 'NONE', #45986, #58163 ) ;
#125678 = CARTESIAN_POINT ( 'NONE',  ( 24.18398860626899705, 28.73617430169804265, 5.000000000000000000 ) ) ;
#125679 = VECTOR ( 'NONE', #40820, 1000.000000000000000 ) ;
#125681 = VERTEX_POINT ( 'NONE', #30464 ) ;
#125680 = DIRECTION ( 'NONE',  ( 0.7071067811865487940, 0.7071067811865463515, -0.000000000000000000 ) ) ;
#125682 = CARTESIAN_POINT ( 'NONE',  ( 18.48921356237309510, -27.52281430457068367, 5.000000000000000000 ) ) ;
#125683 = ORIENTED_EDGE ( 'NONE', *, *, #139592, .F. ) ;
#125684 = FACE_OUTER_BOUND ( 'NONE', #132599, .T. ) ;
#125685 = CARTESIAN_POINT ( 'NONE',  ( 17.84878961325748037, 3.061616997868383634E-16, -2.500000000000000444 ) ) ;
#125686 = EDGE_CURVE ( 'NONE', #30546, #101163, #69911, .T. ) ;
#125688 = EDGE_CURVE ( 'NONE', #143262, #23600, #14767, .T. ) ;
#125687 = VECTOR ( 'NONE', #77728, 999.9999999999998863 ) ;
#125689 = CARTESIAN_POINT ( 'NONE',  ( 23.99999999999981881, -22.22500000000000142, 4.412002311789994913 ) ) ;
#125691 = ORIENTED_EDGE ( 'NONE', *, *, #62281, .F. ) ;
#125690 = AXIS2_PLACEMENT_3D ( 'NONE', #127977, #38106, #7576 ) ;
#125692 = FILL_AREA_STYLE ('',( #41317 ) ) ;
#125693 = CARTESIAN_POINT ( 'NONE',  ( 37.22674160717810565, -11.24070752338416490, 18.24660765846991239 ) ) ;
#125694 = DIRECTION ( 'NONE',  ( -0.6830127018922181881, 0.6830127018922202975, -0.2588190451025214056 ) ) ;
#125695 = LINE ( 'NONE', #26375, #12005 ) ;
#125696 = VECTOR ( 'NONE', #88035, 999.9999999999998863 ) ;
#125697 = VECTOR ( 'NONE', #132553, 999.9999999999998863 ) ;
#125698 = ORIENTED_EDGE ( 'NONE', *, *, #71252, .T. ) ;
#125699 = MECHANICAL_DESIGN_GEOMETRIC_PRESENTATION_REPRESENTATION (  '', ( #93287 ), #86377 ) ;
#125700 = DIRECTION ( 'NONE',  ( 0.000000000000000000, -1.000000000000000000, 0.000000000000000000 ) ) ;
#125701 = DIRECTION ( 'NONE',  ( -0.7071067811865486830, -0.7071067811865464625, 0.000000000000000000 ) ) ;
#125702 = CARTESIAN_POINT ( 'NONE',  ( 7.483306282870439752, 6.094999999999991758, 1.633150327867686880 ) ) ;
#125703 = CARTESIAN_POINT ( 'NONE',  ( -0.8883763810524081261, 9.759292476615621936, 17.35367589129213073 ) ) ;
#125704 = EDGE_CURVE ( 'NONE', #13028, #34174, #124949, .T. ) ;
#125705 = CARTESIAN_POINT ( 'NONE',  ( 8.968407645496675684, 9.139736423841732040E-16, 0.000000000000000000 ) ) ;
#125706 = VERTEX_POINT ( 'NONE', #18852 ) ;
#125707 = EDGE_CURVE ( 'NONE', #73197, #8350, #137276, .T. ) ;
#125708 = ORIENTED_EDGE ( 'NONE', *, *, #52756, .F. ) ;
#125709 = CARTESIAN_POINT ( 'NONE',  ( 36.48921356237310221, -27.52281430457080802, 5.000000000000000000 ) ) ;
#125710 = CARTESIAN_POINT ( 'NONE',  ( 34.49999999999975842, -12.66682484999663139, -0.6294897503863142729 ) ) ;
#125711 = CARTESIAN_POINT ( 'NONE',  ( 8.145403141435220817, -2.126176841940958351, -7.934999999999989839 ) ) ;
#125712 = FACE_OUTER_BOUND ( 'NONE', #119041, .T. ) ;
#125713 = AXIS2_PLACEMENT_3D ( 'NONE', #75091, #119257, #98248 ) ;
#125714 = DIRECTION ( 'NONE',  ( 0.7071067811865487940, 0.7071067811865463515, -0.000000000000000000 ) ) ;
#125715 = DIRECTION ( 'NONE',  ( 0.7071067811865486830, -0.7071067811865464625, -0.000000000000000000 ) ) ;
#125716 = ADVANCED_FACE ( 'NONE', ( #26369 ), #96393, .T. ) ;
#125717 = FACE_OUTER_BOUND ( 'NONE', #28153, .T. ) ;
#125718 = ORIENTED_EDGE ( 'NONE', *, *, #108289, .F. ) ;
#125719 = CARTESIAN_POINT ( 'NONE',  ( 0.000000000000000000, 0.000000000000000000, 5.000000000000000000 ) ) ;
#125720 = LINE ( 'NONE', #50296, #109436 ) ;
#125721 = EDGE_CURVE ( 'NONE', #118382, #34223, #140631, .T. ) ;
#125722 = CARTESIAN_POINT ( 'NONE',  ( -2.510786437626908008, -27.52281430457053446, 5.000000000000000000 ) ) ;
#125723 = CARTESIAN_POINT ( 'NONE',  ( 47.59959685856478018, -6.109999999999998543, -1.637169565754160727 ) ) ;
#125724 = AXIS2_PLACEMENT_3D ( 'NONE', #50589, #62919, #107096 ) ;
#125725 = CARTESIAN_POINT ( 'NONE',  ( 42.18398860626899705, 28.73617430169816700, 5.000000000000000000 ) ) ;
#125726 = ORIENTED_EDGE ( 'NONE', *, *, #93238, .T. ) ;
#125727 = CARTESIAN_POINT ( 'NONE',  ( -34.92500000000001137, 5.718490437204179599, 4.759050581649334255 ) ) ;
#125728 = VECTOR ( 'NONE', #50274, 1000.000000000000000 ) ;
#125729 = ORIENTED_EDGE ( 'NONE', *, *, #118194, .F. ) ;
#125730 = FACE_OUTER_BOUND ( 'NONE', #78304, .T. ) ;
#125731 = ORIENTED_EDGE ( 'NONE', *, *, #104175, .T. ) ;
#125732 = EDGE_CURVE ( 'NONE', #118358, #62370, #92307, .T. ) ;
#125733 = CARTESIAN_POINT ( 'NONE',  ( -25.39999999999996305, 0.000000000000000000, 0.000000000000000000 ) ) ;
#125734 = LINE ( 'NONE', #90224, #101713 ) ;
#125735 = CARTESIAN_POINT ( 'NONE',  ( -18.29974487139159223, -27.71228299555219010, 4.000000000000000000 ) ) ;
#125736 = DIRECTION ( 'NONE',  ( 1.000000000000000000, 0.000000000000000000, 0.000000000000000000 ) ) ;
#125737 = DIRECTION ( 'NONE',  ( -0.7071067811865486830, 0.7071067811865464625, 0.000000000000000000 ) ) ;
#125738 = FILL_AREA_STYLE_COLOUR ( '', #140293 ) ;
#125739 = ORIENTED_EDGE ( 'NONE', *, *, #69354, .F. ) ;
#125740 = PLANE ( 'NONE',  #11639 ) ;
#125741 = FACE_OUTER_BOUND ( 'NONE', #47282, .T. ) ;
#125742 = UNCERTAINTY_MEASURE_WITH_UNIT (LENGTH_MEASURE( 1.000000000000000082E-05 ), #130108, 'distance_accuracy_value', 'NONE');
#125743 = EDGE_CURVE ( 'NONE', #76170, #120928, #103888, .T. ) ;
#125744 = FACE_OUTER_BOUND ( 'NONE', #67324, .T. ) ;
#125745 = LINE ( 'NONE', #124298, #31826 ) ;
#125746 = CIRCLE ( 'NONE', #100280, 0.5000000000000004441 ) ;
#125747 = CARTESIAN_POINT ( 'NONE',  ( 68.76669371712957002, -7.949999999999999289, 2.130196079827424427 ) ) ;
#125748 = EDGE_CURVE ( 'NONE', #141489, #33114, #27064, .T. ) ;
#125749 = CARTESIAN_POINT ( 'NONE',  ( 27.18398860626900060, 28.73617430169806042, 5.000000000000000000 ) ) ;
#125750 = VERTEX_POINT ( 'NONE', #108689 ) ;
#125751 = ORIENTED_EDGE ( 'NONE', *, *, #74222, .T. ) ;
#125752 = CARTESIAN_POINT ( 'NONE',  ( 66.47916666666665719, -7.950000000000001066, 2.130196079827424427 ) ) ;
#125753 = DIRECTION ( 'NONE',  ( -0.7071067811865486830, -0.7071067811865464625, 0.000000000000000000 ) ) ;
#125754 = FACE_OUTER_BOUND ( 'NONE', #83722, .T. ) ;
#125756 = AXIS2_PLACEMENT_3D ( 'NONE', #23419, #69101, #2359 ) ;
#125755 = CARTESIAN_POINT ( 'NONE',  ( 13.09320915088844650, 2.775078171252264969, 4.657771095945244966 ) ) ;
#125757 = AXIS2_PLACEMENT_3D ( 'NONE', #106813, #139506, #41567 ) ;
#125758 = VERTEX_POINT ( 'NONE', #122445 ) ;
#125759 = EDGE_CURVE ( 'NONE', #121677, #58909, #65257, .T. ) ;
#125760 = CARTESIAN_POINT ( 'NONE',  ( -51.48921356237309510, -27.52281430457091460, 5.000000000000000000 ) ) ;
#125761 = DIRECTION ( 'NONE',  ( 0.7071067811865487940, 0.7071067811865463515, 0.000000000000000000 ) ) ;
#125762 = CARTESIAN_POINT ( 'NONE',  ( 57.31293019189811133, -1.637169565754159617, -6.110000000000001208 ) ) ;
#125763 = FACE_OUTER_BOUND ( 'NONE', #42596, .T. ) ;
#125764 = VERTEX_POINT ( 'NONE', #23110 ) ;
#125765 = EDGE_LOOP ( 'NONE', ( #50194, #112606, #77545, #57556 ) ) ;
#125766 = AXIS2_PLACEMENT_3D ( 'NONE', #34562, #23677, #125124 ) ;
#125767 = DIRECTION ( 'NONE',  ( -0.6830127018922180770, -0.6830127018922204085, -0.2588190451025213501 ) ) ;
#125768 = CARTESIAN_POINT ( 'NONE',  ( 5.994519915287488843, 28.92564299267942118, 4.000000000000000000 ) ) ;
#125769 = DIRECTION ( 'NONE',  ( -8.817971600062199903E-18, 0.3543493200069153248, 0.9351131265310292928 ) ) ;
#125770 = CARTESIAN_POINT ( 'NONE',  ( 31.92500000000000782, 22.27000000000000313, -14.71147562388301822 ) ) ;
#125771 = PLANE ( 'NONE',  #81236 ) ;
#125773 = ORIENTED_EDGE ( 'NONE', *, *, #124001, .T. ) ;
#125772 = CARTESIAN_POINT ( 'NONE',  ( 86.60416666666667140, 2.130196079827460398, 7.949999999999981526 ) ) ;
#125774 = CARTESIAN_POINT ( 'NONE',  ( -7.499999999999951150, 0.4497235411627352741, -5.599840258123558456 ) ) ;
#125775 = CARTESIAN_POINT ( 'NONE',  ( 14.99999999999989519, 15.45873954670186201, -0.03131636524297733842 ) ) ;
#125776 = VECTOR ( 'NONE', #55696, 1000.000000000000114 ) ;
#125777 = DIRECTION ( 'NONE',  ( -0.7071067811865486830, -0.7071067811865464625, 0.000000000000000000 ) ) ;
#125778 = DIRECTION ( 'NONE',  ( -1.734723475976805517E-15, -1.000000000000000000, 0.000000000000000000 ) ) ;
#125779 = EDGE_LOOP ( 'NONE', ( #35577, #17013, #106147, #5778 ) ) ;
#125780 = ORIENTED_EDGE ( 'NONE', *, *, #134919, .T. ) ;
#125781 =( NAMED_UNIT ( * ) SI_UNIT ( $, .STERADIAN. ) SOLID_ANGLE_UNIT ( ) );
#125782 = PLANE ( 'NONE',  #113550 ) ;
#125783 = EDGE_CURVE ( 'NONE', #32117, #53287, #78262, .T. ) ;
#125784 = CARTESIAN_POINT ( 'NONE',  ( 111.7875270504628986, 0.000000000000000000, -7.949999999999998401 ) ) ;
#125785 = CARTESIAN_POINT ( 'NONE',  ( 0.000000000000000000, 0.000000000000000000, 5.000000000000000000 ) ) ;
#125786 = ORIENTED_EDGE ( 'NONE', *, *, #133674, .T. ) ;
#125787 = EDGE_LOOP ( 'NONE', ( #75100, #34928, #73586, #54984, #34833 ) ) ;
#125788 = AXIS2_PLACEMENT_3D ( 'NONE', #79013, #113015, #25295 ) ;
#125789 = PLANE ( 'NONE',  #120962 ) ;
#125790 = FACE_OUTER_BOUND ( 'NONE', #83344, .T. ) ;
#125791 = AXIS2_PLACEMENT_3D ( 'NONE', #67546, #111743, #56692 ) ;
#125792 = EDGE_LOOP ( 'NONE', ( #112940, #34075, #46453, #22531 ) ) ;
#125793 = CARTESIAN_POINT ( 'NONE',  ( -21.79333936457831911, 21.75929247661549226, 4.998822639870701856 ) ) ;
#125794 = ADVANCED_FACE ( 'NONE', ( #100006 ), #8653, .F. ) ;
#125795 = ORIENTED_EDGE ( 'NONE', *, *, #139619, .F. ) ;
#125796 = CARTESIAN_POINT ( 'NONE',  ( 62.64169371712956291, -2.130196079827424871, -7.949999999999998401 ) ) ;
#125797 = DIRECTION ( 'NONE',  ( 0.7071067811865487940, 0.7071067811865463515, 0.000000000000000000 ) ) ;
#125798 = AXIS2_PLACEMENT_3D ( 'NONE', #124874, #111867, #123483 ) ;
#125799 = ADVANCED_FACE ( 'NONE', ( #42787 ), #133356, .F. ) ;
#125800 = FACE_BOUND ( 'NONE', #47849, .T. ) ;
#125801 = DIRECTION ( 'NONE',  ( 0.6830127018922181881, 0.6830127018922202975, -0.2588190451025214056 ) ) ;
#125802 = CARTESIAN_POINT ( 'NONE',  ( 66.18398860626901126, 28.73617430169833753, 5.000000000000000000 ) ) ;
#125803 = EDGE_CURVE ( 'NONE', #94938, #81077, #55079, .T. ) ;
#125804 = CARTESIAN_POINT ( 'NONE',  ( 0.000000000000000000, 0.000000000000000000, 5.000000000000000000 ) ) ;
#125805 = CARTESIAN_POINT ( 'NONE',  ( 0.000000000000000000, 0.000000000000000000, 5.000000000000000000 ) ) ;
#125806 = EDGE_CURVE ( 'NONE', #11091, #110710, #76109, .T. ) ;
#125807 = DIRECTION ( 'NONE',  ( 1.000000000000000000, 0.000000000000000000, 0.000000000000000000 ) ) ;
#125808 = SHAPE_DEFINITION_REPRESENTATION ( #132402, #64389 ) ;
#125809 = VERTEX_POINT ( 'NONE', #66669 ) ;
#125810 = VECTOR ( 'NONE', #66874, 1000.000000000000000 ) ;
#125811 = VERTEX_POINT ( 'NONE', #64513 ) ;
#125812 = CARTESIAN_POINT ( 'NONE',  ( 89.45376352523146579, -6.109999999999998543, -3.741295971395162543E-16 ) ) ;
#125813 = EDGE_LOOP ( 'NONE', ( #71840, #117386, #48349, #12237 ) ) ;
#125814 = EDGE_CURVE ( 'NONE', #61548, #95615, #142100, .T. ) ;
#125815 = PLANE ( 'NONE',  #14131 ) ;
#125816 = LINE ( 'NONE', #94578, #67835 ) ;
#125817 = AXIS2_PLACEMENT_3D ( 'NONE', #16323, #106924, #62030 ) ;
#125818 = EDGE_CURVE ( 'NONE', #125750, #123892, #21726, .T. ) ;
#125819 = LINE ( 'NONE', #6828, #100381 ) ;
#125820 = ORIENTED_EDGE ( 'NONE', *, *, #126688, .F. ) ;
#125821 = CARTESIAN_POINT ( 'NONE',  ( 35.99999999999999289, 0.000000000000000000, -7.950000000000000178 ) ) ;
#125822 = LINE ( 'NONE', #15568, #47792 ) ;
#125823 = CIRCLE ( 'NONE', #95680, 0.5000000000000004441 ) ;
#125824 = CARTESIAN_POINT ( 'NONE',  ( 111.2500000000000000, -9.735942053221458872E-16, 7.950000000000000178 ) ) ;
#125826 = CARTESIAN_POINT ( 'NONE',  ( -20.67183060077633527, 17.25929247661555266, 4.000000000000000000 ) ) ;
#125825 = CARTESIAN_POINT ( 'NONE',  ( 0.1839886062690032631, 28.73617430169787568, 5.000000000000000000 ) ) ;
#125827 = DIRECTION ( 'NONE',  ( -0.7071067811865487940, 0.7071067811865463515, 0.000000000000000000 ) ) ;
#125828 = EDGE_CURVE ( 'NONE', #18455, #127835, #37013, .T. ) ;
#125829 = DIRECTION ( 'NONE',  ( -0.000000000000000000, 0.3543493200069153248, 0.9351131265310292928 ) ) ;
#125830 = EDGE_LOOP ( 'NONE', ( #31782, #94569, #16227, #10606 ) ) ;
#125831 = PLANE ( 'NONE',  #45020 ) ;
#125832 =( BOUNDED_CURVE ( )  B_SPLINE_CURVE ( 2, ( #72771, #139437, #27058, #38664, #29200, #82893, #51691, #60443, #18294, #106021, #37963, #49570, #62565 ),
 .UNSPECIFIED., .F., .T. ) 
 B_SPLINE_CURVE_WITH_KNOTS ( ( 3, 2, 2, 2, 2, 2, 3 ),
 ( 0.3500000000000000333, 0.3583333333333333925, 0.3666666666666666963, 0.3750000000000001110, 0.3833333333333334703, 0.3916666666666667740, 0.4000000000000001332 ),
 .UNSPECIFIED. ) 
 CURVE ( )  GEOMETRIC_REPRESENTATION_ITEM ( )  RATIONAL_B_SPLINE_CURVE ( ( 0.9999999999999997780, 0.9659258262890685343, 1.000000000000000000, 0.9659258262890683122, 1.000000000000000000, 0.9659258262890683122, 1.000000000000000000, 0.9659258262890683122, 1.000000000000000000, 0.9659258262890683122, 1.000000000000000000, 0.9659258262890678681, 1.000000000000000444 ) ) 
 REPRESENTATION_ITEM ( '' )  );
#125833 = FACE_OUTER_BOUND ( 'NONE', #141664, .T. ) ;
#125834 = VECTOR ( 'NONE', #60642, 999.9999999999998863 ) ;
#125835 = EDGE_LOOP ( 'NONE', ( #63782, #14040, #55472, #113683 ) ) ;
#125836 = ORIENTED_EDGE ( 'NONE', *, *, #93308, .T. ) ;
#125837 = ORIENTED_EDGE ( 'NONE', *, *, #106808, .F. ) ;
#125838 = CARTESIAN_POINT ( 'NONE',  ( 41.41709685856477563, 3.054999999999998828, 5.291415217122922066 ) ) ;
#125839 = ADVANCED_FACE ( 'NONE', ( #136905 ), #2810, .F. ) ;
#125840 = ORIENTED_EDGE ( 'NONE', *, *, #57594, .F. ) ;
#125841 = AXIS2_PLACEMENT_3D ( 'NONE', #121503, #22184, #110613 ) ;
#125842 = VECTOR ( 'NONE', #88070, 1000.000000000000000 ) ;
#125843 = CARTESIAN_POINT ( 'NONE',  ( 12.58747294953710671, -6.094999999999989981, 3.732111120401553285E-16 ) ) ;
#125844 = AXIS2_PLACEMENT_3D ( 'NONE', #82595, #15168, #103604 ) ;
#125845 = SURFACE_STYLE_USAGE ( .BOTH. , #45447 ) ;
#125846 = VERTEX_POINT ( 'NONE', #45650 ) ;
#125847 = PLANE ( 'NONE',  #47953 ) ;
#125848 = EDGE_CURVE ( 'NONE', #133129, #59855, #80698, .T. ) ;
#125849 = ORIENTED_EDGE ( 'NONE', *, *, #99858, .T. ) ;
#125850 =( NAMED_UNIT ( * ) PLANE_ANGLE_UNIT ( ) SI_UNIT ( $, .RADIAN. ) );
#125851 = PRESENTATION_LAYER_ASSIGNMENT (  '', '', ( #24014 ) ) ;
#125852 = DIRECTION ( 'NONE',  ( -1.000000000000000000, 0.000000000000000000, 0.000000000000000000 ) ) ;
#125854 = ORIENTED_EDGE ( 'NONE', *, *, #36970, .F. ) ;
#125853 = CARTESIAN_POINT ( 'NONE',  ( 20.27718569542926730, -21.72500000000000853, 5.000000000000000000 ) ) ;
#125855 = ORIENTED_EDGE ( 'NONE', *, *, #57378, .F. ) ;
#125856 = PLANE ( 'NONE',  #120901 ) ;
#125857 = CARTESIAN_POINT ( 'NONE',  ( 28.49999999999980815, 6.431123077392117082, 4.000000000000000000 ) ) ;
#125858 = EDGE_CURVE ( 'NONE', #91146, #114341, #13667, .T. ) ;
#125859 = ADVANCED_FACE ( 'NONE', ( #37607 ), #81853, .F. ) ;
#125860 = EDGE_LOOP ( 'NONE', ( #2683, #24028, #104364, #69855, #143401, #34691 ) ) ;
#125861 = DIRECTION ( 'NONE',  ( -0.6830127018922180770, -0.6830127018922204085, -0.2588190451025213501 ) ) ;
#125862 = ORIENTED_EDGE ( 'NONE', *, *, #118681, .T. ) ;
#125863 = ORIENTED_EDGE ( 'NONE', *, *, #99791, .F. ) ;
#125864 = VERTEX_POINT ( 'NONE', #113726 ) ;
#125865 = ORIENTED_EDGE ( 'NONE', *, *, #21440, .T. ) ;
#125866 = SURFACE_STYLE_FILL_AREA ( #101228 ) ;
#125867 = VECTOR ( 'NONE', #5295, 1000.000000000000000 ) ;
#125868 = EDGE_CURVE ( 'NONE', #125809, #141911, #12264, .T. ) ;
#125869 = LINE ( 'NONE', #101955, #28862 ) ;
#125870 = ADVANCED_FACE ( 'NONE', ( #101416 ), #119965, .T. ) ;
#125871 = LINE ( 'NONE', #95356, #129357 ) ;
#125872 = LINE ( 'NONE', #136009, #76628 ) ;
#125873 =( GEOMETRIC_REPRESENTATION_CONTEXT ( 3 ) GLOBAL_UNCERTAINTY_ASSIGNED_CONTEXT ( ( #27111 ) ) GLOBAL_UNIT_ASSIGNED_CONTEXT ( ( #49107, #16422, #94700 ) ) REPRESENTATION_CONTEXT ( 'NONE', 'WORKASPACE' ) );
#125874 = VERTEX_POINT ( 'NONE', #125323 ) ;
#125875 = LINE ( 'NONE', #120667, #79524 ) ;
#125876 = CARTESIAN_POINT ( 'NONE',  ( 23.02040314143522082, 7.934999999999989839, -2.126176841940961904 ) ) ;
#125877 = DIRECTION ( 'NONE',  ( 0.7071067811865486830, -0.7071067811865464625, -0.000000000000000000 ) ) ;
#125878 = ADVANCED_FACE ( 'NONE', ( #2066 ), #123914, .F. ) ;
#125879 = CARTESIAN_POINT ( 'NONE',  ( 12.29974487139158512, -27.71228299555214747, 4.000000000000000000 ) ) ;
#125880 = EDGE_LOOP ( 'NONE', ( #119128, #70439, #29754, #41757, #77005 ) ) ;
#125881 = VERTEX_POINT ( 'NONE', #1366 ) ;
#125882 = VERTEX_POINT ( 'NONE', #81119 ) ;
#125883 = DIRECTION ( 'NONE',  ( 0.000000000000000000, -1.000000000000000000, 0.000000000000000000 ) ) ;
#125884 = CARTESIAN_POINT ( 'NONE',  ( -29.99999999999978684, 7.552185695429095347, 5.000000000000000000 ) ) ;
#125885 = UNCERTAINTY_MEASURE_WITH_UNIT (LENGTH_MEASURE( 1.000000000000000082E-05 ), #196, 'distance_accuracy_value', 'NONE');
#125886 = CARTESIAN_POINT ( 'NONE',  ( -34.42500000000001137, -21.72500000000000142, 0.4999999999999995559 ) ) ;
#125887 = DIRECTION ( 'NONE',  ( -0.7071067811865487940, 0.7071067811865463515, -0.000000000000000000 ) ) ;
#125888 = EDGE_CURVE ( 'NONE', #123049, #99331, #134065, .T. ) ;
#125889 = CARTESIAN_POINT ( 'NONE',  ( 71.37043019189812298, -3.055000000000001936, 5.291415217122918513 ) ) ;
#125890 = VECTOR ( 'NONE', #134006, 1000.000000000000000 ) ;
#125891 = CARTESIAN_POINT ( 'NONE',  ( 74.60002705046289861, 5.819803920172570422, 5.819803920172575751 ) ) ;
#125892 = LINE ( 'NONE', #25844, #134016 ) ;
#125893 = PLANE ( 'NONE',  #115869 ) ;
#125894 = DIRECTION ( 'NONE',  ( 1.000000000000000000, -0.000000000000000000, -0.000000000000000000 ) ) ;
#125895 = DIRECTION ( 'NONE',  ( -0.000000000000000000, -0.3543493200069152693, 0.9351131265310292928 ) ) ;
#125896 = VERTEX_POINT ( 'NONE', #58697 ) ;
#125897 = LINE ( 'NONE', #114959, #82383 ) ;
#125898 = VERTEX_POINT ( 'NONE', #102155 ) ;
#125899 = CARTESIAN_POINT ( 'NONE',  ( -2.700255128608413990, -27.71228299555204089, 4.000000000000000000 ) ) ;
#125901 = ORIENTED_EDGE ( 'NONE', *, *, #11879, .T. ) ;
#125900 = CARTESIAN_POINT ( 'NONE',  ( 17.99999999999988276, 17.58746187583906462, 4.000000000000000000 ) ) ;
#125902 = CARTESIAN_POINT ( 'NONE',  ( -44.99451991528749772, 28.92564299267969474, 4.000000000000000000 ) ) ;
#125903 = CARTESIAN_POINT ( 'NONE',  ( -18.51665438641032679, 22.22500000000000142, 4.500000000000000888 ) ) ;
#125904 = ORIENTED_EDGE ( 'NONE', *, *, #118638, .F. ) ;
#125905 = DIRECTION ( 'NONE',  ( -1.084202172485504434E-16, 1.000000000000000000, -0.000000000000000000 ) ) ;
#125906 = EDGE_LOOP ( 'NONE', ( #18974, #141964, #71801, #50075, #134507 ) ) ;
#125907 = CARTESIAN_POINT ( 'NONE',  ( -0.4892135623730947680, -27.52281430457055578, 5.000000000000000000 ) ) ;
#125908 = ORIENTED_EDGE ( 'NONE', *, *, #126023, .T. ) ;
#125909 = VECTOR ( 'NONE', #95840, 1000.000000000000227 ) ;
#125910 = DIRECTION ( 'NONE',  ( 0.000000000000000000, -1.000000000000000000, 0.000000000000000000 ) ) ;
#125911 = EDGE_CURVE ( 'NONE', #51489, #91902, #70277, .T. ) ;
#125912 = CARTESIAN_POINT ( 'NONE',  ( 101.8708603837962272, 6.884901960086289741, -3.974999999999993427 ) ) ;
#125913 = CARTESIAN_POINT ( 'NONE',  ( -24.79289321881328334, -2.240707523384257716, 5.000000000000000000 ) ) ;
#125914 = VECTOR ( 'NONE', #90599, 1000.000000000000000 ) ;
#125915 = CARTESIAN_POINT ( 'NONE',  ( -33.79289321881321229, 9.759292476615621936, 5.000000000000000000 ) ) ;
#125916 = EDGE_LOOP ( 'NONE', ( #6935, #90741, #30478, #77648 ) ) ;
#125917 = CARTESIAN_POINT ( 'NONE',  ( 34.92499999999998295, -18.28150956279555217, 4.759050581649326261 ) ) ;
#125918 = CARTESIAN_POINT ( 'NONE',  ( -20.21837311707492546, 21.74787736706806740, 4.999607392498048419 ) ) ;
#125919 = DIRECTION ( 'NONE',  ( -0.6830127018922181881, 0.6830127018922202975, -0.2588190451025214056 ) ) ;
#125920 = CARTESIAN_POINT ( 'NONE',  ( 25.52083333333332860, -6.094999999999989981, -1.633150327867689100 ) ) ;
#125921 = DIRECTION ( 'NONE',  ( 0.000000000000000000, 0.000000000000000000, 1.000000000000000000 ) ) ;
#125922 = VERTEX_POINT ( 'NONE', #24570 ) ;
#125923 = VECTOR ( 'NONE', #12436, 1000.000000000000227 ) ;
#125924 = DIRECTION ( 'NONE',  ( -0.7071067811865486830, -0.7071067811865464625, 0.000000000000000000 ) ) ;
#125925 = ORIENTED_EDGE ( 'NONE', *, *, #5726, .T. ) ;
#125926 = CIRCLE ( 'NONE', #19417, 2.500000000000000888 ) ;
#125927 = CARTESIAN_POINT ( 'NONE',  ( 86.77126352523141861, 4.472830434245839371, 4.472830434245842035 ) ) ;
#125928 = CARTESIAN_POINT ( 'NONE',  ( 29.99999999999979039, 7.931123077392108200, 4.000000000000000000 ) ) ;
#125929 = DIRECTION ( 'NONE',  ( 0.7071067811865486830, -0.7071067811865464625, -0.000000000000000000 ) ) ;
#125930 = CARTESIAN_POINT ( 'NONE',  ( 27.79289321881327268, -5.240707523384227073, 5.000000000000000000 ) ) ;
#125931 = VERTEX_POINT ( 'NONE', #35497 ) ;
#125932 = LINE ( 'NONE', #73011, #122951 ) ;
#125933 = VECTOR ( 'NONE', #29218, 1000.000000000000227 ) ;
#125934 = DIRECTION ( 'NONE',  ( 0.6830127018922180770, -0.6830127018922204085, -0.2588190451025213501 ) ) ;
#125935 = AXIS2_PLACEMENT_3D ( 'NONE', #97866, #63824, #141361 ) ;
#125936 = LINE ( 'NONE', #124493, #85545 ) ;
#125937 = CARTESIAN_POINT ( 'NONE',  ( 14.47599861414540534, 22.03583458319438648, 4.979811245910083173 ) ) ;
#125939 = ORIENTED_EDGE ( 'NONE', *, *, #69080, .F. ) ;
#125938 = CARTESIAN_POINT ( 'NONE',  ( 11.72733514412567857, 0.000000000000000000, 2.500000000000000444 ) ) ;
#125940 = CARTESIAN_POINT ( 'NONE',  ( 0.000000000000000000, 0.000000000000000000, 5.000000000000000000 ) ) ;
#125941 = CARTESIAN_POINT ( 'NONE',  ( 18.17159235450331778, -2.500000000000000444, 3.061616997868384620E-16 ) ) ;
#125942 = FILL_AREA_STYLE ('',( #116480 ) ) ;
#125943 = VECTOR ( 'NONE', #89790, 1000.000000000000000 ) ;
#125944 = ORIENTED_EDGE ( 'NONE', *, *, #137953, .T. ) ;
#125945 = ORIENTED_EDGE ( 'NONE', *, *, #119546, .F. ) ;
#125946 = ORIENTED_EDGE ( 'NONE', *, *, #123005, .F. ) ;
#125947 = CARTESIAN_POINT ( 'NONE',  ( 85.75043019189810423, 3.055000000000002824, -5.291415217122919401 ) ) ;
#125948 = VECTOR ( 'NONE', #10105, 1000.000000000000000 ) ;
#125949 = ORIENTED_EDGE ( 'NONE', *, *, #137121, .F. ) ;
#125950 = DIRECTION ( 'NONE',  ( 0.000000000000000000, 1.000000000000000000, 0.000000000000000000 ) ) ;
#125951 = DIRECTION ( 'NONE',  ( -0.7071067811865486830, -0.7071067811865464625, -0.000000000000000000 ) ) ;
#125952 = ADVANCED_FACE ( 'NONE', ( #78991 ), #14415, .T. ) ;
#125953 = VECTOR ( 'NONE', #24428, 999.9999999999998863 ) ;
#125954 = DIRECTION ( 'NONE',  ( -0.7071067811865486830, -0.7071067811865464625, -0.000000000000000000 ) ) ;
#125955 = PLANE ( 'NONE',  #3761 ) ;
#125956 = ORIENTED_EDGE ( 'NONE', *, *, #21759, .F. ) ;
#125957 = CARTESIAN_POINT ( 'NONE',  ( 0.5685132242927012358, -0.3999999999999997446, -2.467792535850613866 ) ) ;
#125958 = CARTESIAN_POINT ( 'NONE',  ( 17.29289321881333308, -18.74070752338409562, 5.000000000000000000 ) ) ;
#125959 = CARTESIAN_POINT ( 'NONE',  ( 79.39126352523146579, -4.472830434245839371, -4.472830434245839371 ) ) ;
#125960 = ADVANCED_FACE ( 'NONE', ( #68826 ), #112999, .T. ) ;
#125961 = ORIENTED_EDGE ( 'NONE', *, *, #105114, .F. ) ;
#125962 = LINE ( 'NONE', #37533, #95281 ) ;
#125963 = EDGE_CURVE ( 'NONE', #24682, #96698, #3503, .T. ) ;
#125964 = CARTESIAN_POINT ( 'NONE',  ( 33.62086038379622011, -6.884901960086286188, 3.974999999999997424 ) ) ;
#125965 = AXIS2_PLACEMENT_3D ( 'NONE', #10822, #32626, #76857 ) ;
#125966 = CARTESIAN_POINT ( 'NONE',  ( -75.48921356237309510, -27.52281430457107803, 5.000000000000000000 ) ) ;
#125967 = ORIENTED_EDGE ( 'NONE', *, *, #47265, .F. ) ;
#125968 = EDGE_LOOP ( 'NONE', ( #92851, #125492, #24862, #13683 ) ) ;
#125969 = EDGE_CURVE ( 'NONE', #103228, #34514, #91293, .T. ) ;
#125970 = DIRECTION ( 'NONE',  ( -0.7071067811865487940, 0.7071067811865463515, -0.000000000000000000 ) ) ;
#125971 = ADVANCED_FACE ( 'NONE', ( #73104 ), #49919, .F. ) ;
#125972 = ADVANCED_FACE ( 'NONE', ( #41154 ), #83243, .F. ) ;
#125973 = LINE ( 'NONE', #106304, #15340 ) ;
#125974 = DIRECTION ( 'NONE',  ( 0.7071067811865487940, 0.7071067811865463515, 0.000000000000000000 ) ) ;
#125975 = LINE ( 'NONE', #29481, #4851 ) ;
#125976 = CARTESIAN_POINT ( 'NONE',  ( 2.999999999999999112, -47.62213595499956398, -36.92499999999996874 ) ) ;
#125977 = CARTESIAN_POINT ( 'NONE',  ( -14.29289321881335617, 20.25929247661551003, 5.000000000000000000 ) ) ;
#125978 = EDGE_CURVE ( 'NONE', #66817, #121662, #60819, .T. ) ;
#125979 = EDGE_CURVE ( 'NONE', #121207, #105943, #4233, .T. ) ;
#125980 = LINE ( 'NONE', #127380, #25759 ) ;
#125981 = VECTOR ( 'NONE', #93028, 1000.000000000000000 ) ;
#125982 = VERTEX_POINT ( 'NONE', #39020 ) ;
#125983 = VERTEX_POINT ( 'NONE', #70956 ) ;
#125985 = EDGE_CURVE ( 'NONE', #14551, #143518, #116579, .T. ) ;
#125984 = CARTESIAN_POINT ( 'NONE',  ( 10.20833333333333570, 3.047499999999997655, 5.278424836066143655 ) ) ;
#125986 = ORIENTED_EDGE ( 'NONE', *, *, #72818, .T. ) ;
#125987 = AXIS2_PLACEMENT_3D ( 'NONE', #16874, #29865, #74109 ) ;
#125988 = LINE ( 'NONE', #128819, #96366 ) ;
#125989 = EDGE_CURVE ( 'NONE', #5949, #90206, #127449, .T. ) ;
#125990 = DIRECTION ( 'NONE',  ( -0.000000000000000000, 0.3543493200069153248, 0.9351131265310292928 ) ) ;
#125991 = ORIENTED_EDGE ( 'NONE', *, *, #52906, .T. ) ;
#125992 = DIRECTION ( 'NONE',  ( -0.000000000000000000, -0.3543493200069152138, 0.9351131265310292928 ) ) ;
#125993 = CARTESIAN_POINT ( 'NONE',  ( 21.18398860626899349, 28.73617430169802134, 5.000000000000000000 ) ) ;
#125994 = FACE_OUTER_BOUND ( 'NONE', #101177, .T. ) ;
#125995 = DIRECTION ( 'NONE',  ( -0.7071067811865486830, -0.7071067811865464625, 0.000000000000000000 ) ) ;
#125996 = ORIENTED_EDGE ( 'NONE', *, *, #108255, .T. ) ;
#125997 = CARTESIAN_POINT ( 'NONE',  ( -7.140000000000001457, -39.92999999999999261, -39.50000000000000000 ) ) ;
#125998 = CARTESIAN_POINT ( 'NONE',  ( 17.99999999999987566, 10.55218569542905627, 5.000000000000000000 ) ) ;
#125999 = EDGE_LOOP ( 'NONE', ( #34070, #113340, #5397, #68130 ) ) ;
#126000 = DIRECTION ( 'NONE',  ( 0.7071067811865487940, 0.7071067811865463515, 0.000000000000000000 ) ) ;
#126001 = ORIENTED_EDGE ( 'NONE', *, *, #59533, .F. ) ;
#126002 = ORIENTED_EDGE ( 'NONE', *, *, #48904, .T. ) ;
#126003 = DIRECTION ( 'NONE',  ( -0.7071067811865487940, 0.7071067811865463515, 0.000000000000000000 ) ) ;
#126004 = ORIENTED_EDGE ( 'NONE', *, *, #116494, .T. ) ;
#126005 = ORIENTED_EDGE ( 'NONE', *, *, #42022, .T. ) ;
#126006 = CARTESIAN_POINT ( 'NONE',  ( 70.00043019189810423, -3.055000000000002380, 5.291415217122920289 ) ) ;
#126008 = EDGE_CURVE ( 'NONE', #9115, #89845, #17942, .T. ) ;
#126007 = VECTOR ( 'NONE', #72914, 1000.000000000000227 ) ;
#126009 = ORIENTED_EDGE ( 'NONE', *, *, #19930, .F. ) ;
#126010 =( BOUNDED_CURVE ( )  B_SPLINE_CURVE ( 2, ( #19100, #62626, #49632, #140180, #63365, #93809, #106806, #82943, #7496, #107534, #51753, #127141, #22635 ),
 .UNSPECIFIED., .F., .T. ) 
 B_SPLINE_CURVE_WITH_KNOTS ( ( 3, 2, 2, 2, 2, 2, 3 ),
 ( 0.2333333333333333370, 0.2361111111111111049, 0.2388888888888889006, 0.2416666666666666685, 0.2444444444444444364, 0.2472222222222222321, 0.2500000000000000000 ),
 .UNSPECIFIED. ) 
 CURVE ( )  GEOMETRIC_REPRESENTATION_ITEM ( )  RATIONAL_B_SPLINE_CURVE ( ( 1.000000000000000000, 0.9659258262890683122, 1.000000000000000000, 0.9659258262890683122, 1.000000000000000000, 0.9659258262890683122, 1.000000000000000000, 0.9659258262890683122, 1.000000000000000000, 0.9659258262890683122, 1.000000000000000000, 0.9659258262890683122, 1.000000000000000000 ) ) 
 REPRESENTATION_ITEM ( '' )  );
#126011 = FACE_OUTER_BOUND ( 'NONE', #126509, .T. ) ;
#126012 = CARTESIAN_POINT ( 'NONE',  ( 20.80599055185816582, -22.22500000000000142, 26.11855565392658463 ) ) ;
#126013 = AXIS2_PLACEMENT_3D ( 'NONE', #21597, #99863, #64382 ) ;
#126014 = FACE_OUTER_BOUND ( 'NONE', #96546, .T. ) ;
#126015 = CARTESIAN_POINT ( 'NONE',  ( 112.1462635252314328, -4.472830434245840259, 4.472830434245838482 ) ) ;
#126016 = CARTESIAN_POINT ( 'NONE',  ( 18.75860074219783868, 21.72500000000000853, 5.000000000000000000 ) ) ;
#126017 = VECTOR ( 'NONE', #28015, 1000.000000000000000 ) ;
#126018 = CARTESIAN_POINT ( 'NONE',  ( 24.59263130292903554, 0.9595543924999635488, 5.000000000000000000 ) ) ;
#126019 = ADVANCED_FACE ( 'NONE', ( #139057 ), #39761, .T. ) ;
#126020 = FACE_OUTER_BOUND ( 'NONE', #77850, .T. ) ;
#126021 = CARTESIAN_POINT ( 'NONE',  ( 35.37086038379622011, 6.884901960086289741, -3.974999999999993427 ) ) ;
#126023 = EDGE_CURVE ( 'NONE', #46563, #63474, #71660, .T. ) ;
#126022 = CARTESIAN_POINT ( 'NONE',  ( 0.000000000000000000, -40.42999999999999261, -40.00000000000000000 ) ) ;
#126024 = ORIENTED_EDGE ( 'NONE', *, *, #75173, .F. ) ;
#126025 = CARTESIAN_POINT ( 'NONE',  ( 36.48921356237310221, -27.52281430457080802, 5.000000000000000000 ) ) ;
#126027 = DIRECTION ( 'NONE',  ( -0.3543493200069163240, 4.681814790819596721E-17, -0.9351131265310288487 ) ) ;
#126026 = VECTOR ( 'NONE', #110671, 1000.000000000000000 ) ;
#126028 = EDGE_LOOP ( 'NONE', ( #49196, #94793, #32464, #125482 ) ) ;
#126029 = ADVANCED_FACE ( 'NONE', ( #73792 ), #117962, .T. ) ;
#126030 = VERTEX_POINT ( 'NONE', #106373 ) ;
#126031 = CARTESIAN_POINT ( 'NONE',  ( 9.183988606268997046, 28.73617430169793607, 5.000000000000000000 ) ) ;
#126032 = VERTEX_POINT ( 'NONE', #50613 ) ;
#126033 = EDGE_CURVE ( 'NONE', #56507, #33017, #95526, .T. ) ;
#126034 = FACE_OUTER_BOUND ( 'NONE', #33607, .T. ) ;
#126035 = CARTESIAN_POINT ( 'NONE',  ( 7.939999999999994174, -60.26999999999998892, -10.00000000000000178 ) ) ;
#126036 = AXIS2_PLACEMENT_3D ( 'NONE', #63124, #94979, #142106 ) ;
#126037 = CARTESIAN_POINT ( 'NONE',  ( -19.49999999999987921, 22.22500000000000142, 4.362957392718803007 ) ) ;
#126038 = DIRECTION ( 'NONE',  ( -0.3543493200069163240, 0.000000000000000000, -0.9351131265310288487 ) ) ;
#126039 = EDGE_LOOP ( 'NONE', ( #136166, #18842, #93872, #19119 ) ) ;
#126040 = LINE ( 'NONE', #26709, #108962 ) ;
#126041 = ORIENTED_EDGE ( 'NONE', *, *, #17977, .T. ) ;
#126042 = EDGE_CURVE ( 'NONE', #9815, #88923, #84670, .T. ) ;
#126044 = VECTOR ( 'NONE', #138509, 1000.000000000000000 ) ;
#126043 = CARTESIAN_POINT ( 'NONE',  ( 5.999999999999950262, -16.02097659208071079, -11.96015758381210148 ) ) ;
#126045 = VECTOR ( 'NONE', #5986, 1000.000000000000227 ) ;
#126046 = CARTESIAN_POINT ( 'NONE',  ( 24.42123647476855552, -9.717572351234235426E-16, -7.934999999999990727 ) ) ;
#126047 = AXIS2_PLACEMENT_3D ( 'NONE', #62950, #140470, #7801 ) ;
#126048 = DIRECTION ( 'NONE',  ( 0.6830127018922181881, 0.6830127018922202975, -0.2588190451025214056 ) ) ;
#126049 = ADVANCED_FACE ( 'NONE', ( #128190 ), #104247, .F. ) ;
#126050 = CARTESIAN_POINT ( 'NONE',  ( 13.79677315470453181, -9.118197820415756993, -2.677214429515783145 ) ) ;
#126051 = VERTEX_POINT ( 'NONE', #82531 ) ;
#126052 = VERTEX_POINT ( 'NONE', #4912 ) ;
#126053 = VERTEX_POINT ( 'NONE', #49210 ) ;
#126054 = CARTESIAN_POINT ( 'NONE',  ( 29.86500426248360185, 3.759292476615688550, 15.36553568819719295 ) ) ;
#126055 = CARTESIAN_POINT ( 'NONE',  ( 10.77958563595370833, 4.584330080086930965E-16, 0.000000000000000000 ) ) ;
#126056 = DIRECTION ( 'NONE',  ( 0.7071067811865487940, 0.7071067811865463515, 0.000000000000000000 ) ) ;
#126057 = VERTEX_POINT ( 'NONE', #107116 ) ;
#126058 = DIRECTION ( 'NONE',  ( 0.3543493200069162685, -0.000000000000000000, -0.9351131265310288487 ) ) ;
#126059 = PLANE ( 'NONE',  #75877 ) ;
#126060 = AXIS2_PLACEMENT_3D ( 'NONE', #70746, #128665, #104019 ) ;
#126061 = DIRECTION ( 'NONE',  ( 0.7071067811865487940, 0.7071067811865463515, 0.000000000000000000 ) ) ;
#126062 = LINE ( 'NONE', #25289, #18763 ) ;
#126063 = DIRECTION ( 'NONE',  ( -1.000000000000000000, 0.000000000000000000, 0.000000000000000000 ) ) ;
#126064 = VERTEX_POINT ( 'NONE', #93402 ) ;
#126065 = CARTESIAN_POINT ( 'NONE',  ( 74.06249999999998579, -5.819803920172573086, -5.819803920172573974 ) ) ;
#126066 = PLANE ( 'NONE',  #97941 ) ;
#126067 = ORIENTED_EDGE ( 'NONE', *, *, #92752, .T. ) ;
#126068 = CARTESIAN_POINT ( 'NONE',  ( 12.40000000000000213, -2.055000000000000160, 0.000000000000000000 ) ) ;
#126071 = ADVANCED_FACE ( 'NONE', ( #28867 ), #7793, .F. ) ;
#126070 = VERTEX_POINT ( 'NONE', #83989 ) ;
#126069 = CARTESIAN_POINT ( 'NONE',  ( -6.299744871391586898, -27.71228299555210484, 4.000000000000000000 ) ) ;
#126072 = ORIENTED_EDGE ( 'NONE', *, *, #81633, .T. ) ;
#126073 = DIRECTION ( 'NONE',  ( 0.6830127018922180770, -0.6830127018922204085, -0.2588190451025213501 ) ) ;
#126074 = PLANE ( 'NONE',  #51648 ) ;
#126075 = PLANE ( 'NONE',  #122485 ) ;
#126076 = VERTEX_POINT ( 'NONE', #119404 ) ;
#126077 = DIRECTION ( 'NONE',  ( 0.7071067811865487940, 0.7071067811865463515, 0.000000000000000000 ) ) ;
#126078 = UNCERTAINTY_MEASURE_WITH_UNIT (LENGTH_MEASURE( 1.000000000000000082E-05 ), #1733, 'distance_accuracy_value', 'NONE');
#126079 = DIRECTION ( 'NONE',  ( 0.7071067811865487940, 0.7071067811865463515, 0.000000000000000000 ) ) ;
#126080 = DIRECTION ( 'NONE',  ( 0.7071067811865487940, -0.7071067811865463515, 0.000000000000000000 ) ) ;
#126081 = EDGE_CURVE ( 'NONE', #59855, #108385, #132497, .T. ) ;
#126082 = CARTESIAN_POINT ( 'NONE',  ( 31.41209685856477662, 5.291415217122922066, -3.054999999999995275 ) ) ;
#126083 = CARTESIAN_POINT ( 'NONE',  ( -9.183988606268997046, 28.73617430169793607, 5.000000000000000000 ) ) ;
#126084 = CARTESIAN_POINT ( 'NONE',  ( -36.18398860626899705, 28.73617430169812437, 5.000000000000000000 ) ) ;
#126085 = CARTESIAN_POINT ( 'NONE',  ( 15.83159235450332147, 2.500000000000001332, 0.000000000000000000 ) ) ;
#126086 = CARTESIAN_POINT ( 'NONE',  ( 51.29974487139158867, -27.71228299555242103, 4.000000000000000000 ) ) ;
#126087 = DIRECTION ( 'NONE',  ( -0.000000000000000000, 0.3543493200069153248, 0.9351131265310292928 ) ) ;
#126088 = CARTESIAN_POINT ( 'NONE',  ( 25.93706980810189222, 2.126176841940952134, -7.934999999999993392 ) ) ;
#126089 = CARTESIAN_POINT ( 'NONE',  ( 8.728736474768551190, 5.808823158059031044, -5.808823158059037262 ) ) ;
#126090 = LINE ( 'NONE', #94141, #110680 ) ;
#126091 = CARTESIAN_POINT ( 'NONE',  ( 36.18398860626899705, 28.73617430169812437, 5.000000000000000000 ) ) ;
#126092 = CARTESIAN_POINT ( 'NONE',  ( 2.999999999999975131, -5.527737879153189482, -7.983877177622378696 ) ) ;
#126093 = ORIENTED_EDGE ( 'NONE', *, *, #67747, .F. ) ;
#126095 = EDGE_CURVE ( 'NONE', #25013, #237, #33183, .T. ) ;
#126094 = AXIS2_PLACEMENT_3D ( 'NONE', #4310, #92817, #111733 ) ;
#126096 = ORIENTED_EDGE ( 'NONE', *, *, #116962, .F. ) ;
#126097 = CARTESIAN_POINT ( 'NONE',  ( 90.54166666666665719, -3.975000000000002753, 6.884901960086286188 ) ) ;
#126098 = EDGE_CURVE ( 'NONE', #32288, #114480, #99821, .T. ) ;
#126099 = ORIENTED_EDGE ( 'NONE', *, *, #119091, .T. ) ;
#126100 = ORIENTED_EDGE ( 'NONE', *, *, #32105, .T. ) ;
#126101 = LINE ( 'NONE', #15157, #4004 ) ;
#126102 = CARTESIAN_POINT ( 'NONE',  ( -5.526639036357822832, -5.240707523384232402, 16.25846745537494442 ) ) ;
#126103 = CARTESIAN_POINT ( 'NONE',  ( 57.48921356237308800, -27.52281430457095368, 5.000000000000000000 ) ) ;
#126104 = VERTEX_POINT ( 'NONE', #44781 ) ;
#126105 = PLANE ( 'NONE',  #134329 ) ;
#126106 = DIRECTION ( 'NONE',  ( -0.000000000000000000, 0.3543493200069153248, 0.9351131265310292928 ) ) ;
#126107 = DIRECTION ( 'NONE',  ( -1.000000000000000000, -1.224606353822377258E-16, -0.000000000000000000 ) ) ;
#126108 = CARTESIAN_POINT ( 'NONE',  ( 125.9664974496730281, 3.788224211676681552, -6.458789565855242110 ) ) ;
#126109 = EDGE_CURVE ( 'NONE', #129906, #137014, #41336, .T. ) ;
#126110 = CARTESIAN_POINT ( 'NONE',  ( -14.99451991528749595, 28.92564299267948513, 4.000000000000000000 ) ) ;
#126111 = FACE_OUTER_BOUND ( 'NONE', #28973, .T. ) ;
#126112 = CARTESIAN_POINT ( 'NONE',  ( -12.69999999999998153, 0.4000000000000001887, -2.467792535850613866 ) ) ;
#126113 = DIRECTION ( 'NONE',  ( -0.7071067811865487940, 0.7071067811865463515, -0.000000000000000000 ) ) ;
#126114 = PLANE ( 'NONE',  #13003 ) ;
#126115 = CARTESIAN_POINT ( 'NONE',  ( 9.591592354503321260, 9.902892378096218942E-16, 0.000000000000000000 ) ) ;
#126116 = AXIS2_PLACEMENT_3D ( 'NONE', #106623, #8715, #130570 ) ;
#126117 = EDGE_LOOP ( 'NONE', ( #137715, #71072, #67511, #58508 ) ) ;
#126118 = ORIENTED_EDGE ( 'NONE', *, *, #55618, .F. ) ;
#126119 = CARTESIAN_POINT ( 'NONE',  ( 112.7295968585647756, -6.110000000000000320, -1.637169565754161393 ) ) ;
#126120 = ORIENTED_EDGE ( 'NONE', *, *, #76467, .T. ) ;
#126121 = AXIS2_PLACEMENT_3D ( 'NONE', #352, #44648, #88838 ) ;
#126122 = FILL_AREA_STYLE ('',( #15868 ) ) ;
#126123 = DIRECTION ( 'NONE',  ( -0.5150380749100710309, 1.049727191138606123E-16, -0.8571673007021021196 ) ) ;
#126124 = ORIENTED_EDGE ( 'NONE', *, *, #64343, .T. ) ;
#126125 = PLANE ( 'NONE',  #65342 ) ;
#126126 = DIRECTION ( 'NONE',  ( 0.7071067811865487940, -0.7071067811865463515, 0.000000000000000000 ) ) ;
#126127 = CARTESIAN_POINT ( 'NONE',  ( 104.3287635252314658, 0.000000000000000000, -6.109999999999998543 ) ) ;
#126128 = TOROIDAL_SURFACE ( 'NONE', #21900, 25.00000000000002487, 3.000000000000000000 ) ;
#126129 = ORIENTED_EDGE ( 'NONE', *, *, #98319, .T. ) ;
#126130 = EDGE_CURVE ( 'NONE', #72096, #50134, #30280, .T. ) ;
#126131 = ORIENTED_EDGE ( 'NONE', *, *, #18722, .T. ) ;
#126132 = CARTESIAN_POINT ( 'NONE',  ( -5.999999999999960032, 2.342191155542443948, -5.001666872980071510 ) ) ;
#126133 = SURFACE_SIDE_STYLE ('',( #100277 ) ) ;
#126134 = CARTESIAN_POINT ( 'NONE',  ( 14.27159235450332098, -2.500000000000000444, 3.061616997868384620E-16 ) ) ;
#126135 = VERTEX_POINT ( 'NONE', #97676 ) ;
#126136 = EDGE_LOOP ( 'NONE', ( #74951, #53748, #26143, #23108 ) ) ;
#126137 = ORIENTED_EDGE ( 'NONE', *, *, #50244, .F. ) ;
#126138 = CARTESIAN_POINT ( 'NONE',  ( 32.99999999999977263, 2.342191155542478587, -5.001666872980161216 ) ) ;
#126139 = EDGE_CURVE ( 'NONE', #22356, #90401, #55619, .T. ) ;
#126140 = CARTESIAN_POINT ( 'NONE',  ( 10.12956980810188767, -3.967499999999998028, -6.871911579029511330 ) ) ;
#126141 = ADVANCED_FACE ( 'NONE', ( #64345 ), #131752, .F. ) ;
#126142 = EDGE_CURVE ( 'NONE', #74888, #35249, #9192, .T. ) ;
#126143 = CIRCLE ( 'NONE', #119290, 2.500000000000000888 ) ;
#126144 = VECTOR ( 'NONE', #113517, 1000.000000000000000 ) ;
#126145 = CARTESIAN_POINT ( 'NONE',  ( -34.92500000000001137, -4.298069433178936194, 4.500000000000000888 ) ) ;
#126146 = EDGE_CURVE ( 'NONE', #142842, #20535, #118709, .T. ) ;
#126147 = ORIENTED_EDGE ( 'NONE', *, *, #42513, .F. ) ;
#126149 = ORIENTED_EDGE ( 'NONE', *, *, #104971, .F. ) ;
#126148 = VECTOR ( 'NONE', #28814, 1000.000000000000000 ) ;
#126151 = ADVANCED_FACE ( 'NONE', ( #43313 ), #66498, .T. ) ;
#126150 = CARTESIAN_POINT ( 'NONE',  ( 36.29177708983025497, -15.74070752338412760, 19.73771281079106288 ) ) ;
#126152 = ORIENTED_EDGE ( 'NONE', *, *, #141056, .F. ) ;
#126153 = ORIENTED_EDGE ( 'NONE', *, *, #84953, .T. ) ;
#126154 = EDGE_CURVE ( 'NONE', #58779, #23719, #31714, .T. ) ;
#126155 = CARTESIAN_POINT ( 'NONE',  ( 19.05000000000000071, 3.174999999999997158, 4.000000000000000000 ) ) ;
#126156 = ADVANCED_FACE ( 'NONE', ( #54219 ), #13592, .T. ) ;
#126157 = CARTESIAN_POINT ( 'NONE',  ( 0.000000000000000000, 0.000000000000000000, 0.000000000000000000 ) ) ;
#126158 = ORIENTED_EDGE ( 'NONE', *, *, #136318, .F. ) ;
#126159 = LINE ( 'NONE', #50732, #1979 ) ;
#126160 = DIRECTION ( 'NONE',  ( -0.6830127018922181881, 0.6830127018922202975, -0.2588190451025214056 ) ) ;
#126161 = EDGE_CURVE ( 'NONE', #66092, #98260, #96926, .T. ) ;
#126162 = FACE_BOUND ( 'NONE', #8012, .T. ) ;
#126163 = ORIENTED_EDGE ( 'NONE', *, *, #79435, .T. ) ;
#126164 = CARTESIAN_POINT ( 'NONE',  ( 64.10002705046287019, 5.819803920172570422, 5.819803920172575751 ) ) ;
#126165 = CARTESIAN_POINT ( 'NONE',  ( 30.79289321881324781, 0.7592924766157104211, 5.000000000000000000 ) ) ;
#126166 = FACE_OUTER_BOUND ( 'NONE', #32563, .T. ) ;
#126167 = ORIENTED_EDGE ( 'NONE', *, *, #31923, .T. ) ;
#126168 = CARTESIAN_POINT ( 'NONE',  ( -19.05000000000000071, 3.174999999999997158, 5.000000000000000000 ) ) ;
#126169 = ORIENTED_EDGE ( 'NONE', *, *, #52801, .T. ) ;
#126170 = ORIENTED_EDGE ( 'NONE', *, *, #133281, .F. ) ;
#126171 = ADVANCED_FACE ( 'NONE', ( #141171 ), #130329, .F. ) ;
#126172 = ORIENTED_EDGE ( 'NONE', *, *, #97701, .F. ) ;
#126173 = CARTESIAN_POINT ( 'NONE',  ( 34.76626352523143737, 4.472830434245838482, -4.472830434245837594 ) ) ;
#126174 = ORIENTED_EDGE ( 'NONE', *, *, #112990, .T. ) ;
#126175 = CARTESIAN_POINT ( 'NONE',  ( 78.48921356237309510, -27.52281430457109934, 5.000000000000000000 ) ) ;
#126176 = PLANE ( 'NONE',  #94624 ) ;
#126177 = LINE ( 'NONE', #79861, #105275 ) ;
#126178 = VERTEX_POINT ( 'NONE', #75935 ) ;
#126179 = CARTESIAN_POINT ( 'NONE',  ( -25.39999999999996305, 0.000000000000000000, 0.000000000000000000 ) ) ;
#126180 = SURFACE_STYLE_USAGE ( .BOTH. , #124743 ) ;
#126181 = CARTESIAN_POINT ( 'NONE',  ( 25.49999999999981526, -10.91253812416064406, 4.000000000000000000 ) ) ;
#126182 = CARTESIAN_POINT ( 'NONE',  ( -9.489213562373095101, -27.52281430457062328, 5.000000000000000000 ) ) ;
#126183 = CARTESIAN_POINT ( 'NONE',  ( 44.99451991528749772, 28.92564299267969474, 4.000000000000000000 ) ) ;
#126184 = FACE_OUTER_BOUND ( 'NONE', #89557, .T. ) ;
#126185 = VERTEX_POINT ( 'NONE', #120847 ) ;
#126186 = EDGE_CURVE ( 'NONE', #105516, #142230, #120109, .T. ) ;
#126187 = ORIENTED_EDGE ( 'NONE', *, *, #31470, .F. ) ;
#126188 = ORIENTED_EDGE ( 'NONE', *, *, #124438, .T. ) ;
#126189 = ORIENTED_EDGE ( 'NONE', *, *, #25368, .F. ) ;
#126190 =( NAMED_UNIT ( * ) PLANE_ANGLE_UNIT ( ) SI_UNIT ( $, .RADIAN. ) );
#126191 = VERTEX_POINT ( 'NONE', #32436 ) ;
#126192 = EDGE_CURVE ( 'NONE', #46533, #81376, #120057, .T. ) ;
#126193 = ORIENTED_EDGE ( 'NONE', *, *, #37705, .T. ) ;
#126194 = PLANE ( 'NONE',  #25848 ) ;
#126195 = CARTESIAN_POINT ( 'NONE',  ( 156.1500000000000057, -57.14999999999999147, 49.92499999999997584 ) ) ;
#126196 = LINE ( 'NONE', #5085, #60196 ) ;
#126197 = ORIENTED_EDGE ( 'NONE', *, *, #96192, .T. ) ;
#126198 = FACE_OUTER_BOUND ( 'NONE', #132356, .T. ) ;
#126199 = ORIENTED_EDGE ( 'NONE', *, *, #113946, .F. ) ;
#126200 = CYLINDRICAL_SURFACE ( 'NONE', #25919, 0.5000000000000004441 ) ;
#126201 = VECTOR ( 'NONE', #1951, 1000.000000000000000 ) ;
#126202 = CARTESIAN_POINT ( 'NONE',  ( 15.15612307739229436, -22.22499999999999432, 4.000000000000000000 ) ) ;
#126203 = CARTESIAN_POINT ( 'NONE',  ( -1.828763525231447584, 0.000000000000000000, 7.934999999999990727 ) ) ;
#126204 = EDGE_LOOP ( 'NONE', ( #19777, #91569, #18026, #43836 ) ) ;
#126206 = FACE_OUTER_BOUND ( 'NONE', #106724, .T. ) ;
#126205 = CARTESIAN_POINT ( 'NONE',  ( 105.4954301918981230, 5.291415217122917625, 3.055000000000002380 ) ) ;
#126207 = AXIS2_PLACEMENT_3D ( 'NONE', #101308, #56432, #121616 ) ;
#126209 = ADVANCED_FACE ( 'NONE', ( #109976 ), #10644, .F. ) ;
#126208 =( NAMED_UNIT ( * ) PLANE_ANGLE_UNIT ( ) SI_UNIT ( $, .RADIAN. ) );
#126210 = LINE ( 'NONE', #62395, #81303 ) ;
#126211 = ORIENTED_EDGE ( 'NONE', *, *, #2826, .F. ) ;
#126212 = ORIENTED_EDGE ( 'NONE', *, *, #119931, .F. ) ;
#126213 = PLANE ( 'NONE',  #51843 ) ;
#126214 = ORIENTED_EDGE ( 'NONE', *, *, #20715, .F. ) ;
#126215 = CARTESIAN_POINT ( 'NONE',  ( -9.489213562373095101, -27.52281430457062328, 5.000000000000000000 ) ) ;
#126216 = DIRECTION ( 'NONE',  ( 0.000000000000000000, -0.000000000000000000, -1.000000000000000000 ) ) ;
#126217 = DIRECTION ( 'NONE',  ( -0.000000000000000000, 0.3543493200069153248, 0.9351131265310292928 ) ) ;
#126218 = LINE ( 'NONE', #114603, #49577 ) ;
#126220 = ORIENTED_EDGE ( 'NONE', *, *, #133383, .F. ) ;
#126219 =( BOUNDED_CURVE ( )  B_SPLINE_CURVE ( 2, ( #102527, #124960, #25646, #15447, #114092, #59052, #103203, #125702, #70633, #59736, #103898, #48853, #93053 ),
 .UNSPECIFIED., .F., .T. ) 
 B_SPLINE_CURVE_WITH_KNOTS ( ( 3, 2, 2, 2, 2, 2, 3 ),
 ( 0.2500000000000000000, 0.2583333333333333592, 0.2666666666666666630, 0.2750000000000000222, 0.2833333333333333814, 0.2916666666666667407, 0.3000000000000000444 ),
 .UNSPECIFIED. ) 
 CURVE ( )  GEOMETRIC_REPRESENTATION_ITEM ( )  RATIONAL_B_SPLINE_CURVE ( ( 1.000000000000000000, 0.9659258262890683122, 1.000000000000000000, 0.9659258262890683122, 1.000000000000000000, 0.9659258262890683122, 1.000000000000000000, 0.9659258262890683122, 1.000000000000000000, 0.9659258262890683122, 1.000000000000000000, 0.9659258262890680902, 1.000000000000000222 ) ) 
 REPRESENTATION_ITEM ( '' )  );
#126221 = CARTESIAN_POINT ( 'NONE',  ( 28.49999999999979750, -14.70932175296475108, -11.46312253303843853 ) ) ;
#126222 = AXIS2_PLACEMENT_3D ( 'NONE', #66696, #132702, #46408 ) ;
#126223 = EDGE_CURVE ( 'NONE', #20803, #115452, #46930, .T. ) ;
#126224 = CARTESIAN_POINT ( 'NONE',  ( 30.18398860626900060, 28.73617430169808173, 5.000000000000000000 ) ) ;
#126225 = CARTESIAN_POINT ( 'NONE',  ( -33.48921356237309510, -27.52281430457078670, 5.000000000000000000 ) ) ;
#126226 = ORIENTED_EDGE ( 'NONE', *, *, #80186, .F. ) ;
#126227 = DIRECTION ( 'NONE',  ( 0.7071067811865487940, 0.7071067811865463515, -0.000000000000000000 ) ) ;
#126228 = CARTESIAN_POINT ( 'NONE',  ( -21.48921356237309155, -27.52281430457070499, 5.000000000000000000 ) ) ;
#126229 = ORIENTED_EDGE ( 'NONE', *, *, #44627, .F. ) ;
#126232 = EDGE_CURVE ( 'NONE', #74261, #107142, #24401, .T. ) ;
#126231 = VERTEX_POINT ( 'NONE', #80242 ) ;
#126230 = PLANE ( 'NONE',  #113459 ) ;
#126233 = EDGE_LOOP ( 'NONE', ( #130359, #104763, #141313, #25833 ) ) ;
#126234 = CARTESIAN_POINT ( 'NONE',  ( 34.92499999999998295, -12.28150956279560369, 4.759050581649325373 ) ) ;
#126235 = DIRECTION ( 'NONE',  ( 1.000000000000000000, 0.000000000000000000, 0.000000000000000000 ) ) ;
#126236 = ORIENTED_EDGE ( 'NONE', *, *, #126130, .F. ) ;
#126237 = CARTESIAN_POINT ( 'NONE',  ( 34.92499999999998295, 20.82781275693360712, 4.470553524000301593 ) ) ;
#126238 = DIRECTION ( 'NONE',  ( 0.000000000000000000, 0.000000000000000000, 1.000000000000000000 ) ) ;
#126239 = AXIS2_PLACEMENT_3D ( 'NONE', #75055, #142436, #96044 ) ;
#126240 = VECTOR ( 'NONE', #46820, 1000.000000000000000 ) ;
#126241 = LINE ( 'NONE', #141390, #131819 ) ;
#126242 = ORIENTED_EDGE ( 'NONE', *, *, #66422, .T. ) ;
#126243 = AXIS2_PLACEMENT_3D ( 'NONE', #108306, #8976, #136511 ) ;
#126244 = DIRECTION ( 'NONE',  ( -0.7071067811865487940, 0.7071067811865463515, 0.000000000000000000 ) ) ;
#126246 = AXIS2_PLACEMENT_3D ( 'NONE', #94167, #49288, #139859 ) ;
#126245 = DIRECTION ( 'NONE',  ( -0.7071067811865486830, -0.7071067811865464625, -0.000000000000000000 ) ) ;
#126247 = LINE ( 'NONE', #103743, #14285 ) ;
#126248 = LINE ( 'NONE', #81337, #100346 ) ;
#126249 = FACE_OUTER_BOUND ( 'NONE', #1457, .T. ) ;
#126250 = CARTESIAN_POINT ( 'NONE',  ( 2.671830600776458287, -12.74070752338415247, 4.000000000000000000 ) ) ;
#126251 = LINE ( 'NONE', #104480, #142603 ) ;
#126252 = ORIENTED_EDGE ( 'NONE', *, *, #105908, .T. ) ;
#126253 = ORIENTED_EDGE ( 'NONE', *, *, #142809, .T. ) ;
#126254 = EDGE_LOOP ( 'NONE', ( #84291, #119791, #108230, #103329 ) ) ;
#126255 = CARTESIAN_POINT ( 'NONE',  ( 124.8125000000000142, 5.819803920172571310, 5.819803920172575751 ) ) ;
#126256 = EDGE_CURVE ( 'NONE', #143315, #139444, #57780, .T. ) ;
#126257 = VERTEX_POINT ( 'NONE', #113536 ) ;
#126258 = VERTEX_POINT ( 'NONE', #12794 ) ;
#126259 = ORIENTED_EDGE ( 'NONE', *, *, #113036, .F. ) ;
#126260 = FACE_OUTER_BOUND ( 'NONE', #190, .T. ) ;
#126261 = CARTESIAN_POINT ( 'NONE',  ( -5.510786437626906675, -27.52281430457051314, 5.000000000000000000 ) ) ;
#126262 = ORIENTED_EDGE ( 'NONE', *, *, #58459, .F. ) ;
#126263 = DIRECTION ( 'NONE',  ( -0.3543493200069162685, -0.000000000000000000, -0.9351131265310288487 ) ) ;
#126264 = CARTESIAN_POINT ( 'NONE',  ( -34.92500000000001137, 22.22500000000000142, 4.000000000000000000 ) ) ;
#126265 = CARTESIAN_POINT ( 'NONE',  ( 29.99451991528749417, 28.92564299267958816, 4.000000000000000000 ) ) ;
#126266 = CARTESIAN_POINT ( 'NONE',  ( 109.2295968585647614, -6.110000000000000320, -1.637169565754161393 ) ) ;
#126267 = EDGE_LOOP ( 'NONE', ( #101545, #77334, #17695, #68763 ) ) ;
#126268 = ADVANCED_FACE ( 'NONE', ( #125139 ), #69359, .T. ) ;
#126269 = DIRECTION ( 'NONE',  ( -0.000000000000000000, 0.3543493200069153248, 0.9351131265310292928 ) ) ;
#126270 = DIRECTION ( 'NONE',  ( 0.7071067811865487940, -0.7071067811865463515, 0.000000000000000000 ) ) ;
#126271 = LINE ( 'NONE', #129115, #84427 ) ;
#126272 = DIRECTION ( 'NONE',  ( 0.7071067811865487940, -0.7071067811865463515, 0.000000000000000000 ) ) ;
#126273 = CARTESIAN_POINT ( 'NONE',  ( 48.18398860626899705, 28.73617430169820608, 5.000000000000000000 ) ) ;
#126274 = CARTESIAN_POINT ( 'NONE',  ( 149.2199999999997999, -3.180000000000061444, -34.92499999999998295 ) ) ;
#126275 = CARTESIAN_POINT ( 'NONE',  ( 40.18336038379622721, -2.130196079827426203, 7.949999999999997513 ) ) ;
#126276 = CARTESIAN_POINT ( 'NONE',  ( -18.48921356237309510, -27.52281430457068367, 5.000000000000000000 ) ) ;
#126277 = CARTESIAN_POINT ( 'NONE',  ( 127.0000000000000000, -4.017717506652945580, -5.045834523320674059 ) ) ;
#126278 = VERTEX_POINT ( 'NONE', #4016 ) ;
#126279 = ORIENTED_EDGE ( 'NONE', *, *, #2727, .T. ) ;
#126280 = CARTESIAN_POINT ( 'NONE',  ( 35.41666666666666430, -6.884901960086287076, -3.975000000000000977 ) ) ;
#126281 = EDGE_LOOP ( 'NONE', ( #71186, #35161, #142277, #53361 ) ) ;
#126282 = VERTEX_POINT ( 'NONE', #57067 ) ;
#126283 = CARTESIAN_POINT ( 'NONE',  ( -34.49999999999975842, 15.43112307739202649, 4.000000000000000000 ) ) ;
#126284 = CARTESIAN_POINT ( 'NONE',  ( -29.99451991528749417, 28.92564299267958816, 4.000000000000000000 ) ) ;
#126285 = LINE ( 'NONE', #120657, #115528 ) ;
#126286 = EDGE_LOOP ( 'NONE', ( #44013, #52112, #19557, #134762, #43135, #9498 ) ) ;
#126287 = PLANE ( 'NONE',  #6242 ) ;
#126288 = FILL_AREA_STYLE ('',( #71939 ) ) ;
#126289 = CARTESIAN_POINT ( 'NONE',  ( -14.01088028653938444, -22.02621442084248216, 4.990779571109223767 ) ) ;
#126290 = CARTESIAN_POINT ( 'NONE',  ( 32.81293019189809002, -1.637169565754159617, -6.110000000000001208 ) ) ;
#126291 = ORIENTED_EDGE ( 'NONE', *, *, #95191, .F. ) ;
#126292 = CARTESIAN_POINT ( 'NONE',  ( 34.49999999999975842, -12.08601207473285832, -10.46905243149102382 ) ) ;
#126293 = ORIENTED_EDGE ( 'NONE', *, *, #128570, .F. ) ;
#126294 = DIRECTION ( 'NONE',  ( -0.000000000000000000, -1.000000000000000000, -0.000000000000000000 ) ) ;
#126295 = LINE ( 'NONE', #50177, #124062 ) ;
#126296 = CARTESIAN_POINT ( 'NONE',  ( 0.2569208697893814453, 4.202752102959690472E-16, 0.000000000000000000 ) ) ;
#126297 = DIRECTION ( 'NONE',  ( 1.000000000000000000, 0.000000000000000000, 0.000000000000000000 ) ) ;
#126298 = ORIENTED_EDGE ( 'NONE', *, *, #68226, .F. ) ;
#126299 = EDGE_LOOP ( 'NONE', ( #55388, #1948, #4304, #19817, #130663 ) ) ;
#126300 = CARTESIAN_POINT ( 'NONE',  ( -54.29974487139159578, -27.71228299555243879, 4.000000000000000000 ) ) ;
#126301 = DIRECTION ( 'NONE',  ( -0.6830127018922180770, -0.6830127018922204085, -0.2588190451025214056 ) ) ;
#126302 = PLANE ( 'NONE',  #1394 ) ;
#126303 = VECTOR ( 'NONE', #101135, 999.9999999999998863 ) ;
#126304 = ADVANCED_FACE ( 'NONE', ( #123744 ), #33869, .F. ) ;
#126305 = CARTESIAN_POINT ( 'NONE',  ( 49.34959685856478728, 6.109999999999996767, 1.637169565754163836 ) ) ;
#126307 = EDGE_CURVE ( 'NONE', #136490, #70384, #36021, .T. ) ;
#126306 = ORIENTED_EDGE ( 'NONE', *, *, #5497, .T. ) ;
#126308 = AXIS2_PLACEMENT_3D ( 'NONE', #59811, #103980, #36604 ) ;
#126309 = DIRECTION ( 'NONE',  ( 0.7071067811865486830, -0.7071067811865464625, -0.000000000000000000 ) ) ;
#126311 = EDGE_CURVE ( 'NONE', #21613, #127309, #78798, .T. ) ;
#126310 = CARTESIAN_POINT ( 'NONE',  ( 23.78840764549667597, 9.139736423841732040E-16, 0.000000000000000000 ) ) ;
#126312 = ORIENTED_EDGE ( 'NONE', *, *, #71326, .T. ) ;
#126313 = EDGE_LOOP ( 'NONE', ( #140954, #121247, #129392, #30301, #143399, #35857 ) ) ;
#126314 = PLANE ( 'NONE',  #2984 ) ;
#126315 = ORIENTED_EDGE ( 'NONE', *, *, #14087, .T. ) ;
#126316 = EDGE_CURVE ( 'NONE', #51626, #25547, #16082, .T. ) ;
#126317 = VECTOR ( 'NONE', #91152, 1000.000000000000000 ) ;
#126318 = CARTESIAN_POINT ( 'NONE',  ( -54.48921356237310221, -27.52281430457093236, 5.000000000000000000 ) ) ;
#126319 = ORIENTED_EDGE ( 'NONE', *, *, #11052, .T. ) ;
#126320 = CARTESIAN_POINT ( 'NONE',  ( 25.49999999999982947, -2.173586137069107860, -4.605770156576055818 ) ) ;
#126321 = EDGE_CURVE ( 'NONE', #27882, #2711, #68648, .T. ) ;
#126322 = FACE_BOUND ( 'NONE', #12396, .T. ) ;
#126323 = EDGE_CURVE ( 'NONE', #22070, #82317, #14237, .T. ) ;
#126324 = CARTESIAN_POINT ( 'NONE',  ( 25.19159235450331735, 9.902892378096218942E-16, 0.000000000000000000 ) ) ;
#126325 = DIRECTION ( 'NONE',  ( 0.6830127018922181881, 0.6830127018922202975, -0.2588190451025214056 ) ) ;
#126326 = CARTESIAN_POINT ( 'NONE',  ( 19.41972383043609440, 4.584330080086930965E-16, 0.000000000000000000 ) ) ;
#126328 = VERTEX_POINT ( 'NONE', #112145 ) ;
#126327 = DIRECTION ( 'NONE',  ( 0.3543493200069162685, -0.000000000000000000, -0.9351131265310288487 ) ) ;
#126329 = CARTESIAN_POINT ( 'NONE',  ( 63.29974487139158867, -27.71228299555250274, 4.000000000000000000 ) ) ;
#126330 = EDGE_CURVE ( 'NONE', #138900, #85225, #122265, .T. ) ;
#126331 = VECTOR ( 'NONE', #1266, 999.9999999999998863 ) ;
#126332 = VERTEX_POINT ( 'NONE', #58522 ) ;
#126334 = ORIENTED_EDGE ( 'NONE', *, *, #39238, .T. ) ;
#126333 = VECTOR ( 'NONE', #116843, 1000.000000000000000 ) ;
#126335 = CARTESIAN_POINT ( 'NONE',  ( 68.16209685856478018, -5.291415217122919401, 3.054999999999997939 ) ) ;
#126336 = VERTEX_POINT ( 'NONE', #34577 ) ;
#126337 = VECTOR ( 'NONE', #11843, 1000.000000000000000 ) ;
#126338 = CARTESIAN_POINT ( 'NONE',  ( -27.49816348513939701, -17.24070752338409918, 8.407044977365289995 ) ) ;
#126339 = CARTESIAN_POINT ( 'NONE',  ( 15.19713381108422290, 7.733989266307781385, 4.000000000000000000 ) ) ;
#126340 = EDGE_LOOP ( 'NONE', ( #43130, #118267, #104945, #112569 ) ) ;
#126341 = CARTESIAN_POINT ( 'NONE',  ( -9.183988606268997046, 28.73617430169793607, 5.000000000000000000 ) ) ;
#126342 = EDGE_CURVE ( 'NONE', #139694, #99063, #102694, .T. ) ;
#126343 = CYLINDRICAL_SURFACE ( 'NONE', #66402, 0.5000000000000001110 ) ;
#126344 = DIRECTION ( 'NONE',  ( 1.000000000000000000, 0.000000000000000000, 0.000000000000000000 ) ) ;
#126345 = DIRECTION ( 'NONE',  ( 0.6830127018922181881, 0.6830127018922202975, -0.2588190451025214056 ) ) ;
#126346 = CARTESIAN_POINT ( 'NONE',  ( 17.35416666666666430, 1.633150327867695095, 6.094999999999988205 ) ) ;
#126347 = ORIENTED_EDGE ( 'NONE', *, *, #58409, .T. ) ;
#126348 = ADVANCED_FACE ( 'NONE', ( #67201 ), #123012, .T. ) ;
#126349 = ORIENTED_EDGE ( 'NONE', *, *, #71290, .T. ) ;
#126350 = DIRECTION ( 'NONE',  ( 0.7071067811865486830, -0.7071067811865464625, -0.000000000000000000 ) ) ;
#126351 = FACE_OUTER_BOUND ( 'NONE', #98844, .T. ) ;
#126352 = ORIENTED_EDGE ( 'NONE', *, *, #45968, .F. ) ;
#126353 = ORIENTED_EDGE ( 'NONE', *, *, #53650, .F. ) ;
#126354 = ORIENTED_EDGE ( 'NONE', *, *, #89467, .T. ) ;
#126355 = DIRECTION ( 'NONE',  ( 0.000000000000000000, 0.000000000000000000, 1.000000000000000000 ) ) ;
#126356 = CARTESIAN_POINT ( 'NONE',  ( 30.60416666666665719, 2.130196079827422206, 7.950000000000001954 ) ) ;
#126357 = ORIENTED_EDGE ( 'NONE', *, *, #51031, .T. ) ;
#126358 = LINE ( 'NONE', #69888, #57905 ) ;
#126359 = CARTESIAN_POINT ( 'NONE',  ( 27.29974487139158512, -27.71228299555225405, 4.000000000000000000 ) ) ;
#126360 = CARTESIAN_POINT ( 'NONE',  ( 4.442069808101886785, 7.934999999999993392, 2.126176841940951689 ) ) ;
#126361 = LINE ( 'NONE', #115450, #61145 ) ;
#126362 = ORIENTED_EDGE ( 'NONE', *, *, #41132, .T. ) ;
#126363 = CARTESIAN_POINT ( 'NONE',  ( 12.79289321881337038, -8.240707523384196875, 5.000000000000000000 ) ) ;
#126365 = EDGE_CURVE ( 'NONE', #83058, #83926, #111398, .T. ) ;
#126364 = CARTESIAN_POINT ( 'NONE',  ( -10.49999999999992539, -8.568876922607726598, 4.000000000000000000 ) ) ;
#126366 = DIRECTION ( 'NONE',  ( -0.7071067811865487940, 0.7071067811865463515, -0.000000000000000000 ) ) ;
#126368 = ORIENTED_EDGE ( 'NONE', *, *, #124702, .T. ) ;
#126367 = DIRECTION ( 'NONE',  ( -0.7071067811865487940, 0.7071067811865463515, 0.000000000000000000 ) ) ;
#126369 = CARTESIAN_POINT ( 'NONE',  ( -31.92499999999997584, -3.270000000000012452, -37.00000000000000000 ) ) ;
#126370 = ORIENTED_EDGE ( 'NONE', *, *, #6308, .T. ) ;
#126371 = CARTESIAN_POINT ( 'NONE',  ( -29.39513766812461171, 21.75929247661548516, 21.32995629748192812 ) ) ;
#126372 = CARTESIAN_POINT ( 'NONE',  ( 57.48921356237308800, -27.52281430457095368, 5.000000000000000000 ) ) ;
#126373 = DIRECTION ( 'NONE',  ( -0.000000000000000000, 0.000000000000000000, 1.000000000000000000 ) ) ;
#126374 = ORIENTED_EDGE ( 'NONE', *, *, #129355, .T. ) ;
#126375 = PRESENTATION_STYLE_ASSIGNMENT (( #63119 ) ) ;
#126376 = EDGE_CURVE ( 'NONE', #116464, #35767, #12085, .T. ) ;
#126377 = DIRECTION ( 'NONE',  ( -0.6830127018922180770, -0.6830127018922204085, -0.2588190451025213501 ) ) ;
#126378 = CARTESIAN_POINT ( 'NONE',  ( 34.75611968250419181, 2.812934254707362580, 4.955485411084882053 ) ) ;
#126379 = DIRECTION ( 'NONE',  ( -0.6830127018922181881, 0.6830127018922202975, -0.2588190451025214056 ) ) ;
#126380 = ORIENTED_EDGE ( 'NONE', *, *, #6295, .T. ) ;
#126381 = CARTESIAN_POINT ( 'NONE',  ( 65.99451991528749772, 28.92564299267984396, 4.000000000000000000 ) ) ;
#126382 = DIRECTION ( 'NONE',  ( 0.7071067811865487940, 0.7071067811865463515, -0.000000000000000000 ) ) ;
#126383 = CARTESIAN_POINT ( 'NONE',  ( 20.66840764549667497, 9.139736423841732040E-16, 0.000000000000000000 ) ) ;
#126384 = DIRECTION ( 'NONE',  ( -0.000000000000000000, 1.000000000000000000, -0.000000000000000000 ) ) ;
#126385 = LINE ( 'NONE', #84354, #131760 ) ;
#126387 = EDGE_CURVE ( 'NONE', #120628, #91989, #116416, .T. ) ;
#126386 = VERTEX_POINT ( 'NONE', #138172 ) ;
#126388 = EDGE_CURVE ( 'NONE', #8796, #25047, #60652, .T. ) ;
#126389 = VERTEX_POINT ( 'NONE', #93936 ) ;
#126390 = DIRECTION ( 'NONE',  ( 0.000000000000000000, -1.000000000000000000, 0.000000000000000000 ) ) ;
#126391 = FACE_OUTER_BOUND ( 'NONE', #30786, .T. ) ;
#126392 =( BOUNDED_CURVE ( )  B_SPLINE_CURVE ( 3, ( #93150, #72880, #117035, #108996 ),
 .UNSPECIFIED., .F., .T. ) 
 B_SPLINE_CURVE_WITH_KNOTS ( ( 4, 4 ),
 ( 2.001653308786167429, 3.503810798801451742 ),
 .UNSPECIFIED. ) 
 CURVE ( )  GEOMETRIC_REPRESENTATION_ITEM ( )  RATIONAL_B_SPLINE_CURVE ( ( 1.000000000000000000, 0.8206354192515235013, 0.8206354192515235013, 1.000000000000000000 ) ) 
 REPRESENTATION_ITEM ( '' )  );
#126393 = CARTESIAN_POINT ( 'NONE',  ( 9.457903141435219041, 6.871911579029515771, 3.967499999999989146 ) ) ;
#126394 = DIRECTION ( 'NONE',  ( -0.000000000000000000, 0.000000000000000000, 1.000000000000000000 ) ) ;
#126395 = LINE ( 'NONE', #69933, #94720 ) ;
#126396 = CARTESIAN_POINT ( 'NONE',  ( -53.99451991528749062, 28.92564299267975869, 4.000000000000000000 ) ) ;
#126397 = DIRECTION ( 'NONE',  ( -0.3543493200069162685, -0.000000000000000000, -0.9351131265310288487 ) ) ;
#126398 = VECTOR ( 'NONE', #49668, 1000.000000000000000 ) ;
#126399 = EDGE_LOOP ( 'NONE', ( #126169, #117780, #56850, #102134 ) ) ;
#126400 = DIRECTION ( 'NONE',  ( -0.7071067811865487940, 0.7071067811865463515, 0.000000000000000000 ) ) ;
#126401 = LINE ( 'NONE', #115489, #28438 ) ;
#126402 = CARTESIAN_POINT ( 'NONE',  ( 0.000000000000000000, 0.000000000000000000, 5.000000000000000000 ) ) ;
#126403 = CARTESIAN_POINT ( 'NONE',  ( 51.39126352523145158, -4.472830434245839371, -4.472830434245839371 ) ) ;
#126404 = CARTESIAN_POINT ( 'NONE',  ( -6.640000000000001457, -34.51840020119762187, 17.97447928118982929 ) ) ;
#126405 = ORIENTED_EDGE ( 'NONE', *, *, #125989, .T. ) ;
#126406 = DIRECTION ( 'NONE',  ( 0.7071067811865487940, -0.7071067811865463515, 0.000000000000000000 ) ) ;
#126407 = EDGE_CURVE ( 'NONE', #31083, #23744, #124755, .T. ) ;
#126408 = VERTEX_POINT ( 'NONE', #28711 ) ;
#126409 = AXIS2_PLACEMENT_3D ( 'NONE', #345, #47498, #24268 ) ;
#126410 = ORIENTED_EDGE ( 'NONE', *, *, #15546, .T. ) ;
#126411 = CARTESIAN_POINT ( 'NONE',  ( 3.328169399223507519, -15.74070752338412404, 4.000000000000000000 ) ) ;
#126412 = LINE ( 'NONE', #136573, #99313 ) ;
#126413 = PLANE ( 'NONE',  #9433 ) ;
#126414 = DIRECTION ( 'NONE',  ( 0.6830127018922180770, -0.6830127018922204085, -0.2588190451025213501 ) ) ;
#126415 = ADVANCED_FACE ( 'NONE', ( #82373 ), #62766, .F. ) ;
#126416 = LINE ( 'NONE', #16202, #92738 ) ;
#126417 = CARTESIAN_POINT ( 'NONE',  ( 11.52083333333333393, -6.094999999999989981, -1.633150327867689322 ) ) ;
#126418 = EDGE_LOOP ( 'NONE', ( #127108, #75250, #118297, #7631 ) ) ;
#126419 = ADVANCED_FACE ( 'NONE', ( #104816 ), #48296, .F. ) ;
#126420 = CARTESIAN_POINT ( 'NONE',  ( -42.48921356237308800, -27.52281430457085065, 5.000000000000000000 ) ) ;
#126421 = DIRECTION ( 'NONE',  ( 0.000000000000000000, -0.000000000000000000, -1.000000000000000000 ) ) ;
#126422 = CARTESIAN_POINT ( 'NONE',  ( 36.85005128541002506, -8.240707523384189770, 17.25253755692247637 ) ) ;
#126423 = CARTESIAN_POINT ( 'NONE',  ( 6.489213562373093325, -27.52281430457059841, 5.000000000000000000 ) ) ;
#126424 = DIRECTION ( 'NONE',  ( -1.000000000000000000, -1.224606353822377258E-16, -0.000000000000000000 ) ) ;
#126425 = CARTESIAN_POINT ( 'NONE',  ( 66.43336038379622721, 2.130196079827431532, -7.949999999999997513 ) ) ;
#126426 = VECTOR ( 'NONE', #97369, 1000.000000000000000 ) ;
#126427 = DIRECTION ( 'NONE',  ( -0.3543493200069162685, -0.000000000000000000, -0.9351131265310288487 ) ) ;
#126428 = EDGE_LOOP ( 'NONE', ( #111568, #116838, #71876, #31333 ) ) ;
#126429 = ORIENTED_EDGE ( 'NONE', *, *, #64358, .F. ) ;
#126430 = CARTESIAN_POINT ( 'NONE',  ( 61.37500000000000000, 7.950000000000000178, 1.460391307983218535E-15 ) ) ;
#126431 = LINE ( 'NONE', #135217, #23920 ) ;
#126432 = AXIS2_PLACEMENT_3D ( 'NONE', #96458, #95055, #29797 ) ;
#126433 = PLANE ( 'NONE',  #16104 ) ;
#126434 = CARTESIAN_POINT ( 'NONE',  ( 3.328169399223507519, -9.740707523384187994, 4.000000000000000000 ) ) ;
#126435 = CONICAL_SURFACE ( 'NONE', #43161, 2.552699999999994418, 1.029744258676651869 ) ;
#126436 = ORIENTED_EDGE ( 'NONE', *, *, #99995, .F. ) ;
#126437 = ADVANCED_FACE ( 'NONE', ( #126552 ), #84521, .T. ) ;
#126438 = CARTESIAN_POINT ( 'NONE',  ( 127.0000000000000568, -4.172191364199829167, -4.786994800550450790 ) ) ;
#126439 = CARTESIAN_POINT ( 'NONE',  ( 17.99451991528748351, 28.92564299267950645, 4.000000000000000000 ) ) ;
#126440 = CARTESIAN_POINT ( 'NONE',  ( 57.45876352523143993, 0.000000000000000000, -6.110000000000001208 ) ) ;
#126441 = CARTESIAN_POINT ( 'NONE',  ( -78.48921356237309510, -27.52281430457109934, 5.000000000000000000 ) ) ;
#126442 = VERTEX_POINT ( 'NONE', #117801 ) ;
#126443 = ORIENTED_EDGE ( 'NONE', *, *, #84173, .T. ) ;
#126444 = DIRECTION ( 'NONE',  ( -0.7071067811865486830, -0.7071067811865464625, 0.000000000000000000 ) ) ;
#126445 = CARTESIAN_POINT ( 'NONE',  ( 28.49999999999979750, -6.839392718269103888, -8.480912228396153552 ) ) ;
#126446 = DIRECTION ( 'NONE',  ( -0.000000000000000000, 0.000000000000000000, 1.000000000000000000 ) ) ;
#126447 = CARTESIAN_POINT ( 'NONE',  ( -63.48921356237309510, -27.52281430457099631, 5.000000000000000000 ) ) ;
#126448 = CARTESIAN_POINT ( 'NONE',  ( 23.42930023009006391, -22.22500000000000142, 27.11262575547401354 ) ) ;
#126450 = ORIENTED_EDGE ( 'NONE', *, *, #62774, .T. ) ;
#126449 = DIRECTION ( 'NONE',  ( -0.7071067811865487940, 0.7071067811865463515, -0.000000000000000000 ) ) ;
#126451 = LINE ( 'NONE', #105412, #106237 ) ;
#126452 = DIRECTION ( 'NONE',  ( 0.000000000000000000, 0.000000000000000000, 1.000000000000000000 ) ) ;
#126453 = LINE ( 'NONE', #127922, #47176 ) ;
#126454 = CARTESIAN_POINT ( 'NONE',  ( 8.292986735706890045, -21.74070752338406365, 4.999753212805221558 ) ) ;
#126455 = EDGE_LOOP ( 'NONE', ( #49408, #100230, #87557 ) ) ;
#126456 = EDGE_CURVE ( 'NONE', #90217, #126591, #39588, .T. ) ;
#126457 = ORIENTED_EDGE ( 'NONE', *, *, #115791, .F. ) ;
#126458 = PLANE ( 'NONE',  #140278 ) ;
#126459 = EDGE_CURVE ( 'NONE', #16751, #2806, #109695, .T. ) ;
#126460 = CARTESIAN_POINT ( 'NONE',  ( 19.93618820137057668, -0.2700000000508058218, -36.99999999997771738 ) ) ;
#126461 = CARTESIAN_POINT ( 'NONE',  ( -0.3281693992235254487, 2.259292476615696099, 4.000000000000000000 ) ) ;
#126462 = PLANE ( 'NONE',  #140404 ) ;
#126463 = CARTESIAN_POINT ( 'NONE',  ( -34.75611968250420603, 14.81293425470721736, 4.955485411084898040 ) ) ;
#126464 = ORIENTED_EDGE ( 'NONE', *, *, #5743, .T. ) ;
#126465 = ORIENTED_EDGE ( 'NONE', *, *, #91607, .T. ) ;
#126466 = CIRCLE ( 'NONE', #3703, 2.500000000000000444 ) ;
#126467 = DIRECTION ( 'NONE',  ( 0.6830127018922180770, -0.6830127018922204085, -0.2588190451025213501 ) ) ;
#126468 = FILL_AREA_STYLE_COLOUR ( '', #118531 ) ;
#126469 = ORIENTED_EDGE ( 'NONE', *, *, #71045, .T. ) ;
#126470 = EDGE_CURVE ( 'NONE', #101316, #6765, #81674, .T. ) ;
#126471 = EDGE_CURVE ( 'NONE', #91252, #130600, #83822, .T. ) ;
#126472 = ORIENTED_EDGE ( 'NONE', *, *, #58767, .F. ) ;
#126473 = FACE_OUTER_BOUND ( 'NONE', #1012, .T. ) ;
#126474 = ORIENTED_EDGE ( 'NONE', *, *, #26801, .F. ) ;
#126475 = FACE_OUTER_BOUND ( 'NONE', #75033, .T. ) ;
#126477 = VECTOR ( 'NONE', #112001, 1000.000000000000000 ) ;
#126476 = LINE ( 'NONE', #16262, #79545 ) ;
#126478 = EDGE_CURVE ( 'NONE', #19726, #82267, #59905, .T. ) ;
#126479 = FACE_BOUND ( 'NONE', #142589, .T. ) ;
#126480 = EDGE_CURVE ( 'NONE', #115809, #16774, #70771, .T. ) ;
#126481 = FACE_OUTER_BOUND ( 'NONE', #138196, .T. ) ;
#126482 = LINE ( 'NONE', #82302, #125377 ) ;
#126483 = DIRECTION ( 'NONE',  ( -0.000000000000000000, 0.000000000000000000, 1.000000000000000000 ) ) ;
#126484 = CARTESIAN_POINT ( 'NONE',  ( 23.51078643762690490, -27.52281430457038880, 5.000000000000000000 ) ) ;
#126486 = EDGE_CURVE ( 'NONE', #99762, #129679, #83077, .T. ) ;
#126485 = PRODUCT_CONTEXT ( 'NONE', #127200, 'mechanical' ) ;
#126488 = ORIENTED_EDGE ( 'NONE', *, *, #112206, .F. ) ;
#126487 = PRESENTATION_LAYER_ASSIGNMENT (  '', '', ( #89451 ) ) ;
#126489 = ORIENTED_EDGE ( 'NONE', *, *, #87092, .F. ) ;
#126490 = CARTESIAN_POINT ( 'NONE',  ( 96.89126352523143737, -4.472830434245838482, -4.472830434245838482 ) ) ;
#126491 = VERTEX_POINT ( 'NONE', #139632 ) ;
#126492 = VECTOR ( 'NONE', #94027, 1000.000000000000000 ) ;
#126493 = CARTESIAN_POINT ( 'NONE',  ( 53.99451991528749062, 28.92564299267975869, 4.000000000000000000 ) ) ;
#126494 = LINE ( 'NONE', #81607, #113824 ) ;
#126495 = EDGE_CURVE ( 'NONE', #3029, #42047, #40312, .T. ) ;
#126496 = LINE ( 'NONE', #83760, #117279 ) ;
#126497 = DIRECTION ( 'NONE',  ( -0.6830127018922180770, -0.6830127018922204085, -0.2588190451025213501 ) ) ;
#126498 = EDGE_LOOP ( 'NONE', ( #94735, #25520, #6587, #126949, #72635 ) ) ;
#126499 = CARTESIAN_POINT ( 'NONE',  ( 47.99451991528749062, 28.92564299267971251, 4.000000000000000000 ) ) ;
#126500 = LINE ( 'NONE', #61318, #142654 ) ;
#126501 = VECTOR ( 'NONE', #101906, 1000.000000000000000 ) ;
#126502 = CARTESIAN_POINT ( 'NONE',  ( -18.81246187583933960, -22.22500000000000142, 4.000000000000000000 ) ) ;
#126504 = LINE ( 'NONE', #60594, #130727 ) ;
#126503 = CARTESIAN_POINT ( 'NONE',  ( 11.99451991528749417, 28.92564299267946382, 4.000000000000000000 ) ) ;
#126505 = CARTESIAN_POINT ( 'NONE',  ( -26.99451991528749417, 28.92564299267956685, 4.000000000000000000 ) ) ;
#126506 = CARTESIAN_POINT ( 'NONE',  ( 181.1391930515557931, -48.09618305010687322, -37.50858089739956824 ) ) ;
#126507 = ADVANCED_FACE ( 'NONE', ( #33014 ), #131580, .T. ) ;
#126508 = LINE ( 'NONE', #139583, #81651 ) ;
#126509 = EDGE_LOOP ( 'NONE', ( #72651, #61759, #80128, #62549 ) ) ;
#126510 = CARTESIAN_POINT ( 'NONE',  ( 17.22560490425083657, 3.821174125832445049E-16, 0.000000000000000000 ) ) ;
#126511 = DIRECTION ( 'NONE',  ( 0.000000000000000000, 0.000000000000000000, -1.000000000000000000 ) ) ;
#126512 = VERTEX_POINT ( 'NONE', #109819 ) ;
#126514 = ORIENTED_EDGE ( 'NONE', *, *, #99440, .F. ) ;
#126513 = VECTOR ( 'NONE', #17693, 1000.000000000000000 ) ;
#126515 = ORIENTED_EDGE ( 'NONE', *, *, #113838, .T. ) ;
#126516 = EDGE_CURVE ( 'NONE', #96047, #127352, #75781, .T. ) ;
#126517 = CARTESIAN_POINT ( 'NONE',  ( 45.79209685856476852, -5.291415217122921177, 3.054999999999999272 ) ) ;
#126518 = EDGE_CURVE ( 'NONE', #50562, #18398, #120671, .T. ) ;
#126519 = ORIENTED_EDGE ( 'NONE', *, *, #47975, .T. ) ;
#126520 = VECTOR ( 'NONE', #25195, 1000.000000000000114 ) ;
#126521 = AXIS2_PLACEMENT_3D ( 'NONE', #48209, #59132, #14854 ) ;
#126522 = EDGE_CURVE ( 'NONE', #119795, #72522, #121397, .T. ) ;
#126523 = CIRCLE ( 'NONE', #142694, 17.45000000000002061 ) ;
#126524 = CARTESIAN_POINT ( 'NONE',  ( 16.52497294953710494, -4.461849672132299993, -4.461849672132299105 ) ) ;
#126525 = CARTESIAN_POINT ( 'NONE',  ( -9.989884667592379586, 9.469783904273665343, -27.25938507612927708 ) ) ;
#126526 = ORIENTED_EDGE ( 'NONE', *, *, #87394, .T. ) ;
#126527 = DIRECTION ( 'NONE',  ( -0.7071067811865486830, -0.7071067811865464625, 0.000000000000000000 ) ) ;
#126528 = VERTEX_POINT ( 'NONE', #22079 ) ;
#126529 = FACE_OUTER_BOUND ( 'NONE', #26533, .T. ) ;
#126530 = VECTOR ( 'NONE', #85089, 1000.000000000000000 ) ;
#126531 = DIRECTION ( 'NONE',  ( 0.7071067811865487940, -0.7071067811865463515, 0.000000000000000000 ) ) ;
#126533 = ORIENTED_EDGE ( 'NONE', *, *, #7980, .T. ) ;
#126532 = DIRECTION ( 'NONE',  ( -0.7071067811865486830, 0.7071067811865464625, 0.000000000000000000 ) ) ;
#126534 = VERTEX_POINT ( 'NONE', #98925 ) ;
#126535 = DIRECTION ( 'NONE',  ( -0.7071067811865486830, -0.7071067811865464625, -0.000000000000000000 ) ) ;
#126536 = CARTESIAN_POINT ( 'NONE',  ( -23.99451991528749062, 28.92564299267954908, 4.000000000000000000 ) ) ;
#126537 = ORIENTED_EDGE ( 'NONE', *, *, #51157, .T. ) ;
#126538 = CARTESIAN_POINT ( 'NONE',  ( -14.99999999999989519, -10.77435723561696435, -9.972017380717193902 ) ) ;
#126539 = ORIENTED_EDGE ( 'NONE', *, *, #51734, .F. ) ;
#126540 = ORIENTED_EDGE ( 'NONE', *, *, #116509, .F. ) ;
#126541 = VERTEX_POINT ( 'NONE', #32270 ) ;
#126542 = ORIENTED_EDGE ( 'NONE', *, *, #104473, .T. ) ;
#126543 = CARTESIAN_POINT ( 'NONE',  ( 30.18398860626900060, 28.73617430169808173, 5.000000000000000000 ) ) ;
#126544 = DIRECTION ( 'NONE',  ( 0.6830127018922181881, 0.6830127018922202975, -0.2588190451025214056 ) ) ;
#126545 = DIRECTION ( 'NONE',  ( 0.6830127018922181881, 0.6830127018922202975, -0.2588190451025214056 ) ) ;
#126546 = CARTESIAN_POINT ( 'NONE',  ( 2.999999999999981792, -13.97847968911260175, -0.1324546996126730880 ) ) ;
#126547 = DIRECTION ( 'NONE',  ( -0.3543493200069162685, -0.000000000000000000, -0.9351131265310288487 ) ) ;
#126548 = ORIENTED_EDGE ( 'NONE', *, *, #57658, .F. ) ;
#126549 = CARTESIAN_POINT ( 'NONE',  ( 13.17183060077637968, 9.759292476615621936, 4.000000000000000000 ) ) ;
#126550 = CARTESIAN_POINT ( 'NONE',  ( 22.72873647476856007, 5.808823158059031044, -5.808823158059038150 ) ) ;
#126551 = LINE ( 'NONE', #18489, #50881 ) ;
#126552 = FACE_OUTER_BOUND ( 'NONE', #23551, .T. ) ;
#126553 = CARTESIAN_POINT ( 'NONE',  ( -11.70025512860841133, -27.71228299555198049, 4.000000000000000000 ) ) ;
#126554 = ORIENTED_EDGE ( 'NONE', *, *, #947, .F. ) ;
#126555 = VERTEX_POINT ( 'NONE', #66340 ) ;
#126556 = EDGE_CURVE ( 'NONE', #93730, #58304, #20652, .T. ) ;
#126557 = VERTEX_POINT ( 'NONE', #51892 ) ;
#126558 = DIRECTION ( 'NONE',  ( 0.7071067811865487940, 0.7071067811865463515, -0.000000000000000000 ) ) ;
#126559 = CARTESIAN_POINT ( 'NONE',  ( -15.48921356237309510, -27.52281430457066236, 5.000000000000000000 ) ) ;
#126560 = CARTESIAN_POINT ( 'NONE',  ( 54.48921356237310221, -27.52281430457093236, 5.000000000000000000 ) ) ;
#126561 = VECTOR ( 'NONE', #70354, 1000.000000000000000 ) ;
#126562 = LINE ( 'NONE', #14247, #137727 ) ;
#126563 = CARTESIAN_POINT ( 'NONE',  ( 28.49999999999981171, 19.46639925780206326, 5.000000000000000000 ) ) ;
#126564 = CARTESIAN_POINT ( 'NONE',  ( 75.45376352523145158, -6.109999999999999432, -3.741295971395163529E-16 ) ) ;
#126565 = CARTESIAN_POINT ( 'NONE',  ( 0.000000000000000000, 0.000000000000000000, 5.000000000000000000 ) ) ;
#126566 = DIRECTION ( 'NONE',  ( -1.000000000000000000, -0.000000000000000000, -0.000000000000000000 ) ) ;
#126567 = LINE ( 'NONE', #61386, #107980 ) ;
#126568 = CARTESIAN_POINT ( 'NONE',  ( 34.92499999999998295, 22.22500000000000142, 4.500000000000000888 ) ) ;
#126569 = CARTESIAN_POINT ( 'NONE',  ( 24.72281430457042717, -21.72500000000000142, 5.000000000000000000 ) ) ;
#126570 = VECTOR ( 'NONE', #53121, 1000.000000000000227 ) ;
#126571 = ORIENTED_EDGE ( 'NONE', *, *, #40746, .T. ) ;
#126572 = CARTESIAN_POINT ( 'NONE',  ( 17.54957349175731451, -3.269999995228190848, -36.08445893746787903 ) ) ;
#126573 = ORIENTED_EDGE ( 'NONE', *, *, #123901, .T. ) ;
#126574 = CARTESIAN_POINT ( 'NONE',  ( -23.99999999999983302, -19.06887692260762179, 4.000000000000000000 ) ) ;
#126576 = VERTEX_POINT ( 'NONE', #54746 ) ;
#126575 = CARTESIAN_POINT ( 'NONE',  ( -16.49999999999987566, -11.94781430457070392, 5.000000000000000000 ) ) ;
#126577 = VECTOR ( 'NONE', #3614, 1000.000000000000227 ) ;
#126578 = ADVANCED_FACE ( 'NONE', ( #65654 ), #140308, .F. ) ;
#126579 = FACE_OUTER_BOUND ( 'NONE', #2715, .T. ) ;
#126580 = CARTESIAN_POINT ( 'NONE',  ( -10.80981832425544731, -18.74070752338408852, 7.910009926591535567 ) ) ;
#126581 = VERTEX_POINT ( 'NONE', #9782 ) ;
#126582 = EDGE_CURVE ( 'NONE', #74261, #20046, #85196, .T. ) ;
#126583 = CARTESIAN_POINT ( 'NONE',  ( 1.179999999999999272, 10.00000000000000178, 10.00000000000000000 ) ) ;
#126584 = ORIENTED_EDGE ( 'NONE', *, *, #125686, .F. ) ;
#126585 = CARTESIAN_POINT ( 'NONE',  ( 121.4125270504628986, -7.949999999999998401, -4.867971026610728450E-16 ) ) ;
#126586 = ORIENTED_EDGE ( 'NONE', *, *, #19330, .F. ) ;
#126587 = DIRECTION ( 'NONE',  ( 0.3543493200069162685, -0.000000000000000000, -0.9351131265310288487 ) ) ;
#126588 = CARTESIAN_POINT ( 'NONE',  ( 97.05836038379621300, -7.949999999999997513, -2.130196079827425759 ) ) ;
#126589 = CARTESIAN_POINT ( 'NONE',  ( 21.81349135397625361, -15.74070752338412049, 8.904080028138892544 ) ) ;
#126590 =( LENGTH_UNIT ( ) NAMED_UNIT ( * ) SI_UNIT ( .MILLI., .METRE. ) );
#126591 = VERTEX_POINT ( 'NONE', #30105 ) ;
#126592 = AXIS2_PLACEMENT_3D ( 'NONE', #43080, #128643, #76420 ) ;
#126593 = ADVANCED_FACE ( 'NONE', ( #74354 ), #10486, .F. ) ;
#126594 = CARTESIAN_POINT ( 'NONE',  ( 34.49999999999975842, -17.94567065516886117, 4.994342998332151673 ) ) ;
#126595 = CARTESIAN_POINT ( 'NONE',  ( -16.49999999999988276, 14.14708470758589520, -0.5283514160166185025 ) ) ;
#126596 = CARTESIAN_POINT ( 'NONE',  ( 19.97916666666667140, 6.094999999999988205, -1.633150327867694651 ) ) ;
#126597 = CARTESIAN_POINT ( 'NONE',  ( -18.18398860626898994, 28.73617430169800002, 5.000000000000000000 ) ) ;
#126598 = DIRECTION ( 'NONE',  ( 0.000000000000000000, 0.000000000000000000, 1.000000000000000000 ) ) ;
#126599 = ORIENTED_EDGE ( 'NONE', *, *, #133361, .F. ) ;
#126600 = EDGE_CURVE ( 'NONE', #115014, #1998, #143276, .T. ) ;
#126601 = CARTESIAN_POINT ( 'NONE',  ( 46.30836038379622721, 7.949999999999996625, 2.130196079827431088 ) ) ;
#126602 = ORIENTED_EDGE ( 'NONE', *, *, #94146, .F. ) ;
#126603 = CARTESIAN_POINT ( 'NONE',  ( 87.93793019189809002, -6.110000000000001208, 1.637169565754158951 ) ) ;
#126604 = LINE ( 'NONE', #103422, #107918 ) ;
#126605 = CARTESIAN_POINT ( 'NONE',  ( 53.99451991528749062, 28.92564299267975869, 4.000000000000000000 ) ) ;
#126606 = CARTESIAN_POINT ( 'NONE',  ( 0.1839886062690032631, 28.73617430169787568, 5.000000000000000000 ) ) ;
#126607 = ORIENTED_EDGE ( 'NONE', *, *, #67562, .T. ) ;
#126608 = ADVANCED_FACE ( 'NONE', ( #54052 ), #9020, .F. ) ;
#126609 = DIRECTION ( 'NONE',  ( 0.7071067811865486830, -0.7071067811865464625, -0.000000000000000000 ) ) ;
#126610 = DIRECTION ( 'NONE',  ( 1.000000000000000000, 0.000000000000000000, 0.000000000000000000 ) ) ;
#126611 = AXIS2_PLACEMENT_3D ( 'NONE', #11089, #206, #101698 ) ;
#126612 = CARTESIAN_POINT ( 'NONE',  ( 117.1833603837962130, -2.130196079827426203, 7.949999999999996625 ) ) ;
#126613 = DIRECTION ( 'NONE',  ( -1.000000000000000000, -0.000000000000000000, -0.000000000000000000 ) ) ;
#126615 = ORIENTED_EDGE ( 'NONE', *, *, #7175, .T. ) ;
#126614 = CARTESIAN_POINT ( 'NONE',  ( -25.49999999999982236, -19.91253812416055524, 4.000000000000000000 ) ) ;
#126616 = DIRECTION ( 'NONE',  ( -0.7071067811865487940, 0.7071067811865463515, 0.000000000000000000 ) ) ;
#126617 = CARTESIAN_POINT ( 'NONE',  ( -20.01088028653933648, -22.02621442084248216, 4.990779571109221102 ) ) ;
#126618 = AXIS2_PLACEMENT_3D ( 'NONE', #53202, #119863, #64821 ) ;
#126619 = CARTESIAN_POINT ( 'NONE',  ( 27.79289321881325847, 18.75929247661552779, 5.000000000000000000 ) ) ;
#126620 = VECTOR ( 'NONE', #92781, 1000.000000000000000 ) ;
#126621 = EDGE_LOOP ( 'NONE', ( #44304, #49870, #103482, #52979 ) ) ;
#126622 = VERTEX_POINT ( 'NONE', #53284 ) ;
#126623 = ORIENTED_EDGE ( 'NONE', *, *, #32833, .F. ) ;
#126624 = VECTOR ( 'NONE', #22282, 1000.000000000000227 ) ;
#126625 = CARTESIAN_POINT ( 'NONE',  ( 79.47959685856477563, 6.109999999999999432, 1.637169565754164280 ) ) ;
#126626 = EDGE_LOOP ( 'NONE', ( #70223, #59172, #138191 ) ) ;
#126627 = DIRECTION ( 'NONE',  ( -1.000000000000000000, 0.000000000000000000, -0.000000000000000000 ) ) ;
#126628 = EDGE_CURVE ( 'NONE', #91076, #108780, #21392, .T. ) ;
#126629 = CIRCLE ( 'NONE', #20142, 2.055000000000000160 ) ;
#126630 = CARTESIAN_POINT ( 'NONE',  ( 74.99451991528749772, 28.92564299267990435, 4.000000000000000000 ) ) ;
#126632 = VECTOR ( 'NONE', #13219, 999.9999999999998863 ) ;
#126631 = DIRECTION ( 'NONE',  ( -0.3543493200069162685, -0.000000000000000000, -0.9351131265310288487 ) ) ;
#126633 = DIRECTION ( 'NONE',  ( -0.7071067811865486830, -0.7071067811865464625, -0.000000000000000000 ) ) ;
#126634 = ORIENTED_EDGE ( 'NONE', *, *, #132793, .F. ) ;
#126635 = DIRECTION ( 'NONE',  ( -1.000000000000000000, -0.000000000000000000, -0.000000000000000000 ) ) ;
#126636 = CARTESIAN_POINT ( 'NONE',  ( 28.49999999999980460, 9.431123077392088661, 4.000000000000000000 ) ) ;
#126637 = EDGE_CURVE ( 'NONE', #113440, #128877, #96755, .T. ) ;
#126638 = ADVANCED_FACE ( 'NONE', ( #119942 ), #97496, .T. ) ;
#126639 = ORIENTED_EDGE ( 'NONE', *, *, #108245, .T. ) ;
#126640 = CARTESIAN_POINT ( 'NONE',  ( 1.153529387357648650, -0.6659121308574033060, 3.830688525020676138 ) ) ;
#126641 = DIRECTION ( 'NONE',  ( -0.7071067811865486830, 0.7071067811865464625, 0.000000000000000000 ) ) ;
#126642 = CARTESIAN_POINT ( 'NONE',  ( -30.48921356237309510, -27.52281430457076894, 5.000000000000000000 ) ) ;
#126643 = EDGE_CURVE ( 'NONE', #1086, #58487, #31555, .T. ) ;
#126644 =( BOUNDED_CURVE ( )  B_SPLINE_CURVE ( 3, ( #115533, #39466, #28585, #27850 ),
 .UNSPECIFIED., .F., .F. ) 
 B_SPLINE_CURVE_WITH_KNOTS ( ( 4, 4 ),
 ( 1.964434688349484537, 3.503810798801452187 ),
 .UNSPECIFIED. ) 
 CURVE ( )  GEOMETRIC_REPRESENTATION_ITEM ( )  RATIONAL_B_SPLINE_CURVE ( ( 1.000000000000000000, 0.8120851936182271746, 0.8120851936182271746, 1.000000000000000000 ) ) 
 REPRESENTATION_ITEM ( '' )  );
#126645 = ORIENTED_EDGE ( 'NONE', *, *, #94161, .T. ) ;
#126646 = VERTEX_POINT ( 'NONE', #57609 ) ;
#126647 = CARTESIAN_POINT ( 'NONE',  ( 21.06011071044006755, -9.740707523384187994, 10.89222023123375926 ) ) ;
#126648 = ADVANCED_FACE ( 'NONE', ( #80778 ), #102538, .F. ) ;
#126649 = EDGE_CURVE ( 'NONE', #129256, #94995, #45318, .T. ) ;
#126650 = CARTESIAN_POINT ( 'NONE',  ( -26.99999999999981171, -11.35517001088074807, -1.126524801160169620 ) ) ;
#126651 = CYLINDRICAL_SURFACE ( 'NONE', #92438, 2.500000000000000000 ) ;
#126652 = DIRECTION ( 'NONE',  ( 0.7071067811865487940, 0.7071067811865463515, -0.000000000000000000 ) ) ;
#126653 = DIRECTION ( 'NONE',  ( -0.000000000000000000, 0.3543493200069153248, 0.9351131265310292928 ) ) ;
#126654 = VECTOR ( 'NONE', #14911, 1000.000000000000000 ) ;
#126655 = PLANE ( 'NONE',  #136778 ) ;
#126656 = CARTESIAN_POINT ( 'NONE',  ( 25.08376352523143638, -6.110000000000001208, -3.741295971395164515E-16 ) ) ;
#126657 = FILL_AREA_STYLE ('',( #93335 ) ) ;
#126658 = ORIENTED_EDGE ( 'NONE', *, *, #63655, .T. ) ;
#126659 = ORIENTED_EDGE ( 'NONE', *, *, #43394, .F. ) ;
#126660 = ORIENTED_EDGE ( 'NONE', *, *, #11070, .T. ) ;
#126661 = EDGE_CURVE ( 'NONE', #68252, #8528, #25658, .T. ) ;
#126662 = ORIENTED_EDGE ( 'NONE', *, *, #64624, .T. ) ;
#126663 = VECTOR ( 'NONE', #89738, 1000.000000000000000 ) ;
#126664 = ADVANCED_FACE ( 'NONE', ( #22764 ), #122109, .T. ) ;
#126665 = DIRECTION ( 'NONE',  ( -0.000000000000000000, -0.3543493200069152693, 0.9351131265310292928 ) ) ;
#126666 =( NAMED_UNIT ( * ) SI_UNIT ( $, .STERADIAN. ) SOLID_ANGLE_UNIT ( ) );
#126667 = ORIENTED_EDGE ( 'NONE', *, *, #140060, .T. ) ;
#126668 = PLANE ( 'NONE',  #92243 ) ;
#126669 = FACE_OUTER_BOUND ( 'NONE', #125663, .T. ) ;
#126670 = CARTESIAN_POINT ( 'NONE',  ( 22.07159235450331991, 2.500000000000001332, 0.000000000000000000 ) ) ;
#126671 = AXIS2_PLACEMENT_3D ( 'NONE', #66546, #33924, #1940 ) ;
#126672 = FACE_OUTER_BOUND ( 'NONE', #58185, .T. ) ;
#126673 = DIRECTION ( 'NONE',  ( 0.7071067811865486830, -0.7071067811865464625, -0.000000000000000000 ) ) ;
#126674 = ORIENTED_EDGE ( 'NONE', *, *, #52476, .T. ) ;
#126675 = CARTESIAN_POINT ( 'NONE',  ( 21.18398860626899349, 28.73617430169802134, 5.000000000000000000 ) ) ;
#126676 = CARTESIAN_POINT ( 'NONE',  ( 35.99451991528749772, 28.92564299267963079, 4.000000000000000000 ) ) ;
#126677 = ORIENTED_EDGE ( 'NONE', *, *, #105415, .T. ) ;
#126678 = CARTESIAN_POINT ( 'NONE',  ( -32.28242261357410570, -21.73023691814492508, 5.000000000000000888 ) ) ;
#126679 = ORIENTED_EDGE ( 'NONE', *, *, #31105, .T. ) ;
#126680 = VERTEX_POINT ( 'NONE', #101796 ) ;
#126681 = CARTESIAN_POINT ( 'NONE',  ( 29.99451991528749417, 28.92564299267958816, 4.000000000000000000 ) ) ;
#126682 = ORIENTED_EDGE ( 'NONE', *, *, #115714, .T. ) ;
#126683 = VERTEX_POINT ( 'NONE', #56904 ) ;
#126684 = CARTESIAN_POINT ( 'NONE',  ( 73.64626352523140440, -4.472830434245840259, 4.472830434245838482 ) ) ;
#126685 = ORIENTED_EDGE ( 'NONE', *, *, #142873, .T. ) ;
#126686 = EDGE_CURVE ( 'NONE', #55719, #141993, #11175, .T. ) ;
#126687 = SURFACE_STYLE_FILL_AREA ( #15748 ) ;
#126688 = EDGE_CURVE ( 'NONE', #3304, #70500, #77921, .T. ) ;
#126689 = DIRECTION ( 'NONE',  ( -0.6830127018922180770, -0.6830127018922204085, -0.2588190451025213501 ) ) ;
#126690 = VECTOR ( 'NONE', #100831, 1000.000000000000000 ) ;
#126691 = CARTESIAN_POINT ( 'NONE',  ( 110.3962635252314328, 4.472830434245840259, -4.472830434245838482 ) ) ;
#126692 = PLANE ( 'NONE',  #70352 ) ;
#126693 = DIRECTION ( 'NONE',  ( -1.000000000000000000, -0.000000000000000000, -0.000000000000000000 ) ) ;
#126694 = DIRECTION ( 'NONE',  ( 0.7071067811865487940, 0.7071067811865463515, 0.000000000000000000 ) ) ;
#126695 = CARTESIAN_POINT ( 'NONE',  ( 25.65999999999999659, 9.521314400968980422E-16, 0.000000000000000000 ) ) ;
#126696 = PLANE ( 'NONE',  #49365 ) ;
#126697 = CARTESIAN_POINT ( 'NONE',  ( 34.78752705046288440, 0.000000000000000000, -7.949999999999998401 ) ) ;
#126698 = CARTESIAN_POINT ( 'NONE',  ( -12.48921356237309155, -27.52281430457064104, 5.000000000000000000 ) ) ;
#126699 = ORIENTED_EDGE ( 'NONE', *, *, #3985, .F. ) ;
#126700 = CARTESIAN_POINT ( 'NONE',  ( 131.5423521607622490, -49.05583548141700589, 39.86617647058822911 ) ) ;
#126701 = PLANE ( 'NONE',  #49893 ) ;
#126702 = VERTEX_POINT ( 'NONE', #55452 ) ;
#126703 = ORIENTED_EDGE ( 'NONE', *, *, #8418, .F. ) ;
#126704 = CARTESIAN_POINT ( 'NONE',  ( -12.69999999999998153, 0.000000000000000000, 0.000000000000000000 ) ) ;
#126705 = ORIENTED_EDGE ( 'NONE', *, *, #39914, .F. ) ;
#126706 = FACE_OUTER_BOUND ( 'NONE', #34249, .T. ) ;
#126707 = DIRECTION ( 'NONE',  ( 0.000000000000000000, -1.000000000000000000, 0.000000000000000000 ) ) ;
#126708 = CARTESIAN_POINT ( 'NONE',  ( -21.48921356237309155, -27.52281430457070499, 5.000000000000000000 ) ) ;
#126709 = FACE_OUTER_BOUND ( 'NONE', #139368, .T. ) ;
#126710 = FACE_OUTER_BOUND ( 'NONE', #43280, .T. ) ;
#126711 = ORIENTED_EDGE ( 'NONE', *, *, #53288, .T. ) ;
#126712 =( NAMED_UNIT ( * ) PLANE_ANGLE_UNIT ( ) SI_UNIT ( $, .RADIAN. ) );
#126713 = VERTEX_POINT ( 'NONE', #99641 ) ;
#126714 = VECTOR ( 'NONE', #3463, 1000.000000000000000 ) ;
#126716 = CARTESIAN_POINT ( 'NONE',  ( -9.299744871391588674, -27.71228299555212971, 4.000000000000000000 ) ) ;
#126715 = AXIS2_PLACEMENT_3D ( 'NONE', #21313, #120591, #139557 ) ;
#126717 = CARTESIAN_POINT ( 'NONE',  ( 30.10873647476854842, -5.808823158059033709, 5.808823158059035485 ) ) ;
#126718 = CARTESIAN_POINT ( 'NONE',  ( 23.99451991528749062, 28.92564299267954908, 4.000000000000000000 ) ) ;
#126719 = CARTESIAN_POINT ( 'NONE',  ( -27.48921356237309155, -27.52281430457074762, 5.000000000000000000 ) ) ;
#126720 = DIRECTION ( 'NONE',  ( 0.7071067811865487940, 0.7071067811865463515, 0.000000000000000000 ) ) ;
#126721 = EDGE_LOOP ( 'NONE', ( #17987, #61813, #92238, #8068 ) ) ;
#126722 = ORIENTED_EDGE ( 'NONE', *, *, #5143, .F. ) ;
#126723 = ORIENTED_EDGE ( 'NONE', *, *, #18720, .F. ) ;
#126724 = FACE_OUTER_BOUND ( 'NONE', #14258, .T. ) ;
#126725 = CARTESIAN_POINT ( 'NONE',  ( -72.48921356237309510, -27.52281430457106026, 5.000000000000000000 ) ) ;
#126726 = VECTOR ( 'NONE', #95440, 1000.000000000000000 ) ;
#126727 = DIRECTION ( 'NONE',  ( 0.000000000000000000, 0.000000000000000000, -1.000000000000000000 ) ) ;
#126728 = CARTESIAN_POINT ( 'NONE',  ( -56.99451991528749062, 28.92564299267978001, 4.000000000000000000 ) ) ;
#126729 = FACE_OUTER_BOUND ( 'NONE', #96173, .T. ) ;
#126730 = CARTESIAN_POINT ( 'NONE',  ( 21.70710678118640402, 20.25929247661551358, 5.000000000000000000 ) ) ;
#126731 = PLANE ( 'NONE',  #9154 ) ;
#126732 = DIRECTION ( 'NONE',  ( -0.7071067811865486830, -0.7071067811865464625, 0.000000000000000000 ) ) ;
#126733 = CARTESIAN_POINT ( 'NONE',  ( -2.816011393730999401, 28.73617430169785436, 5.000000000000000000 ) ) ;
#126734 = VERTEX_POINT ( 'NONE', #90949 ) ;
#126735 = CARTESIAN_POINT ( 'NONE',  ( 73.04166666666667140, -3.975000000000002753, 6.884901960086286188 ) ) ;
#126736 = DIRECTION ( 'NONE',  ( -1.000000000000000000, -1.224606353822377258E-16, -0.000000000000000000 ) ) ;
#126737 = ORIENTED_EDGE ( 'NONE', *, *, #126855, .T. ) ;
#126738 = ADVANCED_FACE ( 'NONE', ( #13340 ), #312, .F. ) ;
#126739 = DIRECTION ( 'NONE',  ( -0.7071067811865486830, -0.7071067811865464625, -0.000000000000000000 ) ) ;
#126741 = ORIENTED_EDGE ( 'NONE', *, *, #67245, .T. ) ;
#126740 = DIRECTION ( 'NONE',  ( -0.000000000000000000, 0.000000000000000000, 1.000000000000000000 ) ) ;
#126742 = VERTEX_POINT ( 'NONE', #88806 ) ;
#126743 = EDGE_CURVE ( 'NONE', #122527, #84994, #67042, .T. ) ;
#126744 = EDGE_CURVE ( 'NONE', #667, #119248, #111225, .T. ) ;
#126745 = DIRECTION ( 'NONE',  ( -0.000000000000000000, 0.3543493200069152138, -0.9351131265310292928 ) ) ;
#126746 = DIRECTION ( 'NONE',  ( -0.000000000000000000, 0.3543493200069153248, 0.9351131265310292928 ) ) ;
#126748 = CONICAL_SURFACE ( 'NONE', #24931, 2.055000000000000604, 0.9599310885968764806 ) ;
#126747 = CARTESIAN_POINT ( 'NONE',  ( 21.29974487139158512, -27.71228299555221142, 4.000000000000000000 ) ) ;
#126749 = ORIENTED_EDGE ( 'NONE', *, *, #111050, .F. ) ;
#126750 = DIRECTION ( 'NONE',  ( -0.000000000000000000, 0.000000000000000000, 1.000000000000000000 ) ) ;
#126751 = ORIENTED_EDGE ( 'NONE', *, *, #83066, .T. ) ;
#126752 = EDGE_CURVE ( 'NONE', #7814, #5802, #58356, .T. ) ;
#126753 = EDGE_CURVE ( 'NONE', #133079, #106729, #89492, .T. ) ;
#126754 = CARTESIAN_POINT ( 'NONE',  ( 18.29974487139159223, -27.71228299555219010, 4.000000000000000000 ) ) ;
#126755 = CARTESIAN_POINT ( 'NONE',  ( 107.0208333333333144, 7.949999999999998401, 2.130196079827431532 ) ) ;
#126756 = CARTESIAN_POINT ( 'NONE',  ( 123.6000270504628702, 5.819803920172570422, 5.819803920172574863 ) ) ;
#126757 = VECTOR ( 'NONE', #115838, 1000.000000000000000 ) ;
#126758 = DIRECTION ( 'NONE',  ( -0.7071067811865486830, 0.7071067811865464625, 0.000000000000000000 ) ) ;
#126759 =( BOUNDED_CURVE ( )  B_SPLINE_CURVE ( 3, ( #143316, #99073, #11338, #88965 ),
 .UNSPECIFIED., .F., .T. ) 
 B_SPLINE_CURVE_WITH_KNOTS ( ( 4, 4 ),
 ( 5.143245962375961433, 6.645403452391247079 ),
 .UNSPECIFIED. ) 
 CURVE ( )  GEOMETRIC_REPRESENTATION_ITEM ( )  RATIONAL_B_SPLINE_CURVE ( ( 1.000000000000000000, 0.8206354192515231682, 0.8206354192515231682, 1.000000000000000000 ) ) 
 REPRESENTATION_ITEM ( '' )  );
#126760 = CARTESIAN_POINT ( 'NONE',  ( 18.29974487139159223, -27.71228299555219010, 4.000000000000000000 ) ) ;
#126761 = EDGE_CURVE ( 'NONE', #82511, #12106, #78512, .T. ) ;
#126762 = DIRECTION ( 'NONE',  ( 0.000000000000000000, -1.000000000000000000, 0.000000000000000000 ) ) ;
#126763 = PLANE ( 'NONE',  #12463 ) ;
#126764 = CARTESIAN_POINT ( 'NONE',  ( -12.69999999999998153, 0.000000000000000000, 0.000000000000000000 ) ) ;
#126765 = CARTESIAN_POINT ( 'NONE',  ( 33.95790314143522437, 6.871911579029515771, 3.967499999999989146 ) ) ;
#126766 = CARTESIAN_POINT ( 'NONE',  ( 9.895403141435220817, 2.126176841940962348, 7.934999999999988951 ) ) ;
#126767 = CARTESIAN_POINT ( 'NONE',  ( -39.48921356237310221, -27.52281430457082934, 5.000000000000000000 ) ) ;
#126768 = CARTESIAN_POINT ( 'NONE',  ( -1.499999999999989120, 6.431123077392125964, 4.000000000000000000 ) ) ;
#126769 = CARTESIAN_POINT ( 'NONE',  ( 57.18398860626899705, 28.73617430169827358, 5.000000000000000000 ) ) ;
#126770 = ORIENTED_EDGE ( 'NONE', *, *, #32598, .F. ) ;
#126771 = EDGE_LOOP ( 'NONE', ( #138323, #38625, #91341, #114289 ) ) ;
#126773 = EDGE_CURVE ( 'NONE', #13028, #136170, #80085, .T. ) ;
#126772 = CARTESIAN_POINT ( 'NONE',  ( 80.18749999999997158, -5.819803920172573086, 5.819803920172572198 ) ) ;
#126774 = ORIENTED_EDGE ( 'NONE', *, *, #82314, .T. ) ;
#126775 = ORIENTED_EDGE ( 'NONE', *, *, #13942, .F. ) ;
#126776 = PRODUCT_DEFINITION_SHAPE ( 'NONE', 'NONE',  #143565 ) ;
#126778 = EDGE_CURVE ( 'NONE', #131518, #60169, #91640, .T. ) ;
#126777 =( NAMED_UNIT ( * ) SI_UNIT ( $, .STERADIAN. ) SOLID_ANGLE_UNIT ( ) );
#126779 = LINE ( 'NONE', #36925, #2322 ) ;
#126780 = LINE ( 'NONE', #94155, #103447 ) ;
#126781 = ORIENTED_EDGE ( 'NONE', *, *, #135064, .F. ) ;
#126782 = ADVANCED_FACE ( 'NONE', ( #56204 ), #100387, .F. ) ;
#126783 = CARTESIAN_POINT ( 'NONE',  ( 5.700255128608413102, -27.71228299555201957, 4.000000000000000000 ) ) ;
#126784 = CARTESIAN_POINT ( 'NONE',  ( 32.29298673570672662, -21.74070752338405654, 4.999753212805222446 ) ) ;
#126786 = VECTOR ( 'NONE', #98360, 1000.000000000000000 ) ;
#126785 = DIRECTION ( 'NONE',  ( 0.000000000000000000, -1.091707662666338270E-16, 1.000000000000000000 ) ) ;
#126787 = CARTESIAN_POINT ( 'NONE',  ( 127.0000000000000000, 1.864289179696898779, 6.174700466780991270 ) ) ;
#126788 = CARTESIAN_POINT ( 'NONE',  ( -25.39999999999996305, 0.000000000000000000, 0.000000000000000000 ) ) ;
#126789 = CARTESIAN_POINT ( 'NONE',  ( 16.49999999999988987, 18.05218569542898521, 5.000000000000000000 ) ) ;
#126790 = EDGE_CURVE ( 'NONE', #17257, #116142, #134446, .T. ) ;
#126791 = LINE ( 'NONE', #17328, #119287 ) ;
#126792 = FACE_OUTER_BOUND ( 'NONE', #103398, .T. ) ;
#126793 = DIRECTION ( 'NONE',  ( -0.3543493200069162685, -0.000000000000000000, -0.9351131265310288487 ) ) ;
#126794 = LINE ( 'NONE', #100437, #68429 ) ;
#126795 = FILL_AREA_STYLE ('',( #80482 ) ) ;
#126796 = ORIENTED_EDGE ( 'NONE', *, *, #81097, .T. ) ;
#126797 = VERTEX_POINT ( 'NONE', #112674 ) ;
#126798 = CARTESIAN_POINT ( 'NONE',  ( 113.3129301918981042, -1.637169565754159617, -6.110000000000001208 ) ) ;
#126799 = VECTOR ( 'NONE', #72909, 1000.000000000000227 ) ;
#126800 = ORIENTED_EDGE ( 'NONE', *, *, #131769, .F. ) ;
#126801 = ADVANCED_FACE ( 'NONE', ( #60471 ), #137298, .T. ) ;
#126802 = DIRECTION ( 'NONE',  ( -0.6830127018922180770, -0.6830127018922204085, -0.2588190451025213501 ) ) ;
#126803 = CARTESIAN_POINT ( 'NONE',  ( -75.29974487139158157, -27.71228299555258445, 4.000000000000000000 ) ) ;
#126804 = ORIENTED_EDGE ( 'NONE', *, *, #54161, .F. ) ;
#126805 = FACE_OUTER_BOUND ( 'NONE', #78063, .T. ) ;
#126806 = PLANE ( 'NONE',  #14224 ) ;
#126807 = EDGE_CURVE ( 'NONE', #114717, #58130, #3866, .T. ) ;
#126808 = CONICAL_SURFACE ( 'NONE', #75916, 2.055000000000000604, 0.9599310885968764806 ) ;
#126809 = CARTESIAN_POINT ( 'NONE',  ( 101.8495968585647660, 6.109999999999996767, 1.637169565754163836 ) ) ;
#126810 = ORIENTED_EDGE ( 'NONE', *, *, #80351, .F. ) ;
#126811 = ADVANCED_FACE ( 'NONE', ( #26395 ), #6011, .T. ) ;
#126812 = LINE ( 'NONE', #45210, #69769 ) ;
#126813 = ORIENTED_EDGE ( 'NONE', *, *, #72861, .T. ) ;
#126814 = DIRECTION ( 'NONE',  ( 0.5735764363510448272, -0.8191520442889927978, 1.003171929053526103E-16 ) ) ;
#126815 = LINE ( 'NONE', #73885, #141813 ) ;
#126816 = PLANE ( 'NONE',  #91758 ) ;
#126817 = CONICAL_SURFACE ( 'NONE', #24986, 1.898649999999993065, 1.029744258676648316 ) ;
#126818 = EDGE_CURVE ( 'NONE', #65462, #119206, #103908, .T. ) ;
#126819 = ORIENTED_EDGE ( 'NONE', *, *, #36969, .F. ) ;
#126820 = VERTEX_POINT ( 'NONE', #93780 ) ;
#126821 = VECTOR ( 'NONE', #96000, 1000.000000000000000 ) ;
#126822 = ORIENTED_EDGE ( 'NONE', *, *, #129122, .F. ) ;
#126823 = DIRECTION ( 'NONE',  ( 0.5735764363510448272, -0.8191520442889927978, 1.003171929053526103E-16 ) ) ;
#126824 = CARTESIAN_POINT ( 'NONE',  ( 4.296236474768552860, 7.934999999999990727, -1.457635852685135314E-15 ) ) ;
#126825 = VECTOR ( 'NONE', #67712, 1000.000000000000000 ) ;
#126826 = CARTESIAN_POINT ( 'NONE',  ( -42.18398860626899705, 28.73617430169816700, 5.000000000000000000 ) ) ;
#126827 = FACE_OUTER_BOUND ( 'NONE', #21802, .T. ) ;
#126828 = ORIENTED_EDGE ( 'NONE', *, *, #14377, .T. ) ;
#126829 = ORIENTED_EDGE ( 'NONE', *, *, #27514, .T. ) ;
#126830 = EDGE_CURVE ( 'NONE', #127624, #139771, #138007, .T. ) ;
#126831 = CARTESIAN_POINT ( 'NONE',  ( -13.27644930412397350, 4.689949953678146599, 5.000000000000000000 ) ) ;
#126832 = VERTEX_POINT ( 'NONE', #136553 ) ;
#126833 = EDGE_LOOP ( 'NONE', ( #111582, #7275, #78383, #34449 ) ) ;
#126834 = EDGE_CURVE ( 'NONE', #141737, #106911, #117881, .T. ) ;
#126835 = DIRECTION ( 'NONE',  ( 0.000000000000000000, 0.000000000000000000, 1.000000000000000000 ) ) ;
#126836 = CARTESIAN_POINT ( 'NONE',  ( 39.18398860626899705, 28.73617430169814568, 5.000000000000000000 ) ) ;
#126837 = CARTESIAN_POINT ( 'NONE',  ( 39.48921356237310221, -27.52281430457082934, 5.000000000000000000 ) ) ;
#126838 = ORIENTED_EDGE ( 'NONE', *, *, #11933, .T. ) ;
#126839 = CARTESIAN_POINT ( 'NONE',  ( 6.854166666666666963, 1.633150327867685103, 6.094999999999992646 ) ) ;
#126840 = CARTESIAN_POINT ( 'NONE',  ( -22.82816939922337340, -14.24070752338413826, 4.000000000000000000 ) ) ;
#126841 = EDGE_LOOP ( 'NONE', ( #85363, #84888, #18407 ) ) ;
#126842 = CARTESIAN_POINT ( 'NONE',  ( -19.49999999999986500, 9.127013188829483425, 4.802533355213530086 ) ) ;
#126843 = EDGE_CURVE ( 'NONE', #94488, #673, #127857, .T. ) ;
#126844 = FACE_BOUND ( 'NONE', #106857, .T. ) ;
#126845 = ORIENTED_EDGE ( 'NONE', *, *, #86590, .F. ) ;
#126846 = CARTESIAN_POINT ( 'NONE',  ( 64.39169371712957002, 2.130196079827421762, 7.950000000000000178 ) ) ;
#126847 = CARTESIAN_POINT ( 'NONE',  ( 0.000000000000000000, 0.000000000000000000, 5.000000000000000000 ) ) ;
#126848 = PLANE ( 'NONE',  #30695 ) ;
#126849 = ORIENTED_EDGE ( 'NONE', *, *, #16859, .T. ) ;
#126850 = PLANE ( 'NONE',  #36597 ) ;
#126851 = VERTEX_POINT ( 'NONE', #94476 ) ;
#126852 = AXIS2_PLACEMENT_3D ( 'NONE', #77691, #22542, #34905 ) ;
#126853 = ORIENTED_EDGE ( 'NONE', *, *, #93938, .F. ) ;
#126854 = ORIENTED_EDGE ( 'NONE', *, *, #141353, .T. ) ;
#126855 = EDGE_CURVE ( 'NONE', #5733, #122911, #15462, .T. ) ;
#126856 = CARTESIAN_POINT ( 'NONE',  ( 33.89126352523143737, -4.472830434245838482, -4.472830434245838482 ) ) ;
#126857 = ORIENTED_EDGE ( 'NONE', *, *, #82838, .F. ) ;
#126858 = LINE ( 'NONE', #137777, #117880 ) ;
#126859 = FACE_OUTER_BOUND ( 'NONE', #131983, .T. ) ;
#126860 = SURFACE_STYLE_USAGE ( .BOTH. , #68966 ) ;
#126861 = DIRECTION ( 'NONE',  ( 0.000000000000000000, 0.000000000000000000, -1.000000000000000000 ) ) ;
#126862 = EDGE_CURVE ( 'NONE', #20488, #3243, #114786, .T. ) ;
#126863 = SURFACE_STYLE_FILL_AREA ( #113866 ) ;
#126864 = EDGE_CURVE ( 'NONE', #107481, #60758, #114105, .T. ) ;
#126865 = CARTESIAN_POINT ( 'NONE',  ( -39.48921356237310221, -27.52281430457082934, 5.000000000000000000 ) ) ;
#126866 = FACE_OUTER_BOUND ( 'NONE', #121135, .T. ) ;
#126867 = DIRECTION ( 'NONE',  ( -0.6830127018922181881, 0.6830127018922202975, -0.2588190451025214056 ) ) ;
#126868 = CARTESIAN_POINT ( 'NONE',  ( -34.42500000000001137, -16.45860074219782021, 5.000000000000000000 ) ) ;
#126869 = ORIENTED_EDGE ( 'NONE', *, *, #74982, .T. ) ;
#126870 = ORIENTED_EDGE ( 'NONE', *, *, #3122, .T. ) ;
#126871 = ORIENTED_EDGE ( 'NONE', *, *, #138615, .T. ) ;
#126872 = VERTEX_POINT ( 'NONE', #59748 ) ;
#126873 = PLANE ( 'NONE',  #51708 ) ;
#126874 = ORIENTED_EDGE ( 'NONE', *, *, #129713, .F. ) ;
#126875 = ORIENTED_EDGE ( 'NONE', *, *, #65035, .F. ) ;
#126876 = DIRECTION ( 'NONE',  ( 0.7071067811865487940, 0.7071067811865463515, 0.000000000000000000 ) ) ;
#126877 = FACE_OUTER_BOUND ( 'NONE', #28280, .T. ) ;
#126878 = EDGE_CURVE ( 'NONE', #137919, #72813, #37995, .T. ) ;
#126879 = DIRECTION ( 'NONE',  ( 0.3543493200069162685, -0.000000000000000000, -0.9351131265310288487 ) ) ;
#126880 = EDGE_LOOP ( 'NONE', ( #48459, #126334, #23724, #76533 ) ) ;
#126881 = LINE ( 'NONE', #37039, #125125 ) ;
#126882 = ORIENTED_EDGE ( 'NONE', *, *, #14340, .T. ) ;
#126883 = LINE ( 'NONE', #18847, #32879 ) ;
#126884 = LINE ( 'NONE', #4343, #102862 ) ;
#126885 = CARTESIAN_POINT ( 'NONE',  ( 4.150403141435219823, 7.934999999999989839, -2.126176841940961904 ) ) ;
#126886 = EDGE_LOOP ( 'NONE', ( #101332, #30444, #72414, #89240 ) ) ;
#126888 = CARTESIAN_POINT ( 'NONE',  ( 23.99999999999982947, -21.84840872380822674, 2.849755605029664185 ) ) ;
#126887 = CARTESIAN_POINT ( 'NONE',  ( 102.8704301918981230, -3.055000000000001936, 5.291415217122918513 ) ) ;
#126889 = VECTOR ( 'NONE', #52519, 1000.000000000000227 ) ;
#126890 = DIRECTION ( 'NONE',  ( 0.7071067811865487940, 0.7071067811865463515, 0.000000000000000000 ) ) ;
#126891 = CARTESIAN_POINT ( 'NONE',  ( 36.48921356237310221, -27.52281430457080802, 5.000000000000000000 ) ) ;
#126892 = ORIENTED_EDGE ( 'NONE', *, *, #139599, .T. ) ;
#126893 = VERTEX_POINT ( 'NONE', #50289 ) ;
#126894 = CARTESIAN_POINT ( 'NONE',  ( -38.99451991528749062, 28.92564299267965211, 4.000000000000000000 ) ) ;
#126895 = ORIENTED_EDGE ( 'NONE', *, *, #2977, .T. ) ;
#126896 = PRESENTATION_STYLE_ASSIGNMENT (( #48658 ) ) ;
#126897 = DIRECTION ( 'NONE',  ( 0.7071067811865487940, 0.7071067811865463515, 0.000000000000000000 ) ) ;
#126898 = DIRECTION ( 'NONE',  ( 0.7071067811865486830, -0.7071067811865464625, -0.000000000000000000 ) ) ;
#126899 = CARTESIAN_POINT ( 'NONE',  ( -27.18398860626900060, 28.73617430169806042, 5.000000000000000000 ) ) ;
#126900 = ORIENTED_EDGE ( 'NONE', *, *, #25823, .T. ) ;
#126901 = CARTESIAN_POINT ( 'NONE',  ( -4.968364840778061620, 2.259292476615697876, 13.77329220150635969 ) ) ;
#126902 = LINE ( 'NONE', #50099, #18649 ) ;
#126903 = LINE ( 'NONE', #136371, #79335 ) ;
#126904 = EDGE_CURVE ( 'NONE', #81952, #35824, #126395, .T. ) ;
#126905 = ORIENTED_EDGE ( 'NONE', *, *, #62455, .F. ) ;
#126906 = DIRECTION ( 'NONE',  ( 0.7071067811865487940, 0.7071067811865463515, -0.000000000000000000 ) ) ;
#126907 = AXIS2_PLACEMENT_3D ( 'NONE', #52890, #98561, #97094 ) ;
#126909 = EDGE_CURVE ( 'NONE', #56401, #73002, #82224, .T. ) ;
#126908 = LINE ( 'NONE', #71872, #65586 ) ;
#126910 = ORIENTED_EDGE ( 'NONE', *, *, #94572, .F. ) ;
#126911 = VECTOR ( 'NONE', #24331, 1000.000000000000000 ) ;
#126913 = ORIENTED_EDGE ( 'NONE', *, *, #125512, .F. ) ;
#126912 = DIRECTION ( 'NONE',  ( 0.6830127018922180770, -0.6830127018922202975, -0.2588190451025213501 ) ) ;
#126914 = EDGE_CURVE ( 'NONE', #84947, #75086, #103214, .T. ) ;
#126915 = EDGE_CURVE ( 'NONE', #38388, #102218, #71327, .T. ) ;
#126916 = VERTEX_POINT ( 'NONE', #45075 ) ;
#126917 = DIRECTION ( 'NONE',  ( 0.6830127018922180770, -0.6830127018922204085, -0.2588190451025213501 ) ) ;
#126918 = DIRECTION ( 'NONE',  ( -0.5735764363510507113, 0.8191520442889885789, 1.003171929053520926E-16 ) ) ;
#126919 = VECTOR ( 'NONE', #129022, 999.9999999999998863 ) ;
#126920 = ORIENTED_EDGE ( 'NONE', *, *, #139354, .F. ) ;
#126921 = DIRECTION ( 'NONE',  ( 0.6830127018922181881, 0.6830127018922202975, -0.2588190451025214056 ) ) ;
#126922 = VECTOR ( 'NONE', #12924, 999.9999999999998863 ) ;
#126923 = EDGE_CURVE ( 'NONE', #73333, #61904, #111718, .T. ) ;
#126924 = EDGE_CURVE ( 'NONE', #107783, #94758, #55928, .T. ) ;
#126925 = DIRECTION ( 'NONE',  ( 0.7071067811865486830, -0.7071067811865464625, -0.000000000000000000 ) ) ;
#126926 = CARTESIAN_POINT ( 'NONE',  ( -33.79289321881321939, 0.7592924766157086447, 5.000000000000000000 ) ) ;
#126927 = EDGE_CURVE ( 'NONE', #127775, #138069, #34523, .T. ) ;
#126928 = EDGE_LOOP ( 'NONE', ( #22143, #114363, #94889, #62558 ) ) ;
#126929 = LINE ( 'NONE', #6543, #138785 ) ;
#126930 = CARTESIAN_POINT ( 'NONE',  ( -33.71757738642545377, -21.73023691814492864, 5.000000000000000888 ) ) ;
#126931 = ADVANCED_FACE ( 'NONE', ( #113122 ), #134191, .T. ) ;
#126932 = DIRECTION ( 'NONE',  ( -0.7071067811865486830, -0.7071067811865464625, 0.000000000000000000 ) ) ;
#126933 = CARTESIAN_POINT ( 'NONE',  ( 2.000000000000011546, 2.638703287232806449, -5.494203305479936184 ) ) ;
#126934 = CARTESIAN_POINT ( 'NONE',  ( 21.66240673564756491, 2.337593264352435085, 0.000000000000000000 ) ) ;
#126936 = VECTOR ( 'NONE', #100208, 1000.000000000000114 ) ;
#126935 = CARTESIAN_POINT ( 'NONE',  ( 0.000000000000000000, 0.000000000000000000, 5.000000000000000000 ) ) ;
#126937 = DIRECTION ( 'NONE',  ( -0.3543493200069163240, 0.000000000000000000, 0.9351131265310288487 ) ) ;
#126938 = EDGE_CURVE ( 'NONE', #34187, #16081, #68949, .T. ) ;
#126939 = CARTESIAN_POINT ( 'NONE',  ( 75.48921356237309510, -27.52281430457107803, 5.000000000000000000 ) ) ;
#126940 = CARTESIAN_POINT ( 'NONE',  ( 34.49999999999975842, -2.173586137069107860, -4.605770156576030949 ) ) ;
#126941 = ORIENTED_EDGE ( 'NONE', *, *, #4857, .F. ) ;
#126942 = VERTEX_POINT ( 'NONE', #782 ) ;
#126943 = ORIENTED_EDGE ( 'NONE', *, *, #51510, .T. ) ;
#126945 = EDGE_CURVE ( 'NONE', #74861, #46809, #11402, .T. ) ;
#126944 = CARTESIAN_POINT ( 'NONE',  ( 116.9375000000000142, 5.819803920172573974, -5.819803920172572198 ) ) ;
#126946 = VECTOR ( 'NONE', #91831, 1000.000000000000000 ) ;
#126947 = VERTEX_POINT ( 'NONE', #122571 ) ;
#126948 = ORIENTED_EDGE ( 'NONE', *, *, #59069, .F. ) ;
#126949 = ORIENTED_EDGE ( 'NONE', *, *, #54109, .F. ) ;
#126950 = AXIS2_PLACEMENT_3D ( 'NONE', #65690, #9820, #1064 ) ;
#126951 = CARTESIAN_POINT ( 'NONE',  ( 0.000000000000000000, 0.000000000000000000, 5.000000000000000000 ) ) ;
#126952 = EDGE_LOOP ( 'NONE', ( #5631, #122309, #14743, #79935 ) ) ;
#126953 = DIRECTION ( 'NONE',  ( -0.7071067811865487940, 0.7071067811865463515, -0.000000000000000000 ) ) ;
#126954 = VECTOR ( 'NONE', #20650, 1000.000000000000000 ) ;
#126955 = EDGE_CURVE ( 'NONE', #61664, #77672, #12385, .T. ) ;
#126956 = CARTESIAN_POINT ( 'NONE',  ( -50.99451991528749062, 28.92564299267973738, 4.000000000000000000 ) ) ;
#126957 = STYLED_ITEM ( 'NONE', ( #32591 ), #107130 ) ;
#126958 = LINE ( 'NONE', #17489, #34747 ) ;
#126959 = CARTESIAN_POINT ( 'NONE',  ( -27.48921356237309155, -27.52281430457074762, 5.000000000000000000 ) ) ;
#126960 = CARTESIAN_POINT ( 'NONE',  ( 114.7712635252314186, 4.472830434245839371, 4.472830434245842035 ) ) ;
#126961 = VERTEX_POINT ( 'NONE', #89939 ) ;
#126962 = CARTESIAN_POINT ( 'NONE',  ( -16.45742106731621845, 0.9613713492673547911, -33.49048331797055766 ) ) ;
#126963 = DIRECTION ( 'NONE',  ( 0.7071067811865486830, -0.7071067811865464625, -0.000000000000000000 ) ) ;
#126964 = CARTESIAN_POINT ( 'NONE',  ( 25.49999999999983658, 19.08746187583905041, 4.000000000000000000 ) ) ;
#126965 = DIRECTION ( 'NONE',  ( -1.000000000000000000, 0.000000000000000000, 0.000000000000000000 ) ) ;
#126966 = EDGE_CURVE ( 'NONE', #17946, #134862, #78380, .T. ) ;
#126967 = CARTESIAN_POINT ( 'NONE',  ( -42.18398860626899705, 28.73617430169816700, 5.000000000000000000 ) ) ;
#126968 = CARTESIAN_POINT ( 'NONE',  ( -48.18398860626899705, 28.73617430169820608, 5.000000000000000000 ) ) ;
#126969 = CARTESIAN_POINT ( 'NONE',  ( 35.80836038379622721, 7.949999999999997513, 2.130196079827431088 ) ) ;
#126970 = PLANE ( 'NONE',  #37461 ) ;
#126971 = CARTESIAN_POINT ( 'NONE',  ( -69.18398860626899705, 28.73617430169835529, 5.000000000000000000 ) ) ;
#126972 = EDGE_LOOP ( 'NONE', ( #51965, #75751, #85949, #8073 ) ) ;
#126973 = VERTEX_POINT ( 'NONE', #81249 ) ;
#126974 = CARTESIAN_POINT ( 'NONE',  ( 35.99999999999999289, 0.000000000000000000, -7.950000000000000178 ) ) ;
#126975 = ORIENTED_EDGE ( 'NONE', *, *, #129093, .F. ) ;
#126976 = CARTESIAN_POINT ( 'NONE',  ( 5.816011393731002066, 28.73617430169783304, 5.000000000000000000 ) ) ;
#126977 = CARTESIAN_POINT ( 'NONE',  ( -20.99451991528748707, 28.92564299267952777, 4.000000000000000000 ) ) ;
#126978 = ORIENTED_EDGE ( 'NONE', *, *, #118474, .T. ) ;
#126979 = VECTOR ( 'NONE', #128331, 1000.000000000000227 ) ;
#126980 = DIRECTION ( 'NONE',  ( 0.7071067811865487940, -0.7071067811865463515, 0.000000000000000000 ) ) ;
#126982 = VECTOR ( 'NONE', #118375, 1000.000000000000000 ) ;
#126981 = DIRECTION ( 'NONE',  ( 0.6830127018922180770, -0.6830127018922204085, -0.2588190451025213501 ) ) ;
#126983 = DIRECTION ( 'NONE',  ( 0.7071067811865486830, -0.7071067811865464625, -0.000000000000000000 ) ) ;
#126984 = CARTESIAN_POINT ( 'NONE',  ( -33.18398860626899705, 28.73617430169810305, 5.000000000000000000 ) ) ;
#126985 = EDGE_CURVE ( 'NONE', #45188, #13042, #134929, .T. ) ;
#126986 = CARTESIAN_POINT ( 'NONE',  ( 31.50043019189810423, -3.055000000000002380, 5.291415217122920289 ) ) ;
#126987 = ORIENTED_EDGE ( 'NONE', *, *, #103217, .F. ) ;
#126988 = ADVANCED_FACE ( 'NONE', ( #133475 ), #70405, .T. ) ;
#126989 = DIRECTION ( 'NONE',  ( 0.7071067811865487940, 0.7071067811865463515, 0.000000000000000000 ) ) ;
#126990 = ORIENTED_EDGE ( 'NONE', *, *, #93063, .F. ) ;
#126991 = CARTESIAN_POINT ( 'NONE',  ( 17.99999999999987566, 14.87792677143811026, -11.06722581663436067 ) ) ;
#126992 = SURFACE_STYLE_USAGE ( .BOTH. , #82811 ) ;
#126994 = EDGE_CURVE ( 'NONE', #124430, #88917, #57359, .T. ) ;
#126993 = CARTESIAN_POINT ( 'NONE',  ( 11.99999999999991296, 18.08204922493374056, 0.9627537363044594843 ) ) ;
#126995 = CARTESIAN_POINT ( 'NONE',  ( 1.499999999999990896, -5.568876922607761237, 4.000000000000000000 ) ) ;
#126996 = EDGE_LOOP ( 'NONE', ( #96877, #75542, #75195, #21577 ) ) ;
#126997 = CARTESIAN_POINT ( 'NONE',  ( 55.56293019189809712, 1.637169565754157174, 6.110000000000002984 ) ) ;
#126998 = EDGE_LOOP ( 'NONE', ( #129893, #68284, #143325, #51151 ) ) ;
#126999 = CARTESIAN_POINT ( 'NONE',  ( 10.17183060077640810, 15.75929247661557042, 4.000000000000000000 ) ) ;
#127000 = FACE_OUTER_BOUND ( 'NONE', #120138, .T. ) ;
#127001 = DIRECTION ( 'NONE',  ( -0.3543493200069162685, -0.000000000000000000, -0.9351131265310288487 ) ) ;
#127002 = CARTESIAN_POINT ( 'NONE',  ( 39.18398860626899705, 28.73617430169814568, 5.000000000000000000 ) ) ;
#127003 = CARTESIAN_POINT ( 'NONE',  ( 52.26626352523145158, 4.472830434245839371, -4.472830434245838482 ) ) ;
#127004 = VERTEX_POINT ( 'NONE', #69667 ) ;
#127005 = CARTESIAN_POINT ( 'NONE',  ( -57.48921356237308800, -27.52281430457095368, 5.000000000000000000 ) ) ;
#127006 = EDGE_CURVE ( 'NONE', #89438, #131559, #92081, .T. ) ;
#127007 = DIRECTION ( 'NONE',  ( 0.000000000000000000, 1.000000000000000000, 0.000000000000000000 ) ) ;
#127008 = ORIENTED_EDGE ( 'NONE', *, *, #16168, .F. ) ;
#127009 = ORIENTED_EDGE ( 'NONE', *, *, #45403, .F. ) ;
#127010 = DIRECTION ( 'NONE',  ( 0.6830127018922180770, -0.6830127018922204085, -0.2588190451025213501 ) ) ;
#127011 = ORIENTED_EDGE ( 'NONE', *, *, #124002, .F. ) ;
#127012 = VECTOR ( 'NONE', #84177, 1000.000000000000227 ) ;
#127013 = PLANE ( 'NONE',  #4776 ) ;
#127014 = EDGE_CURVE ( 'NONE', #101752, #45062, #36301, .T. ) ;
#127015 = ORIENTED_EDGE ( 'NONE', *, *, #132572, .F. ) ;
#127016 = CARTESIAN_POINT ( 'NONE',  ( 44.85002705046287730, -5.819803920172573086, -5.819803920172573086 ) ) ;
#127017 = AXIS2_PLACEMENT_3D ( 'NONE', #107236, #132609, #30405 ) ;
#127018 = VECTOR ( 'NONE', #46195, 1000.000000000000000 ) ;
#127019 = VECTOR ( 'NONE', #127577, 1000.000000000000000 ) ;
#127020 = LINE ( 'NONE', #37912, #118346 ) ;
#127021 = AXIS2_PLACEMENT_3D ( 'NONE', #49341, #126160, #24685 ) ;
#127022 = EDGE_CURVE ( 'NONE', #9261, #88406, #67524, .T. ) ;
#127023 = FACE_BOUND ( 'NONE', #105202, .T. ) ;
#127024 = CARTESIAN_POINT ( 'NONE',  ( 24.81246187583929697, -22.22500000000000142, 4.000000000000000000 ) ) ;
#127025 = CARTESIAN_POINT ( 'NONE',  ( 66.48921356237309510, -27.52281430457101763, 5.000000000000000000 ) ) ;
#127026 = DIRECTION ( 'NONE',  ( -0.7071067811865486830, 0.7071067811865464625, 0.000000000000000000 ) ) ;
#127027 = EDGE_LOOP ( 'NONE', ( #59608, #69293, #91532 ) ) ;
#127028 = PLANE ( 'NONE',  #112866 ) ;
#127030 = VERTEX_POINT ( 'NONE', #56670 ) ;
#127029 = CARTESIAN_POINT ( 'NONE',  ( -18.48921356237309510, -27.52281430457068367, 5.000000000000000000 ) ) ;
#127031 = ORIENTED_EDGE ( 'NONE', *, *, #13063, .F. ) ;
#127032 = VECTOR ( 'NONE', #95508, 1000.000000000000000 ) ;
#127033 = VECTOR ( 'NONE', #14060, 999.9999999999998863 ) ;
#127034 = CARTESIAN_POINT ( 'NONE',  ( -63.48921356237309510, -27.52281430457099631, 5.000000000000000000 ) ) ;
#127035 = VERTEX_POINT ( 'NONE', #34162 ) ;
#127036 = EDGE_LOOP ( 'NONE', ( #114259, #17226, #88193, #137790 ) ) ;
#127037 = CARTESIAN_POINT ( 'NONE',  ( 69.18293019189809456, -1.637169565754158951, -6.109999999999998543 ) ) ;
#127038 = ORIENTED_EDGE ( 'NONE', *, *, #139230, .F. ) ;
#127039 = CARTESIAN_POINT ( 'NONE',  ( -24.18398860626899705, 28.73617430169804265, 5.000000000000000000 ) ) ;
#127040 = CARTESIAN_POINT ( 'NONE',  ( 6.229065384000522343, 3.821174125832445049E-16, 0.000000000000000000 ) ) ;
#127041 = EDGE_LOOP ( 'NONE', ( #28511, #64024, #52696, #13249 ) ) ;
#127042 = LINE ( 'NONE', #114731, #116207 ) ;
#127043 = VECTOR ( 'NONE', #102890, 1000.000000000000000 ) ;
#127044 = VECTOR ( 'NONE', #36754, 999.9999999999998863 ) ;
#127046 = EDGE_CURVE ( 'NONE', #129380, #21344, #27563, .T. ) ;
#127045 =( BOUNDED_CURVE ( )  B_SPLINE_CURVE ( 2, ( #54890, #128851, #32416, #64323, #53437, #84650, #118692, #97651, #19383, #52711, #120084, #31000, #86799 ),
 .UNSPECIFIED., .F., .F. ) 
 B_SPLINE_CURVE_WITH_KNOTS ( ( 3, 2, 2, 2, 2, 2, 3 ),
 ( 0.3333333333333333148, 0.3361111111111111382, 0.3388888888888889062, 0.3416666666666666741, 0.3444444444444444975, 0.3472222222222222654, 0.3500000000000000333 ),
 .UNSPECIFIED. ) 
 CURVE ( )  GEOMETRIC_REPRESENTATION_ITEM ( )  RATIONAL_B_SPLINE_CURVE ( ( 1.000000000000000000, 0.9659258262890683122, 1.000000000000000000, 0.9659258262890683122, 1.000000000000000000, 0.9659258262890683122, 1.000000000000000000, 0.9659258262890683122, 1.000000000000000000, 0.9659258262890683122, 1.000000000000000000, 0.9659258262890676461, 1.000000000000000666 ) ) 
 REPRESENTATION_ITEM ( '' )  );
#127047 = AXIS2_PLACEMENT_3D ( 'NONE', #5521, #83861, #72287 ) ;
#127048 = EDGE_CURVE ( 'NONE', #90674, #87848, #58820, .T. ) ;
#127049 = DIRECTION ( 'NONE',  ( -0.7071067811865486830, -0.7071067811865464625, 0.000000000000000000 ) ) ;
#127050 = CARTESIAN_POINT ( 'NONE',  ( -6.707106781186489286, -6.740707523384216415, 5.000000000000000000 ) ) ;
#127051 = CARTESIAN_POINT ( 'NONE',  ( 0.000000000000000000, 0.000000000000000000, 5.000000000000000000 ) ) ;
#127052 = CARTESIAN_POINT ( 'NONE',  ( 17.50000000000000000, 0.000000000000000000, 6.094999999999989981 ) ) ;
#127053 = CARTESIAN_POINT ( 'NONE',  ( 29.99999999999979394, -9.412538124160654718, 4.000000000000000000 ) ) ;
#127054 = ORIENTED_EDGE ( 'NONE', *, *, #23334, .T. ) ;
#127055 = VECTOR ( 'NONE', #105886, 1000.000000000000227 ) ;
#127056 = ORIENTED_EDGE ( 'NONE', *, *, #22006, .F. ) ;
#127057 = VECTOR ( 'NONE', #80655, 1000.000000000000000 ) ;
#127058 = DIRECTION ( 'NONE',  ( 0.000000000000000000, -1.000000000000000000, 0.000000000000000000 ) ) ;
#127059 =( BOUNDED_CURVE ( )  B_SPLINE_CURVE ( 3, ( #84932, #85629, #129145, #76204 ),
 .UNSPECIFIED., .F., .T. ) 
 B_SPLINE_CURVE_WITH_KNOTS ( ( 4, 4 ),
 ( 5.005968288816728062, 5.074607125596327428 ),
 .UNSPECIFIED. ) 
 CURVE ( )  GEOMETRIC_REPRESENTATION_ITEM ( )  RATIONAL_B_SPLINE_CURVE ( ( 1.000000000000000000, 0.9996074310407765395, 0.9996074310407765395, 1.000000000000000000 ) ) 
 REPRESENTATION_ITEM ( '' )  );
#127060 = LINE ( 'NONE', #36497, #69835 ) ;
#127061 = VERTEX_POINT ( 'NONE', #3619 ) ;
#127062 = VECTOR ( 'NONE', #25854, 1000.000000000000000 ) ;
#127063 = ORIENTED_EDGE ( 'NONE', *, *, #9915, .T. ) ;
#127064 = STYLED_ITEM ( 'NONE', ( #119263 ), #94738 ) ;
#127065 = VERTEX_POINT ( 'NONE', #47916 ) ;
#127066 = DIRECTION ( 'NONE',  ( -0.7071067811865486830, 0.7071067811865464625, 0.000000000000000000 ) ) ;
#127067 = EDGE_CURVE ( 'NONE', #102743, #122233, #2082, .T. ) ;
#127068 = FACE_OUTER_BOUND ( 'NONE', #96322, .T. ) ;
#127069 = ORIENTED_EDGE ( 'NONE', *, *, #58611, .F. ) ;
#127070 = VECTOR ( 'NONE', #88466, 1000.000000000000000 ) ;
#127071 = LINE ( 'NONE', #116206, #76416 ) ;
#127072 = CIRCLE ( 'NONE', #106249, 2.500000000000000888 ) ;
#127073 = DIRECTION ( 'NONE',  ( 0.7071067811865487940, 0.7071067811865463515, 0.000000000000000000 ) ) ;
#127074 = CARTESIAN_POINT ( 'NONE',  ( 11.58790314143521982, 6.871911579029515771, 3.967499999999989146 ) ) ;
#127075 = FACE_OUTER_BOUND ( 'NONE', #112436, .T. ) ;
#127076 = ORIENTED_EDGE ( 'NONE', *, *, #107743, .F. ) ;
#127077 = DIRECTION ( 'NONE',  ( -0.7071067811865487940, 0.7071067811865463515, 0.000000000000000000 ) ) ;
#127078 = CARTESIAN_POINT ( 'NONE',  ( 24.79166666666667140, -3.047499999999994547, 5.278424836066145431 ) ) ;
#127079 = VECTOR ( 'NONE', #93218, 999.9999999999998863 ) ;
#127081 = ORIENTED_EDGE ( 'NONE', *, *, #118790, .T. ) ;
#127080 = FACE_OUTER_BOUND ( 'NONE', #136369, .T. ) ;
#127082 = LINE ( 'NONE', #72039, #51703 ) ;
#127083 = EDGE_LOOP ( 'NONE', ( #18621, #46090, #44842, #88820 ) ) ;
#127084 = CARTESIAN_POINT ( 'NONE',  ( 7.499999999999951150, -12.08601207473287964, -10.46905243149095988 ) ) ;
#127085 = DIRECTION ( 'NONE',  ( -0.7071067811865486830, -0.7071067811865464625, -0.000000000000000000 ) ) ;
#127086 = DIRECTION ( 'NONE',  ( -0.6830127018922180770, -0.6830127018922204085, -0.2588190451025213501 ) ) ;
#127087 = ORIENTED_EDGE ( 'NONE', *, *, #76752, .T. ) ;
#127088 = LINE ( 'NONE', #72050, #91217 ) ;
#127089 = FACE_OUTER_BOUND ( 'NONE', #68462, .T. ) ;
#127090 = CARTESIAN_POINT ( 'NONE',  ( -34.42500000000001137, 0.000000000000000000, 4.500000000000000888 ) ) ;
#127091 = ORIENTED_EDGE ( 'NONE', *, *, #123840, .T. ) ;
#127092 = DIRECTION ( 'NONE',  ( 0.7071067811865487940, 0.7071067811865463515, 0.000000000000000000 ) ) ;
#127093 = CARTESIAN_POINT ( 'NONE',  ( -27.18398860626900060, 28.73617430169806042, 5.000000000000000000 ) ) ;
#127094 = DIRECTION ( 'NONE',  ( 0.7071067811865487940, 0.7071067811865463515, 0.000000000000000000 ) ) ;
#127095 = LINE ( 'NONE', #93055, #58816 ) ;
#127096 = DIRECTION ( 'NONE',  ( 0.000000000000000000, -1.000000000000000000, 0.000000000000000000 ) ) ;
#127097 = ORIENTED_EDGE ( 'NONE', *, *, #39241, .F. ) ;
#127098 = ORIENTED_EDGE ( 'NONE', *, *, #27301, .F. ) ;
#127099 = CARTESIAN_POINT ( 'NONE',  ( 33.18398860626899705, 28.73617430169810305, 5.000000000000000000 ) ) ;
#127100 = CARTESIAN_POINT ( 'NONE',  ( 12.18398860626900060, 28.73617430169795739, 5.000000000000000000 ) ) ;
#127101 = CARTESIAN_POINT ( 'NONE',  ( 5.374569808101886892, 6.871911579029510442, -3.967499999999998916 ) ) ;
#127102 = CARTESIAN_POINT ( 'NONE',  ( 21.59770000000000323, 3.130000000000007887, -22.35000000000000142 ) ) ;
#127103 = EDGE_CURVE ( 'NONE', #14082, #7225, #31018, .T. ) ;
#127104 = CARTESIAN_POINT ( 'NONE',  ( -30.29974487139158867, -27.71228299555227537, 4.000000000000000000 ) ) ;
#127105 = CARTESIAN_POINT ( 'NONE',  ( 0.000000000000000000, 0.000000000000000000, 5.000000000000000000 ) ) ;
#127106 = DIRECTION ( 'NONE',  ( 0.000000000000000000, 1.000000000000000000, 0.000000000000000000 ) ) ;
#127107 = ADVANCED_FACE ( 'NONE', ( #131750 ), #19402, .F. ) ;
#127108 = ORIENTED_EDGE ( 'NONE', *, *, #88725, .F. ) ;
#127109 = FACE_OUTER_BOUND ( 'NONE', #109926, .T. ) ;
#127110 = EDGE_CURVE ( 'NONE', #18669, #94043, #63654, .T. ) ;
#127111 = FACE_OUTER_BOUND ( 'NONE', #128672, .T. ) ;
#127112 = CARTESIAN_POINT ( 'NONE',  ( 32.99999999999976552, 10.93112307739207623, 4.000000000000000000 ) ) ;
#127113 = ADVANCED_FACE ( 'NONE', ( #141169 ), #108514, .T. ) ;
#127114 = CARTESIAN_POINT ( 'NONE',  ( 50.95376352523145158, -6.109999999999999432, -3.741295971395163529E-16 ) ) ;
#127115 = PLANE ( 'NONE',  #88171 ) ;
#127116 = EDGE_LOOP ( 'NONE', ( #6517, #135262, #75494, #70199 ) ) ;
#127117 =( NAMED_UNIT ( * ) SI_UNIT ( $, .STERADIAN. ) SOLID_ANGLE_UNIT ( ) );
#127118 = VERTEX_POINT ( 'NONE', #131033 ) ;
#127119 = EDGE_CURVE ( 'NONE', #42800, #122052, #99820, .T. ) ;
#127120 = ORIENTED_EDGE ( 'NONE', *, *, #70732, .F. ) ;
#127121 = DIRECTION ( 'NONE',  ( -0.000000000000000000, -0.3543493200069152693, 0.9351131265310292928 ) ) ;
#127122 = AXIS2_PLACEMENT_3D ( 'NONE', #72186, #83023, #14892 ) ;
#127123 = VECTOR ( 'NONE', #102983, 1000.000000000000000 ) ;
#127124 = CIRCLE ( 'NONE', #18335, 3.000000000000002665 ) ;
#127125 = DIRECTION ( 'NONE',  ( 0.7071067811865486830, -0.7071067811865464625, -0.000000000000000000 ) ) ;
#127126 = CARTESIAN_POINT ( 'NONE',  ( 0.000000000000000000, 0.000000000000000000, 5.000000000000000000 ) ) ;
#127127 = VECTOR ( 'NONE', #3969, 1000.000000000000000 ) ;
#127128 = ADVANCED_FACE ( 'NONE', ( #110661 ), #485, .F. ) ;
#127129 = LINE ( 'NONE', #135879, #9276 ) ;
#127130 = ADVANCED_FACE ( 'NONE', ( #33182 ), #119402, .F. ) ;
#127131 = CARTESIAN_POINT ( 'NONE',  ( 54.48921356237310221, -27.52281430457093236, 5.000000000000000000 ) ) ;
#127132 = PLANE ( 'NONE',  #110152 ) ;
#127133 = ORIENTED_EDGE ( 'NONE', *, *, #142233, .T. ) ;
#127134 = LINE ( 'NONE', #27109, #25538 ) ;
#127135 = CARTESIAN_POINT ( 'NONE',  ( -14.70025512860841133, -27.71228299555195917, 4.000000000000000000 ) ) ;
#127136 = UNCERTAINTY_MEASURE_WITH_UNIT (LENGTH_MEASURE( 1.000000000000000082E-05 ), #59065, 'distance_accuracy_value', 'NONE');
#127137 = MECHANICAL_DESIGN_GEOMETRIC_PRESENTATION_REPRESENTATION (  '', ( #99284 ), #110867 ) ;
#127138 = DIRECTION ( 'NONE',  ( -0.3543493200069162685, -0.000000000000000000, -0.9351131265310288487 ) ) ;
#127139 = LINE ( 'NONE', #91664, #65914 ) ;
#127140 = EDGE_CURVE ( 'NONE', #142129, #131532, #42620, .T. ) ;
#127141 = CARTESIAN_POINT ( 'NONE',  ( 103.1833603837962130, -2.130196079827426203, 7.949999999999996625 ) ) ;
#127142 = CARTESIAN_POINT ( 'NONE',  ( 61.91252705046289151, -7.949999999999998401, -4.867971026610728450E-16 ) ) ;
#127143 = CARTESIAN_POINT ( 'NONE',  ( 4.031635159221891307, 2.259292476615694323, 13.77329220150638456 ) ) ;
#127144 = ORIENTED_EDGE ( 'NONE', *, *, #16379, .T. ) ;
#127145 = ORIENTED_EDGE ( 'NONE', *, *, #19558, .F. ) ;
#127146 = CARTESIAN_POINT ( 'NONE',  ( 64.72916666666667140, 7.950000000000001954, -2.130196079827421762 ) ) ;
#127147 = LINE ( 'NONE', #85078, #30864 ) ;
#127148 = LINE ( 'NONE', #105396, #97123 ) ;
#127149 = PRESENTATION_LAYER_ASSIGNMENT (  '', '', ( #138769 ) ) ;
#127150 = CIRCLE ( 'NONE', #2108, 2.500000000000000888 ) ;
#127151 = ORIENTED_EDGE ( 'NONE', *, *, #111181, .F. ) ;
#127152 = CARTESIAN_POINT ( 'NONE',  ( 22.85159235450332105, 3.061616997868380183E-16, -2.500000000000001332 ) ) ;
#127153 = VECTOR ( 'NONE', #142335, 999.9999999999998863 ) ;
#127154 = LINE ( 'NONE', #105401, #132429 ) ;
#127155 = CARTESIAN_POINT ( 'NONE',  ( 60.22959685856476142, -6.110000000000000320, -1.637169565754161393 ) ) ;
#127156 = EDGE_CURVE ( 'NONE', #115946, #68778, #109267, .T. ) ;
#127157 = FACE_OUTER_BOUND ( 'NONE', #123181, .T. ) ;
#127158 = VERTEX_POINT ( 'NONE', #21553 ) ;
#127159 = ORIENTED_EDGE ( 'NONE', *, *, #50186, .T. ) ;
#127160 = CARTESIAN_POINT ( 'NONE',  ( -2.999999999999976463, -0.03360074219773551141, 5.000000000000000000 ) ) ;
#127161 = AXIS2_PLACEMENT_3D ( 'NONE', #56269, #45379, #133784 ) ;
#127162 = AXIS2_PLACEMENT_3D ( 'NONE', #122859, #130909, #54076 ) ;
#127163 = DIRECTION ( 'NONE',  ( -0.000000000000000000, 0.3543493200069153248, 0.9351131265310292928 ) ) ;
#127164 = FACE_OUTER_BOUND ( 'NONE', #121468, .T. ) ;
#127165 = VECTOR ( 'NONE', #14453, 1000.000000000000000 ) ;
#127166 = DIRECTION ( 'NONE',  ( -0.6830127018922181881, 0.6830127018922202975, -0.2588190451025214056 ) ) ;
#127167 = CARTESIAN_POINT ( 'NONE',  ( -8.903329358125901649, -2.240707523384260824, 15.26439735382750484 ) ) ;
#127169 = ORIENTED_EDGE ( 'NONE', *, *, #128575, .F. ) ;
#127168 = DIRECTION ( 'NONE',  ( 0.7071067811865486830, -0.7071067811865464625, -0.000000000000000000 ) ) ;
#127170 = DIRECTION ( 'NONE',  ( -0.7071067811865486830, -0.7071067811865464625, 0.000000000000000000 ) ) ;
#127171 = CARTESIAN_POINT ( 'NONE',  ( 1.040834085586084257E-14, 11.58746187583913034, 4.000000000000000000 ) ) ;
#127172 = CARTESIAN_POINT ( 'NONE',  ( -24.79333936457829779, 21.75929247661549581, 4.998822639870701856 ) ) ;
#127173 = VECTOR ( 'NONE', #80285, 1000.000000000000000 ) ;
#127174 = DIRECTION ( 'NONE',  ( 0.6830127018922180770, -0.6830127018922204085, -0.2588190451025213501 ) ) ;
#127175 = VECTOR ( 'NONE', #55449, 999.9999999999998863 ) ;
#127176 = EDGE_CURVE ( 'NONE', #16650, #27906, #65815, .T. ) ;
#127177 = VERTEX_POINT ( 'NONE', #143321 ) ;
#127178 = ORIENTED_EDGE ( 'NONE', *, *, #68491, .T. ) ;
#127179 = PLANE ( 'NONE',  #1367 ) ;
#127180 = CARTESIAN_POINT ( 'NONE',  ( 21.48921356237309155, -27.52281430457070499, 5.000000000000000000 ) ) ;
#127181 = DIRECTION ( 'NONE',  ( -0.5735764363510501562, 0.8191520442889890230, 1.003171929053521419E-16 ) ) ;
#127182 = ADVANCED_FACE ( 'NONE', ( #44026 ), #88243, .F. ) ;
#127183 = DIRECTION ( 'NONE',  ( -0.7071067811865486830, -0.7071067811865464625, 0.000000000000000000 ) ) ;
#127184 = CARTESIAN_POINT ( 'NONE',  ( -29.99999999999979039, -0.8619312979532244290, -5.102805207349895511 ) ) ;
#127185 = EDGE_LOOP ( 'NONE', ( #127954, #48878, #22354, #75645 ) ) ;
#127186 = ORIENTED_EDGE ( 'NONE', *, *, #2329, .F. ) ;
#127187 = AXIS2_PLACEMENT_3D ( 'NONE', #142975, #117623, #18309 ) ;
#127188 = DIRECTION ( 'NONE',  ( -0.7071067811865486830, -0.7071067811865464625, 0.000000000000000000 ) ) ;
#127189 = CARTESIAN_POINT ( 'NONE',  ( 64.00000000000000000, 0.000000000000000000, -7.950000000000000178 ) ) ;
#127190 = VERTEX_POINT ( 'NONE', #114264 ) ;
#127191 = ORIENTED_EDGE ( 'NONE', *, *, #89221, .T. ) ;
#127192 = ADVANCED_FACE ( 'NONE', ( #57779 ), #78797, .T. ) ;
#127193 = DIRECTION ( 'NONE',  ( 1.000000000000000000, 0.000000000000000000, 0.000000000000000000 ) ) ;
#127194 = ORIENTED_EDGE ( 'NONE', *, *, #86110, .T. ) ;
#127195 = PLANE ( 'NONE',  #10913 ) ;
#127196 = CARTESIAN_POINT ( 'NONE',  ( -69.18398860626899705, 28.73617430169835529, 5.000000000000000000 ) ) ;
#127197 = EDGE_CURVE ( 'NONE', #13173, #108474, #100397, .T. ) ;
#127198 = FACE_BOUND ( 'NONE', #43485, .T. ) ;
#127199 = FACE_OUTER_BOUND ( 'NONE', #139353, .T. ) ;
#127200 = APPLICATION_CONTEXT ( 'automotive_design' ) ;
#127201 = CARTESIAN_POINT ( 'NONE',  ( 0.1161069444170876597, 0.000000000000000000, 0.000000000000000000 ) ) ;
#127203 = VERTEX_POINT ( 'NONE', #14236 ) ;
#127202 = CARTESIAN_POINT ( 'NONE',  ( 54.18398860626899705, 28.73617430169825226, 5.000000000000000000 ) ) ;
#127204 = DIRECTION ( 'NONE',  ( -0.3543493200069162685, -0.000000000000000000, -0.9351131265310288487 ) ) ;
#127205 = SHAPE_DEFINITION_REPRESENTATION ( #60877, #104156 ) ;
#127206 = ORIENTED_EDGE ( 'NONE', *, *, #105908, .F. ) ;
#127207 = ORIENTED_EDGE ( 'NONE', *, *, #116017, .T. ) ;
#127208 = CARTESIAN_POINT ( 'NONE',  ( 90.76626352523145158, 4.472830434245838482, -4.472830434245837594 ) ) ;
#127209 = ORIENTED_EDGE ( 'NONE', *, *, #21178, .F. ) ;
#127210 = CARTESIAN_POINT ( 'NONE',  ( -42.18398860626899705, 28.73617430169816700, 5.000000000000000000 ) ) ;
#127211 = DIRECTION ( 'NONE',  ( -0.7071067811865486830, -0.7071067811865464625, 0.000000000000000000 ) ) ;
#127212 = DIRECTION ( 'NONE',  ( 1.000000000000000000, 0.000000000000000000, -0.000000000000000000 ) ) ;
#127213 = EDGE_LOOP ( 'NONE', ( #57892, #29866, #22481, #83265 ) ) ;
#127214 = CARTESIAN_POINT ( 'NONE',  ( 20.99999999999985789, -11.35517001088070010, -1.126524801160061262 ) ) ;
#127215 = EDGE_CURVE ( 'NONE', #108894, #116464, #1195, .T. ) ;
#127216 = DIRECTION ( 'NONE',  ( 1.000000000000000000, 3.115803279706882722E-16, 0.000000000000000000 ) ) ;
#127217 = CARTESIAN_POINT ( 'NONE',  ( 21.72281430457044493, -21.72500000000000142, 5.000000000000000000 ) ) ;
#127218 = PLANE ( 'NONE',  #137651 ) ;
#127219 = PLANE ( 'NONE',  #6844 ) ;
#127220 = AXIS2_PLACEMENT_3D ( 'NONE', #77872, #22728, #59703 ) ;
#127221 = CONICAL_SURFACE ( 'NONE', #64738, 2.500000000000000444, 0.9599310885968830309 ) ;
#127222 = DIRECTION ( 'NONE',  ( -0.5735764363510503783, -0.8191520442889886899, 0.000000000000000000 ) ) ;
#127223 = VECTOR ( 'NONE', #71766, 1000.000000000000000 ) ;
#127224 = ORIENTED_EDGE ( 'NONE', *, *, #24460, .F. ) ;
#127225 = DIRECTION ( 'NONE',  ( 0.7071067811865487940, 0.7071067811865463515, 0.000000000000000000 ) ) ;
#127226 = LINE ( 'NONE', #91749, #76650 ) ;
#127227 = VECTOR ( 'NONE', #120801, 1000.000000000000000 ) ;
#127228 = EDGE_LOOP ( 'NONE', ( #97910, #66162, #95390, #88360, #23171 ) ) ;
#127229 = EDGE_CURVE ( 'NONE', #31359, #29345, #76336, .T. ) ;
#127230 = ORIENTED_EDGE ( 'NONE', *, *, #96776, .F. ) ;
#127231 = EDGE_CURVE ( 'NONE', #76404, #24129, #36019, .T. ) ;
#127232 = ORIENTED_EDGE ( 'NONE', *, *, #5869, .T. ) ;
#127233 = CARTESIAN_POINT ( 'NONE',  ( 47.10459685856477563, 1.637169565754164946, -6.109999999999999432 ) ) ;
#127234 = ORIENTED_EDGE ( 'NONE', *, *, #44018, .T. ) ;
#127235 = AXIS2_PLACEMENT_3D ( 'NONE', #67430, #134837, #12297 ) ;
#127236 =( BOUNDED_SURFACE ( )  B_SPLINE_SURFACE ( 3, 2, ( 
 ( #58766, #47868, #15861 ),
 ( #70348, #94169, #113074 ),
 ( #26088, #114495, #71034 ),
 ( #115182, #48547, #13744 ),
 ( #58034, #7130, #73175 ),
 ( #84737, #28225, #51412 ),
 ( #63018, #139137, #8549 ),
 ( #127527, #50683, #118038 ),
 ( #75307, #141245, #18741 ),
 ( #95604, #116646, #97753 ),
 ( #107192, #52794, #139861 ),
 ( #31089, #107881, #74595 ),
 ( #7867, #52106, #61591 ),
 ( #29622, #96994, #94875 ),
 ( #39840, #40536, #41958 ),
 ( #84060, #96287, #18008 ) ),
 .UNSPECIFIED., .F., .F., .F. ) 
 B_SPLINE_SURFACE_WITH_KNOTS ( ( 4, 2, 2, 2, 2, 2, 2, 4 ),
 ( 3, 3 ),
 ( 6.460584911619955406, 6.634759501914270885, 6.808934092208587252, 6.983108682502903619, 7.157283272797219098, 7.331457863091534577, 7.505632453385850944, 7.853981633974482790 ),
 ( 0.000000000000000000, 1.000000000000000000 ),
 .UNSPECIFIED. ) 
 GEOMETRIC_REPRESENTATION_ITEM ( )  RATIONAL_B_SPLINE_SURFACE ( (
 ( 1.000000000000000000, 0.7180326832784528213, 1.000000000000000000),
 ( 1.000000000000000000, 0.7250426641247393889, 1.000000000000000000),
 ( 1.000000000000000000, 0.7353122387369821489, 1.000000000000000000),
 ( 1.000000000000000000, 0.7604116155349861517, 1.000000000000000000),
 ( 1.000000000000000000, 0.7752313834058587316, 1.000000000000000000),
 ( 1.000000000000000000, 0.8070860741949156258, 1.000000000000000000),
 ( 1.000000000000000000, 0.8241077986061052796, 1.000000000000000000),
 ( 1.000000000000000000, 0.8581174656086261177, 1.000000000000000000),
 ( 1.000000000000000000, 0.8751006588767553662, 1.000000000000000000),
 ( 1.000000000000000000, 0.9071649184812575761, 1.000000000000000000),
 ( 1.000000000000000000, 0.9222453908328933636, 1.000000000000000000),
 ( 1.000000000000000000, 0.9490805577170023932, 1.000000000000000000),
 ( 1.000000000000000000, 0.9608359430471253848, 1.000000000000000000),
 ( 1.000000000000000000, 0.9896287210067384876, 1.000000000000000000),
 ( 1.000000000000000000, 1.000097732991006572, 1.000000000000000000),
 ( 1.000000000000000000, 1.000000000000000000, 1.000000000000000000) ) ) 
 REPRESENTATION_ITEM ( '' )  SURFACE ( )  );
#127237 = VECTOR ( 'NONE', #8831, 1000.000000000000000 ) ;
#127238 = CARTESIAN_POINT ( 'NONE',  ( 14.62913961620377101, 5.278424836066147208, 3.047499999999990550 ) ) ;
#127239 = CARTESIAN_POINT ( 'NONE',  ( -8.338599238176856332, 10.47657132819572645, -28.51096560023557558 ) ) ;
#127240 = ORIENTED_EDGE ( 'NONE', *, *, #108431, .F. ) ;
#127241 = CARTESIAN_POINT ( 'NONE',  ( 3.707106781186525257, 5.259292476615661016, 5.000000000000000000 ) ) ;
#127242 = EDGE_LOOP ( 'NONE', ( #126537, #70656, #103767, #49239 ) ) ;
#127243 = CARTESIAN_POINT ( 'NONE',  ( 18.79333936457835108, 21.75929247661549937, 4.998822639870708073 ) ) ;
#127244 = VECTOR ( 'NONE', #118205, 1000.000000000000000 ) ;
#127245 = AXIS2_PLACEMENT_3D ( 'NONE', #97987, #40761, #96516 ) ;
#127246 = DIRECTION ( 'NONE',  ( 0.6830127018922181881, 0.6830127018922202975, -0.2588190451025214056 ) ) ;
#127248 = ORIENTED_EDGE ( 'NONE', *, *, #96276, .T. ) ;
#127247 = DIRECTION ( 'NONE',  ( 0.7071067811865487940, -0.7071067811865463515, 0.000000000000000000 ) ) ;
#127249 = EDGE_LOOP ( 'NONE', ( #121440, #95046, #82260, #78027 ) ) ;
#127250 = ADVANCED_FACE ( 'NONE', ( #4015 ), #36696, .F. ) ;
#127251 = DIRECTION ( 'NONE',  ( -0.7071067811865486830, -0.7071067811865464625, 0.000000000000000000 ) ) ;
#127252 = LINE ( 'NONE', #72934, #6786 ) ;
#127253 = ORIENTED_EDGE ( 'NONE', *, *, #9440, .F. ) ;
#127254 = AXIS2_PLACEMENT_3D ( 'NONE', #123806, #59278, #114327 ) ;
#127255 = DIRECTION ( 'NONE',  ( 0.000000000000000000, 0.000000000000000000, -1.000000000000000000 ) ) ;
#127256 = VERTEX_POINT ( 'NONE', #100548 ) ;
#127257 = EDGE_LOOP ( 'NONE', ( #65982, #45612, #72958, #38492 ) ) ;
#127258 = VERTEX_POINT ( 'NONE', #3339 ) ;
#127259 = EDGE_LOOP ( 'NONE', ( #134046, #18229, #73184, #133015 ) ) ;
#127260 = FACE_OUTER_BOUND ( 'NONE', #31368, .T. ) ;
#127261 = VECTOR ( 'NONE', #135077, 1000.000000000000227 ) ;
#127262 = AXIS2_PLACEMENT_3D ( 'NONE', #13899, #24097, #48707 ) ;
#127263 = DIRECTION ( 'NONE',  ( 0.000000000000000000, 0.000000000000000000, -1.000000000000000000 ) ) ;
#127264 = VECTOR ( 'NONE', #132534, 1000.000000000000000 ) ;
#127265 = CARTESIAN_POINT ( 'NONE',  ( -8.999999999999934275, 7.552185695429090906, 5.000000000000000000 ) ) ;
#127266 = CARTESIAN_POINT ( 'NONE',  ( 25.49999999999982592, 16.77039438581781639, 0.4657186855307159368 ) ) ;
#127267 = ORIENTED_EDGE ( 'NONE', *, *, #45906, .F. ) ;
#127268 = AXIS2_PLACEMENT_3D ( 'NONE', #104261, #115125, #139805 ) ;
#127269 = CARTESIAN_POINT ( 'NONE',  ( 67.06249999999998579, -5.819803920172573086, -5.819803920172573974 ) ) ;
#127270 = VERTEX_POINT ( 'NONE', #47625 ) ;
#127271 = VECTOR ( 'NONE', #46064, 1000.000000000000227 ) ;
#127272 = PLANE ( 'NONE',  #26291 ) ;
#127273 = CARTESIAN_POINT ( 'NONE',  ( 30.31206980810188512, 7.934999999999993392, 2.126176841940951689 ) ) ;
#127274 = LINE ( 'NONE', #71487, #57836 ) ;
#127275 = EDGE_CURVE ( 'NONE', #65672, #88912, #2631, .T. ) ;
#127276 = CARTESIAN_POINT ( 'NONE',  ( 25.74845587132409364, -11.24070752338416490, 10.39518518046003415 ) ) ;
#127277 = DIRECTION ( 'NONE',  ( -0.000000000000000000, -0.3543493200069152693, 0.9351131265310292928 ) ) ;
#127278 = EDGE_LOOP ( 'NONE', ( #116672, #44195, #25936, #15021, #69695, #88074 ) ) ;
#127279 = EDGE_CURVE ( 'NONE', #80487, #29533, #14938, .T. ) ;
#127280 = VERTEX_POINT ( 'NONE', #123011 ) ;
#127281 = ORIENTED_EDGE ( 'NONE', *, *, #137379, .T. ) ;
#127282 = CARTESIAN_POINT ( 'NONE',  ( 55.56056557994604361, -52.00875322212549179, -39.86617647058817937 ) ) ;
#127283 = PLANE ( 'NONE',  #51092 ) ;
#127284 = UNCERTAINTY_MEASURE_WITH_UNIT (LENGTH_MEASURE( 1.000000000000000082E-05 ), #7776, 'distance_accuracy_value', 'NONE');
#127285 = VECTOR ( 'NONE', #91322, 1000.000000000000000 ) ;
#127286 = DIRECTION ( 'NONE',  ( 0.6830127018922181881, 0.6830127018922202975, -0.2588190451025214056 ) ) ;
#127287 = CARTESIAN_POINT ( 'NONE',  ( 34.92499999999998295, -14.14387692260744878, 4.000000000000000000 ) ) ;
#127288 = CARTESIAN_POINT ( 'NONE',  ( 3.060608989244803180, -48.47007572038050682, -38.12657027910872642 ) ) ;
#127289 = EDGE_CURVE ( 'NONE', #139436, #36014, #25098, .T. ) ;
#127291 = EDGE_CURVE ( 'NONE', #109962, #78214, #48591, .T. ) ;
#127290 = CARTESIAN_POINT ( 'NONE',  ( 77.64126352523146579, 4.472830434245837594, 4.472830434245841147 ) ) ;
#127292 = DIRECTION ( 'NONE',  ( 0.000000000000000000, -1.000000000000000000, 0.000000000000000000 ) ) ;
#127293 = CARTESIAN_POINT ( 'NONE',  ( 34.49999999999976552, 4.087461875839198733, 4.000000000000000000 ) ) ;
#127294 = CARTESIAN_POINT ( 'NONE',  ( -5.721745484314237906, 8.259292476615630818, 11.78515199841149297 ) ) ;
#127295 = LINE ( 'NONE', #108360, #74477 ) ;
#127296 = DIRECTION ( 'NONE',  ( 0.6830127018922181881, 0.6830127018922202975, -0.2588190451025214056 ) ) ;
#127297 = ORIENTED_EDGE ( 'NONE', *, *, #92520, .F. ) ;
#127298 = VECTOR ( 'NONE', #80051, 1000.000000000000227 ) ;
#127299 = LINE ( 'NONE', #137484, #59228 ) ;
#127300 = EDGE_LOOP ( 'NONE', ( #132365, #73597, #104439, #108992 ) ) ;
#127301 = LINE ( 'NONE', #28005, #59931 ) ;
#127303 = VERTEX_POINT ( 'NONE', #70101 ) ;
#127302 = DIRECTION ( 'NONE',  ( -0.7071067811865487940, 0.7071067811865463515, -0.000000000000000000 ) ) ;
#127304 = EDGE_CURVE ( 'NONE', #60449, #17946, #91115, .T. ) ;
#127305 = EDGE_CURVE ( 'NONE', #28418, #89687, #112144, .T. ) ;
#127306 = DIRECTION ( 'NONE',  ( -0.7071067811865487940, 0.7071067811865463515, -0.000000000000000000 ) ) ;
#127307 = FACE_OUTER_BOUND ( 'NONE', #20900, .T. ) ;
#127308 = ORIENTED_EDGE ( 'NONE', *, *, #93860, .F. ) ;
#127309 = VERTEX_POINT ( 'NONE', #111396 ) ;
#127310 = DIRECTION ( 'NONE',  ( -0.6830127018922181881, 0.6830127018922202975, -0.2588190451025214056 ) ) ;
#127311 = SURFACE_STYLE_USAGE ( .BOTH. , #59249 ) ;
#127312 = ORIENTED_EDGE ( 'NONE', *, *, #75388, .T. ) ;
#127313 = DIRECTION ( 'NONE',  ( 0.7071067811865487940, 0.7071067811865463515, -0.000000000000000000 ) ) ;
#127314 = EDGE_CURVE ( 'NONE', #39875, #132680, #12084, .T. ) ;
#127315 = CARTESIAN_POINT ( 'NONE',  ( 89.47502705046288440, -5.819803920172572198, 5.819803920172572198 ) ) ;
#127316 = CARTESIAN_POINT ( 'NONE',  ( 71.43749999999998579, 5.819803920172574863, -5.819803920172573086 ) ) ;
#127317 = CARTESIAN_POINT ( 'NONE',  ( -12.20000000000000284, -34.64999999999999147, -39.50000000000000000 ) ) ;
#127318 = ORIENTED_EDGE ( 'NONE', *, *, #95893, .T. ) ;
#127319 = LINE ( 'NONE', #114305, #58530 ) ;
#127320 = FACE_OUTER_BOUND ( 'NONE', #125765, .T. ) ;
#127321 = CARTESIAN_POINT ( 'NONE',  ( 20.41666666666667140, 5.278424836066147208, 3.047499999999990550 ) ) ;
#127322 = CARTESIAN_POINT ( 'NONE',  ( -63.29974487139158867, -27.71228299555250274, 4.000000000000000000 ) ) ;
#127323 = EDGE_CURVE ( 'NONE', #25649, #104004, #115596, .T. ) ;
#127324 = CARTESIAN_POINT ( 'NONE',  ( -33.29974487139158867, -27.71228299555229313, 4.000000000000000000 ) ) ;
#127325 = ORIENTED_EDGE ( 'NONE', *, *, #105243, .F. ) ;
#127326 = CARTESIAN_POINT ( 'NONE',  ( 46.01669371712956291, 7.950000000000000178, -2.130196079827421318 ) ) ;
#127327 = ORIENTED_EDGE ( 'NONE', *, *, #80829, .T. ) ;
#127328 = AXIS2_PLACEMENT_3D ( 'NONE', #73783, #28857, #129573 ) ;
#127329 = CARTESIAN_POINT ( 'NONE',  ( 87.20876352523143282, -7.482591942790329030E-16, 6.110000000000001208 ) ) ;
#127330 = DIRECTION ( 'NONE',  ( 1.000000000000000000, 0.000000000000000000, 0.000000000000000000 ) ) ;
#127331 = VECTOR ( 'NONE', #30003, 999.9999999999998863 ) ;
#127332 = EDGE_CURVE ( 'NONE', #101826, #11525, #34576, .T. ) ;
#127333 = CARTESIAN_POINT ( 'NONE',  ( -23.99451991528749062, 28.92564299267954908, 4.000000000000000000 ) ) ;
#127334 = DIRECTION ( 'NONE',  ( -0.6830127018922180770, -0.6830127018922204085, -0.2588190451025213501 ) ) ;
#127335 = EDGE_LOOP ( 'NONE', ( #68745, #64928, #98335, #128012 ) ) ;
#127336 = VECTOR ( 'NONE', #85515, 999.9999999999998863 ) ;
#127337 = VECTOR ( 'NONE', #32084, 1000.000000000000114 ) ;
#127338 = VECTOR ( 'NONE', #78269, 1000.000000000000000 ) ;
#127339 = DIRECTION ( 'NONE',  ( 0.7071067811865486830, -0.7071067811865464625, -0.000000000000000000 ) ) ;
#127340 = VECTOR ( 'NONE', #50404, 1000.000000000000000 ) ;
#127341 = DIRECTION ( 'NONE',  ( 1.000000000000000000, 0.000000000000000000, 0.000000000000000000 ) ) ;
#127342 = DIRECTION ( 'NONE',  ( 0.7071067811865487940, -0.7071067811865463515, 0.000000000000000000 ) ) ;
#127343 = DIRECTION ( 'NONE',  ( -1.000000000000000000, -0.000000000000000000, -0.000000000000000000 ) ) ;
#127346 = EDGE_CURVE ( 'NONE', #111310, #61200, #24399, .T. ) ;
#127345 = ORIENTED_EDGE ( 'NONE', *, *, #71039, .F. ) ;
#127344 = FACE_OUTER_BOUND ( 'NONE', #27568, .T. ) ;
#127347 = DIRECTION ( 'NONE',  ( 0.7071067811865486830, -0.7071067811865464625, -0.000000000000000000 ) ) ;
#127348 = CARTESIAN_POINT ( 'NONE',  ( -34.75611968250420603, 13.70565069852392703, 4.955485411084897152 ) ) ;
#127349 = CARTESIAN_POINT ( 'NONE',  ( 1.729826228151208900, -4.601789674110575490, 4.401668811681049398 ) ) ;
#127350 = VECTOR ( 'NONE', #35351, 1000.000000000000000 ) ;
#127351 = DIRECTION ( 'NONE',  ( 0.000000000000000000, -1.000000000000000000, 0.000000000000000000 ) ) ;
#127352 = VERTEX_POINT ( 'NONE', #15614 ) ;
#127353 = EDGE_CURVE ( 'NONE', #18088, #107805, #139374, .T. ) ;
#127354 = ORIENTED_EDGE ( 'NONE', *, *, #112592, .F. ) ;
#127355 = CARTESIAN_POINT ( 'NONE',  ( 78.31293019189810423, -1.637169565754159617, -6.110000000000001208 ) ) ;
#127356 = ORIENTED_EDGE ( 'NONE', *, *, #95013, .T. ) ;
#127357 = DIRECTION ( 'NONE',  ( -0.7071067811865486830, -0.7071067811865464625, -0.000000000000000000 ) ) ;
#127358 = AXIS2_PLACEMENT_3D ( 'NONE', #20836, #87541, #42639 ) ;
#127359 = DIRECTION ( 'NONE',  ( -0.3543493200069162685, -0.000000000000000000, -0.9351131265310288487 ) ) ;
#127360 = PLANE ( 'NONE',  #94023 ) ;
#127361 = ORIENTED_EDGE ( 'NONE', *, *, #128762, .F. ) ;
#127362 = DIRECTION ( 'NONE',  ( -0.000000000000000000, 0.000000000000000000, 1.000000000000000000 ) ) ;
#127363 = CARTESIAN_POINT ( 'NONE',  ( 16.27785539607886633, 4.584330080086930965E-16, 0.000000000000000000 ) ) ;
#127364 = AXIS2_PLACEMENT_3D ( 'NONE', #48924, #27859, #116298 ) ;
#127365 = VERTEX_POINT ( 'NONE', #16347 ) ;
#127366 = EDGE_CURVE ( 'NONE', #12589, #96735, #93934, .T. ) ;
#127367 = CARTESIAN_POINT ( 'NONE',  ( 68.99451991528748351, 28.92564299267986172, 4.000000000000000000 ) ) ;
#127368 = DIRECTION ( 'NONE',  ( 0.7071067811865487940, 0.7071067811865463515, 0.000000000000000000 ) ) ;
#127369 = LINE ( 'NONE', #28068, #23818 ) ;
#127370 = AXIS2_PLACEMENT_3D ( 'NONE', #13024, #12322, #47858 ) ;
#127371 = VERTEX_POINT ( 'NONE', #117799 ) ;
#127372 = ORIENTED_EDGE ( 'NONE', *, *, #36818, .F. ) ;
#127373 = EDGE_CURVE ( 'NONE', #140226, #112363, #62055, .T. ) ;
#127374 = MECHANICAL_DESIGN_GEOMETRIC_PRESENTATION_REPRESENTATION (  '', ( #55688 ), #136685 ) ;
#127375 = CARTESIAN_POINT ( 'NONE',  ( 29.99999999999979039, -12.03360074219761700, 5.000000000000000000 ) ) ;
#127376 = FACE_OUTER_BOUND ( 'NONE', #34992, .T. ) ;
#127377 = CARTESIAN_POINT ( 'NONE',  ( 25.39999999999999503, -6.374147713795669468, -2.268615643378129043 ) ) ;
#127378 = CARTESIAN_POINT ( 'NONE',  ( -2.475998614145493715, 22.03583458319438293, 4.979811245910087614 ) ) ;
#127379 = LINE ( 'NONE', #61460, #1679 ) ;
#127380 = CARTESIAN_POINT ( 'NONE',  ( -38.99451991528749062, 28.92564299267965211, 4.000000000000000000 ) ) ;
#127381 = ORIENTED_EDGE ( 'NONE', *, *, #131504, .F. ) ;
#127382 = VECTOR ( 'NONE', #127204, 1000.000000000000227 ) ;
#127383 = ORIENTED_EDGE ( 'NONE', *, *, #11952, .T. ) ;
#127384 = ORIENTED_EDGE ( 'NONE', *, *, #12697, .F. ) ;
#127385 = ADVANCED_FACE ( 'NONE', ( #104815 ), #55543, .T. ) ;
#127386 = EDGE_LOOP ( 'NONE', ( #101950, #102958, #75308 ) ) ;
#127387 = VECTOR ( 'NONE', #31407, 1000.000000000000227 ) ;
#127388 = LINE ( 'NONE', #26657, #82544 ) ;
#127389 = ORIENTED_EDGE ( 'NONE', *, *, #97999, .F. ) ;
#127390 = PRESENTATION_STYLE_ASSIGNMENT (( #128136 ) ) ;
#127391 = DIRECTION ( 'NONE',  ( 0.7071067811865487940, 0.7071067811865463515, 0.000000000000000000 ) ) ;
#127392 = EDGE_CURVE ( 'NONE', #58699, #121778, #129600, .T. ) ;
#127393 = DIRECTION ( 'NONE',  ( 0.7071067811865487940, 0.7071067811865463515, 0.000000000000000000 ) ) ;
#127394 = DIRECTION ( 'NONE',  ( 0.3543493200069162685, -0.000000000000000000, -0.9351131265310288487 ) ) ;
#127395 = VECTOR ( 'NONE', #112994, 1000.000000000000000 ) ;
#127396 = LINE ( 'NONE', #95480, #14354 ) ;
#127397 = ORIENTED_EDGE ( 'NONE', *, *, #61486, .T. ) ;
#127398 = DIRECTION ( 'NONE',  ( 0.7071067811865486830, -0.7071067811865464625, -0.000000000000000000 ) ) ;
#127399 = DIRECTION ( 'NONE',  ( 0.7071067811865487940, -0.7071067811865463515, 0.000000000000000000 ) ) ;
#127400 = VERTEX_POINT ( 'NONE', #83821 ) ;
#127401 = EDGE_CURVE ( 'NONE', #3555, #103699, #84519, .T. ) ;
#127402 = CARTESIAN_POINT ( 'NONE',  ( -10.82816939922344979, -11.24070752338417023, 4.000000000000000000 ) ) ;
#127403 = VERTEX_POINT ( 'NONE', #128712 ) ;
#127404 = VERTEX_POINT ( 'NONE', #38853 ) ;
#127406 = EDGE_CURVE ( 'NONE', #80026, #49145, #126551, .T. ) ;
#127405 = CARTESIAN_POINT ( 'NONE',  ( 12.87913961620377279, -5.278424836066145431, -3.047499999999993658 ) ) ;
#127407 = ORIENTED_EDGE ( 'NONE', *, *, #56085, .F. ) ;
#127408 = ORIENTED_EDGE ( 'NONE', *, *, #121521, .F. ) ;
#127409 = CARTESIAN_POINT ( 'NONE',  ( 72.04209685856477563, 5.291415217122923842, -3.054999999999996163 ) ) ;
#127411 = VERTEX_POINT ( 'NONE', #61368 ) ;
#127410 = VECTOR ( 'NONE', #81703, 1000.000000000000000 ) ;
#127412 = AXIS2_PLACEMENT_3D ( 'NONE', #114600, #61008, #48659 ) ;
#127413 = FACE_OUTER_BOUND ( 'NONE', #71826, .T. ) ;
#127414 = DIRECTION ( 'NONE',  ( 0.7071067811865487940, 0.7071067811865463515, -0.000000000000000000 ) ) ;
#127415 = CARTESIAN_POINT ( 'NONE',  ( 105.5837635252314328, -6.110000000000001208, -3.741295971395164515E-16 ) ) ;
#127416 = CARTESIAN_POINT ( 'NONE',  ( 34.92499999999998295, -15.89852273831277074, -9.446427897663607354 ) ) ;
#127417 = EDGE_CURVE ( 'NONE', #92047, #91018, #29388, .T. ) ;
#127418 = DIRECTION ( 'NONE',  ( -0.7071067811865486830, -0.7071067811865464625, 0.000000000000000000 ) ) ;
#127419 = PLANE ( 'NONE',  #41773 ) ;
#127420 = CARTESIAN_POINT ( 'NONE',  ( 60.48921356237309510, -27.52281430457097500, 5.000000000000000000 ) ) ;
#127421 = AXIS2_PLACEMENT_3D ( 'NONE', #132070, #14376, #65401 ) ;
#127422 = CARTESIAN_POINT ( 'NONE',  ( 28.82816939922332722, 15.75929247661554733, 4.000000000000000000 ) ) ;
#127423 = EDGE_CURVE ( 'NONE', #62049, #11462, #17102, .T. ) ;
#127424 = CARTESIAN_POINT ( 'NONE',  ( 7.499999999999947597, -19.91253812416055169, 4.000000000000000000 ) ) ;
#127426 = CARTESIAN_POINT ( 'NONE',  ( -44.99451991528749772, 28.92564299267969474, 4.000000000000000000 ) ) ;
#127425 = VECTOR ( 'NONE', #122397, 1000.000000000000000 ) ;
#127428 = ORIENTED_EDGE ( 'NONE', *, *, #116687, .F. ) ;
#127427 = VECTOR ( 'NONE', #5919, 1000.000000000000000 ) ;
#127429 = SURFACE_STYLE_FILL_AREA ( #83225 ) ;
#127430 = VERTEX_POINT ( 'NONE', #83076 ) ;
#127431 = ORIENTED_EDGE ( 'NONE', *, *, #123066, .T. ) ;
#127432 = CARTESIAN_POINT ( 'NONE',  ( 114.7041937171295558, -6.884901960086285300, -3.975000000000000089 ) ) ;
#127434 = EDGE_CURVE ( 'NONE', #28611, #110962, #41651, .T. ) ;
#127433 = VECTOR ( 'NONE', #89813, 1000.000000000000000 ) ;
#127435 = VECTOR ( 'NONE', #10664, 1000.000000000000000 ) ;
#127436 = ORIENTED_EDGE ( 'NONE', *, *, #9171, .T. ) ;
#127437 = VECTOR ( 'NONE', #114439, 1000.000000000000227 ) ;
#127438 = VECTOR ( 'NONE', #46284, 1000.000000000000000 ) ;
#127439 = VECTOR ( 'NONE', #75221, 1000.000000000000227 ) ;
#127440 = FACE_OUTER_BOUND ( 'NONE', #52140, .T. ) ;
#127441 = DIRECTION ( 'NONE',  ( 0.7071067811865486830, -0.7071067811865464625, -0.000000000000000000 ) ) ;
#127442 = CARTESIAN_POINT ( 'NONE',  ( 0.000000000000000000, 0.000000000000000000, 0.000000000000000000 ) ) ;
#127443 = DIRECTION ( 'NONE',  ( 0.3543493200069164351, 2.781805975412904658E-17, -0.9351131265310288487 ) ) ;
#127444 = EDGE_LOOP ( 'NONE', ( #90289, #5077, #30879, #122993 ) ) ;
#127446 = VERTEX_POINT ( 'NONE', #116415 ) ;
#127445 = VECTOR ( 'NONE', #71733, 1000.000000000000000 ) ;
#127447 = CARTESIAN_POINT ( 'NONE',  ( 4.499569808101886004, -3.967499999999998028, -6.871911579029511330 ) ) ;
#127448 = PLANE ( 'NONE',  #130347 ) ;
#127449 = LINE ( 'NONE', #94097, #36682 ) ;
#127450 = CARTESIAN_POINT ( 'NONE',  ( 10.32500000000000107, -8.432637487761466488, 4.375000000000001776 ) ) ;
#127451 = ORIENTED_EDGE ( 'NONE', *, *, #131545, .T. ) ;
#127452 = EDGE_CURVE ( 'NONE', #35648, #110736, #127274, .T. ) ;
#127453 = ORIENTED_EDGE ( 'NONE', *, *, #97162, .T. ) ;
#127454 = EDGE_LOOP ( 'NONE', ( #7446, #105859, #120030, #96715 ) ) ;
#127456 = AXIS2_PLACEMENT_3D ( 'NONE', #10504, #20672, #9038 ) ;
#127455 = CARTESIAN_POINT ( 'NONE',  ( 152.4000000000000057, 0.000000000000000000, 33.92499999999998295 ) ) ;
#127457 = CARTESIAN_POINT ( 'NONE',  ( 16.17183060077636370, -5.240707523384223521, 4.000000000000000000 ) ) ;
#127458 = CARTESIAN_POINT ( 'NONE',  ( -9.707106781186475075, -3.740707523384241728, 5.000000000000000000 ) ) ;
#127459 = DIRECTION ( 'NONE',  ( 0.6830127018922181881, 0.6830127018922202975, -0.2588190451025214056 ) ) ;
#127460 = PLANE ( 'NONE',  #18136 ) ;
#127461 = ADVANCED_FACE ( 'NONE', ( #49758 ), #27976, .T. ) ;
#127462 = ADVANCED_FACE ( 'NONE', ( #6175 ), #27240, .F. ) ;
#127463 = CARTESIAN_POINT ( 'NONE',  ( 8.968407645496675684, 9.139736423841732040E-16, 0.000000000000000000 ) ) ;
#127464 = VECTOR ( 'NONE', #118984, 1000.000000000000000 ) ;
#127465 = DIRECTION ( 'NONE',  ( 0.6830127018922181881, 0.6830127018922202975, -0.2588190451025214056 ) ) ;
#127466 = PLANE ( 'NONE',  #97519 ) ;
#127467 = CARTESIAN_POINT ( 'NONE',  ( -0.4892135623730947680, -27.52281430457055578, 5.000000000000000000 ) ) ;
#127468 = AXIS2_PLACEMENT_3D ( 'NONE', #5162, #29096, #18177 ) ;
#127469 = ORIENTED_EDGE ( 'NONE', *, *, #34613, .T. ) ;
#127470 = LINE ( 'NONE', #48483, #39425 ) ;
#127473 = EDGE_CURVE ( 'NONE', #84275, #34917, #72246, .T. ) ;
#127472 = AXIS2_PLACEMENT_3D ( 'NONE', #119954, #19256, #130898 ) ;
#127471 = CARTESIAN_POINT ( 'NONE',  ( 18.95159235450331892, 2.500000000000001776, 0.000000000000000000 ) ) ;
#127474 = ORIENTED_EDGE ( 'NONE', *, *, #61915, .T. ) ;
#127475 = CARTESIAN_POINT ( 'NONE',  ( 21.48921356237309155, -27.52281430457070499, 5.000000000000000000 ) ) ;
#127477 = ORIENTED_EDGE ( 'NONE', *, *, #59265, .T. ) ;
#127476 = FACE_OUTER_BOUND ( 'NONE', #28447, .T. ) ;
#127478 = ADVANCED_FACE ( 'NONE', ( #49032 ), #93227, .T. ) ;
#127479 = STYLED_ITEM ( 'NONE', ( #119093 ), #82437 ) ;
#127480 = EDGE_CURVE ( 'NONE', #66788, #6851, #40309, .T. ) ;
#127481 = LINE ( 'NONE', #16558, #7463 ) ;
#127482 = LINE ( 'NONE', #49944, #115527 ) ;
#127483 = VERTEX_POINT ( 'NONE', #56736 ) ;
#127484 = DIRECTION ( 'NONE',  ( -0.6830127018922181881, 0.6830127018922202975, -0.2588190451025214056 ) ) ;
#127485 = UNCERTAINTY_MEASURE_WITH_UNIT (LENGTH_MEASURE( 1.000000000000000082E-05 ), #31779, 'distance_accuracy_value', 'NONE');
#127486 = ORIENTED_EDGE ( 'NONE', *, *, #40589, .T. ) ;
#127487 = LINE ( 'NONE', #17292, #121544 ) ;
#127488 = CARTESIAN_POINT ( 'NONE',  ( 117.4750270504628702, -5.819803920172572198, 5.819803920172572198 ) ) ;
#127489 = EDGE_CURVE ( 'NONE', #68456, #142084, #77042, .T. ) ;
#127490 = FACE_OUTER_BOUND ( 'NONE', #91693, .T. ) ;
#127491 = VECTOR ( 'NONE', #12648, 1000.000000000000000 ) ;
#127492 = ADVANCED_FACE ( 'NONE', ( #100897 ), #127221, .T. ) ;
#127493 = CARTESIAN_POINT ( 'NONE',  ( -32.20666063542130075, 21.75929247661549226, 4.998822639870715179 ) ) ;
#127494 = DIRECTION ( 'NONE',  ( -0.7071067811865486830, 0.7071067811865464625, 0.000000000000000000 ) ) ;
#127495 = CARTESIAN_POINT ( 'NONE',  ( -63.48921356237309510, -27.52281430457099631, 5.000000000000000000 ) ) ;
#127496 = PLANE ( 'NONE',  #115444 ) ;
#127498 = AXIS2_PLACEMENT_3D ( 'NONE', #22465, #130562, #21784 ) ;
#127497 = CARTESIAN_POINT ( 'NONE',  ( 33.22873647476855297, 5.808823158059031044, -5.808823158059038150 ) ) ;
#127499 = CARTESIAN_POINT ( 'NONE',  ( 8.291236474768552966, -9.717572351234235426E-16, -7.934999999999990727 ) ) ;
#127500 = DIRECTION ( 'NONE',  ( 0.7071067811865487940, 0.7071067811865463515, -0.000000000000000000 ) ) ;
#127501 = EDGE_CURVE ( 'NONE', #19604, #21453, #2182, .T. ) ;
#127502 = LINE ( 'NONE', #60867, #76801 ) ;
#127503 = LINE ( 'NONE', #61569, #1505 ) ;
#127504 = ORIENTED_EDGE ( 'NONE', *, *, #102956, .F. ) ;
#127505 = ORIENTED_EDGE ( 'NONE', *, *, #12704, .F. ) ;
#127506 = CARTESIAN_POINT ( 'NONE',  ( 81.79166666666667140, 3.975000000000003642, -6.884901960086285300 ) ) ;
#127507 = CARTESIAN_POINT ( 'NONE',  ( -25.17183060077628909, -20.24070752338406365, 4.000000000000000000 ) ) ;
#127508 = ORIENTED_EDGE ( 'NONE', *, *, #46372, .T. ) ;
#127509 = CARTESIAN_POINT ( 'NONE',  ( 47.99451991528749062, 28.92564299267971251, 4.000000000000000000 ) ) ;
#127510 = LINE ( 'NONE', #113781, #113477 ) ;
#127511 = ADVANCED_FACE ( 'NONE', ( #88622 ), #100203, .T. ) ;
#127512 =( GEOMETRIC_REPRESENTATION_CONTEXT ( 3 ) GLOBAL_UNCERTAINTY_ASSIGNED_CONTEXT ( ( #12993 ) ) GLOBAL_UNIT_ASSIGNED_CONTEXT ( ( #36176, #126712, #27400 ) ) REPRESENTATION_CONTEXT ( 'NONE', 'WORKASPACE' ) );
#127513 = CARTESIAN_POINT ( 'NONE',  ( 30.12086038379621655, -6.884901960086286188, 3.974999999999997424 ) ) ;
#127514 = ORIENTED_EDGE ( 'NONE', *, *, #141371, .T. ) ;
#127515 = DIRECTION ( 'NONE',  ( -0.3543493200069162685, -0.000000000000000000, -0.9351131265310288487 ) ) ;
#127516 = DIRECTION ( 'NONE',  ( 0.6830127018922180770, -0.6830127018922204085, -0.2588190451025213501 ) ) ;
#127517 = PLANE ( 'NONE',  #62692 ) ;
#127518 = LINE ( 'NONE', #7121, #79023 ) ;
#127519 = CARTESIAN_POINT ( 'NONE',  ( 25.49999999999982947, 9.052185695429072254, 5.000000000000000000 ) ) ;
#127520 = CARTESIAN_POINT ( 'NONE',  ( -24.20969143188526118, 6.176090689687629975, 5.000000000000000000 ) ) ;
#127521 = EDGE_CURVE ( 'NONE', #88704, #16399, #121216, .T. ) ;
#127522 = DIRECTION ( 'NONE',  ( -0.7071067811865486830, 0.7071067811865464625, 0.000000000000000000 ) ) ;
#127523 = AXIS2_PLACEMENT_3D ( 'NONE', #19797, #140172, #131436 ) ;
#127524 = DIRECTION ( 'NONE',  ( -0.7071067811865486830, 0.7071067811865464625, 0.000000000000000000 ) ) ;
#127525 = CARTESIAN_POINT ( 'NONE',  ( 15.32816939922343202, 8.259292476615637923, 4.000000000000000000 ) ) ;
#127526 = DIRECTION ( 'NONE',  ( 1.000000000000000000, 0.000000000000000000, 0.000000000000000000 ) ) ;
#127527 = CARTESIAN_POINT ( 'NONE',  ( 57.10144406050385868, -49.69743550128991671, 36.79359617903139679 ) ) ;
#127528 = EDGE_CURVE ( 'NONE', #46561, #58967, #33541, .T. ) ;
#127529 = EDGE_LOOP ( 'NONE', ( #113592, #88583, #47047, #69260 ) ) ;
#127530 = ORIENTED_EDGE ( 'NONE', *, *, #121688, .T. ) ;
#127531 = CARTESIAN_POINT ( 'NONE',  ( 98.87543019189810423, -5.291415217122920289, -3.055000000000001492 ) ) ;
#127532 = ORIENTED_EDGE ( 'NONE', *, *, #24057, .T. ) ;
#127533 = CARTESIAN_POINT ( 'NONE',  ( 122.6835989386367345, -43.14999999999999147, 34.92499999999998295 ) ) ;
#127534 = CARTESIAN_POINT ( 'NONE',  ( 8.312500000000000000, -4.461849672132299993, -4.461849672132299105 ) ) ;
#127535 = ORIENTED_EDGE ( 'NONE', *, *, #124819, .T. ) ;
#127537 = EDGE_CURVE ( 'NONE', #16019, #142252, #68322, .T. ) ;
#127536 = AXIS2_PLACEMENT_3D ( 'NONE', #10127, #54389, #97096 ) ;
#127538 = LINE ( 'NONE', #118047, #62946 ) ;
#127539 = CARTESIAN_POINT ( 'NONE',  ( -16.17183060077635659, -14.24070752338413648, 4.000000000000000000 ) ) ;
#127540 = AXIS2_PLACEMENT_3D ( 'NONE', #137416, #47588, #105466 ) ;
#127541 = VECTOR ( 'NONE', #86753, 1000.000000000000000 ) ;
#127542 = CARTESIAN_POINT ( 'NONE',  ( 103.3079301918981088, -6.109999999999998543, 1.637169565754158063 ) ) ;
#127543 = ORIENTED_EDGE ( 'NONE', *, *, #8095, .F. ) ;
#127544 = CARTESIAN_POINT ( 'NONE',  ( 16.30000000000000071, 9.521314400968980422E-16, 0.000000000000000000 ) ) ;
#127545 = ORIENTED_EDGE ( 'NONE', *, *, #86219, .F. ) ;
#127546 = DIRECTION ( 'NONE',  ( 0.000000000000000000, 1.000000000000000000, 0.000000000000000000 ) ) ;
#127547 = AXIS2_PLACEMENT_3D ( 'NONE', #116933, #106028, #109624 ) ;
#127548 = VECTOR ( 'NONE', #130737, 1000.000000000000000 ) ;
#127549 = CARTESIAN_POINT ( 'NONE',  ( 14.08373646989360317, 3.061616997868383634E-16, -2.500000000000000444 ) ) ;
#127550 = VECTOR ( 'NONE', #87370, 999.9999999999998863 ) ;
#127551 = VECTOR ( 'NONE', #91881, 1000.000000000000000 ) ;
#127552 = CARTESIAN_POINT ( 'NONE',  ( -5.999999999999951150, -6.412538124160692909, 4.000000000000000000 ) ) ;
#127553 = CARTESIAN_POINT ( 'NONE',  ( 18.48921356237309510, -27.52281430457068367, 5.000000000000000000 ) ) ;
#127554 = MECHANICAL_DESIGN_GEOMETRIC_PRESENTATION_REPRESENTATION (  '', ( #109003 ), #25715 ) ;
#127555 = ORIENTED_EDGE ( 'NONE', *, *, #87663, .T. ) ;
#127556 = ORIENTED_EDGE ( 'NONE', *, *, #47915, .F. ) ;
#127557 = ORIENTED_EDGE ( 'NONE', *, *, #33840, .T. ) ;
#127558 = DIRECTION ( 'NONE',  ( 0.7071067811865487940, -0.7071067811865463515, 0.000000000000000000 ) ) ;
#127559 = DIRECTION ( 'NONE',  ( -0.7071067811865486830, -0.7071067811865464625, 0.000000000000000000 ) ) ;
#127560 = CARTESIAN_POINT ( 'NONE',  ( 12.02540314143521982, 2.126176841940962348, 7.934999999999988951 ) ) ;
#127561 = AXIS2_PLACEMENT_3D ( 'NONE', #93991, #115000, #106270 ) ;
#127562 = LINE ( 'NONE', #94200, #54933 ) ;
#127563 = FILL_AREA_STYLE_COLOUR ( '', #102524 ) ;
#127564 = EDGE_LOOP ( 'NONE', ( #63204, #114270, #44768, #57159 ) ) ;
#127565 = ORIENTED_EDGE ( 'NONE', *, *, #15736, .F. ) ;
#127566 = VECTOR ( 'NONE', #23426, 1000.000000000000227 ) ;
#127567 = CARTESIAN_POINT ( 'NONE',  ( -19.49999999999985789, -8.947814304570730570, 5.000000000000000000 ) ) ;
#127569 = EDGE_CURVE ( 'NONE', #34714, #111174, #7624, .T. ) ;
#127568 = EDGE_LOOP ( 'NONE', ( #111798, #14465, #73055, #139275 ) ) ;
#127570 = VERTEX_POINT ( 'NONE', #78452 ) ;
#127571 = CARTESIAN_POINT ( 'NONE',  ( 113.5162635252314516, -4.472830434245838482, 4.472830434245838482 ) ) ;
#127572 = VECTOR ( 'NONE', #37173, 1000.000000000000000 ) ;
#127573 = VECTOR ( 'NONE', #71382, 1000.000000000000000 ) ;
#127574 = LINE ( 'NONE', #137023, #12067 ) ;
#127575 = PLANE ( 'NONE',  #112066 ) ;
#127576 = EDGE_LOOP ( 'NONE', ( #67081, #29635, #85618, #104517, #49692, #117993 ) ) ;
#127577 = DIRECTION ( 'NONE',  ( -0.000000000000000000, -0.3543493200069152693, 0.9351131265310292928 ) ) ;
#127578 = CYLINDRICAL_SURFACE ( 'NONE', #29314, 0.5000000000000004441 ) ;
#127579 = FACE_OUTER_BOUND ( 'NONE', #136781, .T. ) ;
#127580 = CIRCLE ( 'NONE', #118248, 2.500000000000000888 ) ;
#127581 = DIRECTION ( 'NONE',  ( 0.6830127018922181881, 0.6830127018922202975, -0.2588190451025214056 ) ) ;
#127582 = ORIENTED_EDGE ( 'NONE', *, *, #105983, .F. ) ;
#127583 = EDGE_CURVE ( 'NONE', #82818, #131125, #69416, .T. ) ;
#127584 = LINE ( 'NONE', #106505, #134726 ) ;
#127585 = CARTESIAN_POINT ( 'NONE',  ( 36.48921356237310221, -27.52281430457080802, 5.000000000000000000 ) ) ;
#127586 = ORIENTED_EDGE ( 'NONE', *, *, #101936, .F. ) ;
#127587 = CARTESIAN_POINT ( 'NONE',  ( 25.60343192894627862, -14.24070752338413293, 19.24067776001731644 ) ) ;
#127588 = ADVANCED_FACE ( 'NONE', ( #42978 ), #81002, .T. ) ;
#127589 = LINE ( 'NONE', #81977, #36506 ) ;
#127590 = AXIS2_PLACEMENT_3D ( 'NONE', #9595, #98070, #55287 ) ;
#127591 = DIRECTION ( 'NONE',  ( -0.7071067811865486830, 0.7071067811865464625, 0.000000000000000000 ) ) ;
#127592 = EDGE_LOOP ( 'NONE', ( #8508, #118496, #77761, #30978 ) ) ;
#127593 = CARTESIAN_POINT ( 'NONE',  ( -25.39999999999996305, 0.000000000000000000, 0.000000000000000000 ) ) ;
#127594 = ORIENTED_EDGE ( 'NONE', *, *, #113345, .T. ) ;
#127595 = ORIENTED_EDGE ( 'NONE', *, *, #79226, .F. ) ;
#127596 = ADVANCED_FACE ( 'NONE', ( #89317 ), #51889, .T. ) ;
#127597 = VERTEX_POINT ( 'NONE', #45838 ) ;
#127598 = ADVANCED_FACE ( 'NONE', ( #87887 ), #11003, .F. ) ;
#127599 = EDGE_CURVE ( 'NONE', #110134, #71568, #1550, .T. ) ;
#127600 = CARTESIAN_POINT ( 'NONE',  ( 31.41209685856477662, 5.291415217122921177, -3.054999999999994831 ) ) ;
#127601 = EDGE_LOOP ( 'NONE', ( #119048, #36093, #55301, #41315 ) ) ;
#127602 = CIRCLE ( 'NONE', #30321, 3.000000000000000444 ) ;
#127603 = CARTESIAN_POINT ( 'NONE',  ( 34.92499999999998295, 10.80009451602706783, 4.759050581649326261 ) ) ;
#127604 = DIRECTION ( 'NONE',  ( -0.7071067811865486830, -0.7071067811865464625, -0.000000000000000000 ) ) ;
#127605 =( NAMED_UNIT ( * ) SI_UNIT ( $, .STERADIAN. ) SOLID_ANGLE_UNIT ( ) );
#127606 = LINE ( 'NONE', #50053, #139972 ) ;
#127607 = ADVANCED_FACE ( 'NONE', ( #142976 ), #90014, .F. ) ;
#127608 = CARTESIAN_POINT ( 'NONE',  ( 25.49999999999982592, -15.29013452822851882, 0.3645803511610929970 ) ) ;
#127610 = DIRECTION ( 'NONE',  ( 0.000000000000000000, -1.000000000000000000, -1.286409696682840916E-16 ) ) ;
#127609 = VECTOR ( 'NONE', #104130, 999.9999999999998863 ) ;
#127611 = VECTOR ( 'NONE', #126063, 1000.000000000000000 ) ;
#127612 = LINE ( 'NONE', #72564, #84038 ) ;
#127613 = ADVANCED_FACE ( 'NONE', ( #76311 ), #120472, .F. ) ;
#127614 = DIRECTION ( 'NONE',  ( -1.000000000000000000, 0.000000000000000000, 0.000000000000000000 ) ) ;
#127615 = PLANE ( 'NONE',  #96889 ) ;
#127616 = DIRECTION ( 'NONE',  ( 0.6830127018922180770, -0.6830127018922204085, -0.2588190451025213501 ) ) ;
#127617 = EDGE_LOOP ( 'NONE', ( #13980, #114241, #5263, #83969 ) ) ;
#127618 = EDGE_LOOP ( 'NONE', ( #111183, #133864, #79018, #35836 ) ) ;
#127619 = ORIENTED_EDGE ( 'NONE', *, *, #59101, .F. ) ;
#127620 = VECTOR ( 'NONE', #126906, 999.9999999999998863 ) ;
#127621 = VERTEX_POINT ( 'NONE', #98745 ) ;
#127622 = CARTESIAN_POINT ( 'NONE',  ( 23.20710678118638981, 18.75929247661552779, 5.000000000000000000 ) ) ;
#127623 = EDGE_CURVE ( 'NONE', #15696, #49015, #43671, .T. ) ;
#127624 = VERTEX_POINT ( 'NONE', #37068 ) ;
#127625 = ORIENTED_EDGE ( 'NONE', *, *, #51628, .T. ) ;
#127626 = FACE_OUTER_BOUND ( 'NONE', #42481, .T. ) ;
#127627 = DIRECTION ( 'NONE',  ( 0.000000000000000000, 0.000000000000000000, 1.000000000000000000 ) ) ;
#127628 = CARTESIAN_POINT ( 'NONE',  ( 21.79996877983149517, 8.259292476615627265, 16.85664084051835943 ) ) ;
#127629 = ORIENTED_EDGE ( 'NONE', *, *, #95395, .F. ) ;
#127630 = FACE_OUTER_BOUND ( 'NONE', #33989, .T. ) ;
#127631 = EDGE_CURVE ( 'NONE', #92458, #91018, #81321, .T. ) ;
#127632 = VECTOR ( 'NONE', #22467, 999.9999999999998863 ) ;
#127633 = VERTEX_POINT ( 'NONE', #124090 ) ;
#127634 = CARTESIAN_POINT ( 'NONE',  ( -12.70000000000000462, -22.26999999999999247, -0.5000000000000004441 ) ) ;
#127635 = DIRECTION ( 'NONE',  ( 0.7071067811865487940, 0.7071067811865463515, -0.000000000000000000 ) ) ;
#127636 = CARTESIAN_POINT ( 'NONE',  ( -0.3704301918981141029, -3.967499999999998028, -6.871911579029511330 ) ) ;
#127637 = ORIENTED_EDGE ( 'NONE', *, *, #98828, .F. ) ;
#127639 = PLANE ( 'NONE',  #107792 ) ;
#127638 = CARTESIAN_POINT ( 'NONE',  ( 103.8912635252314516, -4.472830434245839371, -4.472830434245839371 ) ) ;
#127640 =( BOUNDED_CURVE ( )  B_SPLINE_CURVE ( 3, ( #25163, #13559, #4073, #24458 ),
 .UNSPECIFIED., .F., .T. ) 
 B_SPLINE_CURVE_WITH_KNOTS ( ( 4, 4 ),
 ( 5.043186909253412509, 5.074607125596365620 ),
 .UNSPECIFIED. ) 
 CURVE ( )  GEOMETRIC_REPRESENTATION_ITEM ( )  RATIONAL_B_SPLINE_CURVE ( ( 1.000000000000000000, 0.9999177325257868620, 0.9999177325257868620, 1.000000000000000000 ) ) 
 REPRESENTATION_ITEM ( '' )  );
#127641 = DIRECTION ( 'NONE',  ( -0.000000000000000000, 0.000000000000000000, 1.000000000000000000 ) ) ;
#127642 = ORIENTED_EDGE ( 'NONE', *, *, #77224, .F. ) ;
#127643 = EDGE_CURVE ( 'NONE', #93367, #77389, #78821, .T. ) ;
#127644 = ORIENTED_EDGE ( 'NONE', *, *, #35424, .T. ) ;
#127645 = DIRECTION ( 'NONE',  ( 0.6830127018922180770, -0.6830127018922204085, -0.2588190451025213501 ) ) ;
#127646 = ORIENTED_EDGE ( 'NONE', *, *, #17802, .F. ) ;
#127647 = CARTESIAN_POINT ( 'NONE',  ( 30.29974487139158867, -27.71228299555227537, 4.000000000000000000 ) ) ;
#127648 = STYLED_ITEM ( 'NONE', ( #37048 ), #73585 ) ;
#127649 = FACE_OUTER_BOUND ( 'NONE', #122663, .T. ) ;
#127650 = EDGE_LOOP ( 'NONE', ( #15506, #76884, #84484, #90831 ) ) ;
#127651 = ADVANCED_FACE ( 'NONE', ( #27612 ), #5118, .F. ) ;
#127653 = ADVANCED_FACE ( 'NONE', ( #60281 ), #126230, .F. ) ;
#127652 = VECTOR ( 'NONE', #124927, 1000.000000000000000 ) ;
#127654 = CARTESIAN_POINT ( 'NONE',  ( 14.99451991528749595, 28.92564299267948513, 4.000000000000000000 ) ) ;
#127655 = VECTOR ( 'NONE', #43249, 1000.000000000000000 ) ;
#127656 =( LENGTH_UNIT ( ) NAMED_UNIT ( * ) SI_UNIT ( .MILLI., .METRE. ) );
#127657 = CARTESIAN_POINT ( 'NONE',  ( -31.49999999999978684, -9.462702396501040170, -9.474982329943443915 ) ) ;
#127658 = VERTEX_POINT ( 'NONE', #37813 ) ;
#127659 = CARTESIAN_POINT ( 'NONE',  ( 20.99451991528748707, 28.92564299267952777, 4.000000000000000000 ) ) ;
#127660 = VECTOR ( 'NONE', #13681, 1000.000000000000000 ) ;
#127661 = AXIS2_PLACEMENT_3D ( 'NONE', #76708, #139824, #120879 ) ;
#127662 = AXIS2_PLACEMENT_3D ( 'NONE', #2152, #136270, #46459 ) ;
#127664 = ADVANCED_FACE ( 'NONE', ( #79918 ), #69012, .F. ) ;
#127663 = LINE ( 'NONE', #116044, #88745 ) ;
#127666 = ORIENTED_EDGE ( 'NONE', *, *, #95210, .T. ) ;
#127665 = AXIS2_PLACEMENT_3D ( 'NONE', #81296, #37047, #114595 ) ;
#127668 = VERTEX_POINT ( 'NONE', #113920 ) ;
#127667 = CARTESIAN_POINT ( 'NONE',  ( 0.2535635638417852444, -51.76057561339556656, -38.69631370864703257 ) ) ;
#127669 = ADVANCED_FACE ( 'NONE', ( #82732 ), #15281, .F. ) ;
#127670 = ORIENTED_EDGE ( 'NONE', *, *, #140388, .T. ) ;
#127671 = CARTESIAN_POINT ( 'NONE',  ( -17.44530448566515446, 4.797056265612570591, -29.43923607413351462 ) ) ;
#127672 = VECTOR ( 'NONE', #90840, 1000.000000000000000 ) ;
#127673 = DIRECTION ( 'NONE',  ( -0.7071067811865487940, 0.7071067811865463515, 0.000000000000000000 ) ) ;
#127674 = ORIENTED_EDGE ( 'NONE', *, *, #17580, .F. ) ;
#127675 = CARTESIAN_POINT ( 'NONE',  ( -15.29974487139158867, -27.71228299555216879, 4.000000000000000000 ) ) ;
#127676 = DIRECTION ( 'NONE',  ( 0.7071067811865487940, 0.7071067811865463515, -0.000000000000000000 ) ) ;
#127677 = DIRECTION ( 'NONE',  ( 0.3543493200069162685, -0.000000000000000000, -0.9351131265310288487 ) ) ;
#127678 = ORIENTED_EDGE ( 'NONE', *, *, #24448, .T. ) ;
#127680 = ADVANCED_FACE ( 'NONE', ( #69742 ), #135685, .F. ) ;
#127679 = VECTOR ( 'NONE', #52147, 1000.000000000000000 ) ;
#127681 = LINE ( 'NONE', #30506, #2126 ) ;
#127682 = PLANE ( 'NONE',  #58206 ) ;
#127683 = CARTESIAN_POINT ( 'NONE',  ( 26.67183060077628909, 17.25929247661554555, 4.000000000000000000 ) ) ;
#127684 = DIRECTION ( 'NONE',  ( 0.7071067811865487940, 0.7071067811865463515, -0.000000000000000000 ) ) ;
#127685 = CARTESIAN_POINT ( 'NONE',  ( -39.29974487139159578, -27.71228299555233576, 4.000000000000000000 ) ) ;
#127686 = CARTESIAN_POINT ( 'NONE',  ( -25.96836484077792306, 2.259292476615697876, 13.77329220150631173 ) ) ;
#127687 = CARTESIAN_POINT ( 'NONE',  ( 26.48225813788241112, 5.499261314031191006, -3.174999999999997158 ) ) ;
#127688 = EDGE_CURVE ( 'NONE', #135612, #119750, #103048, .T. ) ;
#127689 = PLANE ( 'NONE',  #78976 ) ;
#127690 = ORIENTED_EDGE ( 'NONE', *, *, #89791, .F. ) ;
#127691 = MECHANICAL_DESIGN_GEOMETRIC_PRESENTATION_REPRESENTATION (  '', ( #67586 ), #90655 ) ;
#127692 = ORIENTED_EDGE ( 'NONE', *, *, #71039, .T. ) ;
#127693 = EDGE_LOOP ( 'NONE', ( #30959, #12088, #56254, #62895 ) ) ;
#127694 = CARTESIAN_POINT ( 'NONE',  ( 114.8958333333333286, -2.130196079827427091, 7.949999999999999289 ) ) ;
#127695 = AXIS2_PLACEMENT_3D ( 'NONE', #73033, #128794, #117185 ) ;
#127696 = ORIENTED_EDGE ( 'NONE', *, *, #116268, .T. ) ;
#127697 = ORIENTED_EDGE ( 'NONE', *, *, #28551, .T. ) ;
#127698 = AXIS2_PLACEMENT_3D ( 'NONE', #65420, #29885, #42942 ) ;
#127699 = ORIENTED_EDGE ( 'NONE', *, *, #59560, .F. ) ;
#127700 = DIRECTION ( 'NONE',  ( 0.3543493200069162685, -0.000000000000000000, -0.9351131265310288487 ) ) ;
#127701 = VECTOR ( 'NONE', #14460, 1000.000000000000000 ) ;
#127702 = EDGE_LOOP ( 'NONE', ( #75176, #97480, #51669, #31501 ) ) ;
#127703 = DIRECTION ( 'NONE',  ( -0.000000000000000000, 0.000000000000000000, 1.000000000000000000 ) ) ;
#127704 = SURFACE_STYLE_FILL_AREA ( #83490 ) ;
#127705 = CARTESIAN_POINT ( 'NONE',  ( 11.99999999999991296, 20.70535890316562444, 1.956823837851888959 ) ) ;
#127706 = CARTESIAN_POINT ( 'NONE',  ( 12.19999999999999574, -25.83999999999998565, 13.17925390838734323 ) ) ;
#127707 = CARTESIAN_POINT ( 'NONE',  ( 111.7087635252314470, -7.482591942790329030E-16, 6.110000000000001208 ) ) ;
#127708 = VECTOR ( 'NONE', #27832, 1000.000000000000000 ) ;
#127709 = ORIENTED_EDGE ( 'NONE', *, *, #123711, .F. ) ;
#127710 = CARTESIAN_POINT ( 'NONE',  ( -38.99451991528749062, 28.92564299267965211, 4.000000000000000000 ) ) ;
#127711 = CARTESIAN_POINT ( 'NONE',  ( -54.18398860626899705, 28.73617430169825226, 5.000000000000000000 ) ) ;
#127712 = CARTESIAN_POINT ( 'NONE',  ( 8.207106781186489286, -11.24070752338417023, 5.000000000000000000 ) ) ;
#127713 = CARTESIAN_POINT ( 'NONE',  ( 8.999999999999937828, 9.631307414974335401, -9.079085613539522370 ) ) ;
#127714 = SURFACE_SIDE_STYLE ('',( #87581 ) ) ;
#127715 = CARTESIAN_POINT ( 'NONE',  ( 15.18398860626900237, 28.73617430169797871, 5.000000000000000000 ) ) ;
#127716 =( NAMED_UNIT ( * ) SI_UNIT ( $, .STERADIAN. ) SOLID_ANGLE_UNIT ( ) );
#127717 = CARTESIAN_POINT ( 'NONE',  ( 37.26669371712955581, -7.949999999999999289, 2.130196079827424427 ) ) ;
#127718 =( BOUNDED_CURVE ( )  B_SPLINE_CURVE ( 3, ( #128726, #18503, #63508, #107675 ),
 .UNSPECIFIED., .F., .T. ) 
 B_SPLINE_CURVE_WITH_KNOTS ( ( 4, 4 ),
 ( 1.964434688349488978, 3.503810798801449522 ),
 .UNSPECIFIED. ) 
 CURVE ( )  GEOMETRIC_REPRESENTATION_ITEM ( )  RATIONAL_B_SPLINE_CURVE ( ( 1.000000000000000000, 0.8120851936182288400, 0.8120851936182288400, 1.000000000000000000 ) ) 
 REPRESENTATION_ITEM ( '' )  );
#127719 = LINE ( 'NONE', #92196, #81458 ) ;
#127720 = EDGE_CURVE ( 'NONE', #60449, #31525, #57425, .T. ) ;
#127721 = CARTESIAN_POINT ( 'NONE',  ( -2.916851932270679626, 21.75929247661549581, 7.311836541448045068 ) ) ;
#127722 = EDGE_LOOP ( 'NONE', ( #81546, #37090, #99043, #82461 ) ) ;
#127723 = ORIENTED_EDGE ( 'NONE', *, *, #43465, .T. ) ;
#127724 = CARTESIAN_POINT ( 'NONE',  ( 26.81249999999998934, 5.819803920172571310, 5.819803920172575751 ) ) ;
#127725 = ORIENTED_EDGE ( 'NONE', *, *, #134132, .T. ) ;
#127726 = LINE ( 'NONE', #28406, #9263 ) ;
#127727 = PRESENTATION_LAYER_ASSIGNMENT (  '', '', ( #51342 ) ) ;
#127728 = CARTESIAN_POINT ( 'NONE',  ( -12.32816939922345334, 14.25929247661557753, 4.000000000000000000 ) ) ;
#127729 = VECTOR ( 'NONE', #18149, 1000.000000000000227 ) ;
#127730 = PLANE ( 'NONE',  #119673 ) ;
#127731 = DIRECTION ( 'NONE',  ( -0.000000000000000000, -0.3543493200069152693, 0.9351131265310292928 ) ) ;
#127732 = PLANE ( 'NONE',  #72180 ) ;
#127733 = DIRECTION ( 'NONE',  ( -0.000000000000000000, 0.3543493200069153248, 0.9351131265310292928 ) ) ;
#127734 = CARTESIAN_POINT ( 'NONE',  ( 29.31293019189811133, -1.637169565754159617, -6.110000000000001208 ) ) ;
#127735 = VERTEX_POINT ( 'NONE', #4371 ) ;
#127736 = AXIS2_PLACEMENT_3D ( 'NONE', #634, #99222, #143460 ) ;
#127737 = DIRECTION ( 'NONE',  ( 0.7071067811865486830, -0.7071067811865464625, -0.000000000000000000 ) ) ;
#127738 = ORIENTED_EDGE ( 'NONE', *, *, #34013, .F. ) ;
#127739 = AXIS2_PLACEMENT_3D ( 'NONE', #102353, #101600, #66851 ) ;
#127740 = DIRECTION ( 'NONE',  ( 0.6830127018922181881, 0.6830127018922202975, -0.2588190451025214056 ) ) ;
#127741 = CARTESIAN_POINT ( 'NONE',  ( -26.48334561358936412, 22.22500000000000142, 4.500000000000000888 ) ) ;
#127742 = CARTESIAN_POINT ( 'NONE',  ( 63.12500000000000000, -7.950000000000000178, -4.867971026610729436E-16 ) ) ;
#127743 = ORIENTED_EDGE ( 'NONE', *, *, #40251, .F. ) ;
#127744 = CARTESIAN_POINT ( 'NONE',  ( 50.60459685856477563, 1.637169565754164946, -6.109999999999999432 ) ) ;
#127745 = ORIENTED_EDGE ( 'NONE', *, *, #74108, .T. ) ;
#127746 = DIRECTION ( 'NONE',  ( -0.7071067811865486830, -0.7071067811865464625, -0.000000000000000000 ) ) ;
#127747 = LINE ( 'NONE', #84261, #39221 ) ;
#127748 = DIRECTION ( 'NONE',  ( 0.6830127018922180770, -0.6830127018922204085, -0.2588190451025213501 ) ) ;
#127749 = CARTESIAN_POINT ( 'NONE',  ( 5.999999999999956479, -4.068876922607770119, 4.000000000000000000 ) ) ;
#127750 = VECTOR ( 'NONE', #19617, 1000.000000000000000 ) ;
#127751 = CARTESIAN_POINT ( 'NONE',  ( 46.72459685856476597, -1.637169565754160949, 6.109999999999997655 ) ) ;
#127752 = ORIENTED_EDGE ( 'NONE', *, *, #103378, .T. ) ;
#127753 = CARTESIAN_POINT ( 'NONE',  ( 123.5000000000000000, 0.000000000000000000, -7.950000000000000178 ) ) ;
#127754 = CARTESIAN_POINT ( 'NONE',  ( -65.99451991528749772, 28.92564299267984396, 4.000000000000000000 ) ) ;
#127755 = ORIENTED_EDGE ( 'NONE', *, *, #3268, .F. ) ;
#127756 = ORIENTED_EDGE ( 'NONE', *, *, #74778, .F. ) ;
#127757 = CARTESIAN_POINT ( 'NONE',  ( 14.08373646989360317, -2.500000000000001776, 0.000000000000000000 ) ) ;
#127758 = VECTOR ( 'NONE', #40313, 1000.000000000000227 ) ;
#127759 = VECTOR ( 'NONE', #34924, 1000.000000000000000 ) ;
#127760 = ORIENTED_EDGE ( 'NONE', *, *, #55378, .F. ) ;
#127761 = CONICAL_SURFACE ( 'NONE', #65271, 2.055000000000000604, 0.9599310885968764806 ) ;
#127762 = CIRCLE ( 'NONE', #60738, 2.500000000000000444 ) ;
#127763 = DIRECTION ( 'NONE',  ( 0.6830127018922181881, 0.6830127018922202975, -0.2588190451025214056 ) ) ;
#127764 = EDGE_LOOP ( 'NONE', ( #90229, #118783, #89899, #142838 ) ) ;
#127765 =( NAMED_UNIT ( * ) PLANE_ANGLE_UNIT ( ) SI_UNIT ( $, .RADIAN. ) );
#127766 = ADVANCED_FACE ( 'NONE', ( #47297 ), #64852, .T. ) ;
#127767 = VECTOR ( 'NONE', #49811, 1000.000000000000000 ) ;
#127768 = CARTESIAN_POINT ( 'NONE',  ( 0.000000000000000000, 0.000000000000000000, 5.000000000000000000 ) ) ;
#127769 = EDGE_CURVE ( 'NONE', #20060, #22051, #48673, .T. ) ;
#127770 = FACE_BOUND ( 'NONE', #118378, .T. ) ;
#127771 = LINE ( 'NONE', #28460, #50353 ) ;
#127772 = EDGE_CURVE ( 'NONE', #52005, #63170, #24766, .T. ) ;
#127773 = ADVANCED_FACE ( 'NONE', ( #112496 ), #124797, .F. ) ;
#127774 = PLANE ( 'NONE',  #130139 ) ;
#127775 = VERTEX_POINT ( 'NONE', #137108 ) ;
#127777 = CARTESIAN_POINT ( 'NONE',  ( 33.18398860626899705, 28.73617430169810305, 5.000000000000000000 ) ) ;
#127776 = AXIS2_PLACEMENT_3D ( 'NONE', #29821, #18959, #53754 ) ;
#127779 = ORIENTED_EDGE ( 'NONE', *, *, #143093, .F. ) ;
#127778 = CARTESIAN_POINT ( 'NONE',  ( 53.99451991528749062, 28.92564299267975869, 4.000000000000000000 ) ) ;
#127780 = ORIENTED_EDGE ( 'NONE', *, *, #102614, .F. ) ;
#127781 = PLANE ( 'NONE',  #121221 ) ;
#127782 = ORIENTED_EDGE ( 'NONE', *, *, #26001, .T. ) ;
#127783 = EDGE_CURVE ( 'NONE', #26300, #73694, #13153, .T. ) ;
#127784 = ADVANCED_FACE ( 'NONE', ( #134994 ), #6528, .F. ) ;
#127785 = ORIENTED_EDGE ( 'NONE', *, *, #55588, .F. ) ;
#127786 = CARTESIAN_POINT ( 'NONE',  ( 65.68293019189810877, -1.637169565754158951, -6.109999999999998543 ) ) ;
#127787 = VERTEX_POINT ( 'NONE', #63842 ) ;
#127788 = DIRECTION ( 'NONE',  ( -0.7071067811865486830, -0.7071067811865464625, -0.000000000000000000 ) ) ;
#127789 = DIRECTION ( 'NONE',  ( -1.000000000000000000, -1.224606353822377258E-16, -0.000000000000000000 ) ) ;
#127790 = ADVANCED_FACE ( 'NONE', ( #51540 ), #16745, .F. ) ;
#127791 = ORIENTED_EDGE ( 'NONE', *, *, #20418, .T. ) ;
#127792 = PRESENTATION_STYLE_ASSIGNMENT (( #63954 ) ) ;
#127793 = EDGE_CURVE ( 'NONE', #2756, #8484, #118905, .T. ) ;
#127794 = VECTOR ( 'NONE', #56326, 1000.000000000000227 ) ;
#127795 = ADVANCED_FACE ( 'NONE', ( #83447 ), #129786, .F. ) ;
#127796 = AXIS2_PLACEMENT_3D ( 'NONE', #51808, #85121, #61292 ) ;
#127797 = LINE ( 'NONE', #125653, #17714 ) ;
#127798 = CARTESIAN_POINT ( 'NONE',  ( -14.22995720542196985, 21.73644205237998150, 5.000000000000000888 ) ) ;
#127799 = VECTOR ( 'NONE', #71119, 1000.000000000000000 ) ;
#127800 = CARTESIAN_POINT ( 'NONE',  ( 16.62500000000000000, 6.094999999999989981, -1.119633336120465690E-15 ) ) ;
#127801 = CARTESIAN_POINT ( 'NONE',  ( 0.000000000000000000, -4.870000000000014317, -36.99999999997771738 ) ) ;
#127802 = ORIENTED_EDGE ( 'NONE', *, *, #83613, .F. ) ;
#127803 = ORIENTED_EDGE ( 'NONE', *, *, #26982, .F. ) ;
#127804 = AXIS2_PLACEMENT_3D ( 'NONE', #91517, #125581, #137162 ) ;
#127805 = DIRECTION ( 'NONE',  ( 0.5735764363510444941, 0.8191520442889929088, 0.000000000000000000 ) ) ;
#127806 = LINE ( 'NONE', #105999, #74467 ) ;
#127807 = VERTEX_POINT ( 'NONE', #140653 ) ;
#127808 = ADVANCED_FACE ( 'NONE', ( #39226 ), #28353, .F. ) ;
#127809 = ORIENTED_EDGE ( 'NONE', *, *, #136683, .F. ) ;
#127810 = ORIENTED_EDGE ( 'NONE', *, *, #141269, .F. ) ;
#127811 = DIRECTION ( 'NONE',  ( -0.6830127018922180770, -0.6830127018922204085, -0.2588190451025213501 ) ) ;
#127812 = CARTESIAN_POINT ( 'NONE',  ( 55.20419371712956291, -6.884901960086285300, -3.975000000000000089 ) ) ;
#127813 = LINE ( 'NONE', #47433, #64737 ) ;
#127814 = ORIENTED_EDGE ( 'NONE', *, *, #125227, .T. ) ;
#127815 = LINE ( 'NONE', #91598, #108749 ) ;
#127816 = EDGE_CURVE ( 'NONE', #94981, #47967, #107318, .T. ) ;
#127817 = AXIS2_PLACEMENT_3D ( 'NONE', #121338, #122768, #2385 ) ;
#127818 = SURFACE_STYLE_FILL_AREA ( #129207 ) ;
#127819 = CARTESIAN_POINT ( 'NONE',  ( 7.796236474768553748, 7.934999999999990727, -1.457635852685135314E-15 ) ) ;
#127820 = CARTESIAN_POINT ( 'NONE',  ( 51.18398860626899705, 28.73617430169823095, 5.000000000000000000 ) ) ;
#127821 = ORIENTED_EDGE ( 'NONE', *, *, #114101, .T. ) ;
#127822 = CARTESIAN_POINT ( 'NONE',  ( 128.8287635252314658, 0.000000000000000000, -6.109999999999999432 ) ) ;
#127823 = DIRECTION ( 'NONE',  ( -0.3543493200069162685, -0.000000000000000000, -0.9351131265310288487 ) ) ;
#127824 = VECTOR ( 'NONE', #73030, 1000.000000000000000 ) ;
#127825 = EDGE_CURVE ( 'NONE', #104004, #45858, #244, .T. ) ;
#127826 = DIRECTION ( 'NONE',  ( 0.000000000000000000, 0.000000000000000000, -1.000000000000000000 ) ) ;
#127828 = ORIENTED_EDGE ( 'NONE', *, *, #23476, .F. ) ;
#127827 = LINE ( 'NONE', #5284, #19103 ) ;
#127830 = AXIS2_PLACEMENT_3D ( 'NONE', #128225, #139834, #141211 ) ;
#127829 = FACE_OUTER_BOUND ( 'NONE', #110792, .T. ) ;
#127831 = ORIENTED_EDGE ( 'NONE', *, *, #49890, .F. ) ;
#127832 = CARTESIAN_POINT ( 'NONE',  ( -1.499999999999994449, -1.592773361805376098, -6.492772025301226435 ) ) ;
#127833 = DIRECTION ( 'NONE',  ( -0.000000000000000000, 0.000000000000000000, 1.000000000000000000 ) ) ;
#127834 = LINE ( 'NONE', #26367, #10007 ) ;
#127835 = VERTEX_POINT ( 'NONE', #29746 ) ;
#127836 = EDGE_CURVE ( 'NONE', #5733, #62841, #130528, .T. ) ;
#127837 = EDGE_CURVE ( 'NONE', #112904, #111757, #7988, .T. ) ;
#127838 = PLANE ( 'NONE',  #44977 ) ;
#127839 = FACE_OUTER_BOUND ( 'NONE', #89083, .T. ) ;
#127840 = DIRECTION ( 'NONE',  ( -0.7071067811865486830, -0.7071067811865464625, 0.000000000000000000 ) ) ;
#127841 = VECTOR ( 'NONE', #33534, 1000.000000000000227 ) ;
#127842 = VERTEX_POINT ( 'NONE', #105178 ) ;
#127843 = CARTESIAN_POINT ( 'NONE',  ( 8.999999999999941380, -12.41253812416062985, 4.000000000000000000 ) ) ;
#127844 = DIRECTION ( 'NONE',  ( 0.7071067811865487940, 0.7071067811865463515, -0.000000000000000000 ) ) ;
#127846 = EDGE_CURVE ( 'NONE', #2765, #72157, #94996, .T. ) ;
#127845 = DIRECTION ( 'NONE',  ( -0.7071067811865486830, -0.7071067811865464625, 0.000000000000000000 ) ) ;
#127847 = DIRECTION ( 'NONE',  ( -0.7071067811865487940, 0.7071067811865463515, 0.000000000000000000 ) ) ;
#127848 = CARTESIAN_POINT ( 'NONE',  ( 0.000000000000000000, 0.000000000000000000, 0.000000000000000000 ) ) ;
#127849 = EDGE_LOOP ( 'NONE', ( #77619, #115881, #52775, #50546, #53254 ) ) ;
#127850 = ORIENTED_EDGE ( 'NONE', *, *, #27688, .F. ) ;
#127851 = VECTOR ( 'NONE', #28026, 1000.000000000000000 ) ;
#127852 = CARTESIAN_POINT ( 'NONE',  ( -12.20000000000000284, -34.64999999999999147, 17.49210858042622263 ) ) ;
#127853 =( NAMED_UNIT ( * ) SI_UNIT ( $, .STERADIAN. ) SOLID_ANGLE_UNIT ( ) );
#127854 = EDGE_CURVE ( 'NONE', #51304, #23998, #62417, .T. ) ;
#127855 = CARTESIAN_POINT ( 'NONE',  ( 7.562069808101887780, -7.934999999999991616, -2.126176841940955242 ) ) ;
#127856 = DIRECTION ( 'NONE',  ( 0.7071067811865487940, 0.7071067811865463515, -0.000000000000000000 ) ) ;
#127857 = LINE ( 'NONE', #127104, #36884 ) ;
#127858 = CARTESIAN_POINT ( 'NONE',  ( 34.49999999999975842, -13.53574439159937093, 4.994342998332162331 ) ) ;
#127859 = PLANE ( 'NONE',  #109313 ) ;
#127860 = ORIENTED_EDGE ( 'NONE', *, *, #20189, .F. ) ;
#127861 = EDGE_CURVE ( 'NONE', #20060, #86073, #138538, .T. ) ;
#127862 = PLANE ( 'NONE',  #9363 ) ;
#127863 = CARTESIAN_POINT ( 'NONE',  ( 128.8219055147127960, -52.14999999999999147, 41.05261164187028555 ) ) ;
#127864 = CARTESIAN_POINT ( 'NONE',  ( 19.93618820137057668, -3.269999999999996021, -36.39086428165683174 ) ) ;
#127865 = VECTOR ( 'NONE', #77924, 1000.000000000000000 ) ;
#127866 = VECTOR ( 'NONE', #134796, 1000.000000000000000 ) ;
#127867 = VECTOR ( 'NONE', #66763, 1000.000000000000000 ) ;
#127868 = LINE ( 'NONE', #72805, #126982 ) ;
#127869 = CARTESIAN_POINT ( 'NONE',  ( 44.24543019189810877, -5.291415217122919401, -3.055000000000000604 ) ) ;
#127870 = CARTESIAN_POINT ( 'NONE',  ( 183.8964364361580692, -51.76057561339556656, -38.69631370864702546 ) ) ;
#127871 = VECTOR ( 'NONE', #101046, 1000.000000000000000 ) ;
#127872 = VECTOR ( 'NONE', #117389, 999.9999999999998863 ) ;
#127873 = ORIENTED_EDGE ( 'NONE', *, *, #87012, .F. ) ;
#127874 = EDGE_CURVE ( 'NONE', #141465, #126332, #39968, .T. ) ;
#127875 = ORIENTED_EDGE ( 'NONE', *, *, #107287, .F. ) ;
#127876 = ORIENTED_EDGE ( 'NONE', *, *, #70818, .F. ) ;
#127877 = VECTOR ( 'NONE', #13928, 1000.000000000000000 ) ;
#127878 = AXIS2_PLACEMENT_3D ( 'NONE', #62622, #18345, #106801 ) ;
#127879 = CARTESIAN_POINT ( 'NONE',  ( 3.250000000000000000, 0.000000000000000000, 0.000000000000000000 ) ) ;
#127880 = AXIS2_PLACEMENT_3D ( 'NONE', #8925, #141658, #53195 ) ;
#127881 = CARTESIAN_POINT ( 'NONE',  ( -1.628234450443837744, -8.240707523384200428, 11.38925528200752879 ) ) ;
#127882 = CARTESIAN_POINT ( 'NONE',  ( 19.88840764549667384, -2.500000000000000888, 0.000000000000000000 ) ) ;
#127883 = CARTESIAN_POINT ( 'NONE',  ( -60.29974487139158867, -27.71228299555248142, 4.000000000000000000 ) ) ;
#127884 = EDGE_CURVE ( 'NONE', #65533, #131264, #111172, .T. ) ;
#127885 = FACE_OUTER_BOUND ( 'NONE', #117315, .T. ) ;
#127886 = ORIENTED_EDGE ( 'NONE', *, *, #18601, .F. ) ;
#127887 = DIRECTION ( 'NONE',  ( -0.7071067811865486830, -0.7071067811865464625, 0.000000000000000000 ) ) ;
#127888 = DIRECTION ( 'NONE',  ( -0.000000000000000000, -0.3543493200069152693, 0.9351131265310292928 ) ) ;
#127889 = CARTESIAN_POINT ( 'NONE',  ( 0.000000000000000000, 0.000000000000000000, 10.00000000000000000 ) ) ;
#127890 = CARTESIAN_POINT ( 'NONE',  ( -48.18398860626899705, 28.73617430169820608, 5.000000000000000000 ) ) ;
#127891 = LINE ( 'NONE', #130011, #71273 ) ;
#127892 = CARTESIAN_POINT ( 'NONE',  ( 67.30836038379622721, 7.949999999999997513, 2.130196079827431088 ) ) ;
#127893 = CARTESIAN_POINT ( 'NONE',  ( 72.48921356237309510, -27.52281430457106026, 5.000000000000000000 ) ) ;
#127894 = VERTEX_POINT ( 'NONE', #95733 ) ;
#127895 = ORIENTED_EDGE ( 'NONE', *, *, #62018, .F. ) ;
#127896 = CARTESIAN_POINT ( 'NONE',  ( 60.35416666666667140, -2.130196079827425315, -7.950000000000001066 ) ) ;
#127897 = PLANE ( 'NONE',  #125757 ) ;
#127898 = CARTESIAN_POINT ( 'NONE',  ( 0.000000000000000000, 0.000000000000000000, 5.000000000000000000 ) ) ;
#127899 = PLANE ( 'NONE',  #129426 ) ;
#127900 = EDGE_LOOP ( 'NONE', ( #75579, #99799, #133306, #87904 ) ) ;
#127901 = EDGE_CURVE ( 'NONE', #90863, #32826, #139981, .T. ) ;
#127902 = COLOUR_RGB ( '', 0.31764706, 0.68627451, 0.89019608) ;
#127903 = CARTESIAN_POINT ( 'NONE',  ( 34.24999999999998579, -9.735942053221458872E-16, 7.950000000000000178 ) ) ;
#127904 = ADVANCED_FACE ( 'NONE', ( #42809 ), #89154, .F. ) ;
#127905 = CARTESIAN_POINT ( 'NONE',  ( 12.03892749862900402, 2.055000000000001048, 2.516649172247811554E-16 ) ) ;
#127906 = CARTESIAN_POINT ( 'NONE',  ( 59.35459685856476142, -1.637169565754161615, 6.110000000000000320 ) ) ;
#127907 = VECTOR ( 'NONE', #122254, 1000.000000000000000 ) ;
#127908 = EDGE_LOOP ( 'NONE', ( #130916, #133956, #93392, #38572 ) ) ;
#127909 = CARTESIAN_POINT ( 'NONE',  ( 8.999999999999952038, 20.58746187583903264, 4.000000000000000000 ) ) ;
#127910 = ORIENTED_EDGE ( 'NONE', *, *, #74482, .F. ) ;
#127911 = ORIENTED_EDGE ( 'NONE', *, *, #84935, .T. ) ;
#127912 =( GEOMETRIC_REPRESENTATION_CONTEXT ( 3 ) GLOBAL_UNCERTAINTY_ASSIGNED_CONTEXT ( ( #108546 ) ) GLOBAL_UNIT_ASSIGNED_CONTEXT ( ( #60894, #79800, #102934 ) ) REPRESENTATION_CONTEXT ( 'NONE', 'WORKASPACE' ) );
#127913 = CARTESIAN_POINT ( 'NONE',  ( 29.99999999999979394, 12.83542986846999945, -1.025386466790438433 ) ) ;
#127914 = DIRECTION ( 'NONE',  ( 0.7071067811865487940, 0.7071067811865463515, -0.000000000000000000 ) ) ;
#127915 = DIRECTION ( 'NONE',  ( 0.000000000000000000, 0.000000000000000000, 1.000000000000000000 ) ) ;
#127916 = EDGE_CURVE ( 'NONE', #106511, #43627, #56572, .T. ) ;
#127917 = FACE_OUTER_BOUND ( 'NONE', #116541, .T. ) ;
#127919 = EDGE_LOOP ( 'NONE', ( #15913, #129816, #17572, #102635 ) ) ;
#127918 = CARTESIAN_POINT ( 'NONE',  ( 101.1416937171295558, -2.130196079827424871, -7.949999999999998401 ) ) ;
#127920 = DIRECTION ( 'NONE',  ( -0.000000000000000000, -0.3543493200069152693, 0.9351131265310292928 ) ) ;
#127921 = DIRECTION ( 'NONE',  ( 1.000000000000000000, 0.000000000000000000, 0.000000000000000000 ) ) ;
#127922 = CARTESIAN_POINT ( 'NONE',  ( -36.29974487139159578, -27.71228299555231445, 4.000000000000000000 ) ) ;
#127923 = CARTESIAN_POINT ( 'NONE',  ( 61.46640106136307935, -57.15000000000009095, 34.92499999999998295 ) ) ;
#127924 = ORIENTED_EDGE ( 'NONE', *, *, #108867, .F. ) ;
#127925 = ORIENTED_EDGE ( 'NONE', *, *, #101122, .F. ) ;
#127926 = DIRECTION ( 'NONE',  ( 0.7071067811865487940, 0.7071067811865463515, 0.000000000000000000 ) ) ;
#127927 = CARTESIAN_POINT ( 'NONE',  ( 30.48921356237309510, -27.52281430457076894, 5.000000000000000000 ) ) ;
#127928 = CARTESIAN_POINT ( 'NONE',  ( -25.49999999999982236, 18.05218569542898521, 5.000000000000000000 ) ) ;
#127929 = VECTOR ( 'NONE', #77312, 999.9999999999998863 ) ;
#127930 = CARTESIAN_POINT ( 'NONE',  ( -28.11017322888191217, -22.22500000000000142, 4.785647885939352086 ) ) ;
#127931 = ORIENTED_EDGE ( 'NONE', *, *, #118690, .F. ) ;
#127932 = VERTEX_POINT ( 'NONE', #34069 ) ;
#127933 = AXIS2_PLACEMENT_3D ( 'NONE', #59257, #135380, #57819 ) ;
#127934 = CARTESIAN_POINT ( 'NONE',  ( -32.38161509397984616, -2.240707523384260824, 13.37739548510246834 ) ) ;
#127935 = CYLINDRICAL_SURFACE ( 'NONE', #69956, 7.950000000000000178 ) ;
#127936 = ORIENTED_EDGE ( 'NONE', *, *, #114977, .F. ) ;
#127937 =( BOUNDED_CURVE ( )  B_SPLINE_CURVE ( 3, ( #26665, #102094, #92614, #4124 ),
 .UNSPECIFIED., .F., .F. ) 
 B_SPLINE_CURVE_WITH_KNOTS ( ( 4, 4 ),
 ( 2.779374508378134045, 4.199602562396839822 ),
 .UNSPECIFIED. ) 
 CURVE ( )  GEOMETRIC_REPRESENTATION_ITEM ( )  RATIONAL_B_SPLINE_CURVE ( ( 1.000000000000000000, 0.8388583629366623828, 0.8388583629366623828, 1.000000000000000000 ) ) 
 REPRESENTATION_ITEM ( '' )  );
#127938 = ORIENTED_EDGE ( 'NONE', *, *, #107315, .T. ) ;
#127939 = CARTESIAN_POINT ( 'NONE',  ( -19.25154412867563636, -11.24070752338416845, 10.39518518046013718 ) ) ;
#127940 = ORIENTED_EDGE ( 'NONE', *, *, #43133, .T. ) ;
#127941 = CARTESIAN_POINT ( 'NONE',  ( 0.000000000000000000, -21.72500000000000142, 4.500000000000000888 ) ) ;
#127942 = LINE ( 'NONE', #112511, #19263 ) ;
#127943 = VECTOR ( 'NONE', #19494, 999.9999999999998863 ) ;
#127944 =( BOUNDED_CURVE ( )  B_SPLINE_CURVE ( 3, ( #116896, #17567, #61831, #105991 ),
 .UNSPECIFIED., .F., .T. ) 
 B_SPLINE_CURVE_WITH_KNOTS ( ( 4, 4 ),
 ( 3.101920907804236460, 3.199716232068803290 ),
 .UNSPECIFIED. ) 
 CURVE ( )  GEOMETRIC_REPRESENTATION_ITEM ( )  RATIONAL_B_SPLINE_CURVE ( ( 1.000000000000000000, 0.9992031649997842324, 0.9992031649997842324, 1.000000000000000000 ) ) 
 REPRESENTATION_ITEM ( '' )  );
#127945 = FACE_BOUND ( 'NONE', #14850, .T. ) ;
#127946 = SURFACE_SIDE_STYLE ('',( #83006 ) ) ;
#127947 = EDGE_CURVE ( 'NONE', #39432, #9860, #122783, .T. ) ;
#127948 = DIRECTION ( 'NONE',  ( 0.6830127018922180770, -0.6830127018922204085, -0.2588190451025213501 ) ) ;
#127949 = VECTOR ( 'NONE', #115179, 1000.000000000000000 ) ;
#127951 = ORIENTED_EDGE ( 'NONE', *, *, #106620, .F. ) ;
#127950 = LINE ( 'NONE', #139558, #41243 ) ;
#127952 =( LENGTH_UNIT ( ) NAMED_UNIT ( * ) SI_UNIT ( .MILLI., .METRE. ) );
#127953 = SHAPE_DEFINITION_REPRESENTATION ( #22372, #108808 ) ;
#127954 = ORIENTED_EDGE ( 'NONE', *, *, #83613, .T. ) ;
#127955 = ADVANCED_FACE ( 'NONE', ( #23135 ), #77581, .F. ) ;
#127956 = EDGE_CURVE ( 'NONE', #39694, #62221, #20294, .T. ) ;
#127957 = VERTEX_POINT ( 'NONE', #122467 ) ;
#127958 = CARTESIAN_POINT ( 'NONE',  ( 95.28709685856479439, 3.054999999999997495, 5.291415217122919401 ) ) ;
#127959 = EDGE_LOOP ( 'NONE', ( #139755, #126189, #28003, #20094 ) ) ;
#127960 = EDGE_CURVE ( 'NONE', #16274, #128301, #121048, .T. ) ;
#127961 = LINE ( 'NONE', #50389, #81332 ) ;
#127962 = EDGE_CURVE ( 'NONE', #467, #28420, #54407, .T. ) ;
#127963 = DIRECTION ( 'NONE',  ( 0.7071067811865486830, -0.7071067811865464625, -0.000000000000000000 ) ) ;
#127964 = VECTOR ( 'NONE', #141563, 1000.000000000000227 ) ;
#127965 = VECTOR ( 'NONE', #71586, 1000.000000000000227 ) ;
#127966 = EDGE_CURVE ( 'NONE', #6023, #33545, #33381, .T. ) ;
#127967 = PLANE ( 'NONE',  #73448 ) ;
#127968 = VECTOR ( 'NONE', #65443, 1000.000000000000227 ) ;
#127969 = VECTOR ( 'NONE', #1671, 999.9999999999998863 ) ;
#127970 = CARTESIAN_POINT ( 'NONE',  ( -34.92500000000001137, 22.22500000000000142, 4.000000000000000000 ) ) ;
#127971 = ORIENTED_EDGE ( 'NONE', *, *, #50180, .T. ) ;
#127972 = DIRECTION ( 'NONE',  ( 0.7071067811865486830, -0.7071067811865464625, -0.000000000000000000 ) ) ;
#127973 = EDGE_CURVE ( 'NONE', #38542, #91904, #686, .T. ) ;
#127974 = CARTESIAN_POINT ( 'NONE',  ( -36.18398860626899705, 28.73617430169812437, 5.000000000000000000 ) ) ;
#127975 = DIRECTION ( 'NONE',  ( -0.000000000000000000, 0.000000000000000000, 1.000000000000000000 ) ) ;
#127976 = DIRECTION ( 'NONE',  ( -0.7071067811865487940, 0.7071067811865463515, 0.000000000000000000 ) ) ;
#127977 = CARTESIAN_POINT ( 'NONE',  ( 39.18398860626899705, 28.73617430169814568, 5.000000000000000000 ) ) ;
#127978 = DIRECTION ( 'NONE',  ( 0.7071067811865486830, -0.7071067811865464625, -0.000000000000000000 ) ) ;
#127979 = VECTOR ( 'NONE', #100257, 1000.000000000000000 ) ;
#127980 = VECTOR ( 'NONE', #94689, 1000.000000000000000 ) ;
#127981 = COLOUR_RGB ( '', 0.40784314, 0.44705882, 0.49803922) ;
#127982 = DIRECTION ( 'NONE',  ( -0.3543493200069163240, 0.000000000000000000, 0.9351131265310288487 ) ) ;
#127983 = EDGE_LOOP ( 'NONE', ( #25437, #70918, #139870, #59999, #130294 ) ) ;
#127984 = FACE_OUTER_BOUND ( 'NONE', #62877, .T. ) ;
#127985 = DIRECTION ( 'NONE',  ( 0.6830127018922181881, 0.6830127018922202975, -0.2588190451025214056 ) ) ;
#127986 = EDGE_CURVE ( 'NONE', #119991, #38500, #121749, .T. ) ;
#127987 = ORIENTED_EDGE ( 'NONE', *, *, #124988, .F. ) ;
#127988 = ORIENTED_EDGE ( 'NONE', *, *, #58497, .F. ) ;
#127989 = EDGE_CURVE ( 'NONE', #63130, #138721, #22427, .T. ) ;
#127990 = EDGE_LOOP ( 'NONE', ( #113519, #89309, #137496, #131021 ) ) ;
#127991 = CARTESIAN_POINT ( 'NONE',  ( 47.97959685856477563, 6.109999999999999432, 1.637169565754164280 ) ) ;
#127992 = ORIENTED_EDGE ( 'NONE', *, *, #17137, .F. ) ;
#127993 = EDGE_CURVE ( 'NONE', #30706, #102869, #12286, .T. ) ;
#127994 = VECTOR ( 'NONE', #137304, 999.9999999999998863 ) ;
#127995 = CARTESIAN_POINT ( 'NONE',  ( 20.31663961620377279, -1.633150327867691987, -6.094999999999989093 ) ) ;
#127996 = ORIENTED_EDGE ( 'NONE', *, *, #65791, .F. ) ;
#127997 = DIRECTION ( 'NONE',  ( -0.000000000000000000, 0.000000000000000000, 1.000000000000000000 ) ) ;
#127998 = ORIENTED_EDGE ( 'NONE', *, *, #140831, .T. ) ;
#127999 = LINE ( 'NONE', #106184, #115929 ) ;
#128000 = LINE ( 'NONE', #3991, #89207 ) ;
#128002 = EDGE_LOOP ( 'NONE', ( #94000, #113148, #86214, #117776 ) ) ;
#128001 = CARTESIAN_POINT ( 'NONE',  ( 15.20840764549667767, 9.139736423841732040E-16, 0.000000000000000000 ) ) ;
#128003 = ORIENTED_EDGE ( 'NONE', *, *, #128754, .F. ) ;
#128004 = FACE_OUTER_BOUND ( 'NONE', #85893, .T. ) ;
#128005 = AXIS2_PLACEMENT_3D ( 'NONE', #65955, #78234, #23082 ) ;
#128006 = FACE_OUTER_BOUND ( 'NONE', #95481, .T. ) ;
#128007 = EDGE_LOOP ( 'NONE', ( #30639, #141825, #142964, #91392 ) ) ;
#128008 = CARTESIAN_POINT ( 'NONE',  ( -39.18398860626899705, 28.73617430169814568, 5.000000000000000000 ) ) ;
#128009 = ORIENTED_EDGE ( 'NONE', *, *, #121882, .T. ) ;
#128010 = ORIENTED_EDGE ( 'NONE', *, *, #108303, .T. ) ;
#128011 = VECTOR ( 'NONE', #40138, 1000.000000000000000 ) ;
#128012 = ORIENTED_EDGE ( 'NONE', *, *, #31583, .F. ) ;
#128013 = VERTEX_POINT ( 'NONE', #64536 ) ;
#128014 = EDGE_CURVE ( 'NONE', #93893, #117034, #143519, .T. ) ;
#128015 = DIRECTION ( 'NONE',  ( -0.7071067811865486830, -0.7071067811865464625, 0.000000000000000000 ) ) ;
#128016 = VECTOR ( 'NONE', #111101, 1000.000000000000227 ) ;
#128017 = VECTOR ( 'NONE', #47702, 1000.000000000000000 ) ;
#128018 = CARTESIAN_POINT ( 'NONE',  ( -3.489213562373097322, -27.52281430457057709, 5.000000000000000000 ) ) ;
#128019 = CARTESIAN_POINT ( 'NONE',  ( -24.84463820744543838, 1.742823668393624903, 4.000000000000000000 ) ) ;
#128020 = DIRECTION ( 'NONE',  ( -0.000000000000000000, -0.3543493200069152693, 0.9351131265310292928 ) ) ;
#128021 = EDGE_LOOP ( 'NONE', ( #120129, #46843, #22084, #70417 ) ) ;
#128022 = FACE_OUTER_BOUND ( 'NONE', #131536, .T. ) ;
#128023 = EDGE_LOOP ( 'NONE', ( #19350, #85062, #27786, #64850 ) ) ;
#128024 = DIRECTION ( 'NONE',  ( 0.7071067811865486830, -0.7071067811865464625, -0.000000000000000000 ) ) ;
#128025 = EDGE_CURVE ( 'NONE', #60140, #133539, #142122, .T. ) ;
#128026 = AXIS2_PLACEMENT_3D ( 'NONE', #689, #34072, #21755 ) ;
#128027 = CARTESIAN_POINT ( 'NONE',  ( 33.52040314143522437, 7.934999999999989839, -2.126176841940961904 ) ) ;
#128028 = CARTESIAN_POINT ( 'NONE',  ( 27.48921356237309155, -27.52281430457074762, 5.000000000000000000 ) ) ;
#128029 = DIRECTION ( 'NONE',  ( 0.7071067811865486830, -0.7071067811865464625, -0.000000000000000000 ) ) ;
#128030 = ORIENTED_EDGE ( 'NONE', *, *, #27693, .T. ) ;
#128031 = ORIENTED_EDGE ( 'NONE', *, *, #54152, .T. ) ;
#128032 = ADVANCED_FACE ( 'NONE', ( #53684 ), #11546, .F. ) ;
#128033 = AXIS2_PLACEMENT_3D ( 'NONE', #133137, #121500, #1823 ) ;
#128034 = ORIENTED_EDGE ( 'NONE', *, *, #76417, .T. ) ;
#128035 = CARTESIAN_POINT ( 'NONE',  ( 34.49999999999975842, 14.14708470758594139, -0.5283514160167365192 ) ) ;
#128036 = PLANE ( 'NONE',  #2507 ) ;
#128037 = DIRECTION ( 'NONE',  ( -0.000000000000000000, -0.000000000000000000, -1.000000000000000000 ) ) ;
#128038 = VECTOR ( 'NONE', #95951, 1000.000000000000000 ) ;
#128039 = CARTESIAN_POINT ( 'NONE',  ( -5.999999999999956479, 16.93112307739201583, 4.000000000000000000 ) ) ;
#128040 = CARTESIAN_POINT ( 'NONE',  ( 0.8183591370940841436, -49.14999999999998437, -41.64500000000001023 ) ) ;
#128041 = CARTESIAN_POINT ( 'NONE',  ( 73.99543019189810877, 5.291415217122917625, 3.055000000000002380 ) ) ;
#128042 = PLANE ( 'NONE',  #32498 ) ;
#128043 = CARTESIAN_POINT ( 'NONE',  ( -8.708222910169469699, -15.74070752338412404, 19.73771281079095630 ) ) ;
#128044 = DIRECTION ( 'NONE',  ( 1.369518533665900312E-16, -1.000000000000000000, 0.000000000000000000 ) ) ;
#128045 = EDGE_CURVE ( 'NONE', #105369, #106357, #46358, .T. ) ;
#128046 = DIRECTION ( 'NONE',  ( 0.7071067811865487940, 0.7071067811865463515, -0.000000000000000000 ) ) ;
#128047 = DIRECTION ( 'NONE',  ( 0.7071067811865486830, -0.7071067811865464625, -0.000000000000000000 ) ) ;
#128048 = ORIENTED_EDGE ( 'NONE', *, *, #138657, .F. ) ;
#128049 = CARTESIAN_POINT ( 'NONE',  ( -26.20710678118635784, 9.759292476615618384, 5.000000000000000000 ) ) ;
#128050 = ORIENTED_EDGE ( 'NONE', *, *, #119679, .T. ) ;
#128051 = FACE_OUTER_BOUND ( 'NONE', #126313, .T. ) ;
#128053 = ORIENTED_EDGE ( 'NONE', *, *, #116, .F. ) ;
#128052 = DIRECTION ( 'NONE',  ( 0.000000000000000000, 1.000000000000000000, 0.000000000000000000 ) ) ;
#128054 = EDGE_CURVE ( 'NONE', #100921, #65559, #76135, .T. ) ;
#128055 = CARTESIAN_POINT ( 'NONE',  ( -24.48921356237309510, -27.52281430457072631, 5.000000000000000000 ) ) ;
#128056 = PLANE ( 'NONE',  #135185 ) ;
#128057 = VERTEX_POINT ( 'NONE', #100035 ) ;
#128059 = EDGE_LOOP ( 'NONE', ( #28703, #35586, #100771, #64069 ) ) ;
#128058 = CIRCLE ( 'NONE', #139661, 2.500000000000000888 ) ;
#128060 = SURFACE_SIDE_STYLE ('',( #140340 ) ) ;
#128061 = CARTESIAN_POINT ( 'NONE',  ( -17.67183060077635659, 20.25929247661551713, 4.000000000000000000 ) ) ;
#128062 = CARTESIAN_POINT ( 'NONE',  ( -62.99451991528749772, 28.92564299267982264, 4.000000000000000000 ) ) ;
#128063 = CARTESIAN_POINT ( 'NONE',  ( 89.62086038379622721, -6.884901960086286188, 3.974999999999997424 ) ) ;
#128064 = DIRECTION ( 'NONE',  ( 0.3543493200069162685, -0.000000000000000000, -0.9351131265310288487 ) ) ;
#128065 = EDGE_CURVE ( 'NONE', #288, #138468, #94925, .T. ) ;
#128066 = CARTESIAN_POINT ( 'NONE',  ( -33.70710678118631165, 17.25929247661554911, 5.000000000000000000 ) ) ;
#128067 = VERTEX_POINT ( 'NONE', #113748 ) ;
#128068 = LINE ( 'NONE', #128753, #139544 ) ;
#128069 = DIRECTION ( 'NONE',  ( -1.000000000000000000, -1.224606353822377258E-16, -0.000000000000000000 ) ) ;
#128070 = CARTESIAN_POINT ( 'NONE',  ( 30.77083333333333215, 6.094999999999991758, 1.633150327867687102 ) ) ;
#128071 = VECTOR ( 'NONE', #128377, 1000.000000000000000 ) ;
#128072 = CARTESIAN_POINT ( 'NONE',  ( 0.000000000000000000, 0.000000000000000000, 0.000000000000000000 ) ) ;
#128073 = ORIENTED_EDGE ( 'NONE', *, *, #16701, .F. ) ;
#128074 = VECTOR ( 'NONE', #89273, 1000.000000000000000 ) ;
#128075 = CARTESIAN_POINT ( 'NONE',  ( 45.43336038379621300, 2.130196079827431532, -7.949999999999996625 ) ) ;
#128076 = ORIENTED_EDGE ( 'NONE', *, *, #26656, .F. ) ;
#128077 = EDGE_CURVE ( 'NONE', #23623, #65100, #49237, .T. ) ;
#128078 = CARTESIAN_POINT ( 'NONE',  ( 82.25043019189810423, 3.055000000000002824, -5.291415217122919401 ) ) ;
#128079 = DIRECTION ( 'NONE',  ( 0.7071067811865487940, 0.7071067811865463515, -0.000000000000000000 ) ) ;
#128081 = CARTESIAN_POINT ( 'NONE',  ( 3.469446951953614189E-15, 13.55218569542902785, 5.000000000000000000 ) ) ;
#128080 = AXIS2_PLACEMENT_3D ( 'NONE', #30907, #141810, #119996 ) ;
#128082 =( GEOMETRIC_REPRESENTATION_CONTEXT ( 3 ) GLOBAL_UNCERTAINTY_ASSIGNED_CONTEXT ( ( #74825 ) ) GLOBAL_UNIT_ASSIGNED_CONTEXT ( ( #73720, #71595, #83179 ) ) REPRESENTATION_CONTEXT ( 'NONE', 'WORKASPACE' ) );
#128083 = LINE ( 'NONE', #38210, #91869 ) ;
#128084 = ORIENTED_EDGE ( 'NONE', *, *, #142555, .F. ) ;
#128085 = CARTESIAN_POINT ( 'NONE',  ( 0.005480084712502889671, 28.92564299267938210, 4.000000000000000000 ) ) ;
#128086 = LINE ( 'NONE', #49819, #16386 ) ;
#128087 = CARTESIAN_POINT ( 'NONE',  ( 32.99451991528749062, 28.92564299267960948, 4.000000000000000000 ) ) ;
#128088 = ADVANCED_FACE ( 'NONE', ( #14442 ), #92693, .F. ) ;
#128090 = ORIENTED_EDGE ( 'NONE', *, *, #51778, .T. ) ;
#128089 = CARTESIAN_POINT ( 'NONE',  ( -14.60438740478481989, -0.8081507193758268315, 4.000000000000000000 ) ) ;
#128091 = DIRECTION ( 'NONE',  ( -0.7071067811865486830, -0.7071067811865464625, 0.000000000000000000 ) ) ;
#128092 = CARTESIAN_POINT ( 'NONE',  ( 17.52487387214943837, 14.25929247661557220, 9.797011795316677762 ) ) ;
#128093 = CARTESIAN_POINT ( 'NONE',  ( 1.419567793309648884, -0.7546808561705602436, 6.635328531539133934 ) ) ;
#128094 = PLANE ( 'NONE',  #139617 ) ;
#128095 = PRODUCT_DEFINITION ( 'UNKNOWN', '', #104965, #58982 ) ;
#128096 = ORIENTED_EDGE ( 'NONE', *, *, #44082, .T. ) ;
#128097 = ORIENTED_EDGE ( 'NONE', *, *, #99940, .F. ) ;
#128098 = CARTESIAN_POINT ( 'NONE',  ( 70.87543019189810423, -5.291415217122920289, -3.055000000000001492 ) ) ;
#128099 = STYLED_ITEM ( 'NONE', ( #26922 ), #102640 ) ;
#128100 = ORIENTED_EDGE ( 'NONE', *, *, #6508, .T. ) ;
#128101 = FACE_OUTER_BOUND ( 'NONE', #52763, .T. ) ;
#128102 = PLANE ( 'NONE',  #115119 ) ;
#128103 = LINE ( 'NONE', #116492, #24905 ) ;
#128104 = ORIENTED_EDGE ( 'NONE', *, *, #63844, .T. ) ;
#128105 = CARTESIAN_POINT ( 'NONE',  ( -3.524001385854469870, 22.03583458319438648, 4.979811245910087614 ) ) ;
#128106 = LINE ( 'NONE', #38937, #35167 ) ;
#128107 = AXIS2_PLACEMENT_3D ( 'NONE', #89633, #101940, #78776 ) ;
#128108 = ORIENTED_EDGE ( 'NONE', *, *, #112248, .T. ) ;
#128109 = DIRECTION ( 'NONE',  ( -0.7071067811865487940, 0.7071067811865463515, 0.000000000000000000 ) ) ;
#128110 = DIRECTION ( 'NONE',  ( 1.000000000000000000, 0.000000000000000000, 0.000000000000000000 ) ) ;
#128111 = CARTESIAN_POINT ( 'NONE',  ( 7.139999999999992575, -35.14999999999999858, 17.49210858042621908 ) ) ;
#128112 = ORIENTED_EDGE ( 'NONE', *, *, #79705, .F. ) ;
#128114 = ORIENTED_EDGE ( 'NONE', *, *, #34040, .T. ) ;
#128113 = VECTOR ( 'NONE', #67028, 1000.000000000000000 ) ;
#128115 = LINE ( 'NONE', #62142, #101037 ) ;
#128116 = CARTESIAN_POINT ( 'NONE',  ( 11.99999999999993072, 11.58746187583912324, 4.000000000000000000 ) ) ;
#128117 = CARTESIAN_POINT ( 'NONE',  ( 2.292893218813443657, -9.740707523384184441, 5.000000000000000000 ) ) ;
#128118 = LINE ( 'NONE', #117195, #23201 ) ;
#128119 = CARTESIAN_POINT ( 'NONE',  ( 27.99999999999996803, -49.14999999999999147, 49.92499999999997584 ) ) ;
#128120 =( BOUNDED_CURVE ( )  B_SPLINE_CURVE ( 2, ( #130664, #119728, #31336, #20424, #106718, #108852, #117581, #51665, #53817, #87138, #95144, #139412, #128510 ),
 .UNSPECIFIED., .F., .T. ) 
 B_SPLINE_CURVE_WITH_KNOTS ( ( 3, 2, 2, 2, 2, 2, 3 ),
 ( 0.6000000000000000888, 0.6083333333333333925, 0.6166666666666668073, 0.6250000000000001110, 0.6333333333333334147, 0.6416666666666668295, 0.6500000000000001332 ),
 .UNSPECIFIED. ) 
 CURVE ( )  GEOMETRIC_REPRESENTATION_ITEM ( )  RATIONAL_B_SPLINE_CURVE ( ( 0.9999999999999995559, 0.9659258262890687563, 1.000000000000000000, 0.9659258262890683122, 1.000000000000000000, 0.9659258262890683122, 1.000000000000000000, 0.9659258262890683122, 1.000000000000000000, 0.9659258262890683122, 1.000000000000000000, 0.9659258262890678681, 1.000000000000000444 ) ) 
 REPRESENTATION_ITEM ( '' )  );
#128121 = DIRECTION ( 'NONE',  ( -0.7071067811865487940, 0.7071067811865463515, -0.000000000000000000 ) ) ;
#128122 = ORIENTED_EDGE ( 'NONE', *, *, #11254, .T. ) ;
#128123 = EDGE_CURVE ( 'NONE', #94183, #9187, #68846, .T. ) ;
#128124 =( GEOMETRIC_REPRESENTATION_CONTEXT ( 3 ) GLOBAL_UNCERTAINTY_ASSIGNED_CONTEXT ( ( #81147 ) ) GLOBAL_UNIT_ASSIGNED_CONTEXT ( ( #13492, #2627, #21000 ) ) REPRESENTATION_CONTEXT ( 'NONE', 'WORKASPACE' ) );
#128126 = VERTEX_POINT ( 'NONE', #79016 ) ;
#128125 = AXIS2_PLACEMENT_3D ( 'NONE', #7596, #51137, #140968 ) ;
#128127 = ORIENTED_EDGE ( 'NONE', *, *, #49823, .T. ) ;
#128128 = EDGE_CURVE ( 'NONE', #5353, #27958, #103561, .T. ) ;
#128129 = ORIENTED_EDGE ( 'NONE', *, *, #88668, .T. ) ;
#128130 = ADVANCED_FACE ( 'NONE', ( #125347 ), #134088, .F. ) ;
#128131 = VECTOR ( 'NONE', #112902, 1000.000000000000000 ) ;
#128132 = ADVANCED_FACE ( 'NONE', ( #136207 ), #27131, .T. ) ;
#128133 = FACE_OUTER_BOUND ( 'NONE', #137135, .T. ) ;
#128134 = DIRECTION ( 'NONE',  ( -1.000000000000000000, 0.000000000000000000, 0.000000000000000000 ) ) ;
#128135 = ORIENTED_EDGE ( 'NONE', *, *, #77838, .T. ) ;
#128136 = SURFACE_STYLE_USAGE ( .BOTH. , #93348 ) ;
#128137 = PLANE ( 'NONE',  #130549 ) ;
#128138 = CARTESIAN_POINT ( 'NONE',  ( -5.510786437626906675, -27.52281430457051314, 5.000000000000000000 ) ) ;
#128139 = DIRECTION ( 'NONE',  ( -0.7071067811865487940, 0.7071067811865463515, -0.000000000000000000 ) ) ;
#128140 = CIRCLE ( 'NONE', #93352, 3.000000000000000000 ) ;
#128141 = PLANE ( 'NONE',  #86184 ) ;
#128142 = ORIENTED_EDGE ( 'NONE', *, *, #88746, .F. ) ;
#128143 = DIRECTION ( 'NONE',  ( 0.7071067811865487940, 0.7071067811865463515, -0.000000000000000000 ) ) ;
#128144 = CARTESIAN_POINT ( 'NONE',  ( 11.99999999999991651, -18.03360074219755660, 5.000000000000000000 ) ) ;
#128145 = ADVANCED_FACE ( 'NONE', ( #127476 ), #94820, .T. ) ;
#128146 = ORIENTED_EDGE ( 'NONE', *, *, #122066, .T. ) ;
#128147 = DIRECTION ( 'NONE',  ( 0.3543493200069162685, -0.000000000000000000, -0.9351131265310288487 ) ) ;
#128148 = ORIENTED_EDGE ( 'NONE', *, *, #89811, .F. ) ;
#128149 = ADVANCED_FACE ( 'NONE', ( #27429 ), #40494, .F. ) ;
#128150 = CARTESIAN_POINT ( 'NONE',  ( 13.17080628287043886, -3.047499999999997211, -5.278424836066143655 ) ) ;
#128151 = VERTEX_POINT ( 'NONE', #5673 ) ;
#128152 = EDGE_LOOP ( 'NONE', ( #52658, #116386, #24020, #32595, #92933, #50901 ) ) ;
#128153 = CIRCLE ( 'NONE', #65686, 28.00000000000002487 ) ;
#128154 = CARTESIAN_POINT ( 'NONE',  ( 73.93793019189809002, -6.110000000000001208, 1.637169565754158951 ) ) ;
#128155 = ORIENTED_EDGE ( 'NONE', *, *, #82645, .T. ) ;
#128156 = EDGE_CURVE ( 'NONE', #75329, #94548, #52067, .T. ) ;
#128157 = LINE ( 'NONE', #73755, #81351 ) ;
#128158 = AXIS2_PLACEMENT_3D ( 'NONE', #65046, #118686, #63631 ) ;
#128159 = FACE_OUTER_BOUND ( 'NONE', #24319, .T. ) ;
#128160 = CARTESIAN_POINT ( 'NONE',  ( 110.5420968585647756, 5.291415217122923842, -3.054999999999996163 ) ) ;
#128161 = LINE ( 'NONE', #104213, #72621 ) ;
#128162 = LINE ( 'NONE', #17237, #32845 ) ;
#128163 = CARTESIAN_POINT ( 'NONE',  ( -12.48921356237309155, -27.52281430457064104, 5.000000000000000000 ) ) ;
#128164 = ADVANCED_FACE ( 'NONE', ( #28889 ), #106397, .T. ) ;
#128165 = DIRECTION ( 'NONE',  ( 0.6830127018922181881, 0.6830127018922202975, -0.2588190451025214056 ) ) ;
#128166 = DIRECTION ( 'NONE',  ( 0.000000000000000000, 0.000000000000000000, -1.000000000000000000 ) ) ;
#128167 = VECTOR ( 'NONE', #139740, 1000.000000000000000 ) ;
#128168 = CARTESIAN_POINT ( 'NONE',  ( -33.48921356237309510, -27.52281430457078670, 5.000000000000000000 ) ) ;
#128169 = CARTESIAN_POINT ( 'NONE',  ( 21.48921356237309155, -27.52281430457070499, 5.000000000000000000 ) ) ;
#128170 = EDGE_LOOP ( 'NONE', ( #131585, #122466, #107435, #63409 ) ) ;
#128171 = LINE ( 'NONE', #84653, #64541 ) ;
#128172 = DIRECTION ( 'NONE',  ( -0.6830127018922180770, -0.6830127018922204085, -0.2588190451025213501 ) ) ;
#128173 = ORIENTED_EDGE ( 'NONE', *, *, #84284, .F. ) ;
#128174 = VERTEX_POINT ( 'NONE', #16555 ) ;
#128175 = ADVANCED_FACE ( 'NONE', ( #105003 ), #58054, .T. ) ;
#128176 = LINE ( 'NONE', #108751, #132050 ) ;
#128177 = CARTESIAN_POINT ( 'NONE',  ( 114.2666937171295700, -7.949999999999998401, 2.130196079827423983 ) ) ;
#128178 = VERTEX_POINT ( 'NONE', #6357 ) ;
#128179 = LINE ( 'NONE', #97665, #26067 ) ;
#128180 = DIRECTION ( 'NONE',  ( 0.6830127018922180770, -0.6830127018922204085, -0.2588190451025213501 ) ) ;
#128181 = CARTESIAN_POINT ( 'NONE',  ( 2.292893218813443657, -18.74070752338408852, 5.000000000000000000 ) ) ;
#128182 = LINE ( 'NONE', #109072, #113458 ) ;
#128183 = ORIENTED_EDGE ( 'NONE', *, *, #101514, .F. ) ;
#128184 =( LENGTH_UNIT ( ) NAMED_UNIT ( * ) SI_UNIT ( .MILLI., .METRE. ) );
#128185 = ORIENTED_EDGE ( 'NONE', *, *, #120630, .T. ) ;
#128186 = AXIS2_PLACEMENT_3D ( 'NONE', #96523, #5943, #29860 ) ;
#128187 = EDGE_CURVE ( 'NONE', #100848, #123054, #116603, .T. ) ;
#128188 = AXIS2_PLACEMENT_3D ( 'NONE', #52769, #77436, #75975 ) ;
#128189 = CARTESIAN_POINT ( 'NONE',  ( 7.562069808101886892, -7.934999999999991616, -2.126176841940955242 ) ) ;
#128190 = FACE_OUTER_BOUND ( 'NONE', #134936, .T. ) ;
#128191 = CARTESIAN_POINT ( 'NONE',  ( 14.69991882521100557, -9.499962616874643828, 0.2903383370780639461 ) ) ;
#128192 = ORIENTED_EDGE ( 'NONE', *, *, #22469, .T. ) ;
#128193 = ORIENTED_EDGE ( 'NONE', *, *, #19445, .T. ) ;
#128194 = ORIENTED_EDGE ( 'NONE', *, *, #40625, .F. ) ;
#128195 = LINE ( 'NONE', #141177, #42673 ) ;
#128196 = DIRECTION ( 'NONE',  ( -0.7071067811865486830, 0.7071067811865464625, 0.000000000000000000 ) ) ;
#128197 = DIRECTION ( 'NONE',  ( -0.7071067811865486830, -0.7071067811865464625, 0.000000000000000000 ) ) ;
#128198 = AXIS2_PLACEMENT_3D ( 'NONE', #16147, #37961, #82197 ) ;
#128199 = FACE_OUTER_BOUND ( 'NONE', #42584, .T. ) ;
#128200 = CARTESIAN_POINT ( 'NONE',  ( -26.99999999999981171, 4.965500833774304290, -4.007596771432594629 ) ) ;
#128201 = CARTESIAN_POINT ( 'NONE',  ( -5.381615093979999820, -2.240707523384260824, 13.37739548510240617 ) ) ;
#128202 = VECTOR ( 'NONE', #11705, 1000.000000000000000 ) ;
#128203 = EDGE_CURVE ( 'NONE', #57963, #16196, #105695, .T. ) ;
#128204 = DIRECTION ( 'NONE',  ( 0.7071067811865486830, -0.7071067811865464625, -0.000000000000000000 ) ) ;
#128205 = ORIENTED_EDGE ( 'NONE', *, *, #19289, .T. ) ;
#128206 = PLANE ( 'NONE',  #90419 ) ;
#128207 = CARTESIAN_POINT ( 'NONE',  ( 19.41972383043609440, 4.584330080086930965E-16, 0.000000000000000000 ) ) ;
#128208 = ORIENTED_EDGE ( 'NONE', *, *, #14870, .T. ) ;
#128209 = AXIS2_PLACEMENT_3D ( 'NONE', #16174, #39410, #106043 ) ;
#128210 = CYLINDRICAL_SURFACE ( 'NONE', #52958, 2.500000000000000000 ) ;
#128212 = ORIENTED_EDGE ( 'NONE', *, *, #34657, .T. ) ;
#128211 = DIRECTION ( 'NONE',  ( -0.7071067811865486830, 0.7071067811865464625, 0.000000000000000000 ) ) ;
#128213 = EDGE_CURVE ( 'NONE', #77481, #19566, #62241, .T. ) ;
#128214 = LINE ( 'NONE', #106399, #74671 ) ;
#128215 = CARTESIAN_POINT ( 'NONE',  ( 34.92499999999998295, -9.908632306349565155, -7.176634499130175371 ) ) ;
#128216 = ORIENTED_EDGE ( 'NONE', *, *, #139385, .F. ) ;
#128217 = DIRECTION ( 'NONE',  ( -1.000000000000000000, 0.000000000000000000, 0.000000000000000000 ) ) ;
#128218 = VERTEX_POINT ( 'NONE', #95556 ) ;
#128219 = CIRCLE ( 'NONE', #19438, 3.000000000000001776 ) ;
#128220 = DIRECTION ( 'NONE',  ( -0.7071067811865486830, -0.7071067811865464625, -0.000000000000000000 ) ) ;
#128221 = CARTESIAN_POINT ( 'NONE',  ( 123.7458603837962272, 3.974999999999996980, 6.884901960086287964 ) ) ;
#128223 = VECTOR ( 'NONE', #20253, 1000.000000000000000 ) ;
#128222 = LINE ( 'NONE', #131065, #99381 ) ;
#128224 = LINE ( 'NONE', #49952, #138563 ) ;
#128225 = CARTESIAN_POINT ( 'NONE',  ( 9.489213562373095101, -27.52281430457062328, 5.000000000000000000 ) ) ;
#128226 = LINE ( 'NONE', #28190, #123550 ) ;
#128227 = CARTESIAN_POINT ( 'NONE',  ( -18.29974487139159223, -27.71228299555219010, 4.000000000000000000 ) ) ;
#128228 = CARTESIAN_POINT ( 'NONE',  ( 26.66623647476855652, 7.934999999999990727, -1.457635852685135314E-15 ) ) ;
#128229 = CARTESIAN_POINT ( 'NONE',  ( 7.562069808101886892, -7.934999999999990727, -2.126176841940955242 ) ) ;
#128230 = VECTOR ( 'NONE', #15648, 1000.000000000000227 ) ;
#128231 = LINE ( 'NONE', #37661, #25117 ) ;
#128232 = CARTESIAN_POINT ( 'NONE',  ( -17.99451991528748351, 28.92564299267950645, 4.000000000000000000 ) ) ;
#128233 = CARTESIAN_POINT ( 'NONE',  ( -9.792893218813384593, -8.240707523384198652, 5.000000000000000000 ) ) ;
#128234 = VERTEX_POINT ( 'NONE', #139818 ) ;
#128235 = EDGE_LOOP ( 'NONE', ( #23355, #97450, #86395, #71245 ) ) ;
#128236 = CARTESIAN_POINT ( 'NONE',  ( 80.47916666666664298, -7.950000000000001066, 2.130196079827424427 ) ) ;
#128237 = DIRECTION ( 'NONE',  ( -0.7071067811865486830, -0.7071067811865464625, 0.000000000000000000 ) ) ;
#128238 = ORIENTED_EDGE ( 'NONE', *, *, #132187, .T. ) ;
#128239 = ADVANCED_FACE ( 'NONE', ( #73817 ), #54931, .F. ) ;
#128240 = CARTESIAN_POINT ( 'NONE',  ( 8.207106781186489286, -2.240707523384260824, 5.000000000000000000 ) ) ;
#128241 = DIRECTION ( 'NONE',  ( 0.7071067811865487940, 0.7071067811865463515, 0.000000000000000000 ) ) ;
#128242 = VECTOR ( 'NONE', #18473, 1000.000000000000000 ) ;
#128243 = CARTESIAN_POINT ( 'NONE',  ( 30.85002705046288085, -5.819803920172573086, -5.819803920172573086 ) ) ;
#128244 = ORIENTED_EDGE ( 'NONE', *, *, #141182, .T. ) ;
#128245 = DIRECTION ( 'NONE',  ( 0.7071067811865487940, 0.7071067811865463515, 0.000000000000000000 ) ) ;
#128246 = LINE ( 'NONE', #16599, #92714 ) ;
#128247 = CARTESIAN_POINT ( 'NONE',  ( -16.17183060077636014, -8.240707523384191546, 4.000000000000000000 ) ) ;
#128248 = LINE ( 'NONE', #72474, #141499 ) ;
#128249 = ADVANCED_FACE ( 'NONE', ( #99847 ), #66519, .T. ) ;
#128250 = ADVANCED_FACE ( 'NONE', ( #20122 ), #9217, .F. ) ;
#128251 = DIRECTION ( 'NONE',  ( -0.7071067811865486830, -0.7071067811865464625, 0.000000000000000000 ) ) ;
#128252 = LINE ( 'NONE', #105736, #3444 ) ;
#128253 = DIRECTION ( 'NONE',  ( 0.6830127018922180770, -0.6830127018922204085, -0.2588190451025213501 ) ) ;
#128254 = LINE ( 'NONE', #48543, #103151 ) ;
#128255 = DIRECTION ( 'NONE',  ( -0.000000000000000000, 0.000000000000000000, 1.000000000000000000 ) ) ;
#128256 = PLANE ( 'NONE',  #84948 ) ;
#128257 = CARTESIAN_POINT ( 'NONE',  ( 7.499999999999951150, 9.052185695429074030, 5.000000000000000000 ) ) ;
#128258 = CARTESIAN_POINT ( 'NONE',  ( 13.49999999999990052, -15.29013452822853480, 0.3645803511610678505 ) ) ;
#128259 = ORIENTED_EDGE ( 'NONE', *, *, #102383, .T. ) ;
#128260 = VERTEX_POINT ( 'NONE', #54242 ) ;
#128261 = CARTESIAN_POINT ( 'NONE',  ( 101.2087635252314470, -7.482591942790329030E-16, 6.110000000000001208 ) ) ;
#128262 = CIRCLE ( 'NONE', #38028, 2.500000000000000888 ) ;
#128263 = VERTEX_POINT ( 'NONE', #31738 ) ;
#128264 = SURFACE_STYLE_USAGE ( .BOTH. , #83328 ) ;
#128265 = LINE ( 'NONE', #63025, #57339 ) ;
#128266 = ORIENTED_EDGE ( 'NONE', *, *, #132645, .T. ) ;
#128267 = ADVANCED_FACE ( 'NONE', ( #77420 ), #88993, .T. ) ;
#128268 = CARTESIAN_POINT ( 'NONE',  ( -24.79289321881328334, 9.759292476615614831, 5.000000000000000000 ) ) ;
#128270 = CIRCLE ( 'NONE', #88855, 6.350000000000001421 ) ;
#128269 = PLANE ( 'NONE',  #37320 ) ;
#128271 = CARTESIAN_POINT ( 'NONE',  ( 96.16209685856478018, -5.291415217122919401, 3.054999999999997939 ) ) ;
#128272 = EDGE_LOOP ( 'NONE', ( #128468, #128509, #48581, #46957 ) ) ;
#128273 = DIRECTION ( 'NONE',  ( 0.000000000000000000, 0.000000000000000000, 1.000000000000000000 ) ) ;
#128274 = VERTEX_POINT ( 'NONE', #98424 ) ;
#128275 = CARTESIAN_POINT ( 'NONE',  ( 24.06011071044004979, -9.740707523384187994, 10.89222023123375216 ) ) ;
#128276 = DIRECTION ( 'NONE',  ( -0.7071067811865487940, 0.7071067811865463515, -0.000000000000000000 ) ) ;
#128277 = DIRECTION ( 'NONE',  ( 0.7071067811865486830, -0.7071067811865464625, -0.000000000000000000 ) ) ;
#128278 = ORIENTED_EDGE ( 'NONE', *, *, #31528, .F. ) ;
#128279 = ORIENTED_EDGE ( 'NONE', *, *, #42057, .T. ) ;
#128280 = ORIENTED_EDGE ( 'NONE', *, *, #94990, .T. ) ;
#128281 = DIRECTION ( 'NONE',  ( -0.000000000000000000, -0.3543493200069152693, 0.9351131265310292928 ) ) ;
#128282 = CARTESIAN_POINT ( 'NONE',  ( -18.48921356237309510, -27.52281430457068367, 5.000000000000000000 ) ) ;
#128283 = CARTESIAN_POINT ( 'NONE',  ( 12.17123647476855375, 0.000000000000000000, 7.934999999999990727 ) ) ;
#128284 = VECTOR ( 'NONE', #35817, 1000.000000000000000 ) ;
#128285 = DIRECTION ( 'NONE',  ( -1.000000000000000000, -0.000000000000000000, -0.000000000000000000 ) ) ;
#128286 = EDGE_CURVE ( 'NONE', #87171, #29769, #36461, .T. ) ;
#128287 = SURFACE_STYLE_USAGE ( .BOTH. , #51444 ) ;
#128288 = VECTOR ( 'NONE', #20859, 1000.000000000000000 ) ;
#128289 = EDGE_CURVE ( 'NONE', #52479, #115565, #11715, .T. ) ;
#128290 = EDGE_LOOP ( 'NONE', ( #20522, #63868, #140509, #15787, #2841 ) ) ;
#128291 = VERTEX_POINT ( 'NONE', #41914 ) ;
#128292 = EDGE_CURVE ( 'NONE', #130094, #126512, #22960, .T. ) ;
#128293 = FACE_OUTER_BOUND ( 'NONE', #142805, .T. ) ;
#128294 = EDGE_LOOP ( 'NONE', ( #110221, #43393, #5568, #20318 ) ) ;
#128295 = VERTEX_POINT ( 'NONE', #86123 ) ;
#128296 = ADVANCED_FACE ( 'NONE', ( #109999 ), #22255, .F. ) ;
#128297 = ADVANCED_FACE ( 'NONE', ( #31042 ), #64368, .F. ) ;
#128298 = CARTESIAN_POINT ( 'NONE',  ( 117.0162635252314374, -4.472830434245838482, 4.472830434245838482 ) ) ;
#128299 = DIRECTION ( 'NONE',  ( 0.7071067811865487940, 0.7071067811865463515, 0.000000000000000000 ) ) ;
#128300 = CARTESIAN_POINT ( 'NONE',  ( 4.658131166821905644, 3.821174125832445049E-16, 0.000000000000000000 ) ) ;
#128301 = VERTEX_POINT ( 'NONE', #20845 ) ;
#128302 = AXIS2_PLACEMENT_3D ( 'NONE', #57075, #32444, #21566 ) ;
#128303 = LINE ( 'NONE', #48587, #133975 ) ;
#128304 = VECTOR ( 'NONE', #92950, 1000.000000000000000 ) ;
#128305 = DIRECTION ( 'NONE',  ( 0.7071067811865486830, -0.7071067811865464625, -0.000000000000000000 ) ) ;
#128306 = LINE ( 'NONE', #42012, #73853 ) ;
#128307 = DIRECTION ( 'NONE',  ( -0.000000000000000000, 0.3543493200069153248, 0.9351131265310292928 ) ) ;
#128308 = ORIENTED_EDGE ( 'NONE', *, *, #138082, .F. ) ;
#128309 = AXIS2_PLACEMENT_3D ( 'NONE', #19063, #106771, #32823 ) ;
#128310 = DIRECTION ( 'NONE',  ( 0.000000000000000000, 0.3543493200069153248, 0.9351131265310291818 ) ) ;
#128311 = DIRECTION ( 'NONE',  ( 0.7071067811865486830, -0.7071067811865464625, -0.000000000000000000 ) ) ;
#128312 = ADVANCED_FACE ( 'NONE', ( #110685 ), #87547, .F. ) ;
#128314 = VERTEX_POINT ( 'NONE', #133218 ) ;
#128313 = VECTOR ( 'NONE', #20446, 1000.000000000000000 ) ;
#128315 = CARTESIAN_POINT ( 'NONE',  ( -11.99999999999991296, 14.87792677143807651, -11.06722581663442639 ) ) ;
#128316 = CARTESIAN_POINT ( 'NONE',  ( 0.000000000000000000, 0.000000000000000000, 5.000000000000000000 ) ) ;
#128317 = DIRECTION ( 'NONE',  ( -0.7071067811865487940, 0.7071067811865463515, -0.000000000000000000 ) ) ;
#128318 = EDGE_CURVE ( 'NONE', #122297, #28555, #21582, .T. ) ;
#128319 = ORIENTED_EDGE ( 'NONE', *, *, #73298, .T. ) ;
#128320 = CARTESIAN_POINT ( 'NONE',  ( 26.99999999999981171, 7.588810512006234354, -3.013526669885291387 ) ) ;
#128321 = ORIENTED_EDGE ( 'NONE', *, *, #121701, .F. ) ;
#128322 = ORIENTED_EDGE ( 'NONE', *, *, #139614, .F. ) ;
#128323 = ORIENTED_EDGE ( 'NONE', *, *, #90452, .T. ) ;
#128324 = CARTESIAN_POINT ( 'NONE',  ( 29.07876352523144803, -7.482591942790325086E-16, 6.109999999999998543 ) ) ;
#128325 = VECTOR ( 'NONE', #72041, 1000.000000000000000 ) ;
#128326 = EDGE_CURVE ( 'NONE', #71954, #131551, #115160, .T. ) ;
#128327 = DIRECTION ( 'NONE',  ( -0.7071067811865486830, 0.7071067811865464625, 0.000000000000000000 ) ) ;
#128328 = LINE ( 'NONE', #63085, #14785 ) ;
#128329 = CARTESIAN_POINT ( 'NONE',  ( 0.5685132242927012358, 4.584330080086930965E-16, 0.000000000000000000 ) ) ;
#128330 = DIRECTION ( 'NONE',  ( 1.000000000000000000, 0.000000000000000000, 0.000000000000000000 ) ) ;
#128331 = DIRECTION ( 'NONE',  ( 0.3543493200069162685, -0.000000000000000000, -0.9351131265310288487 ) ) ;
#128333 = CARTESIAN_POINT ( 'NONE',  ( 51.48921356237309510, -27.52281430457091460, 5.000000000000000000 ) ) ;
#128332 = FACE_OUTER_BOUND ( 'NONE', #120280, .T. ) ;
#128334 = EDGE_CURVE ( 'NONE', #132789, #15438, #67337, .T. ) ;
#128335 = CARTESIAN_POINT ( 'NONE',  ( -23.90332935812580928, -2.240707523384260824, 15.26439735382746932 ) ) ;
#128336 = DIRECTION ( 'NONE',  ( -0.7071067811865487940, 0.7071067811865463515, 0.000000000000000000 ) ) ;
#128337 = DIRECTION ( 'NONE',  ( -0.7071067811865486830, 0.7071067811865464625, 0.000000000000000000 ) ) ;
#128338 = PLANE ( 'NONE',  #109622 ) ;
#128339 = ORIENTED_EDGE ( 'NONE', *, *, #116326, .F. ) ;
#128340 = ORIENTED_EDGE ( 'NONE', *, *, #80829, .F. ) ;
#128342 = ORIENTED_EDGE ( 'NONE', *, *, #18839, .T. ) ;
#128341 = EDGE_CURVE ( 'NONE', #19533, #75064, #125373, .T. ) ;
#128343 = ORIENTED_EDGE ( 'NONE', *, *, #85443, .T. ) ;
#128344 = DIRECTION ( 'NONE',  ( -0.000000000000000000, -0.000000000000000000, 1.000000000000000000 ) ) ;
#128345 = ORIENTED_EDGE ( 'NONE', *, *, #31398, .T. ) ;
#128346 = ORIENTED_EDGE ( 'NONE', *, *, #49779, .F. ) ;
#128347 = CARTESIAN_POINT ( 'NONE',  ( 0.2997448713915885632, -27.71228299555206220, 4.000000000000000000 ) ) ;
#128348 = PLANE ( 'NONE',  #131330 ) ;
#128349 = CARTESIAN_POINT ( 'NONE',  ( 54.18398860626899705, 28.73617430169825226, 5.000000000000000000 ) ) ;
#128350 = EDGE_CURVE ( 'NONE', #87398, #83942, #123766, .T. ) ;
#128351 = ORIENTED_EDGE ( 'NONE', *, *, #104908, .T. ) ;
#128352 = EDGE_CURVE ( 'NONE', #9752, #116419, #115923, .T. ) ;
#128353 = LINE ( 'NONE', #105838, #64923 ) ;
#128354 = VERTEX_POINT ( 'NONE', #112854 ) ;
#128355 = DIRECTION ( 'NONE',  ( -0.7071067811865486830, -0.7071067811865464625, -0.000000000000000000 ) ) ;
#128356 = EDGE_CURVE ( 'NONE', #103836, #75802, #14263, .T. ) ;
#128357 = CARTESIAN_POINT ( 'NONE',  ( -41.99451991528749062, 28.92564299267967343, 4.000000000000000000 ) ) ;
#128358 = CARTESIAN_POINT ( 'NONE',  ( 12.90040314143522160, -7.934999999999989839, 2.126176841940957907 ) ) ;
#128359 = VERTEX_POINT ( 'NONE', #47654 ) ;
#128360 = CARTESIAN_POINT ( 'NONE',  ( 104.4745968585647802, 1.637169565754164280, -6.109999999999997655 ) ) ;
#128361 = DIRECTION ( 'NONE',  ( -0.7071067811865487940, 0.7071067811865463515, -0.000000000000000000 ) ) ;
#128362 = CARTESIAN_POINT ( 'NONE',  ( 15.29974487139158867, -27.71228299555216879, 4.000000000000000000 ) ) ;
#128363 = ORIENTED_EDGE ( 'NONE', *, *, #78359, .T. ) ;
#128364 = VERTEX_POINT ( 'NONE', #125900 ) ;
#128365 = CARTESIAN_POINT ( 'NONE',  ( 8.999999999999941380, -13.44781430457069149, 5.000000000000000000 ) ) ;
#128366 = VERTEX_POINT ( 'NONE', #1219 ) ;
#128367 = FACE_OUTER_BOUND ( 'NONE', #57030, .T. ) ;
#128368 = EDGE_CURVE ( 'NONE', #59884, #35253, #35339, .T. ) ;
#128369 = PLANE ( 'NONE',  #7932 ) ;
#128370 = CARTESIAN_POINT ( 'NONE',  ( 184.1173099067128192, -47.89015928895675955, -37.22465919495432729 ) ) ;
#128372 = ORIENTED_EDGE ( 'NONE', *, *, #120953, .T. ) ;
#128371 = VECTOR ( 'NONE', #87478, 1000.000000000000000 ) ;
#128373 = LINE ( 'NONE', #71143, #64424 ) ;
#128374 = PLANE ( 'NONE',  #48870 ) ;
#128375 = ORIENTED_EDGE ( 'NONE', *, *, #41035, .T. ) ;
#128376 = CARTESIAN_POINT ( 'NONE',  ( 19.49999999999986500, -19.91253812416055879, 4.000000000000000000 ) ) ;
#128377 = DIRECTION ( 'NONE',  ( -0.7071067811865487940, 0.7071067811865463515, 0.000000000000000000 ) ) ;
#128378 = ORIENTED_EDGE ( 'NONE', *, *, #9227, .F. ) ;
#128380 = ORIENTED_EDGE ( 'NONE', *, *, #57651, .T. ) ;
#128379 = DIRECTION ( 'NONE',  ( -0.7071067811865486830, 0.7071067811865464625, 0.000000000000000000 ) ) ;
#128381 = ORIENTED_EDGE ( 'NONE', *, *, #17630, .T. ) ;
#128382 = CARTESIAN_POINT ( 'NONE',  ( 30.29974487139158867, -27.71228299555227537, 4.000000000000000000 ) ) ;
#128383 = DIRECTION ( 'NONE',  ( -0.000000000000000000, -0.3543493200069152693, 0.9351131265310292928 ) ) ;
#128384 = VECTOR ( 'NONE', #10962, 1000.000000000000000 ) ;
#128385 = VERTEX_POINT ( 'NONE', #2655 ) ;
#128386 = LINE ( 'NONE', #37821, #53451 ) ;
#128387 = DIRECTION ( 'NONE',  ( -0.7071067811865487940, 0.7071067811865463515, -0.000000000000000000 ) ) ;
#128388 = VECTOR ( 'NONE', #94346, 1000.000000000000227 ) ;
#128389 = CARTESIAN_POINT ( 'NONE',  ( 45.48921356237309510, -27.52281430457087197, 5.000000000000000000 ) ) ;
#128390 = DIRECTION ( 'NONE',  ( 0.7071067811865487940, -0.7071067811865463515, 0.000000000000000000 ) ) ;
#128392 = LINE ( 'NONE', #7284, #18806 ) ;
#128391 = VECTOR ( 'NONE', #17649, 1000.000000000000000 ) ;
#128393 = ADVANCED_FACE ( 'NONE', ( #70816 ), #102715, .T. ) ;
#128395 = EDGE_CURVE ( 'NONE', #68456, #98878, #91816, .T. ) ;
#128394 = LINE ( 'NONE', #94317, #90681 ) ;
#128396 = CARTESIAN_POINT ( 'NONE',  ( 47.37500000000000000, 7.950000000000000178, 1.460391307983218535E-15 ) ) ;
#128397 = CARTESIAN_POINT ( 'NONE',  ( -22.00193056682082471, -22.22500000000000142, 4.500000000000000888 ) ) ;
#128398 = DIRECTION ( 'NONE',  ( -0.7071067811865486830, -0.7071067811865464625, 0.000000000000000000 ) ) ;
#128399 = CARTESIAN_POINT ( 'NONE',  ( 21.70710678118639336, 17.25929247661554200, 5.000000000000000000 ) ) ;
#128400 = PLANE ( 'NONE',  #32714 ) ;
#128401 = DIRECTION ( 'NONE',  ( 1.000000000000000000, 1.224606353822377258E-16, 0.000000000000000000 ) ) ;
#128402 = ORIENTED_EDGE ( 'NONE', *, *, #48779, .F. ) ;
#128403 = EDGE_LOOP ( 'NONE', ( #117289, #115187, #48522, #53630 ) ) ;
#128404 = ORIENTED_EDGE ( 'NONE', *, *, #48196, .F. ) ;
#128405 = CARTESIAN_POINT ( 'NONE',  ( 114.4583333333333286, 3.974999999999997424, 6.884901960086288852 ) ) ;
#128406 = VERTEX_POINT ( 'NONE', #14961 ) ;
#128407 = CIRCLE ( 'NONE', #130803, 2.055000000000000604 ) ;
#128408 = EDGE_LOOP ( 'NONE', ( #34134, #30699, #138709, #142913 ) ) ;
#128409 = ORIENTED_EDGE ( 'NONE', *, *, #70196, .T. ) ;
#128410 = CARTESIAN_POINT ( 'NONE',  ( -9.299744871391588674, -27.71228299555212971, 4.000000000000000000 ) ) ;
#128411 = FACE_OUTER_BOUND ( 'NONE', #136429, .T. ) ;
#128412 = ORIENTED_EDGE ( 'NONE', *, *, #14768, .T. ) ;
#128413 = FACE_OUTER_BOUND ( 'NONE', #41864, .T. ) ;
#128414 = CARTESIAN_POINT ( 'NONE',  ( 0.3281693992235271695, 8.259292476615637923, 4.000000000000000000 ) ) ;
#128415 = CARTESIAN_POINT ( 'NONE',  ( 34.49999999999976552, 6.431123077392124188, 4.000000000000000000 ) ) ;
#128416 = DIRECTION ( 'NONE',  ( 0.000000000000000000, 1.000000000000000000, -0.000000000000000000 ) ) ;
#128417 = CARTESIAN_POINT ( 'NONE',  ( 100.3337635252314328, 6.110000000000001208, 1.122388791418549305E-15 ) ) ;
#128418 = EDGE_CURVE ( 'NONE', #14590, #137119, #13525, .T. ) ;
#128419 = ORIENTED_EDGE ( 'NONE', *, *, #62139, .F. ) ;
#128420 = PLANE ( 'NONE',  #127468 ) ;
#128421 = CARTESIAN_POINT ( 'NONE',  ( 151.4000000000000057, -18.48000000000005372, 34.92499999999998295 ) ) ;
#128422 = EDGE_CURVE ( 'NONE', #49880, #79180, #91142, .T. ) ;
#128423 = DIRECTION ( 'NONE',  ( -0.7071067811865487940, 0.7071067811865463515, 0.000000000000000000 ) ) ;
#128424 = PLANE ( 'NONE',  #1168 ) ;
#128425 = CARTESIAN_POINT ( 'NONE',  ( -65.99451991528749772, 28.92564299267984396, 4.000000000000000000 ) ) ;
#128426 = CARTESIAN_POINT ( 'NONE',  ( -2.999999999999973355, -9.412538124160660047, 4.000000000000000000 ) ) ;
#128427 = VECTOR ( 'NONE', #67951, 1000.000000000000227 ) ;
#128428 = CARTESIAN_POINT ( 'NONE',  ( 39.74586038379622721, 3.974999999999996980, 6.884901960086287964 ) ) ;
#128429 = CARTESIAN_POINT ( 'NONE',  ( 45.18398860626900415, 28.73617430169818832, 5.000000000000000000 ) ) ;
#128430 = AXIS2_PLACEMENT_3D ( 'NONE', #57409, #2252, #71859 ) ;
#128431 = DIRECTION ( 'NONE',  ( 0.6830127018922181881, 0.6830127018922202975, -0.2588190451025214056 ) ) ;
#128432 = ORIENTED_EDGE ( 'NONE', *, *, #79206, .T. ) ;
#128433 = ORIENTED_EDGE ( 'NONE', *, *, #15007, .T. ) ;
#128434 = VECTOR ( 'NONE', #60828, 1000.000000000000000 ) ;
#128435 = CARTESIAN_POINT ( 'NONE',  ( 126.8754301918981184, -5.291415217122920289, -3.055000000000001492 ) ) ;
#128436 = ORIENTED_EDGE ( 'NONE', *, *, #99080, .F. ) ;
#128438 = EDGE_CURVE ( 'NONE', #84400, #8423, #4039, .T. ) ;
#128437 = MECHANICAL_DESIGN_GEOMETRIC_PRESENTATION_REPRESENTATION (  '', ( #28868 ), #121473 ) ;
#128439 = DIRECTION ( 'NONE',  ( -0.7071067811865487940, 0.7071067811865463515, -0.000000000000000000 ) ) ;
#128440 = DIRECTION ( 'NONE',  ( 0.3543493200069162685, -0.000000000000000000, -0.9351131265310288487 ) ) ;
#128441 = PLANE ( 'NONE',  #68823 ) ;
#128442 = DIRECTION ( 'NONE',  ( -0.6830127018922181881, 0.6830127018922202975, -0.2588190451025214056 ) ) ;
#128443 = EDGE_CURVE ( 'NONE', #77659, #28316, #46952, .T. ) ;
#128444 = SURFACE_STYLE_FILL_AREA ( #106645 ) ;
#128445 = DIRECTION ( 'NONE',  ( 0.7071067811865487940, 0.7071067811865463515, 0.000000000000000000 ) ) ;
#128446 = CARTESIAN_POINT ( 'NONE',  ( 125.0370968585647944, -3.054999999999998828, -5.291415217122919401 ) ) ;
#128447 = ORIENTED_EDGE ( 'NONE', *, *, #14636, .T. ) ;
#128448 = CARTESIAN_POINT ( 'NONE',  ( -6.489213562373093325, -27.52281430457059841, 5.000000000000000000 ) ) ;
#128449 = ORIENTED_EDGE ( 'NONE', *, *, #40741, .F. ) ;
#128450 = EDGE_CURVE ( 'NONE', #85002, #78692, #41101, .T. ) ;
#128451 = DIRECTION ( 'NONE',  ( 0.7071067811865486830, -0.7071067811865464625, -0.000000000000000000 ) ) ;
#128452 = DIRECTION ( 'NONE',  ( 0.7071067811865487940, 0.7071067811865463515, 0.000000000000000000 ) ) ;
#128453 = FACE_OUTER_BOUND ( 'NONE', #40688, .T. ) ;
#128454 = ORIENTED_EDGE ( 'NONE', *, *, #109950, .T. ) ;
#128455 = CARTESIAN_POINT ( 'NONE',  ( 47.39626352523143282, 4.472830434245840259, -4.472830434245839371 ) ) ;
#128456 = ORIENTED_EDGE ( 'NONE', *, *, #47739, .T. ) ;
#128457 = DIRECTION ( 'NONE',  ( -0.000000000000000000, -0.3543493200069152693, 0.9351131265310292928 ) ) ;
#128458 = FACE_OUTER_BOUND ( 'NONE', #53723, .T. ) ;
#128459 = CARTESIAN_POINT ( 'NONE',  ( 11.21837311707497342, 21.74787736706806740, 4.999607392498049308 ) ) ;
#128460 = ADVANCED_FACE ( 'NONE', ( #89681 ), #113566, .T. ) ;
#128461 = CARTESIAN_POINT ( 'NONE',  ( 128.5894344200537773, -49.14999999999999147, -39.86617647058817226 ) ) ;
#128462 = CARTESIAN_POINT ( 'NONE',  ( 51.82876352523144448, 0.000000000000000000, -6.109999999999998543 ) ) ;
#128463 = ORIENTED_EDGE ( 'NONE', *, *, #12524, .T. ) ;
#128464 = PLANE ( 'NONE',  #62782 ) ;
#128465 = EDGE_CURVE ( 'NONE', #123393, #69699, #23714, .T. ) ;
#128466 = FACE_OUTER_BOUND ( 'NONE', #25569, .T. ) ;
#128467 = ORIENTED_EDGE ( 'NONE', *, *, #132696, .T. ) ;
#128468 = ORIENTED_EDGE ( 'NONE', *, *, #101794, .T. ) ;
#128469 = ORIENTED_EDGE ( 'NONE', *, *, #5304, .T. ) ;
#128470 = VECTOR ( 'NONE', #13103, 1000.000000000000227 ) ;
#128471 = EDGE_CURVE ( 'NONE', #5899, #27583, #16377, .T. ) ;
#128472 = EDGE_CURVE ( 'NONE', #64350, #83371, #51282, .T. ) ;
#128473 = CARTESIAN_POINT ( 'NONE',  ( 60.60002705046289861, 5.819803920172570422, 5.819803920172575751 ) ) ;
#128474 = PRODUCT_DEFINITION_CONTEXT ( 'detailed design', #129112, 'design' ) ;
#128475 = ORIENTED_EDGE ( 'NONE', *, *, #24868, .T. ) ;
#128476 = CARTESIAN_POINT ( 'NONE',  ( 43.68336038379622011, -2.130196079827426203, 7.949999999999996625 ) ) ;
#128477 = EDGE_CURVE ( 'NONE', #89594, #12213, #51914, .T. ) ;
#128478 = CARTESIAN_POINT ( 'NONE',  ( 34.71789321881347945, -22.26999999999999247, -0.2071067811865477115 ) ) ;
#128479 = FACE_BOUND ( 'NONE', #71985, .T. ) ;
#128480 = ADVANCED_FACE ( 'NONE', ( #15643 ), #83848, .F. ) ;
#128481 = SURFACE_STYLE_USAGE ( .BOTH. , #129168 ) ;
#128482 = DIRECTION ( 'NONE',  ( 0.7071067811865487940, -0.7071067811865463515, 0.000000000000000000 ) ) ;
#128483 = DIRECTION ( 'NONE',  ( -0.7071067811865486830, 0.7071067811865464625, 0.000000000000000000 ) ) ;
#128484 = EDGE_CURVE ( 'NONE', #57093, #32412, #41019, .T. ) ;
#128485 = VERTEX_POINT ( 'NONE', #49786 ) ;
#128486 = FILL_AREA_STYLE_COLOUR ( '', #11011 ) ;
#128487 = ORIENTED_EDGE ( 'NONE', *, *, #48886, .T. ) ;
#128488 = ORIENTED_EDGE ( 'NONE', *, *, #48582, .F. ) ;
#128489 = DIRECTION ( 'NONE',  ( 0.7071067811865487940, 0.7071067811865463515, 0.000000000000000000 ) ) ;
#128490 = ORIENTED_EDGE ( 'NONE', *, *, #129966, .F. ) ;
#128491 = CONICAL_SURFACE ( 'NONE', #68294, 2.500000000000000888, 0.9599310885968822538 ) ;
#128492 = CARTESIAN_POINT ( 'NONE',  ( 60.72459685856477307, -1.637169565754160949, 6.109999999999997655 ) ) ;
#128493 = ORIENTED_EDGE ( 'NONE', *, *, #61472, .T. ) ;
#128494 =( BOUNDED_CURVE ( )  B_SPLINE_CURVE ( 2, ( #40958, #130850, #85161, #20611, #130120, #76461, #107626, #52536, #120629, #129375, #57569, #135138, #89449 ),
 .UNSPECIFIED., .F., .T. ) 
 B_SPLINE_CURVE_WITH_KNOTS ( ( 3, 2, 2, 2, 2, 2, 3 ),
 ( 0.7666666666666666075, 0.7694444444444443754, 0.7722222222222221433, 0.7749999999999999112, 0.7777777777777777901, 0.7805555555555555580, 0.7833333333333333259 ),
 .UNSPECIFIED. ) 
 CURVE ( )  GEOMETRIC_REPRESENTATION_ITEM ( )  RATIONAL_B_SPLINE_CURVE ( ( 1.000000000000001332, 0.9659258262890669799, 1.000000000000000000, 0.9659258262890683122, 1.000000000000000000, 0.9659258262890683122, 1.000000000000000000, 0.9659258262890683122, 1.000000000000000000, 0.9659258262890683122, 1.000000000000000000, 0.9659258262890683122, 1.000000000000000000 ) ) 
 REPRESENTATION_ITEM ( '' )  );
#128495 = ADVANCED_FACE ( 'NONE', ( #30130 ), #125164, .T. ) ;
#128496 = CARTESIAN_POINT ( 'NONE',  ( 42.48921356237308800, -27.52281430457085065, 5.000000000000000000 ) ) ;
#128497 = AXIS2_PLACEMENT_3D ( 'NONE', #134306, #25514, #126272 ) ;
#128498 = CARTESIAN_POINT ( 'NONE',  ( -27.48921356237309155, -27.52281430457074762, 5.000000000000000000 ) ) ;
#128499 = ORIENTED_EDGE ( 'NONE', *, *, #138395, .T. ) ;
#128500 = DIRECTION ( 'NONE',  ( 0.7071067811865486830, -0.7071067811865464625, -0.000000000000000000 ) ) ;
#128501 = EDGE_CURVE ( 'NONE', #73867, #68609, #18517, .T. ) ;
#128502 = CARTESIAN_POINT ( 'NONE',  ( 35.99999999999999289, 0.000000000000000000, -7.950000000000000178 ) ) ;
#128503 = VECTOR ( 'NONE', #110870, 1000.000000000000000 ) ;
#128504 = CARTESIAN_POINT ( 'NONE',  ( -12.79333936457838661, 21.75929247661549581, 4.998822639870701856 ) ) ;
#128505 = CARTESIAN_POINT ( 'NONE',  ( 34.42499999999998295, -21.72500000000000142, 0.000000000000000000 ) ) ;
#128506 = DIRECTION ( 'NONE',  ( -0.7071067811865487940, 0.7071067811865463515, -0.000000000000000000 ) ) ;
#128507 = FACE_OUTER_BOUND ( 'NONE', #20987, .T. ) ;
#128508 = EDGE_LOOP ( 'NONE', ( #39888, #40833, #40315, #78825 ) ) ;
#128509 = ORIENTED_EDGE ( 'NONE', *, *, #114068, .T. ) ;
#128510 = CARTESIAN_POINT ( 'NONE',  ( 20.46247294953710849, -7.464222240803106570E-16, -6.094999999999989981 ) ) ;
#128511 = DIRECTION ( 'NONE',  ( 1.000000000000000000, 0.000000000000000000, 0.000000000000000000 ) ) ;
#128512 = ORIENTED_EDGE ( 'NONE', *, *, #74069, .F. ) ;
#128513 = VERTEX_POINT ( 'NONE', #126575 ) ;
#128514 = ORIENTED_EDGE ( 'NONE', *, *, #64840, .T. ) ;
#128515 = CARTESIAN_POINT ( 'NONE',  ( 19.41999999999999815, -2.055000000000000160, 0.000000000000000000 ) ) ;
#128516 = DIRECTION ( 'NONE',  ( 0.000000000000000000, -1.000000000000000000, 0.000000000000000000 ) ) ;
#128517 = VERTEX_POINT ( 'NONE', #61394 ) ;
#128518 = DIRECTION ( 'NONE',  ( -0.7071067811865487940, 8.659560562354918067E-17, -0.7071067811865463515 ) ) ;
#128519 = VECTOR ( 'NONE', #132733, 1000.000000000000227 ) ;
#128520 = EDGE_CURVE ( 'NONE', #132519, #49642, #94662, .T. ) ;
#128521 = CARTESIAN_POINT ( 'NONE',  ( -34.92500000000001137, 10.70193056682090749, 4.500000000000000888 ) ) ;
#128523 = EDGE_CURVE ( 'NONE', #59504, #57055, #4753, .T. ) ;
#128522 = VECTOR ( 'NONE', #43123, 999.9999999999998863 ) ;
#128524 = CARTESIAN_POINT ( 'NONE',  ( 10.27540314143522160, -2.126176841940958351, -7.934999999999989839 ) ) ;
#128525 = VECTOR ( 'NONE', #98386, 1000.000000000000000 ) ;
#128526 = CARTESIAN_POINT ( 'NONE',  ( -2.999999999999975131, 1.552185695429149304, 5.000000000000000000 ) ) ;
#128527 = ORIENTED_EDGE ( 'NONE', *, *, #82428, .F. ) ;
#128528 = DIRECTION ( 'NONE',  ( 0.3543493200069162685, -0.000000000000000000, -0.9351131265310288487 ) ) ;
#128529 = CIRCLE ( 'NONE', #12796, 2.055000000000001048 ) ;
#128530 = CARTESIAN_POINT ( 'NONE',  ( -17.99999999999986855, -10.44781430457071991, 5.000000000000000000 ) ) ;
#128531 = PLANE ( 'NONE',  #91280 ) ;
#128533 = EDGE_LOOP ( 'NONE', ( #130597, #16328, #105007, #95231 ) ) ;
#128532 = CARTESIAN_POINT ( 'NONE',  ( -15.18398860626900237, 28.73617430169797871, 5.000000000000000000 ) ) ;
#128534 = DIRECTION ( 'NONE',  ( 0.7071067811865486830, -0.7071067811865464625, -0.000000000000000000 ) ) ;
#128535 = ORIENTED_EDGE ( 'NONE', *, *, #22109, .F. ) ;
#128536 = FACE_OUTER_BOUND ( 'NONE', #37536, .T. ) ;
#128537 = FACE_OUTER_BOUND ( 'NONE', #120932, .T. ) ;
#128538 = ORIENTED_EDGE ( 'NONE', *, *, #130876, .F. ) ;
#128539 = CARTESIAN_POINT ( 'NONE',  ( -9.489213562373095101, -27.52281430457062328, 5.000000000000000000 ) ) ;
#128540 = CARTESIAN_POINT ( 'NONE',  ( -39.18398860626899705, 28.73617430169814568, 5.000000000000000000 ) ) ;
#128541 = CARTESIAN_POINT ( 'NONE',  ( -23.48334561358938899, 22.22500000000000142, 4.500000000000000888 ) ) ;
#128542 = ORIENTED_EDGE ( 'NONE', *, *, #33910, .F. ) ;
#128543 = CARTESIAN_POINT ( 'NONE',  ( -3.489213562373097322, -27.52281430457057709, 5.000000000000000000 ) ) ;
#128544 = DIRECTION ( 'NONE',  ( 0.6830127018922180770, -0.6830127018922204085, -0.2588190451025213501 ) ) ;
#128545 = CARTESIAN_POINT ( 'NONE',  ( 11.50183651486036496, -17.24070752338410628, 8.407044977365197624 ) ) ;
#128546 = LINE ( 'NONE', #29213, #21708 ) ;
#128547 = CARTESIAN_POINT ( 'NONE',  ( 16.17183060077635304, -20.24070752338408141, 4.000000000000000000 ) ) ;
#128548 = ORIENTED_EDGE ( 'NONE', *, *, #90615, .F. ) ;
#128549 = ORIENTED_EDGE ( 'NONE', *, *, #61278, .T. ) ;
#128550 = CARTESIAN_POINT ( 'NONE',  ( -39.18398860626899705, 28.73617430169814568, 5.000000000000000000 ) ) ;
#128551 = LINE ( 'NONE', #116946, #110778 ) ;
#128552 = CARTESIAN_POINT ( 'NONE',  ( 14.70790314143522082, -6.871911579029513106, -3.967499999999993587 ) ) ;
#128553 = DIRECTION ( 'NONE',  ( 0.6830127018922180770, -0.6830127018922204085, -0.2588190451025213501 ) ) ;
#128554 = DIRECTION ( 'NONE',  ( 0.6830127018922180770, -0.6830127018922204085, -0.2588190451025213501 ) ) ;
#128555 = CARTESIAN_POINT ( 'NONE',  ( 9.792893218813388145, 12.75929247661558996, 5.000000000000000000 ) ) ;
#128556 = ORIENTED_EDGE ( 'NONE', *, *, #73034, .T. ) ;
#128557 = FACE_OUTER_BOUND ( 'NONE', #138070, .T. ) ;
#128558 = DIRECTION ( 'NONE',  ( -1.000000000000000000, -1.224606353822377258E-16, -0.000000000000000000 ) ) ;
#128559 = DIRECTION ( 'NONE',  ( 0.7071067811865487940, 0.7071067811865463515, -0.000000000000000000 ) ) ;
#128560 = CARTESIAN_POINT ( 'NONE',  ( 2.999999999999999112, -4.599999999999996980, -17.44999999999995310 ) ) ;
#128561 = CARTESIAN_POINT ( 'NONE',  ( 48.91209685856478018, 5.291415217122922066, -3.054999999999995275 ) ) ;
#128562 = CARTESIAN_POINT ( 'NONE',  ( -21.79333936457831911, 21.75929247661549226, 4.998822639870701856 ) ) ;
#128563 = VERTEX_POINT ( 'NONE', #116441 ) ;
#128564 = DIRECTION ( 'NONE',  ( -0.7071067811865487940, 0.7071067811865463515, -0.000000000000000000 ) ) ;
#128565 = EDGE_LOOP ( 'NONE', ( #57492, #92979, #42049, #61080 ) ) ;
#128566 = ORIENTED_EDGE ( 'NONE', *, *, #88573, .T. ) ;
#128567 = DIRECTION ( 'NONE',  ( -0.000000000000000000, -0.3543493200069152693, 0.9351131265310292928 ) ) ;
#128568 = DIRECTION ( 'NONE',  ( 0.000000000000000000, 0.000000000000000000, -1.000000000000000000 ) ) ;
#128569 = LINE ( 'NONE', #27104, #58159 ) ;
#128570 = EDGE_CURVE ( 'NONE', #9436, #34226, #128737, .T. ) ;
#128571 = DIRECTION ( 'NONE',  ( 0.7071067811865487940, -0.7071067811865463515, 0.000000000000000000 ) ) ;
#128572 = CARTESIAN_POINT ( 'NONE',  ( 83.10416666666667140, 2.130196079827498146, 7.949999999999958433 ) ) ;
#128573 = CARTESIAN_POINT ( 'NONE',  ( 127.1670968585647756, -3.055000000000000160, -5.291415217122921177 ) ) ;
#128574 = EDGE_CURVE ( 'NONE', #25072, #44387, #140191, .T. ) ;
#128575 = EDGE_CURVE ( 'NONE', #1453, #98880, #28006, .T. ) ;
#128576 = VERTEX_POINT ( 'NONE', #72976 ) ;
#128577 = CARTESIAN_POINT ( 'NONE',  ( -32.99999999999975842, -16.06887692260765377, 4.000000000000000000 ) ) ;
#128578 = FACE_OUTER_BOUND ( 'NONE', #49676, .T. ) ;
#128579 = FACE_OUTER_BOUND ( 'NONE', #122569, .T. ) ;
#128580 = DIRECTION ( 'NONE',  ( 0.000000000000000000, 0.000000000000000000, -1.000000000000000000 ) ) ;
#128581 = DIRECTION ( 'NONE',  ( 0.7071067811865486830, -0.7071067811865464625, -0.000000000000000000 ) ) ;
#128582 = CARTESIAN_POINT ( 'NONE',  ( 45.29974487139158867, -27.71228299555237840, 4.000000000000000000 ) ) ;
#128583 = EDGE_CURVE ( 'NONE', #50248, #135356, #17126, .T. ) ;
#128585 = EDGE_CURVE ( 'NONE', #99872, #105758, #95392, .T. ) ;
#128584 = CARTESIAN_POINT ( 'NONE',  ( 64.68336038379622721, -2.130196079827426203, 7.949999999999997513 ) ) ;
#128586 = AXIS2_PLACEMENT_3D ( 'NONE', #3921, #46082, #135917 ) ;
#128587 = FACE_OUTER_BOUND ( 'NONE', #95925, .T. ) ;
#128588 = VERTEX_POINT ( 'NONE', #27267 ) ;
#128589 = ORIENTED_EDGE ( 'NONE', *, *, #133885, .F. ) ;
#128590 = CARTESIAN_POINT ( 'NONE',  ( 55.24999999999999289, -9.735942053221458872E-16, 7.950000000000000178 ) ) ;
#128591 = DIRECTION ( 'NONE',  ( 0.3543493200069162685, -0.000000000000000000, -0.9351131265310288487 ) ) ;
#128592 = AXIS2_PLACEMENT_3D ( 'NONE', #59295, #114346, #103450 ) ;
#128593 = ADVANCED_FACE ( 'NONE', ( #40335 ), #137488, .F. ) ;
#128594 = DIRECTION ( 'NONE',  ( -0.7071067811865486830, -0.7071067811865464625, -0.000000000000000000 ) ) ;
#128595 = DIRECTION ( 'NONE',  ( -0.6830127018922181881, 0.6830127018922202975, -0.2588190451025214056 ) ) ;
#128596 = VERTEX_POINT ( 'NONE', #105540 ) ;
#128597 = CARTESIAN_POINT ( 'NONE',  ( 0.000000000000000000, 0.000000000000000000, 5.000000000000000000 ) ) ;
#128598 = ADVANCED_FACE ( 'NONE', ( #6199 ), #50476, .F. ) ;
#128599 = PRESENTATION_LAYER_ASSIGNMENT (  '', '', ( #107469 ) ) ;
#128600 = CARTESIAN_POINT ( 'NONE',  ( 61.25043019189810423, 3.055000000000002824, -5.291415217122919401 ) ) ;
#128601 = ORIENTED_EDGE ( 'NONE', *, *, #37309, .F. ) ;
#128602 = FACE_OUTER_BOUND ( 'NONE', #48095, .T. ) ;
#128603 = EDGE_LOOP ( 'NONE', ( #140916, #49056, #14539, #10396, #123683, #130753 ) ) ;
#128604 = ORIENTED_EDGE ( 'NONE', *, *, #116290, .T. ) ;
#128605 = FACE_OUTER_BOUND ( 'NONE', #46671, .T. ) ;
#128606 = EDGE_CURVE ( 'NONE', #71584, #116900, #142489, .T. ) ;
#128607 = FILL_AREA_STYLE ('',( #71378 ) ) ;
#128608 = PLANE ( 'NONE',  #76780 ) ;
#128609 = DIRECTION ( 'NONE',  ( 0.7071067811865487940, -0.7071067811865463515, 0.000000000000000000 ) ) ;
#128610 = DIRECTION ( 'NONE',  ( 0.000000000000000000, -1.000000000000000000, 0.000000000000000000 ) ) ;
#128612 = VERTEX_POINT ( 'NONE', #44638 ) ;
#128611 = CARTESIAN_POINT ( 'NONE',  ( -2.816011393730999401, 28.73617430169785436, 5.000000000000000000 ) ) ;
#128613 = DIRECTION ( 'NONE',  ( -0.000000000000000000, 0.3543493200069153248, 0.9351131265310292928 ) ) ;
#128614 = CARTESIAN_POINT ( 'NONE',  ( 59.99451991528749772, 28.92564299267980132, 4.000000000000000000 ) ) ;
#128615 = DIRECTION ( 'NONE',  ( -0.7071067811865486830, -0.7071067811865464625, -0.000000000000000000 ) ) ;
#128616 = ADVANCED_FACE ( 'NONE', ( #53310 ), #341, .F. ) ;
#128617 = LINE ( 'NONE', #62655, #57941 ) ;
#128618 = DIRECTION ( 'NONE',  ( 0.7071067811865486830, -0.7071067811865464625, -0.000000000000000000 ) ) ;
#128619 = VECTOR ( 'NONE', #105054, 1000.000000000000000 ) ;
#128620 = EDGE_LOOP ( 'NONE', ( #93263, #13756, #44605, #22358 ) ) ;
#128621 = AXIS2_PLACEMENT_3D ( 'NONE', #34829, #23948, #68894 ) ;
#128622 = ORIENTED_EDGE ( 'NONE', *, *, #43553, .F. ) ;
#128623 = AXIS2_PLACEMENT_3D ( 'NONE', #116554, #51311, #61501 ) ;
#128624 = DIRECTION ( 'NONE',  ( 1.000000000000000000, 0.000000000000000000, 0.000000000000000000 ) ) ;
#128625 = CARTESIAN_POINT ( 'NONE',  ( 72.39126352523145158, -4.472830434245839371, -4.472830434245839371 ) ) ;
#128626 = LINE ( 'NONE', #40904, #99693 ) ;
#128627 = EDGE_CURVE ( 'NONE', #108744, #101850, #88828, .T. ) ;
#128628 = CARTESIAN_POINT ( 'NONE',  ( 29.28769006033951783, -21.73547319004780931, 4.999917730833664642 ) ) ;
#128629 = PLANE ( 'NONE',  #89480 ) ;
#128630 = ORIENTED_EDGE ( 'NONE', *, *, #18015, .T. ) ;
#128631 = VERTEX_POINT ( 'NONE', #54077 ) ;
#128632 = STYLED_ITEM ( 'NONE', ( #96773 ), #133701 ) ;
#128633 = DIRECTION ( 'NONE',  ( 0.000000000000000000, 0.000000000000000000, 1.000000000000000000 ) ) ;
#128634 = ORIENTED_EDGE ( 'NONE', *, *, #141537, .T. ) ;
#128635 = ADVANCED_FACE ( 'NONE', ( #130910 ), #79056, .T. ) ;
#128636 = ORIENTED_EDGE ( 'NONE', *, *, #99577, .F. ) ;
#128637 = FACE_OUTER_BOUND ( 'NONE', #73292, .T. ) ;
#128639 = EDGE_CURVE ( 'NONE', #7557, #80484, #118568, .T. ) ;
#128638 = ORIENTED_EDGE ( 'NONE', *, *, #26455, .T. ) ;
#128640 = CARTESIAN_POINT ( 'NONE',  ( -33.18398860626899705, 28.73617430169810305, 5.000000000000000000 ) ) ;
#128641 = EDGE_CURVE ( 'NONE', #126683, #3334, #19268, .T. ) ;
#128642 = FACE_BOUND ( 'NONE', #133323, .T. ) ;
#128643 = DIRECTION ( 'NONE',  ( 0.000000000000000000, 0.000000000000000000, -1.000000000000000000 ) ) ;
#128644 = PLANE ( 'NONE',  #58263 ) ;
#128645 = DIRECTION ( 'NONE',  ( 0.7071067811865486830, -0.7071067811865464625, -0.000000000000000000 ) ) ;
#128647 = ORIENTED_EDGE ( 'NONE', *, *, #140104, .F. ) ;
#128646 = CARTESIAN_POINT ( 'NONE',  ( -11.29289321881337571, -9.740707523384186217, 5.000000000000000000 ) ) ;
#128648 = CARTESIAN_POINT ( 'NONE',  ( 0.000000000000000000, 22.27000000000000668, -40.00000000000000000 ) ) ;
#128649 = APPLICATION_PROTOCOL_DEFINITION ( 'draft international standard', 'automotive_design', 1998, #35596 ) ;
#128650 = ORIENTED_EDGE ( 'NONE', *, *, #19793, .T. ) ;
#128651 = VERTEX_POINT ( 'NONE', #97529 ) ;
#128652 = CARTESIAN_POINT ( 'NONE',  ( 82.89126352523143737, -4.472830434245838482, -4.472830434245838482 ) ) ;
#128653 = ORIENTED_EDGE ( 'NONE', *, *, #95673, .T. ) ;
#128654 = CARTESIAN_POINT ( 'NONE',  ( 8.816011393731004731, 28.73617430169781173, 5.000000000000000000 ) ) ;
#128655 = EDGE_CURVE ( 'NONE', #75592, #38197, #43177, .T. ) ;
#128656 = DIRECTION ( 'NONE',  ( -0.3543493200069163240, 0.000000000000000000, -0.9351131265310288487 ) ) ;
#128657 = DIRECTION ( 'NONE',  ( -0.7071067811865486830, -0.7071067811865464625, 0.000000000000000000 ) ) ;
#128658 = CARTESIAN_POINT ( 'NONE',  ( 24.98480450340313652, 2.536990198832462351, 5.000000000000000000 ) ) ;
#128659 = CARTESIAN_POINT ( 'NONE',  ( 6.328169399223492420, 5.259292476615662792, 4.000000000000000000 ) ) ;
#128660 = ORIENTED_EDGE ( 'NONE', *, *, #27023, .T. ) ;
#128661 = CARTESIAN_POINT ( 'NONE',  ( 22.07159235450331991, -3.851859888774471706E-31, 2.500000000000001332 ) ) ;
#128662 = EDGE_CURVE ( 'NONE', #29861, #72725, #120702, .T. ) ;
#128663 = CARTESIAN_POINT ( 'NONE',  ( -63.48921356237309510, -27.52281430457099631, 5.000000000000000000 ) ) ;
#128664 = FACE_OUTER_BOUND ( 'NONE', #131488, .T. ) ;
#128665 = DIRECTION ( 'NONE',  ( 0.6830127018922180770, -0.6830127018922204085, -0.2588190451025213501 ) ) ;
#128666 = CARTESIAN_POINT ( 'NONE',  ( 14.67183060077637080, -15.74070752338412049, 4.000000000000000000 ) ) ;
#128667 = CARTESIAN_POINT ( 'NONE',  ( -45.48921356237309510, -27.52281430457087197, 5.000000000000000000 ) ) ;
#128668 = CARTESIAN_POINT ( 'NONE',  ( -32.19990655525713663, -22.22500000000000142, 3.967360224444566708 ) ) ;
#128669 = ORIENTED_EDGE ( 'NONE', *, *, #54619, .T. ) ;
#128670 = CARTESIAN_POINT ( 'NONE',  ( 9.328169399223467551, 2.259292476615690770, 4.000000000000000000 ) ) ;
#128671 = CARTESIAN_POINT ( 'NONE',  ( 34.92499999999998295, 22.22500000000000142, 4.000000000000000000 ) ) ;
#128672 = EDGE_LOOP ( 'NONE', ( #46499, #54816, #141701, #15266 ) ) ;
#128673 = ADVANCED_FACE ( 'NONE', ( #21416 ), #96778, .F. ) ;
#128674 = ORIENTED_EDGE ( 'NONE', *, *, #142582, .F. ) ;
#128675 = ORIENTED_EDGE ( 'NONE', *, *, #25315, .F. ) ;
#128676 = ADVANCED_FACE ( 'NONE', ( #107689 ), #19964, .F. ) ;
#128677 = CARTESIAN_POINT ( 'NONE',  ( 35.00043019189810423, -3.055000000000002380, 5.291415217122920289 ) ) ;
#128678 = ORIENTED_EDGE ( 'NONE', *, *, #75932, .T. ) ;
#128679 = VECTOR ( 'NONE', #137731, 1000.000000000000000 ) ;
#128680 = EDGE_CURVE ( 'NONE', #142920, #77362, #88099, .T. ) ;
#128681 = CARTESIAN_POINT ( 'NONE',  ( 19.14997294953710849, -4.461849672132299105, 4.461849672132299993 ) ) ;
#128682 = PRESENTATION_STYLE_ASSIGNMENT (( #125845 ) ) ;
#128683 = ORIENTED_EDGE ( 'NONE', *, *, #116222, .F. ) ;
#128684 = VECTOR ( 'NONE', #107569, 1000.000000000000000 ) ;
#128685 = LINE ( 'NONE', #61336, #47145 ) ;
#128686 = ORIENTED_EDGE ( 'NONE', *, *, #113138, .T. ) ;
#128687 = DIRECTION ( 'NONE',  ( -0.7071067811865487940, 0.7071067811865463515, -0.000000000000000000 ) ) ;
#128688 = CARTESIAN_POINT ( 'NONE',  ( -15.29974487139158867, -27.71228299555216879, 4.000000000000000000 ) ) ;
#128690 = VERTEX_POINT ( 'NONE', #98949 ) ;
#128689 = DIRECTION ( 'NONE',  ( 4.681814790819592407E-17, 0.3543493200069153248, 0.9351131265310292928 ) ) ;
#128691 = VERTEX_POINT ( 'NONE', #141032 ) ;
#128692 = DIRECTION ( 'NONE',  ( 0.3543493200069163240, 0.000000000000000000, -0.9351131265310288487 ) ) ;
#128693 = ORIENTED_EDGE ( 'NONE', *, *, #28806, .F. ) ;
#128694 = EDGE_CURVE ( 'NONE', #17414, #65959, #109841, .T. ) ;
#128695 = CARTESIAN_POINT ( 'NONE',  ( 8.188407645496676324, 9.139736423841732040E-16, 0.000000000000000000 ) ) ;
#128696 = ORIENTED_EDGE ( 'NONE', *, *, #117351, .T. ) ;
#128697 = VERTEX_POINT ( 'NONE', #22102 ) ;
#128698 = EDGE_LOOP ( 'NONE', ( #116507, #110891, #118074, #65097, #93021 ) ) ;
#128699 = VECTOR ( 'NONE', #121427, 1000.000000000000000 ) ;
#128700 = ORIENTED_EDGE ( 'NONE', *, *, #67653, .T. ) ;
#128701 = CARTESIAN_POINT ( 'NONE',  ( -20.54016161050247646, 18.75929247661552779, 8.305906642995438460 ) ) ;
#128702 = SPHERICAL_SURFACE ( 'NONE', #107071, 0.5000000000000000000 ) ;
#128703 = CARTESIAN_POINT ( 'NONE',  ( -0.7928932188134485415, -14.24070752338414003, 5.000000000000000000 ) ) ;
#128704 = DIRECTION ( 'NONE',  ( -0.000000000000000000, 0.3543493200069153248, 0.9351131265310292928 ) ) ;
#128705 = EDGE_CURVE ( 'NONE', #15253, #50127, #86682, .T. ) ;
#128706 = VERTEX_POINT ( 'NONE', #11201 ) ;
#128707 = DIRECTION ( 'NONE',  ( 0.7071067811865487940, -0.7071067811865463515, 0.000000000000000000 ) ) ;
#128708 = ORIENTED_EDGE ( 'NONE', *, *, #138528, .F. ) ;
#128709 = DIRECTION ( 'NONE',  ( -0.6830127018922181881, 0.6830127018922202975, -0.2588190451025214056 ) ) ;
#128710 = VECTOR ( 'NONE', #2518, 999.9999999999998863 ) ;
#128711 = DIRECTION ( 'NONE',  ( 0.6830127018922180770, -0.6830127018922204085, -0.2588190451025213501 ) ) ;
#128712 = CARTESIAN_POINT ( 'NONE',  ( 24.79289321881327623, 18.75929247661552779, 5.000000000000000000 ) ) ;
#128713 = VECTOR ( 'NONE', #104704, 999.9999999999998863 ) ;
#128714 = ORIENTED_EDGE ( 'NONE', *, *, #140704, .T. ) ;
#128715 = CARTESIAN_POINT ( 'NONE',  ( 96.95833333333334281, 3.974999999999997424, 6.884901960086288852 ) ) ;
#128716 = FILL_AREA_STYLE_COLOUR ( '', #14205 ) ;
#128717 = ORIENTED_EDGE ( 'NONE', *, *, #115524, .F. ) ;
#128718 = AXIS2_PLACEMENT_3D ( 'NONE', #76921, #21064, #30543 ) ;
#128719 = ORIENTED_EDGE ( 'NONE', *, *, #32490, .F. ) ;
#128720 = EDGE_LOOP ( 'NONE', ( #97031, #6147, #29056, #2016 ) ) ;
#128721 = FACE_OUTER_BOUND ( 'NONE', #141629, .T. ) ;
#128722 = DIRECTION ( 'NONE',  ( -1.000000000000000000, 0.000000000000000000, 0.000000000000000000 ) ) ;
#128723 = CARTESIAN_POINT ( 'NONE',  ( -17.18650864602350126, -15.74070752338412404, 8.904080028138981362 ) ) ;
#128724 = VECTOR ( 'NONE', #11196, 1000.000000000000000 ) ;
#128725 = CARTESIAN_POINT ( 'NONE',  ( 3.250000000000000000, 0.000000000000000000, 9.119999999999999218 ) ) ;
#128726 = CARTESIAN_POINT ( 'NONE',  ( 21.70701326429288613, -21.74070752338406365, 4.999753212805217117 ) ) ;
#128727 = CARTESIAN_POINT ( 'NONE',  ( 74.72459685856476597, -1.637169565754161171, 6.109999999999998543 ) ) ;
#128728 = FACE_OUTER_BOUND ( 'NONE', #35849, .T. ) ;
#128729 = LINE ( 'NONE', #140322, #106336 ) ;
#128730 = DIRECTION ( 'NONE',  ( 0.7071067811865487940, -0.7071067811865463515, 0.000000000000000000 ) ) ;
#128731 = CARTESIAN_POINT ( 'NONE',  ( 6.489213562373093325, -27.52281430457059841, 5.000000000000000000 ) ) ;
#128732 = CARTESIAN_POINT ( 'NONE',  ( 34.42499999999998295, 21.72500000000000142, 0.5000000000000000000 ) ) ;
#128733 = ORIENTED_EDGE ( 'NONE', *, *, #126945, .F. ) ;
#128734 = FACE_OUTER_BOUND ( 'NONE', #91731, .T. ) ;
#128735 = ORIENTED_EDGE ( 'NONE', *, *, #91204, .F. ) ;
#128736 = LINE ( 'NONE', #75106, #32294 ) ;
#128738 = VERTEX_POINT ( 'NONE', #64209 ) ;
#128737 = LINE ( 'NONE', #38879, #46469 ) ;
#128739 = LINE ( 'NONE', #27270, #44022 ) ;
#128740 = PLANE ( 'NONE',  #93550 ) ;
#128741 = ADVANCED_FACE ( 'NONE', ( #20681 ), #64927, .F. ) ;
#128742 = EDGE_LOOP ( 'NONE', ( #89097, #113802, #105257, #80624 ) ) ;
#128743 = ORIENTED_EDGE ( 'NONE', *, *, #53272, .F. ) ;
#128744 = LINE ( 'NONE', #96790, #132453 ) ;
#128745 = DIRECTION ( 'NONE',  ( -0.7071067811865487940, 0.7071067811865463515, 0.000000000000000000 ) ) ;
#128746 = EDGE_CURVE ( 'NONE', #58008, #61053, #131606, .T. ) ;
#128748 = ADVANCED_FACE ( 'NONE', ( #12655 ), #59078, .F. ) ;
#128747 = CARTESIAN_POINT ( 'NONE',  ( 98.51669371712955581, 7.950000000000001066, -2.130196079827421318 ) ) ;
#128749 = CARTESIAN_POINT ( 'NONE',  ( 75.48921356237309510, -27.52281430457107803, 5.000000000000000000 ) ) ;
#128750 = PLANE ( 'NONE',  #52947 ) ;
#128752 = EDGE_CURVE ( 'NONE', #23590, #5533, #46042, .T. ) ;
#128751 = ORIENTED_EDGE ( 'NONE', *, *, #86039, .T. ) ;
#128753 = CARTESIAN_POINT ( 'NONE',  ( 38.99451991528749062, 28.92564299267965211, 4.000000000000000000 ) ) ;
#128754 = EDGE_CURVE ( 'NONE', #108299, #114924, #112003, .T. ) ;
#128755 = CARTESIAN_POINT ( 'NONE',  ( 34.49999999999975842, 5.696342897626535340, -7.587980461218318595 ) ) ;
#128756 = CARTESIAN_POINT ( 'NONE',  ( 33.25000000000000000, -7.464222240803106570E-16, -6.094999999999989981 ) ) ;
#128757 = AXIS2_PLACEMENT_3D ( 'NONE', #104123, #6226, #113596 ) ;
#128758 = FACE_OUTER_BOUND ( 'NONE', #140737, .T. ) ;
#128759 = EDGE_CURVE ( 'NONE', #42096, #95953, #90225, .T. ) ;
#128760 = VERTEX_POINT ( 'NONE', #34426 ) ;
#128761 = CARTESIAN_POINT ( 'NONE',  ( 32.99999999999976552, 13.93112307739204248, 4.000000000000000000 ) ) ;
#128763 = VERTEX_POINT ( 'NONE', #124286 ) ;
#128762 = EDGE_CURVE ( 'NONE', #35471, #39260, #1051, .T. ) ;
#128764 = CARTESIAN_POINT ( 'NONE',  ( 87.35459685856476142, -1.637169565754161615, 6.110000000000000320 ) ) ;
#128765 = DIRECTION ( 'NONE',  ( -0.3543493200069162685, -0.000000000000000000, -0.9351131265310288487 ) ) ;
#128766 = VECTOR ( 'NONE', #19960, 1000.000000000000227 ) ;
#128767 = DIRECTION ( 'NONE',  ( -0.000000000000000000, -0.3543493200069152693, 0.9351131265310292928 ) ) ;
#128768 = ORIENTED_EDGE ( 'NONE', *, *, #33729, .T. ) ;
#128769 = CARTESIAN_POINT ( 'NONE',  ( -31.92499999999997584, -6.270000000000012008, -37.00000000000000000 ) ) ;
#128770 =( BOUNDED_CURVE ( )  B_SPLINE_CURVE ( 3, ( #74942, #39452, #63363, #95226 ),
 .UNSPECIFIED., .F., .T. ) 
 B_SPLINE_CURVE_WITH_KNOTS ( ( 4, 4 ),
 ( 2.001653308786169205, 3.503810798801451742 ),
 .UNSPECIFIED. ) 
 CURVE ( )  GEOMETRIC_REPRESENTATION_ITEM ( )  RATIONAL_B_SPLINE_CURVE ( ( 1.000000000000000000, 0.8206354192515237234, 0.8206354192515237234, 1.000000000000000000 ) ) 
 REPRESENTATION_ITEM ( '' )  );
#128771 = ADVANCED_FACE ( 'NONE', ( #3884 ), #123610, .F. ) ;
#128772 = LINE ( 'NONE', #85254, #9447 ) ;
#128773 = PLANE ( 'NONE',  #41574 ) ;
#128775 = ORIENTED_EDGE ( 'NONE', *, *, #134738, .F. ) ;
#128774 = LINE ( 'NONE', #141068, #112439 ) ;
#128776 = CARTESIAN_POINT ( 'NONE',  ( 13.41666666666666785, 5.278424836066147208, 3.047499999999990550 ) ) ;
#128777 = CARTESIAN_POINT ( 'NONE',  ( 47.99451991528749062, 28.92564299267971251, 4.000000000000000000 ) ) ;
#128778 = CARTESIAN_POINT ( 'NONE',  ( 2.000000000000256239, -6.019044215166783118, 0.9592349742722835471 ) ) ;
#128779 = ADVANCED_FACE ( 'NONE', ( #91657 ), #33740, .F. ) ;
#128780 = VERTEX_POINT ( 'NONE', #3205 ) ;
#128781 = AXIS2_PLACEMENT_3D ( 'NONE', #118486, #85863, #54687 ) ;
#128782 = ORIENTED_EDGE ( 'NONE', *, *, #119815, .F. ) ;
#128783 = CARTESIAN_POINT ( 'NONE',  ( 74.22959685856476142, -6.110000000000000320, -1.637169565754161393 ) ) ;
#128784 = ORIENTED_EDGE ( 'NONE', *, *, #34344, .F. ) ;
#128785 = CIRCLE ( 'NONE', #61655, 2.055000000000001048 ) ;
#128786 = CARTESIAN_POINT ( 'NONE',  ( -4.828169399223503078, 18.75929247661552424, 4.000000000000000000 ) ) ;
#128787 = FACE_OUTER_BOUND ( 'NONE', #52901, .T. ) ;
#128788 = FACE_OUTER_BOUND ( 'NONE', #46489, .T. ) ;
#128789 = ORIENTED_EDGE ( 'NONE', *, *, #51509, .T. ) ;
#128790 = LINE ( 'NONE', #49840, #58427 ) ;
#128791 = DIRECTION ( 'NONE',  ( -1.000000000000000000, 0.000000000000000000, -0.000000000000000000 ) ) ;
#128792 = EDGE_LOOP ( 'NONE', ( #72689, #37771, #48351, #139623 ) ) ;
#128793 = VECTOR ( 'NONE', #20044, 1000.000000000000114 ) ;
#128794 = DIRECTION ( 'NONE',  ( -0.000000000000000000, 0.000000000000000000, 1.000000000000000000 ) ) ;
#128795 = ADVANCED_FACE ( 'NONE', ( #101097 ), #114122, .F. ) ;
#128796 = DIRECTION ( 'NONE',  ( 0.7071067811865486830, -0.7071067811865464625, -0.000000000000000000 ) ) ;
#128797 = CARTESIAN_POINT ( 'NONE',  ( -57.48921356237308800, -27.52281430457095368, 5.000000000000000000 ) ) ;
#128798 = EDGE_CURVE ( 'NONE', #92118, #92154, #100408, .T. ) ;
#128799 = ORIENTED_EDGE ( 'NONE', *, *, #29895, .T. ) ;
#128800 = EDGE_LOOP ( 'NONE', ( #90919, #33071, #42411, #108640 ) ) ;
#128801 = VECTOR ( 'NONE', #133274, 1000.000000000000000 ) ;
#128802 = CARTESIAN_POINT ( 'NONE',  ( 180.4193221990230143, -49.14999999999999147, 40.92499999999998295 ) ) ;
#128803 = CARTESIAN_POINT ( 'NONE',  ( 6.183988606268994381, 28.73617430169791476, 5.000000000000000000 ) ) ;
#128804 = LINE ( 'NONE', #62870, #122990 ) ;
#128805 = FACE_OUTER_BOUND ( 'NONE', #15015, .T. ) ;
#128806 = DIRECTION ( 'NONE',  ( 0.7071067811865487940, 0.7071067811865463515, 0.000000000000000000 ) ) ;
#128807 = EDGE_CURVE ( 'NONE', #56699, #139467, #68511, .T. ) ;
#128808 = VECTOR ( 'NONE', #91695, 1000.000000000000000 ) ;
#128809 = VECTOR ( 'NONE', #61964, 999.9999999999998863 ) ;
#128810 = CARTESIAN_POINT ( 'NONE',  ( -17.99999999999986500, -3.412538124160723108, 4.000000000000000000 ) ) ;
#128811 = VERTEX_POINT ( 'NONE', #90970 ) ;
#128812 = VECTOR ( 'NONE', #82625, 1000.000000000000000 ) ;
#128813 = VERTEX_POINT ( 'NONE', #46788 ) ;
#128814 = VERTEX_POINT ( 'NONE', #112692 ) ;
#128815 = EDGE_CURVE ( 'NONE', #47195, #23039, #80104, .T. ) ;
#128816 = ORIENTED_EDGE ( 'NONE', *, *, #132510, .F. ) ;
#128817 = VECTOR ( 'NONE', #86148, 1000.000000000000000 ) ;
#128818 = CARTESIAN_POINT ( 'NONE',  ( 180.8518557880187529, -48.98056306480232536, 39.49745726092412212 ) ) ;
#128819 = CARTESIAN_POINT ( 'NONE',  ( -31.49999999999978684, 1.030536316426473809, -5.498701923753729126 ) ) ;
#128820 = CARTESIAN_POINT ( 'NONE',  ( 23.99999999999983302, -6.108550654416937675, -3.114665004254912439 ) ) ;
#128821 = ORIENTED_EDGE ( 'NONE', *, *, #6380, .T. ) ;
#128822 = DIRECTION ( 'NONE',  ( -0.7071067811865486830, -0.7071067811865464625, -0.000000000000000000 ) ) ;
#128823 = LINE ( 'NONE', #85302, #21773 ) ;
#128824 = CARTESIAN_POINT ( 'NONE',  ( 34.92499999999998295, -7.298069433178939747, 4.500000000000000888 ) ) ;
#128825 = LINE ( 'NONE', #29502, #16063 ) ;
#128826 = CARTESIAN_POINT ( 'NONE',  ( 27.00000000000001066, -6.477409876647271858, -3.272594246810044627 ) ) ;
#128827 = ORIENTED_EDGE ( 'NONE', *, *, #71929, .T. ) ;
#128828 = CARTESIAN_POINT ( 'NONE',  ( 33.78162688292471216, 21.74787736706807095, 4.999607392498048419 ) ) ;
#128829 = DIRECTION ( 'NONE',  ( -0.7071067811865486830, -0.7071067811865464625, 0.000000000000000000 ) ) ;
#128830 = ORIENTED_EDGE ( 'NONE', *, *, #126753, .F. ) ;
#128832 = EDGE_CURVE ( 'NONE', #23962, #85630, #55862, .T. ) ;
#128831 = CARTESIAN_POINT ( 'NONE',  ( 15.83159235450332147, 9.902892378096218942E-16, 0.000000000000000000 ) ) ;
#128833 = ORIENTED_EDGE ( 'NONE', *, *, #51044, .T. ) ;
#128834 = ADVANCED_FACE ( 'NONE', ( #13358 ), #57631, .F. ) ;
#128835 = DIRECTION ( 'NONE',  ( -0.000000000000000000, -0.000000000000000000, 1.000000000000000000 ) ) ;
#128836 = VERTEX_POINT ( 'NONE', #14078 ) ;
#128837 = EDGE_CURVE ( 'NONE', #1472, #102338, #25678, .T. ) ;
#128838 = CARTESIAN_POINT ( 'NONE',  ( 71.89626352523143282, 4.472830434245840259, -4.472830434245838482 ) ) ;
#128839 = ORIENTED_EDGE ( 'NONE', *, *, #94425, .T. ) ;
#128840 = ORIENTED_EDGE ( 'NONE', *, *, #73956, .T. ) ;
#128841 = DIRECTION ( 'NONE',  ( -0.5735764363510507113, 0.8191520442889885789, 1.003171929053520926E-16 ) ) ;
#128842 = ADVANCED_FACE ( 'NONE', ( #102557 ), #135878, .F. ) ;
#128843 = DIRECTION ( 'NONE',  ( 1.000000000000000000, 0.000000000000000000, 0.000000000000000000 ) ) ;
#128844 = CARTESIAN_POINT ( 'NONE',  ( 108.6462635252314186, -4.472830434245840259, 4.472830434245838482 ) ) ;
#128845 = CARTESIAN_POINT ( 'NONE',  ( -10.82816939922345867, 9.759292476615614831, 4.000000000000000000 ) ) ;
#128846 = PLANE ( 'NONE',  #25886 ) ;
#128847 = LINE ( 'NONE', #18634, #71915 ) ;
#128848 = FACE_OUTER_BOUND ( 'NONE', #49169, .T. ) ;
#128849 = VECTOR ( 'NONE', #29112, 1000.000000000000000 ) ;
#128850 = CARTESIAN_POINT ( 'NONE',  ( -12.69999999999998153, 3.061616997868383634E-16, -2.500000000000000444 ) ) ;
#128851 = CARTESIAN_POINT ( 'NONE',  ( 91.85416666666667140, -2.130196079827425759, -7.950000000000000178 ) ) ;
#128852 = DIRECTION ( 'NONE',  ( -0.7071067811865486830, 0.7071067811865464625, 0.000000000000000000 ) ) ;
#128853 = EDGE_LOOP ( 'NONE', ( #17702, #117486, #105067, #128244, #38391 ) ) ;
#128854 = EDGE_CURVE ( 'NONE', #23121, #95547, #18337, .T. ) ;
#128855 = CARTESIAN_POINT ( 'NONE',  ( -6.328169399223490643, 20.25929247661551003, 4.000000000000000000 ) ) ;
#128856 = DIRECTION ( 'NONE',  ( -0.6830127018922180770, -0.6830127018922204085, -0.2588190451025213501 ) ) ;
#128857 = ORIENTED_EDGE ( 'NONE', *, *, #75588, .T. ) ;
#128858 = ORIENTED_EDGE ( 'NONE', *, *, #85776, .T. ) ;
#128859 = ORIENTED_EDGE ( 'NONE', *, *, #95489, .F. ) ;
#128860 = ORIENTED_EDGE ( 'NONE', *, *, #35527, .T. ) ;
#128861 = CARTESIAN_POINT ( 'NONE',  ( -29.56319896779151790, -12.74070752338415247, 9.898150129686444032 ) ) ;
#128862 = FACE_OUTER_BOUND ( 'NONE', #42555, .T. ) ;
#128863 = VECTOR ( 'NONE', #113839, 1000.000000000000000 ) ;
#128864 = LINE ( 'NONE', #85350, #111162 ) ;
#128865 = EDGE_CURVE ( 'NONE', #28348, #29516, #114804, .T. ) ;
#128866 = CARTESIAN_POINT ( 'NONE',  ( 5.671830600776431197, -6.740707523384218192, 4.000000000000000000 ) ) ;
#128867 = ORIENTED_EDGE ( 'NONE', *, *, #129668, .F. ) ;
#128868 = CARTESIAN_POINT ( 'NONE',  ( 0.3252437201521669041, -48.93522302958528769, 39.28544916627436123 ) ) ;
#128869 = VERTEX_POINT ( 'NONE', #136574 ) ;
#128870 = VECTOR ( 'NONE', #95133, 1000.000000000000000 ) ;
#128871 = CARTESIAN_POINT ( 'NONE',  ( 2.020403141435219485, 7.934999999999989839, -2.126176841940961904 ) ) ;
#128872 = CARTESIAN_POINT ( 'NONE',  ( -24.29974487139158867, -27.71228299555223273, 4.000000000000000000 ) ) ;
#128873 = DIRECTION ( 'NONE',  ( 0.000000000000000000, -1.000000000000000000, 0.000000000000000000 ) ) ;
#128874 = AXIS2_PLACEMENT_3D ( 'NONE', #64100, #21311, #130811 ) ;
#128875 = LINE ( 'NONE', #75248, #141620 ) ;
#128876 = ORIENTED_EDGE ( 'NONE', *, *, #68839, .T. ) ;
#128877 = VERTEX_POINT ( 'NONE', #39441 ) ;
#128878 = EDGE_LOOP ( 'NONE', ( #128084, #31132, #6005, #122038, #54929, #59509 ) ) ;
#128879 = CARTESIAN_POINT ( 'NONE',  ( 2.999999999999975131, 20.58746187583904330, 4.000000000000000000 ) ) ;
#128880 = PLANE ( 'NONE',  #2400 ) ;
#128881 = LINE ( 'NONE', #95535, #77527 ) ;
#128882 = CARTESIAN_POINT ( 'NONE',  ( -11.99999999999991651, 13.55218569542903317, 5.000000000000000000 ) ) ;
#128883 = CARTESIAN_POINT ( 'NONE',  ( 8.188407645496676324, 9.139736423841732040E-16, 0.000000000000000000 ) ) ;
#128884 = LINE ( 'NONE', #141943, #96624 ) ;
#128885 = CARTESIAN_POINT ( 'NONE',  ( 57.18398860626899705, 28.73617430169827358, 5.000000000000000000 ) ) ;
#128886 = DIRECTION ( 'NONE',  ( 0.000000000000000000, -1.000000000000000000, 0.000000000000000000 ) ) ;
#128887 = CARTESIAN_POINT ( 'NONE',  ( 33.83376352523143282, 6.110000000000001208, 1.122388791418549305E-15 ) ) ;
#128888 = DIRECTION ( 'NONE',  ( 0.6830127018922181881, 0.6830127018922202975, -0.2588190451025214056 ) ) ;
#128889 = LINE ( 'NONE', #39779, #51254 ) ;
#128890 = EDGE_LOOP ( 'NONE', ( #37745, #111885, #16351, #29463 ) ) ;
#128891 = CARTESIAN_POINT ( 'NONE',  ( 15.18398860626900237, 28.73617430169797871, 5.000000000000000000 ) ) ;
#128892 = CARTESIAN_POINT ( 'NONE',  ( -30.79289321881324781, -5.240707523384225297, 5.000000000000000000 ) ) ;
#128893 = VERTEX_POINT ( 'NONE', #51741 ) ;
#128894 = CARTESIAN_POINT ( 'NONE',  ( 23.01088028653932582, -22.02621442084247860, 4.990779571109218438 ) ) ;
#128896 = ORIENTED_EDGE ( 'NONE', *, *, #110621, .F. ) ;
#128895 = DIRECTION ( 'NONE',  ( 0.3543493200069162685, -0.000000000000000000, -0.9351131265310288487 ) ) ;
#128897 = PRESENTATION_LAYER_ASSIGNMENT (  '', '', ( #112663 ) ) ;
#128898 = LINE ( 'NONE', #29581, #12130 ) ;
#128899 = LINE ( 'NONE', #29582, #90107 ) ;
#128900 = ORIENTED_EDGE ( 'NONE', *, *, #93888, .T. ) ;
#128901 = CARTESIAN_POINT ( 'NONE',  ( -54.48921356237310221, -27.52281430457093236, 5.000000000000000000 ) ) ;
#128902 = UNCERTAINTY_MEASURE_WITH_UNIT (LENGTH_MEASURE( 1.000000000000000082E-05 ), #122294, 'distance_accuracy_value', 'NONE');
#128903 = VERTEX_POINT ( 'NONE', #95215 ) ;
#128904 = VECTOR ( 'NONE', #107043, 1000.000000000000000 ) ;
#128906 = VECTOR ( 'NONE', #53905, 999.9999999999998863 ) ;
#128905 = VECTOR ( 'NONE', #105091, 1000.000000000000000 ) ;
#128907 = CARTESIAN_POINT ( 'NONE',  ( 13.92145407031093818, 2.500000000000000444, 0.000000000000000000 ) ) ;
#128910 = EDGE_CURVE ( 'NONE', #80757, #90561, #16199, .T. ) ;
#128909 = CARTESIAN_POINT ( 'NONE',  ( 121.4125270504628986, -7.949999999999998401, -4.867971026610728450E-16 ) ) ;
#128908 =( GEOMETRIC_REPRESENTATION_CONTEXT ( 3 ) GLOBAL_UNCERTAINTY_ASSIGNED_CONTEXT ( ( #115512 ) ) GLOBAL_UNIT_ASSIGNED_CONTEXT ( ( #87579, #21612, #11399 ) ) REPRESENTATION_CONTEXT ( 'NONE', 'WORKASPACE' ) );
#128911 = PLANE ( 'NONE',  #110971 ) ;
#128912 = DIRECTION ( 'NONE',  ( 0.000000000000000000, 1.000000000000000000, 0.000000000000000000 ) ) ;
#128913 = EDGE_CURVE ( 'NONE', #110130, #11132, #90505, .T. ) ;
#128914 = EDGE_CURVE ( 'NONE', #88713, #89781, #106796, .T. ) ;
#128915 = CARTESIAN_POINT ( 'NONE',  ( 26.99999999999981526, -15.41253812416059432, 4.000000000000000000 ) ) ;
#128916 = CARTESIAN_POINT ( 'NONE',  ( -17.81601139373099940, 28.73617430169775133, 5.000000000000000000 ) ) ;
#128917 = VECTOR ( 'NONE', #88322, 1000.000000000000000 ) ;
#128918 = EDGE_CURVE ( 'NONE', #29177, #6529, #6031, .T. ) ;
#128919 = CARTESIAN_POINT ( 'NONE',  ( 22.53999999999999915, 9.521314400968980422E-16, 0.000000000000000000 ) ) ;
#128920 = CARTESIAN_POINT ( 'NONE',  ( 1.604166666666666297, -1.633150327867691987, -6.094999999999989093 ) ) ;
#128921 = CARTESIAN_POINT ( 'NONE',  ( 9.166236474768552966, 7.934999999999990727, -1.457635852685135314E-15 ) ) ;
#128922 = VECTOR ( 'NONE', #24128, 1000.000000000000000 ) ;
#128923 = DIRECTION ( 'NONE',  ( 0.7071067811865487940, 0.7071067811865463515, -0.000000000000000000 ) ) ;
#128925 = ADVANCED_FACE ( 'NONE', ( #104667 ), #73487, .F. ) ;
#128924 = CARTESIAN_POINT ( 'NONE',  ( -7.140000000000001457, -39.92999999999999261, -12.10072711459627293 ) ) ;
#128926 = ORIENTED_EDGE ( 'NONE', *, *, #75338, .T. ) ;
#128927 = VERTEX_POINT ( 'NONE', #127882 ) ;
#128928 = CARTESIAN_POINT ( 'NONE',  ( 86.31249999999997158, 5.819803920172571310, 5.819803920172575751 ) ) ;
#128929 = DIRECTION ( 'NONE',  ( 1.000000000000000000, 0.000000000000000000, 0.000000000000000000 ) ) ;
#128930 = VERTEX_POINT ( 'NONE', #50307 ) ;
#128931 = EDGE_CURVE ( 'NONE', #125049, #122112, #103928, .T. ) ;
#128932 = FACE_OUTER_BOUND ( 'NONE', #101413, .T. ) ;
#128933 = CARTESIAN_POINT ( 'NONE',  ( 22.49999999999984013, -2.568876922607788327, 4.000000000000000000 ) ) ;
#128934 = FACE_OUTER_BOUND ( 'NONE', #48615, .T. ) ;
#128935 = CARTESIAN_POINT ( 'NONE',  ( 0.000000000000000000, 0.000000000000000000, 5.000000000000000000 ) ) ;
#128936 = ORIENTED_EDGE ( 'NONE', *, *, #85761, .T. ) ;
#128937 = CARTESIAN_POINT ( 'NONE',  ( 3.469446951953614189E-15, 20.96639925780204550, 5.000000000000000000 ) ) ;
#128938 = EDGE_CURVE ( 'NONE', #53759, #67529, #29245, .T. ) ;
#128939 = DIRECTION ( 'NONE',  ( -0.000000000000000000, 0.3543493200069153248, 0.9351131265310292928 ) ) ;
#128940 = LINE ( 'NONE', #129644, #199 ) ;
#128941 = EDGE_CURVE ( 'NONE', #82859, #40404, #72817, .T. ) ;
#128942 = DIRECTION ( 'NONE',  ( 0.7071067811865486830, -0.7071067811865464625, -0.000000000000000000 ) ) ;
#128944 = ORIENTED_EDGE ( 'NONE', *, *, #27179, .T. ) ;
#128943 = FACE_OUTER_BOUND ( 'NONE', #104750, .T. ) ;
#128945 = CARTESIAN_POINT ( 'NONE',  ( 41.10416666666666430, 2.130196079827422206, 7.950000000000001954 ) ) ;
#128946 = AXIS2_PLACEMENT_3D ( 'NONE', #36857, #102854, #24557 ) ;
#128947 = DIRECTION ( 'NONE',  ( 0.6830127018922180770, -0.6830127018922204085, -0.2588190451025213501 ) ) ;
#128948 = CARTESIAN_POINT ( 'NONE',  ( 11.14818355038138087, 17.25929247661554911, 8.802941693769225751 ) ) ;
#128949 = DIRECTION ( 'NONE',  ( -0.000000000000000000, 0.3543493200069153248, 0.9351131265310292928 ) ) ;
#128951 = ADVANCED_FACE ( 'NONE', ( #61231 ), #70659, .F. ) ;
#128950 =( BOUNDED_CURVE ( )  B_SPLINE_CURVE ( 3, ( #33775, #80842, #133780, #36589 ),
 .UNSPECIFIED., .F., .T. ) 
 B_SPLINE_CURVE_WITH_KNOTS ( ( 4, 4 ),
 ( -7.105427357601001859E-15, 1.570796326794900111 ),
 .UNSPECIFIED. ) 
 CURVE ( )  GEOMETRIC_REPRESENTATION_ITEM ( )  RATIONAL_B_SPLINE_CURVE ( ( 1.000000000000000000, 0.8047378541243626060, 0.8047378541243626060, 1.000000000000000000 ) ) 
 REPRESENTATION_ITEM ( '' )  );
#128952 = CARTESIAN_POINT ( 'NONE',  ( -10.49999999999992006, 3.052185695429133538, 5.000000000000000000 ) ) ;
#128953 = ORIENTED_EDGE ( 'NONE', *, *, #33167, .T. ) ;
#128954 = ORIENTED_EDGE ( 'NONE', *, *, #45487, .T. ) ;
#128955 = CARTESIAN_POINT ( 'NONE',  ( 103.3962635252314328, 4.472830434245840259, -4.472830434245839371 ) ) ;
#128956 = AXIS2_PLACEMENT_3D ( 'NONE', #66410, #55530, #33788 ) ;
#128957 = VERTEX_POINT ( 'NONE', #59766 ) ;
#128958 = CARTESIAN_POINT ( 'NONE',  ( 128.0580420323229873, -46.73296206246176610, 36.09967824800666136 ) ) ;
#128959 = AXIS2_PLACEMENT_3D ( 'NONE', #25184, #23021, #111488 ) ;
#128960 = CARTESIAN_POINT ( 'NONE',  ( -3.489213562373097322, -27.52281430457057709, 5.000000000000000000 ) ) ;
#128961 = ORIENTED_EDGE ( 'NONE', *, *, #111850, .F. ) ;
#128962 = CARTESIAN_POINT ( 'NONE',  ( 75.22916666666667140, 7.950000000000001954, -2.130196079827421762 ) ) ;
#128963 = CARTESIAN_POINT ( 'NONE',  ( -12.00548008471251293, 28.92564299267929684, 4.000000000000000000 ) ) ;
#128964 = CARTESIAN_POINT ( 'NONE',  ( 96.30793019189810877, -6.109999999999998543, 1.637169565754158063 ) ) ;
#128965 = ORIENTED_EDGE ( 'NONE', *, *, #10092, .T. ) ;
#128966 = DIRECTION ( 'NONE',  ( -1.000000000000000000, -1.224606353822377258E-16, -0.000000000000000000 ) ) ;
#128967 = ORIENTED_EDGE ( 'NONE', *, *, #130066, .T. ) ;
#128969 = EDGE_CURVE ( 'NONE', #47934, #81908, #49621, .T. ) ;
#128968 = CARTESIAN_POINT ( 'NONE',  ( 33.70710678118631165, 5.259292476615667233, 5.000000000000000000 ) ) ;
#128970 = AXIS2_PLACEMENT_3D ( 'NONE', #66884, #3036, #88649 ) ;
#128971 = CARTESIAN_POINT ( 'NONE',  ( -2.000000000000000000, 2.375000000000000000, 0.000000000000000000 ) ) ;
#128972 = CARTESIAN_POINT ( 'NONE',  ( -34.92499999999997584, -21.76999999999999247, -37.00000000000000000 ) ) ;
#128973 = ORIENTED_EDGE ( 'NONE', *, *, #119078, .T. ) ;
#128974 = ORIENTED_EDGE ( 'NONE', *, *, #23398, .F. ) ;
#128975 = ORIENTED_EDGE ( 'NONE', *, *, #58814, .F. ) ;
#128976 = DIRECTION ( 'NONE',  ( 0.7071067811865487940, 0.7071067811865463515, 0.000000000000000000 ) ) ;
#128977 = CARTESIAN_POINT ( 'NONE',  ( 181.1500000000000057, -43.14999999999999147, -34.92499999999998295 ) ) ;
#128978 = CARTESIAN_POINT ( 'NONE',  ( 6.629569808101885897, -3.967499999999998028, -6.871911579029511330 ) ) ;
#128979 = CARTESIAN_POINT ( 'NONE',  ( 22.60416666666666785, -1.633150327867672447, -6.094999999999999751 ) ) ;
#128980 = EDGE_LOOP ( 'NONE', ( #130188, #39204, #2535, #113448, #87356 ) ) ;
#128981 = VECTOR ( 'NONE', #71254, 1000.000000000000000 ) ;
#128982 = ORIENTED_EDGE ( 'NONE', *, *, #107825, .F. ) ;
#128983 = CARTESIAN_POINT ( 'NONE',  ( -13.24976746729824129, 4.588264127556670680, 4.661243073242808066 ) ) ;
#128985 = ORIENTED_EDGE ( 'NONE', *, *, #58959, .T. ) ;
#128984 = EDGE_CURVE ( 'NONE', #67467, #137150, #116266, .T. ) ;
#128986 = ORIENTED_EDGE ( 'NONE', *, *, #135348, .T. ) ;
#128987 = CARTESIAN_POINT ( 'NONE',  ( -8.999999999999952038, -16.02097659208073566, -11.96015758381207128 ) ) ;
#128988 = DIRECTION ( 'NONE',  ( 0.7071067811865487940, 0.7071067811865463515, 0.000000000000000000 ) ) ;
#128989 = VERTEX_POINT ( 'NONE', #84381 ) ;
#128990 = DIRECTION ( 'NONE',  ( -0.7071067811865486830, -0.7071067811865464625, -0.000000000000000000 ) ) ;
#128991 = EDGE_CURVE ( 'NONE', #127597, #138729, #128569, .T. ) ;
#128992 = CARTESIAN_POINT ( 'NONE',  ( 13.49999999999991473, 5.696342897626525570, -7.587980461218370998 ) ) ;
#128993 = PLANE ( 'NONE',  #78516 ) ;
#128994 = CARTESIAN_POINT ( 'NONE',  ( 11.51078643762690490, -27.52281430457047406, 5.000000000000000000 ) ) ;
#128995 = ORIENTED_EDGE ( 'NONE', *, *, #129595, .F. ) ;
#128996 = LINE ( 'NONE', #73914, #115801 ) ;
#128998 = FACE_BOUND ( 'NONE', #7847, .T. ) ;
#128997 = VECTOR ( 'NONE', #110067, 999.9999999999998863 ) ;
#128999 = EDGE_LOOP ( 'NONE', ( #47203, #83872, #115015, #91428 ) ) ;
#129000 = LINE ( 'NONE', #128315, #29519 ) ;
#129002 = EDGE_CURVE ( 'NONE', #49688, #140587, #138024, .T. ) ;
#129001 = CARTESIAN_POINT ( 'NONE',  ( -27.32816939922333432, -12.74070752338415247, 4.000000000000000000 ) ) ;
#129003 = LINE ( 'NONE', #96342, #107039 ) ;
#129004 = ORIENTED_EDGE ( 'NONE', *, *, #124533, .F. ) ;
#129005 = CARTESIAN_POINT ( 'NONE',  ( -51.18398860626899705, 28.73617430169823095, 5.000000000000000000 ) ) ;
#129006 = VERTEX_POINT ( 'NONE', #82934 ) ;
#129007 = ORIENTED_EDGE ( 'NONE', *, *, #43413, .F. ) ;
#129008 = VECTOR ( 'NONE', #133805, 1000.000000000000000 ) ;
#129009 = ORIENTED_EDGE ( 'NONE', *, *, #139487, .T. ) ;
#129010 = VECTOR ( 'NONE', #141281, 1000.000000000000000 ) ;
#129011 = VECTOR ( 'NONE', #32703, 1000.000000000000227 ) ;
#129012 = PLANE ( 'NONE',  #39649 ) ;
#129013 = CARTESIAN_POINT ( 'NONE',  ( 11.81601139373100651, 28.73617430169779041, 5.000000000000000000 ) ) ;
#129014 = CARTESIAN_POINT ( 'NONE',  ( 18.48921356237309510, -27.52281430457068367, 5.000000000000000000 ) ) ;
#129015 = CARTESIAN_POINT ( 'NONE',  ( 8.700255128608413102, -27.71228299555199825, 4.000000000000000000 ) ) ;
#129016 = CARTESIAN_POINT ( 'NONE',  ( 30.48921356237309510, -27.52281430457076894, 5.000000000000000000 ) ) ;
#129017 = CARTESIAN_POINT ( 'NONE',  ( 1.499999999999980460, 1.030536316426505117, -5.498701923753805509 ) ) ;
#129018 = VECTOR ( 'NONE', #33954, 1000.000000000000000 ) ;
#129019 = CARTESIAN_POINT ( 'NONE',  ( 48.18398860626899705, 28.73617430169820608, 5.000000000000000000 ) ) ;
#129020 = CARTESIAN_POINT ( 'NONE',  ( -12.19999999999999929, -60.26999999999998892, -40.00000000000000000 ) ) ;
#129021 = ADVANCED_FACE ( 'NONE', ( #82239 ), #126413, .T. ) ;
#129022 = DIRECTION ( 'NONE',  ( 0.7071067811865487940, 0.7071067811865463515, 0.000000000000000000 ) ) ;
#129023 = PLANE ( 'NONE',  #33194 ) ;
#129024 = ORIENTED_EDGE ( 'NONE', *, *, #7060, .T. ) ;
#129025 = VERTEX_POINT ( 'NONE', #16955 ) ;
#129026 = VERTEX_POINT ( 'NONE', #66185 ) ;
#129027 = ORIENTED_EDGE ( 'NONE', *, *, #60791, .F. ) ;
#129028 = CARTESIAN_POINT ( 'NONE',  ( -19.05000000000000071, 3.174999999999997158, 5.000000000000000000 ) ) ;
#129029 = EDGE_LOOP ( 'NONE', ( #119421, #64325, #137247, #83236 ) ) ;
#129030 = EDGE_LOOP ( 'NONE', ( #141913, #32012, #71619, #128965 ) ) ;
#129031 = FACE_OUTER_BOUND ( 'NONE', #80595, .T. ) ;
#129032 = DIRECTION ( 'NONE',  ( 1.000000000000000000, 0.000000000000000000, 0.000000000000000000 ) ) ;
#129033 = CARTESIAN_POINT ( 'NONE',  ( 34.42499999999998295, -1.458600742197942779, 5.000000000000000000 ) ) ;
#129034 = EDGE_CURVE ( 'NONE', #108517, #143240, #109001, .T. ) ;
#129035 = EDGE_CURVE ( 'NONE', #58614, #52888, #52421, .T. ) ;
#129036 = CARTESIAN_POINT ( 'NONE',  ( 0.3281693992235185098, 20.25929247661552068, 4.000000000000000000 ) ) ;
#129037 = ORIENTED_EDGE ( 'NONE', *, *, #45160, .T. ) ;
#129038 = CONICAL_SURFACE ( 'NONE', #13330, 2.500000000000000888, 0.9599310885968822538 ) ;
#129039 = DIRECTION ( 'NONE',  ( -0.7071067811865486830, -0.7071067811865464625, -0.000000000000000000 ) ) ;
#129040 = ORIENTED_EDGE ( 'NONE', *, *, #105482, .T. ) ;
#129041 = CARTESIAN_POINT ( 'NONE',  ( 0.000000000000000000, -59.76999999999998892, -39.50000000000000000 ) ) ;
#129042 = CARTESIAN_POINT ( 'NONE',  ( 34.42499999999998295, -21.72500000000000142, 4.500000000000000888 ) ) ;
#129043 = AXIS2_PLACEMENT_3D ( 'NONE', #139803, #51350, #130339 ) ;
#129044 = CARTESIAN_POINT ( 'NONE',  ( 12.02540314143521982, 2.126176841940962348, 7.934999999999989839 ) ) ;
#129045 = ORIENTED_EDGE ( 'NONE', *, *, #125279, .F. ) ;
#129046 = CARTESIAN_POINT ( 'NONE',  ( 88.72459685856478018, -1.637169565754161171, 6.109999999999998543 ) ) ;
#129047 = DIRECTION ( 'NONE',  ( -0.7071067811865486830, -0.7071067811865464625, 0.000000000000000000 ) ) ;
#129048 = VERTEX_POINT ( 'NONE', #131434 ) ;
#129049 = ORIENTED_EDGE ( 'NONE', *, *, #129621, .F. ) ;
#129050 = DIRECTION ( 'NONE',  ( -0.7071067811865487940, 0.7071067811865463515, -0.000000000000000000 ) ) ;
#129051 = VERTEX_POINT ( 'NONE', #121249 ) ;
#129052 = VECTOR ( 'NONE', #35936, 1000.000000000000000 ) ;
#129053 = FACE_OUTER_BOUND ( 'NONE', #139110, .T. ) ;
#129054 = LINE ( 'NONE', #75411, #13977 ) ;
#129055 = DIRECTION ( 'NONE',  ( 0.7071067811865487940, 0.7071067811865463515, -0.000000000000000000 ) ) ;
#129056 = CARTESIAN_POINT ( 'NONE',  ( -14.99999999999989875, -6.108550654416973202, -3.114665004255002589 ) ) ;
#129057 = EDGE_CURVE ( 'NONE', #84757, #41451, #42300, .T. ) ;
#129058 = ORIENTED_EDGE ( 'NONE', *, *, #96974, .T. ) ;
#129060 =( BOUNDED_CURVE ( )  B_SPLINE_CURVE ( 3, ( #62508, #42899, #18980, #131314 ),
 .UNSPECIFIED., .F., .T. ) 
 B_SPLINE_CURVE_WITH_KNOTS ( ( 4, 4 ),
 ( 1.208578181583235267, 1.359146454359429379 ),
 .UNSPECIFIED. ) 
 CURVE ( )  GEOMETRIC_REPRESENTATION_ITEM ( )  RATIONAL_B_SPLINE_CURVE ( ( 1.000000000000000000, 0.9981116584018954185, 0.9981116584018954185, 1.000000000000000000 ) ) 
 REPRESENTATION_ITEM ( '' )  );
#129059 = DIRECTION ( 'NONE',  ( -0.7071067811865487940, 0.7071067811865463515, -0.000000000000000000 ) ) ;
#129061 = CARTESIAN_POINT ( 'NONE',  ( 0.000000000000000000, 0.000000000000000000, 5.000000000000000000 ) ) ;
#129062 = CARTESIAN_POINT ( 'NONE',  ( -27.18398860626900060, 28.73617430169806042, 5.000000000000000000 ) ) ;
#129063 = VECTOR ( 'NONE', #85408, 1000.000000000000000 ) ;
#129064 = ORIENTED_EDGE ( 'NONE', *, *, #136760, .T. ) ;
#129065 = LINE ( 'NONE', #86303, #88307 ) ;
#129066 = CARTESIAN_POINT ( 'NONE',  ( -0.2997448713915885632, -27.71228299555206220, 4.000000000000000000 ) ) ;
#129067 = EDGE_LOOP ( 'NONE', ( #49781, #5963, #76856 ) ) ;
#129068 = CIRCLE ( 'NONE', #105967, 0.4999999999999996669 ) ;
#129070 = ORIENTED_EDGE ( 'NONE', *, *, #115451, .F. ) ;
#129069 = DIRECTION ( 'NONE',  ( 0.6830127018922181881, 0.6830127018922202975, -0.2588190451025214056 ) ) ;
#129071 = VERTEX_POINT ( 'NONE', #21939 ) ;
#129072 = CARTESIAN_POINT ( 'NONE',  ( 0.000000000000000000, 0.000000000000000000, 5.000000000000000000 ) ) ;
#129073 = LINE ( 'NONE', #84865, #55366 ) ;
#129074 = ORIENTED_EDGE ( 'NONE', *, *, #44322, .T. ) ;
#129075 = CARTESIAN_POINT ( 'NONE',  ( 0.6684674115985667076, -18.74070752338408496, 20.73178291233841009 ) ) ;
#129076 = UNCERTAINTY_MEASURE_WITH_UNIT (LENGTH_MEASURE( 1.000000000000000082E-05 ), #99489, 'distance_accuracy_value', 'NONE');
#129077 = CARTESIAN_POINT ( 'NONE',  ( 14.21837311707495743, 21.74787736706806740, 4.999607392498049308 ) ) ;
#129078 = ADVANCED_FACE ( 'NONE', ( #141596 ), #43004, .F. ) ;
#129079 = AXIS2_PLACEMENT_3D ( 'NONE', #48599, #81248, #60205 ) ;
#129080 = DIRECTION ( 'NONE',  ( -0.000000000000000000, 0.000000000000000000, 1.000000000000000000 ) ) ;
#129081 = ADVANCED_FACE ( 'NONE', ( #95933 ), #140170, .F. ) ;
#129082 = CARTESIAN_POINT ( 'NONE',  ( 32.35416666666665719, -2.130196079827501698, -7.949999999999956657 ) ) ;
#129083 = LINE ( 'NONE', #19612, #65229 ) ;
#129084 = PLANE ( 'NONE',  #30924 ) ;
#129085 = FACE_OUTER_BOUND ( 'NONE', #40432, .T. ) ;
#129086 = DIRECTION ( 'NONE',  ( 0.6830127018922180770, -0.6830127018922204085, -0.2588190451025213501 ) ) ;
#129087 = CARTESIAN_POINT ( 'NONE',  ( -29.20710678118632586, -11.24070752338416668, 5.000000000000000000 ) ) ;
#129088 = DIRECTION ( 'NONE',  ( -0.7071067811865487940, 0.7071067811865463515, 0.000000000000000000 ) ) ;
#129089 = DIRECTION ( 'NONE',  ( -0.7071067811865486830, -0.7071067811865464625, -0.000000000000000000 ) ) ;
#129091 = EDGE_CURVE ( 'NONE', #51626, #96824, #67456, .T. ) ;
#129090 = SURFACE_STYLE_USAGE ( .BOTH. , #41365 ) ;
#129093 = EDGE_CURVE ( 'NONE', #80606, #126512, #30708, .T. ) ;
#129092 = ORIENTED_EDGE ( 'NONE', *, *, #129833, .T. ) ;
#129094 = ORIENTED_EDGE ( 'NONE', *, *, #69355, .T. ) ;
#129095 = ORIENTED_EDGE ( 'NONE', *, *, #38407, .F. ) ;
#129096 = CARTESIAN_POINT ( 'NONE',  ( 107.0208333333333002, 7.949999999999999289, 2.130196079827431532 ) ) ;
#129097 = ORIENTED_EDGE ( 'NONE', *, *, #73378, .T. ) ;
#129098 = ORIENTED_EDGE ( 'NONE', *, *, #91169, .F. ) ;
#129099 = ORIENTED_EDGE ( 'NONE', *, *, #87375, .F. ) ;
#129100 = DIRECTION ( 'NONE',  ( -0.7071067811865486830, 0.7071067811865464625, 0.000000000000000000 ) ) ;
#129101 = CARTESIAN_POINT ( 'NONE',  ( 34.91107144025653497, 21.84219451764873909, 4.000000000000000000 ) ) ;
#129102 = ORIENTED_EDGE ( 'NONE', *, *, #50229, .F. ) ;
#129103 = VECTOR ( 'NONE', #34022, 1000.000000000000000 ) ;
#129104 = CARTESIAN_POINT ( 'NONE',  ( -6.005480084712508493, 28.92564299267933947, 4.000000000000000000 ) ) ;
#129105 = CARTESIAN_POINT ( 'NONE',  ( -25.99806943317883423, -22.22500000000000142, 4.500000000000000888 ) ) ;
#129106 = EDGE_CURVE ( 'NONE', #30609, #93894, #140849, .T. ) ;
#129107 = LINE ( 'NONE', #29786, #32576 ) ;
#129108 = DIRECTION ( 'NONE',  ( -0.3543493200069162685, -0.000000000000000000, -0.9351131265310288487 ) ) ;
#129109 = CARTESIAN_POINT ( 'NONE',  ( 105.8754301918981042, -5.291415217122920289, -3.055000000000001492 ) ) ;
#129110 = ORIENTED_EDGE ( 'NONE', *, *, #42728, .T. ) ;
#129111 = EDGE_CURVE ( 'NONE', #68534, #105207, #32112, .T. ) ;
#129113 = LINE ( 'NONE', #27652, #76596 ) ;
#129112 = APPLICATION_CONTEXT ( 'automotive_design' ) ;
#129114 = FILL_AREA_STYLE_COLOUR ( '', #79480 ) ;
#129115 = CARTESIAN_POINT ( 'NONE',  ( 63.48921356237309510, -27.52281430457099631, 5.000000000000000000 ) ) ;
#129117 = FACE_OUTER_BOUND ( 'NONE', #96579, .T. ) ;
#129116 = VECTOR ( 'NONE', #26836, 1000.000000000000000 ) ;
#129118 = PLANE ( 'NONE',  #53863 ) ;
#129119 = CARTESIAN_POINT ( 'NONE',  ( 7.499999999999949374, 21.05218569542895324, 5.000000000000000000 ) ) ;
#129120 = VECTOR ( 'NONE', #69115, 1000.000000000000000 ) ;
#129121 = DIRECTION ( 'NONE',  ( -0.000000000000000000, 0.000000000000000000, 1.000000000000000000 ) ) ;
#129122 = EDGE_CURVE ( 'NONE', #91522, #54031, #31405, .T. ) ;
#129123 = DIRECTION ( 'NONE',  ( -0.000000000000000000, 0.000000000000000000, 1.000000000000000000 ) ) ;
#129124 = LINE ( 'NONE', #131811, #136470 ) ;
#129125 = VERTEX_POINT ( 'NONE', #118388 ) ;
#129126 = ORIENTED_EDGE ( 'NONE', *, *, #23351, .T. ) ;
#129127 = CARTESIAN_POINT ( 'NONE',  ( 125.2712635252314470, 4.472830434245839371, 4.472830434245842035 ) ) ;
#129128 = VERTEX_POINT ( 'NONE', #63352 ) ;
#129129 = CARTESIAN_POINT ( 'NONE',  ( 5.691592354503320905, -3.851859888774471706E-31, 2.500000000000001332 ) ) ;
#129130 = CARTESIAN_POINT ( 'NONE',  ( 0.005480084712502889671, 28.92564299267938210, 4.000000000000000000 ) ) ;
#129131 = B_SPLINE_CURVE_WITH_KNOTS ( 'NONE', 3,
 ( #22001, #100303, #98159, #66960 ),
 .UNSPECIFIED., .F., .F.,
 ( 4, 4 ),
 ( 0.001201692628197130247, 0.001634763834693580111 ),
 .UNSPECIFIED. ) ;
#129132 = EDGE_CURVE ( 'NONE', #117635, #108859, #74932, .T. ) ;
#129133 = DIRECTION ( 'NONE',  ( 0.7071067811865487940, 0.7071067811865463515, 0.000000000000000000 ) ) ;
#129134 = DIRECTION ( 'NONE',  ( 0.6830127018922180770, -0.6830127018922204085, -0.2588190451025213501 ) ) ;
#129135 = DIRECTION ( 'NONE',  ( -1.000000000000000000, -0.000000000000000000, -0.000000000000000000 ) ) ;
#129136 = PRESENTATION_STYLE_ASSIGNMENT (( #140041 ) ) ;
#129137 = CARTESIAN_POINT ( 'NONE',  ( 122.2662635252314374, 4.472830434245839371, -4.472830434245838482 ) ) ;
#129138 = ORIENTED_EDGE ( 'NONE', *, *, #119802, .F. ) ;
#129139 = CARTESIAN_POINT ( 'NONE',  ( -15.18398860626900237, 28.73617430169797871, 5.000000000000000000 ) ) ;
#129140 = ORIENTED_EDGE ( 'NONE', *, *, #39987, .F. ) ;
#129141 = EDGE_CURVE ( 'NONE', #71727, #116539, #8181, .T. ) ;
#129142 = DIRECTION ( 'NONE',  ( -0.7071067811865486830, 0.7071067811865464625, 0.000000000000000000 ) ) ;
#129143 = DIRECTION ( 'NONE',  ( -0.6830127018922181881, 0.6830127018922202975, -0.2588190451025214056 ) ) ;
#129144 = CARTESIAN_POINT ( 'NONE',  ( 60.29974487139158867, -27.71228299555248142, 4.000000000000000000 ) ) ;
#129145 = CARTESIAN_POINT ( 'NONE',  ( 29.22995720542186149, 21.73644205237998506, 5.000000000000000888 ) ) ;
#129146 = EDGE_LOOP ( 'NONE', ( #56353, #87381, #83633, #108331 ) ) ;
#129147 = CARTESIAN_POINT ( 'NONE',  ( 41.56293019189811133, 1.637169565754157174, 6.110000000000002984 ) ) ;
#129148 = ORIENTED_EDGE ( 'NONE', *, *, #13634, .T. ) ;
#129149 = DIRECTION ( 'NONE',  ( -0.000000000000000000, 0.000000000000000000, 1.000000000000000000 ) ) ;
#129150 = CARTESIAN_POINT ( 'NONE',  ( 20.99999999999985789, 11.96639925780214320, 5.000000000000000000 ) ) ;
#129151 = CARTESIAN_POINT ( 'NONE',  ( -81.48921356237309510, -27.52281430457112066, 5.000000000000000000 ) ) ;
#129152 = EDGE_CURVE ( 'NONE', #101337, #80109, #98088, .T. ) ;
#129153 = AXIS2_PLACEMENT_3D ( 'NONE', #85497, #18079, #105816 ) ;
#129154 = CARTESIAN_POINT ( 'NONE',  ( 36.29974487139159578, -27.71228299555231445, 4.000000000000000000 ) ) ;
#129155 = EDGE_CURVE ( 'NONE', #55245, #43089, #142322, .T. ) ;
#129156 = CARTESIAN_POINT ( 'NONE',  ( 43.95376352523145158, -6.109999999999998543, -3.741295971395162543E-16 ) ) ;
#129157 = VERTEX_POINT ( 'NONE', #119800 ) ;
#129158 = CARTESIAN_POINT ( 'NONE',  ( -36.48921356237310221, -27.52281430457080802, 5.000000000000000000 ) ) ;
#129159 = EDGE_LOOP ( 'NONE', ( #102881, #131822, #28525, #44631, #21107 ) ) ;
#129160 = ORIENTED_EDGE ( 'NONE', *, *, #126146, .F. ) ;
#129161 = ORIENTED_EDGE ( 'NONE', *, *, #107641, .F. ) ;
#129162 =( BOUNDED_CURVE ( )  B_SPLINE_CURVE ( 3, ( #137590, #136147, #39721, #7012 ),
 .UNSPECIFIED., .F., .F. ) 
 B_SPLINE_CURVE_WITH_KNOTS ( ( 4, 4 ),
 ( 5.143245962375964986, 6.645403452391246191 ),
 .UNSPECIFIED. ) 
 CURVE ( )  GEOMETRIC_REPRESENTATION_ITEM ( )  RATIONAL_B_SPLINE_CURVE ( ( 1.000000000000000000, 0.8206354192515240564, 0.8206354192515240564, 1.000000000000000000 ) ) 
 REPRESENTATION_ITEM ( '' )  );
#129163 = VERTEX_POINT ( 'NONE', #32852 ) ;
#129164 = CARTESIAN_POINT ( 'NONE',  ( 11.99451991528749417, 28.92564299267946382, 4.000000000000000000 ) ) ;
#129165 = LINE ( 'NONE', #29847, #139186 ) ;
#129166 = FACE_BOUND ( 'NONE', #62819, .T. ) ;
#129167 = VERTEX_POINT ( 'NONE', #76339 ) ;
#129168 = SURFACE_SIDE_STYLE ('',( #84286 ) ) ;
#129169 = CARTESIAN_POINT ( 'NONE',  ( 22.85159235450332105, 2.500000000000001776, 0.000000000000000000 ) ) ;
#129170 = ORIENTED_EDGE ( 'NONE', *, *, #40155, .T. ) ;
#129171 = LINE ( 'NONE', #75528, #50382 ) ;
#129172 = VERTEX_POINT ( 'NONE', #20492 ) ;
#129173 = ORIENTED_EDGE ( 'NONE', *, *, #4451, .T. ) ;
#129174 = CARTESIAN_POINT ( 'NONE',  ( -4.171830600776436526, 9.759292476615614831, 4.000000000000000000 ) ) ;
#129175 = ORIENTED_EDGE ( 'NONE', *, *, #134532, .F. ) ;
#129176 = CARTESIAN_POINT ( 'NONE',  ( 56.34959685856478018, 6.109999999999996767, 1.637169565754163836 ) ) ;
#129177 = ORIENTED_EDGE ( 'NONE', *, *, #116123, .F. ) ;
#129178 = VECTOR ( 'NONE', #72006, 1000.000000000000227 ) ;
#129179 = LINE ( 'NONE', #29864, #16294 ) ;
#129180 = PLANE ( 'NONE',  #125987 ) ;
#129181 = ADVANCED_FACE ( 'NONE', ( #120503 ), #132343, .T. ) ;
#129182 = ORIENTED_EDGE ( 'NONE', *, *, #11334, .F. ) ;
#129183 = ADVANCED_FACE ( 'NONE', ( #65490 ), #98774, .F. ) ;
#129184 = LINE ( 'NONE', #19011, #101142 ) ;
#129185 = CARTESIAN_POINT ( 'NONE',  ( -7.171830600776425868, 12.75929247661559529, 4.000000000000000000 ) ) ;
#129186 = DIRECTION ( 'NONE',  ( 0.7071067811865487940, 0.7071067811865463515, 0.000000000000000000 ) ) ;
#129187 = CARTESIAN_POINT ( 'NONE',  ( -12.69999999999998153, 0.000000000000000000, 2.500000000000000444 ) ) ;
#129188 = DIRECTION ( 'NONE',  ( 0.7071067811865487940, 0.7071067811865463515, 0.000000000000000000 ) ) ;
#129189 = ORIENTED_EDGE ( 'NONE', *, *, #3135, .F. ) ;
#129190 = ORIENTED_EDGE ( 'NONE', *, *, #127046, .F. ) ;
#129191 = CARTESIAN_POINT ( 'NONE',  ( 7.940000000000001279, -35.14999999999999858, -10.00000000000000178 ) ) ;
#129193 = DIRECTION ( 'NONE',  ( -0.7071067811865486830, 0.7071067811865464625, 0.000000000000000000 ) ) ;
#129192 = VECTOR ( 'NONE', #72226, 999.9999999999998863 ) ;
#129194 = ORIENTED_EDGE ( 'NONE', *, *, #81606, .T. ) ;
#129195 = ORIENTED_EDGE ( 'NONE', *, *, #106297, .F. ) ;
#129197 = VERTEX_POINT ( 'NONE', #24794 ) ;
#129196 = VECTOR ( 'NONE', #7556, 1000.000000000000114 ) ;
#129198 = CARTESIAN_POINT ( 'NONE',  ( 5.292986735706907808, -21.74070752338406365, 4.999753212805221558 ) ) ;
#129199 = CARTESIAN_POINT ( 'NONE',  ( 54.62086038379622721, -6.884901960086286188, 3.974999999999997424 ) ) ;
#129200 = EDGE_CURVE ( 'NONE', #135168, #11025, #55306, .T. ) ;
#129201 = EDGE_CURVE ( 'NONE', #85105, #64105, #102392, .T. ) ;
#129202 = DIRECTION ( 'NONE',  ( -0.000000000000000000, -0.000000000000000000, 1.000000000000000000 ) ) ;
#129203 = ORIENTED_EDGE ( 'NONE', *, *, #112869, .F. ) ;
#129204 = CARTESIAN_POINT ( 'NONE',  ( -4.499999999999959144, -14.94781430457067373, 5.000000000000000000 ) ) ;
#129205 = AXIS2_PLACEMENT_3D ( 'NONE', #125655, #70590, #2394 ) ;
#129206 = AXIS2_PLACEMENT_3D ( 'NONE', #15223, #71089, #60209 ) ;
#129207 = FILL_AREA_STYLE ('',( #83604 ) ) ;
#129208 = CARTESIAN_POINT ( 'NONE',  ( 20.62956980810188412, -3.967499999999998028, -6.871911579029511330 ) ) ;
#129209 = DIRECTION ( 'NONE',  ( 0.7071067811865486830, -0.7071067811865464625, -0.000000000000000000 ) ) ;
#129210 = ORIENTED_EDGE ( 'NONE', *, *, #92887, .F. ) ;
#129211 = CARTESIAN_POINT ( 'NONE',  ( 119.4954301918981230, 5.291415217122917625, 3.055000000000002380 ) ) ;
#129212 = ADVANCED_FACE ( 'NONE', ( #12486 ), #89346, .T. ) ;
#129213 = DIRECTION ( 'NONE',  ( -0.7071067811865486830, 0.7071067811865463515, 0.000000000000000000 ) ) ;
#129214 = FACE_OUTER_BOUND ( 'NONE', #11886, .T. ) ;
#129216 = VERTEX_POINT ( 'NONE', #99480 ) ;
#129215 = DIRECTION ( 'NONE',  ( -0.6830127018922180770, -0.6830127018922204085, -0.2588190451025213501 ) ) ;
#129217 = CARTESIAN_POINT ( 'NONE',  ( -15.18398860626900237, 28.73617430169797871, 5.000000000000000000 ) ) ;
#129218 = ORIENTED_EDGE ( 'NONE', *, *, #135486, .T. ) ;
#129219 = LINE ( 'NONE', #19755, #24115 ) ;
#129220 = CARTESIAN_POINT ( 'NONE',  ( 0.000000000000000000, -21.72500000000000142, 4.500000000000000888 ) ) ;
#129221 = LINE ( 'NONE', #118344, #35613 ) ;
#129222 = ADVANCED_FACE ( 'NONE', ( #22621 ), #11758, .F. ) ;
#129223 = ORIENTED_EDGE ( 'NONE', *, *, #75860, .F. ) ;
#129224 = DIRECTION ( 'NONE',  ( -0.7071067811865486830, 0.7071067811865464625, 0.000000000000000000 ) ) ;
#129225 = PLANE ( 'NONE',  #120580 ) ;
#129226 = CARTESIAN_POINT ( 'NONE',  ( 24.66846741159842082, -18.74070752338409562, 20.73178291233847048 ) ) ;
#129227 = ORIENTED_EDGE ( 'NONE', *, *, #125471, .F. ) ;
#129228 = VECTOR ( 'NONE', #116623, 1000.000000000000227 ) ;
#129229 = EDGE_CURVE ( 'NONE', #5611, #95146, #100232, .T. ) ;
#129230 = DIRECTION ( 'NONE',  ( -0.6830127018922181881, 0.6830127018922202975, -0.2588190451025214056 ) ) ;
#129231 = CARTESIAN_POINT ( 'NONE',  ( 21.18398860626899349, 28.73617430169802134, 5.000000000000000000 ) ) ;
#129233 = VECTOR ( 'NONE', #10317, 1000.000000000000000 ) ;
#129232 = DIRECTION ( 'NONE',  ( -0.3543493200069162685, -0.000000000000000000, -0.9351131265310288487 ) ) ;
#129234 = CARTESIAN_POINT ( 'NONE',  ( -33.48921356237309510, -27.52281430457078670, 5.000000000000000000 ) ) ;
#129235 = LINE ( 'NONE', #29921, #11351 ) ;
#129236 = ORIENTED_EDGE ( 'NONE', *, *, #94771, .T. ) ;
#129237 = ORIENTED_EDGE ( 'NONE', *, *, #49867, .T. ) ;
#129238 = CARTESIAN_POINT ( 'NONE',  ( 0.000000000000000000, 0.000000000000000000, 0.000000000000000000 ) ) ;
#129239 = CARTESIAN_POINT ( 'NONE',  ( 11.99999999999992006, 5.966399257802200040, 5.000000000000000000 ) ) ;
#129240 = CARTESIAN_POINT ( 'NONE',  ( 12.22873647476855119, 5.808823158059031044, -5.808823158059038150 ) ) ;
#129241 = DIRECTION ( 'NONE',  ( -0.000000000000000000, 0.3543493200069153248, 0.9351131265310291818 ) ) ;
#129242 = DIRECTION ( 'NONE',  ( -0.3543493200069163240, -0.000000000000000000, -0.9351131265310288487 ) ) ;
#129243 = CARTESIAN_POINT ( 'NONE',  ( 0.8183591370940056509, -52.14999999999999147, 41.64499999999997470 ) ) ;
#129244 = ORIENTED_EDGE ( 'NONE', *, *, #111916, .F. ) ;
#129245 = EDGE_CURVE ( 'NONE', #72134, #1799, #32775, .T. ) ;
#129246 = DIRECTION ( 'NONE',  ( 0.6830127018922181881, 0.6830127018922202975, -0.2588190451025214056 ) ) ;
#129247 = CARTESIAN_POINT ( 'NONE',  ( 24.56840764549667355, 2.500000000000003553, 3.061616997868386099E-16 ) ) ;
#129248 = LINE ( 'NONE', #30687, #21495 ) ;
#129249 = CIRCLE ( 'NONE', #66772, 31.92999999999999261 ) ;
#129250 = FACE_OUTER_BOUND ( 'NONE', #121078, .T. ) ;
#129251 = CARTESIAN_POINT ( 'NONE',  ( 35.78709685856478018, 3.054999999999997939, 5.291415217122920289 ) ) ;
#129252 = DIRECTION ( 'NONE',  ( -0.7071067811865487940, 0.7071067811865463515, -0.000000000000000000 ) ) ;
#129254 = ADVANCED_FACE ( 'NONE', ( #151 ), #91504, .T. ) ;
#129253 = VECTOR ( 'NONE', #19951, 1000.000000000000000 ) ;
#129255 = EDGE_CURVE ( 'NONE', #56732, #126282, #123442, .T. ) ;
#129256 = VERTEX_POINT ( 'NONE', #66888 ) ;
#129257 = LINE ( 'NONE', #116964, #102046 ) ;
#129258 = EDGE_LOOP ( 'NONE', ( #142162, #56748, #91679, #58643 ) ) ;
#129259 = ORIENTED_EDGE ( 'NONE', *, *, #118218, .F. ) ;
#129260 = DIRECTION ( 'NONE',  ( 0.000000000000000000, -1.000000000000000000, 0.000000000000000000 ) ) ;
#129261 = DIRECTION ( 'NONE',  ( -0.7071067811865486830, -0.7071067811865464625, -0.000000000000000000 ) ) ;
#129262 = ADVANCED_FACE ( 'NONE', ( #13184 ), #57458, .T. ) ;
#129263 = DIRECTION ( 'NONE',  ( -0.000000000000000000, 0.000000000000000000, 1.000000000000000000 ) ) ;
#129264 = DIRECTION ( 'NONE',  ( 0.6830127018922181881, 0.6830127018922202975, -0.2588190451025214056 ) ) ;
#129265 = LINE ( 'NONE', #53130, #129663 ) ;
#129266 = EDGE_CURVE ( 'NONE', #127303, #16103, #31803, .T. ) ;
#129267 = DIRECTION ( 'NONE',  ( -0.3543493200069162685, -0.000000000000000000, -0.9351131265310288487 ) ) ;
#129268 = DIRECTION ( 'NONE',  ( 0.7071067811865486830, -0.7071067811865464625, -0.000000000000000000 ) ) ;
#129269 = VERTEX_POINT ( 'NONE', #880 ) ;
#129270 = ADVANCED_FACE ( 'NONE', ( #111066 ), #67633, .F. ) ;
#129271 = DIRECTION ( 'NONE',  ( 0.6830127018922180770, -0.6830127018922204085, -0.2588190451025213501 ) ) ;
#129272 = LINE ( 'NONE', #140855, #72336 ) ;
#129273 = DIRECTION ( 'NONE',  ( -1.000000000000000000, 0.000000000000000000, 0.000000000000000000 ) ) ;
#129274 = CARTESIAN_POINT ( 'NONE',  ( -6.489213562373093325, -27.52281430457059841, 5.000000000000000000 ) ) ;
#129275 = CARTESIAN_POINT ( 'NONE',  ( -5.207106781186501721, -14.24070752338413293, 5.000000000000000000 ) ) ;
#129276 = CARTESIAN_POINT ( 'NONE',  ( -26.99999999999980460, 14.58746187583909837, 4.000000000000000000 ) ) ;
#129277 = CARTESIAN_POINT ( 'NONE',  ( 56.37086038379622721, 6.884901960086289741, -3.974999999999993427 ) ) ;
#129278 = EDGE_CURVE ( 'NONE', #106598, #89590, #58867, .T. ) ;
#129279 = DIRECTION ( 'NONE',  ( 0.7071067811865486830, -0.7071067811865464625, -0.000000000000000000 ) ) ;
#129280 = ORIENTED_EDGE ( 'NONE', *, *, #83119, .F. ) ;
#129281 = ORIENTED_EDGE ( 'NONE', *, *, #30960, .F. ) ;
#129282 = CARTESIAN_POINT ( 'NONE',  ( 54.81249999999998579, 5.819803920172571310, 5.819803920172575751 ) ) ;
#129283 = ADVANCED_FACE ( 'NONE', ( #62996 ), #39072, .T. ) ;
#129284 = DIRECTION ( 'NONE',  ( -0.3543493200069163240, 0.000000000000000000, 0.9351131265310288487 ) ) ;
#129285 = CARTESIAN_POINT ( 'NONE',  ( 29.99999999999979039, -21.84840872380821963, 2.849755605029675731 ) ) ;
#129286 = CARTESIAN_POINT ( 'NONE',  ( 19.49999999999986500, -15.29013452822852770, 0.3645803511610800074 ) ) ;
#129287 = VERTEX_POINT ( 'NONE', #19457 ) ;
#129288 = EDGE_CURVE ( 'NONE', #56372, #23069, #8529, .T. ) ;
#129289 = CARTESIAN_POINT ( 'NONE',  ( -8.816011393731004731, 28.73617430169781173, 5.000000000000000000 ) ) ;
#129290 = CARTESIAN_POINT ( 'NONE',  ( 47.68793019189809712, 6.110000000000002984, -1.637169565754156730 ) ) ;
#129291 = VERTEX_POINT ( 'NONE', #106423 ) ;
#129292 = FACE_OUTER_BOUND ( 'NONE', #53611, .T. ) ;
#129293 = ORIENTED_EDGE ( 'NONE', *, *, #140376, .T. ) ;
#129294 = ORIENTED_EDGE ( 'NONE', *, *, #42513, .T. ) ;
#129295 = DIRECTION ( 'NONE',  ( -0.6830127018922181881, 0.6830127018922202975, -0.2588190451025214056 ) ) ;
#129296 = VECTOR ( 'NONE', #141292, 999.9999999999998863 ) ;
#129297 = VECTOR ( 'NONE', #62218, 1000.000000000000000 ) ;
#129298 = AXIS2_PLACEMENT_3D ( 'NONE', #53778, #121835, #66778 ) ;
#129299 =( NAMED_UNIT ( * ) SI_UNIT ( $, .STERADIAN. ) SOLID_ANGLE_UNIT ( ) );
#129300 = FACE_OUTER_BOUND ( 'NONE', #23192, .T. ) ;
#129301 = VECTOR ( 'NONE', #141484, 1000.000000000000227 ) ;
#129302 = CARTESIAN_POINT ( 'NONE',  ( -28.49999999999979750, 7.466399257802189382, 5.000000000000000000 ) ) ;
#129303 = ORIENTED_EDGE ( 'NONE', *, *, #79310, .F. ) ;
#129305 = CIRCLE ( 'NONE', #15851, 2.247899999999995568 ) ;
#129304 = CARTESIAN_POINT ( 'NONE',  ( -9.328169399223463998, -12.74070752338415780, 4.000000000000000000 ) ) ;
#129307 = EDGE_LOOP ( 'NONE', ( #34894, #37474, #106745, #108952 ) ) ;
#129306 = DIRECTION ( 'NONE',  ( -0.3543493200069162685, -0.000000000000000000, -0.9351131265310288487 ) ) ;
#129308 = CARTESIAN_POINT ( 'NONE',  ( -28.59167451900981405, -0.7407075233842735917, 14.76736230305374065 ) ) ;
#129309 = CARTESIAN_POINT ( 'NONE',  ( 23.99451991528749062, 28.92564299267954908, 4.000000000000000000 ) ) ;
#129310 = EDGE_CURVE ( 'NONE', #116472, #21645, #74574, .T. ) ;
#129311 =( GEOMETRIC_REPRESENTATION_CONTEXT ( 3 ) GLOBAL_UNCERTAINTY_ASSIGNED_CONTEXT ( ( #36029 ) ) GLOBAL_UNIT_ASSIGNED_CONTEXT ( ( #89960, #68970, #137059 ) ) REPRESENTATION_CONTEXT ( 'NONE', 'WORKASPACE' ) );
#129312 = CARTESIAN_POINT ( 'NONE',  ( 24.29177708983032957, -15.74070752338412049, 19.73771281079103446 ) ) ;
#129313 = VECTOR ( 'NONE', #101848, 1000.000000000000000 ) ;
#129314 = EDGE_CURVE ( 'NONE', #122713, #43483, #63703, .T. ) ;
#129315 = EDGE_LOOP ( 'NONE', ( #93920, #141132, #21984, #29904 ) ) ;
#129316 = ADVANCED_FACE ( 'NONE', ( #31072 ), #94150, .T. ) ;
#129317 = ORIENTED_EDGE ( 'NONE', *, *, #117813, .T. ) ;
#129318 = CARTESIAN_POINT ( 'NONE',  ( 62.91209685856477307, 5.291415217122921177, -3.054999999999994831 ) ) ;
#129319 = DIRECTION ( 'NONE',  ( 1.000000000000000000, 0.000000000000000000, 0.000000000000000000 ) ) ;
#129320 = LINE ( 'NONE', #107572, #121853 ) ;
#129321 = LINE ( 'NONE', #74251, #105697 ) ;
#129322 = VERTEX_POINT ( 'NONE', #127507 ) ;
#129323 = ORIENTED_EDGE ( 'NONE', *, *, #87263, .T. ) ;
#129324 = AXIS2_PLACEMENT_3D ( 'NONE', #19771, #86482, #74171 ) ;
#129325 = PLANE ( 'NONE',  #60792 ) ;
#129327 = EDGE_CURVE ( 'NONE', #39945, #110130, #95584, .T. ) ;
#129326 = CARTESIAN_POINT ( 'NONE',  ( -21.18398860626899349, 28.73617430169802134, 5.000000000000000000 ) ) ;
#129328 = VERTEX_POINT ( 'NONE', #96972 ) ;
#129329 = ORIENTED_EDGE ( 'NONE', *, *, #110667, .T. ) ;
#129330 = VECTOR ( 'NONE', #136591, 1000.000000000000000 ) ;
#129331 = CARTESIAN_POINT ( 'NONE',  ( -6.643187427517349697, -20.24070752338407786, 21.22881796311211389 ) ) ;
#129332 = ORIENTED_EDGE ( 'NONE', *, *, #63006, .F. ) ;
#129333 = DIRECTION ( 'NONE',  ( -0.000000000000000000, 0.000000000000000000, 1.000000000000000000 ) ) ;
#129334 = CARTESIAN_POINT ( 'NONE',  ( -34.92500000000001137, -22.22500000000000142, 4.500000000000000888 ) ) ;
#129335 = VECTOR ( 'NONE', #76154, 1000.000000000000000 ) ;
#129336 = VECTOR ( 'NONE', #83511, 1000.000000000000000 ) ;
#129337 = AXIS2_PLACEMENT_3D ( 'NONE', #20844, #89680, #65840 ) ;
#129339 = DIRECTION ( 'NONE',  ( 0.7071067811865487940, 0.7071067811865463515, 0.000000000000000000 ) ) ;
#129338 = AXIS2_PLACEMENT_3D ( 'NONE', #103002, #105820, #115988 ) ;
#129340 = FACE_BOUND ( 'NONE', #51891, .T. ) ;
#129341 = CARTESIAN_POINT ( 'NONE',  ( -11.20710678118645731, -14.24070752338412937, 5.000000000000000000 ) ) ;
#129342 = LINE ( 'NONE', #74274, #39701 ) ;
#129343 = DIRECTION ( 'NONE',  ( -0.7071067811865487940, 0.7071067811865463515, -0.000000000000000000 ) ) ;
#129345 = ORIENTED_EDGE ( 'NONE', *, *, #136320, .T. ) ;
#129344 = CARTESIAN_POINT ( 'NONE',  ( 62.25000000000000000, -9.735942053221458872E-16, 7.950000000000000178 ) ) ;
#129346 = AXIS2_PLACEMENT_3D ( 'NONE', #128919, #84709, #39806 ) ;
#129347 = VECTOR ( 'NONE', #135316, 1000.000000000000000 ) ;
#129348 = ORIENTED_EDGE ( 'NONE', *, *, #54368, .F. ) ;
#129349 = ORIENTED_EDGE ( 'NONE', *, *, #91430, .T. ) ;
#129350 = CARTESIAN_POINT ( 'NONE',  ( 81.87043019189812298, -3.055000000000001492, 5.291415217122917625 ) ) ;
#129351 = ORIENTED_EDGE ( 'NONE', *, *, #65697, .F. ) ;
#129352 = CARTESIAN_POINT ( 'NONE',  ( -38.99451991528749062, 28.92564299267965211, 4.000000000000000000 ) ) ;
#129353 = PLANE ( 'NONE',  #25730 ) ;
#129354 = EDGE_CURVE ( 'NONE', #80143, #120101, #17312, .T. ) ;
#129355 = EDGE_CURVE ( 'NONE', #13817, #1460, #109114, .T. ) ;
#129356 = CARTESIAN_POINT ( 'NONE',  ( 20.99999999999985079, -16.60178936734446609, 0.8616154019347975757 ) ) ;
#129357 = VECTOR ( 'NONE', #6169, 1000.000000000000000 ) ;
#129358 = FACE_OUTER_BOUND ( 'NONE', #6195, .T. ) ;
#129359 = LINE ( 'NONE', #41641, #53022 ) ;
#129360 = LINE ( 'NONE', #143105, #13064 ) ;
#129361 = CARTESIAN_POINT ( 'NONE',  ( -18.18398860626898994, 28.73617430169800002, 5.000000000000000000 ) ) ;
#129362 = CARTESIAN_POINT ( 'NONE',  ( 0.000000000000000000, 0.000000000000000000, 0.000000000000000000 ) ) ;
#129363 = DIRECTION ( 'NONE',  ( -0.6830127018922180770, -0.6830127018922204085, -0.2588190451025213501 ) ) ;
#129364 = DIRECTION ( 'NONE',  ( -0.7071067811865486830, 0.7071067811865464625, 0.000000000000000000 ) ) ;
#129365 = DIRECTION ( 'NONE',  ( -0.000000000000000000, 0.000000000000000000, 1.000000000000000000 ) ) ;
#129366 = VERTEX_POINT ( 'NONE', #16585 ) ;
#129367 = CARTESIAN_POINT ( 'NONE',  ( -16.50229999999999819, 3.130000000000007887, -22.35000000000000142 ) ) ;
#129368 = ADVANCED_FACE ( 'NONE', ( #117318 ), #41199, .T. ) ;
#129369 = ORIENTED_EDGE ( 'NONE', *, *, #116883, .T. ) ;
#129370 = ORIENTED_EDGE ( 'NONE', *, *, #138594, .F. ) ;
#129371 = EDGE_CURVE ( 'NONE', #52857, #33478, #84718, .T. ) ;
#129372 = ORIENTED_EDGE ( 'NONE', *, *, #84434, .T. ) ;
#129373 = CARTESIAN_POINT ( 'NONE',  ( 37.47959685856476142, 6.109999999999999432, 1.637169565754164280 ) ) ;
#129374 = ORIENTED_EDGE ( 'NONE', *, *, #36606, .T. ) ;
#129375 = CARTESIAN_POINT ( 'NONE',  ( 45.18749999999998579, -5.819803920172573974, 5.819803920172573086 ) ) ;
#129376 = ADVANCED_FACE ( 'NONE', ( #17989 ), #139845, .T. ) ;
#129377 = EDGE_CURVE ( 'NONE', #68934, #48693, #1285, .T. ) ;
#129378 = CARTESIAN_POINT ( 'NONE',  ( 26.14997294953710139, -4.461849672132299105, 4.461849672132299993 ) ) ;
#129379 = CARTESIAN_POINT ( 'NONE',  ( 7.515903222916713311, 10.89581445352136946, -28.18232836037424605 ) ) ;
#129380 = VERTEX_POINT ( 'NONE', #1247 ) ;
#129381 = EDGE_CURVE ( 'NONE', #84436, #79777, #64391, .T. ) ;
#129382 = FACE_OUTER_BOUND ( 'NONE', #89075, .T. ) ;
#129383 = ORIENTED_EDGE ( 'NONE', *, *, #21387, .T. ) ;
#129384 = CARTESIAN_POINT ( 'NONE',  ( -21.64318742751725821, -20.24070752338407075, 21.22881796311207836 ) ) ;
#129385 = FACE_OUTER_BOUND ( 'NONE', #25240, .T. ) ;
#129387 = ORIENTED_EDGE ( 'NONE', *, *, #24513, .T. ) ;
#129386 = DIRECTION ( 'NONE',  ( -0.7071067811865487940, 0.7071067811865463515, 0.000000000000000000 ) ) ;
#129388 = ORIENTED_EDGE ( 'NONE', *, *, #134725, .F. ) ;
#129389 = LINE ( 'NONE', #76477, #93173 ) ;
#129390 = CARTESIAN_POINT ( 'NONE',  ( -25.11017322888192993, -22.22500000000000142, 4.785647885939352086 ) ) ;
#129391 = ADVANCED_FACE ( 'NONE', ( #86870 ), #31768, .T. ) ;
#129392 = ORIENTED_EDGE ( 'NONE', *, *, #85085, .F. ) ;
#129393 = PLANE ( 'NONE',  #101366 ) ;
#129394 = ORIENTED_EDGE ( 'NONE', *, *, #5595, .F. ) ;
#129395 = AXIS2_PLACEMENT_3D ( 'NONE', #63833, #30480, #86297 ) ;
#129396 = ORIENTED_EDGE ( 'NONE', *, *, #14352, .T. ) ;
#129397 = EDGE_LOOP ( 'NONE', ( #127530, #49626, #11388, #49214 ) ) ;
#129398 = DIRECTION ( 'NONE',  ( 1.000000000000000000, 0.000000000000000000, 0.000000000000000000 ) ) ;
#129399 = AXIS2_PLACEMENT_3D ( 'NONE', #66070, #10220, #55906 ) ;
#129401 = EDGE_CURVE ( 'NONE', #125809, #119594, #88299, .T. ) ;
#129400 = VECTOR ( 'NONE', #72907, 1000.000000000000000 ) ;
#129402 = VECTOR ( 'NONE', #4730, 1000.000000000000227 ) ;
#129403 = COLOUR_RGB ( '', 0.08235294, 0.09019608, 0.10196078) ;
#129404 = CARTESIAN_POINT ( 'NONE',  ( 8.999999999999937828, -10.44781430457071991, 5.000000000000000000 ) ) ;
#129405 = DIRECTION ( 'NONE',  ( 0.3543493200069162685, -0.000000000000000000, -0.9351131265310288487 ) ) ;
#129406 = VECTOR ( 'NONE', #59492, 1000.000000000000000 ) ;
#129407 = LINE ( 'NONE', #96058, #44845 ) ;
#129408 = LINE ( 'NONE', #110494, #46100 ) ;
#129409 = VERTEX_POINT ( 'NONE', #34621 ) ;
#129410 = DIRECTION ( 'NONE',  ( 0.7071067811865487940, 0.7071067811865463515, 0.000000000000000000 ) ) ;
#129411 = ORIENTED_EDGE ( 'NONE', *, *, #11241, .T. ) ;
#129412 = ADVANCED_FACE ( 'NONE', ( #131080 ), #119454, .F. ) ;
#129413 = VECTOR ( 'NONE', #62427, 1000.000000000000000 ) ;
#129414 = CARTESIAN_POINT ( 'NONE',  ( 13.49999999999990763, -5.947814304570766986, 5.000000000000000000 ) ) ;
#129415 = CARTESIAN_POINT ( 'NONE',  ( 29.87456980810189222, 6.871911579029510442, -3.967499999999998916 ) ) ;
#129416 = ORIENTED_EDGE ( 'NONE', *, *, #16644, .T. ) ;
#129417 = CARTESIAN_POINT ( 'NONE',  ( -26.99451991528749417, 28.92564299267956685, 4.000000000000000000 ) ) ;
#129418 = DIRECTION ( 'NONE',  ( 0.7071067811865487940, 0.7071067811865463515, 0.000000000000000000 ) ) ;
#129419 = ORIENTED_EDGE ( 'NONE', *, *, #96108, .F. ) ;
#129420 = ORIENTED_EDGE ( 'NONE', *, *, #4841, .T. ) ;
#129421 = EDGE_CURVE ( 'NONE', #27623, #22382, #53523, .T. ) ;
#129422 = CARTESIAN_POINT ( 'NONE',  ( 63.18398860626900415, 28.73617430169831621, 5.000000000000000000 ) ) ;
#129423 = CARTESIAN_POINT ( 'NONE',  ( 94.28752705046289861, 0.000000000000000000, -7.949999999999998401 ) ) ;
#129424 = CARTESIAN_POINT ( 'NONE',  ( 0.000000000000000000, 0.000000000000000000, 5.000000000000000000 ) ) ;
#129425 = VECTOR ( 'NONE', #108008, 1000.000000000000114 ) ;
#129426 = AXIS2_PLACEMENT_3D ( 'NONE', #37497, #7504, #62636 ) ;
#129427 = CARTESIAN_POINT ( 'NONE',  ( 5.207106781186507050, 9.759292476615614831, 5.000000000000000000 ) ) ;
#129428 = CARTESIAN_POINT ( 'NONE',  ( 0.6130698085681498544, -49.19053253528764458, -40.77637019027829979 ) ) ;
#129429 = CARTESIAN_POINT ( 'NONE',  ( 67.72459685856478018, -1.637169565754161171, 6.109999999999998543 ) ) ;
#129430 = DIRECTION ( 'NONE',  ( 0.3543493200069162685, -0.000000000000000000, -0.9351131265310288487 ) ) ;
#129431 = ADVANCED_FACE ( 'NONE', ( #32488 ), #10688, .T. ) ;
#129432 = COLOUR_RGB ( '', 0.66274510, 0.83137255, 0.94901961) ;
#129433 = CARTESIAN_POINT ( 'NONE',  ( 9.279999999999999361, 2.055000000000001492, 2.516649172247811554E-16 ) ) ;
#129434 = LINE ( 'NONE', #139648, #118420 ) ;
#129435 = EDGE_CURVE ( 'NONE', #38928, #19893, #76727, .T. ) ;
#129436 = ORIENTED_EDGE ( 'NONE', *, *, #22688, .T. ) ;
#129437 = LINE ( 'NONE', #30123, #25623 ) ;
#129438 = ORIENTED_EDGE ( 'NONE', *, *, #4728, .F. ) ;
#129439 = LINE ( 'NONE', #4202, #33152 ) ;
#129440 = PLANE ( 'NONE',  #47639 ) ;
#129441 = ORIENTED_EDGE ( 'NONE', *, *, #57587, .F. ) ;
#129442 = VECTOR ( 'NONE', #51061, 1000.000000000000000 ) ;
#129444 = EDGE_CURVE ( 'NONE', #76266, #139011, #110714, .T. ) ;
#129443 = VECTOR ( 'NONE', #86681, 1000.000000000000114 ) ;
#129445 = AXIS2_PLACEMENT_3D ( 'NONE', #63670, #107829, #34588 ) ;
#129446 = CARTESIAN_POINT ( 'NONE',  ( -66.18398860626901126, 28.73617430169833753, 5.000000000000000000 ) ) ;
#129447 = VERTEX_POINT ( 'NONE', #21606 ) ;
#129448 = CARTESIAN_POINT ( 'NONE',  ( 12.48921356237309155, -27.52281430457064104, 5.000000000000000000 ) ) ;
#129449 = LINE ( 'NONE', #118572, #90363 ) ;
#129450 = DIRECTION ( 'NONE',  ( -0.7071067811865486830, -0.7071067811865464625, -0.000000000000000000 ) ) ;
#129451 = VERTEX_POINT ( 'NONE', #65133 ) ;
#129452 = ORIENTED_EDGE ( 'NONE', *, *, #26546, .T. ) ;
#129453 = DIRECTION ( 'NONE',  ( -0.000000000000000000, 0.3543493200069153248, 0.9351131265310292928 ) ) ;
#129454 = VECTOR ( 'NONE', #91835, 1000.000000000000000 ) ;
#129455 = AXIS2_PLACEMENT_3D ( 'NONE', #121395, #54743, #77227 ) ;
#129456 = CARTESIAN_POINT ( 'NONE',  ( -5.671830600776429421, 11.25929247661560240, 4.000000000000000000 ) ) ;
#129457 = CARTESIAN_POINT ( 'NONE',  ( 96.47502705046288440, -5.819803920172572198, 5.819803920172572198 ) ) ;
#129458 = CARTESIAN_POINT ( 'NONE',  ( 12.79289321881337038, -20.24070752338407431, 5.000000000000000000 ) ) ;
#129459 = PLANE ( 'NONE',  #120087 ) ;
#129460 = EDGE_LOOP ( 'NONE', ( #34484, #65658, #47050 ) ) ;
#129461 = EDGE_CURVE ( 'NONE', #39821, #50567, #54269, .T. ) ;
#129462 = CARTESIAN_POINT ( 'NONE',  ( 0.000000000000000000, 9.735942053221458872E-16, -7.950000000000000178 ) ) ;
#129463 = CARTESIAN_POINT ( 'NONE',  ( -14.81601139373099585, 28.73617430169776910, 5.000000000000000000 ) ) ;
#129464 = CARTESIAN_POINT ( 'NONE',  ( 34.27083333333333570, 6.094999999999991758, 1.633150327867687102 ) ) ;
#129465 = VECTOR ( 'NONE', #56007, 1000.000000000000000 ) ;
#129466 = CARTESIAN_POINT ( 'NONE',  ( 20.25795612380215971, -2.670494247963030698, 4.000000000000000000 ) ) ;
#129467 = ORIENTED_EDGE ( 'NONE', *, *, #11999, .T. ) ;
#129468 = EDGE_CURVE ( 'NONE', #89471, #46947, #78139, .T. ) ;
#129469 = DIRECTION ( 'NONE',  ( 0.7071067811865487940, 0.7071067811865463515, 0.000000000000000000 ) ) ;
#129470 = VERTEX_POINT ( 'NONE', #44079 ) ;
#129471 = CARTESIAN_POINT ( 'NONE',  ( 70.87543019189810423, -5.291415217122920289, -3.055000000000001492 ) ) ;
#129472 = DIRECTION ( 'NONE',  ( 0.6830127018922180770, -0.6830127018922204085, -0.2588190451025213501 ) ) ;
#129473 = DIRECTION ( 'NONE',  ( 0.3543493200069162685, -0.000000000000000000, -0.9351131265310288487 ) ) ;
#129474 = ORIENTED_EDGE ( 'NONE', *, *, #20401, .T. ) ;
#129475 = CARTESIAN_POINT ( 'NONE',  ( 160.0000000000000000, 6.349999999999997868, 0.000000000000000000 ) ) ;
#129476 = LINE ( 'NONE', #42511, #46588 ) ;
#129477 = LINE ( 'NONE', #30169, #115736 ) ;
#129479 = ORIENTED_EDGE ( 'NONE', *, *, #7285, .T. ) ;
#129478 = DIRECTION ( 'NONE',  ( -0.7071067811865487940, 0.7071067811865463515, -0.000000000000000000 ) ) ;
#129480 = LINE ( 'NONE', #95430, #69244 ) ;
#129481 = LINE ( 'NONE', #141070, #12897 ) ;
#129482 = DIRECTION ( 'NONE',  ( -0.000000000000000000, 0.000000000000000000, 1.000000000000000000 ) ) ;
#129483 = FACE_OUTER_BOUND ( 'NONE', #44982, .T. ) ;
#129484 = ORIENTED_EDGE ( 'NONE', *, *, #127366, .T. ) ;
#129485 = EDGE_CURVE ( 'NONE', #132586, #65489, #132548, .T. ) ;
#129486 = ORIENTED_EDGE ( 'NONE', *, *, #1356, .F. ) ;
#129487 = CARTESIAN_POINT ( 'NONE',  ( 75.25043019189811844, 3.055000000000002824, -5.291415217122919401 ) ) ;
#129488 = VERTEX_POINT ( 'NONE', #121608 ) ;
#129489 = CARTESIAN_POINT ( 'NONE',  ( 17.99999999999987566, 19.55218569542897100, 5.000000000000000000 ) ) ;
#129490 = CARTESIAN_POINT ( 'NONE',  ( 14.27159235450332098, 9.902892378096218942E-16, 0.000000000000000000 ) ) ;
#129491 = CARTESIAN_POINT ( 'NONE',  ( 20.77868544475317947, 8.889383937919465239, 4.212719859983347526 ) ) ;
#129492 = LINE ( 'NONE', #110583, #33933 ) ;
#129493 = ORIENTED_EDGE ( 'NONE', *, *, #107462, .F. ) ;
#129494 = DIRECTION ( 'NONE',  ( 0.6830127018922180770, -0.6830127018922204085, -0.2588190451025213501 ) ) ;
#129495 = VERTEX_POINT ( 'NONE', #22276 ) ;
#129496 = CARTESIAN_POINT ( 'NONE',  ( 0.3440661715655736752, -1.278132184730745857, 3.986082177731342657 ) ) ;
#129497 = CARTESIAN_POINT ( 'NONE',  ( -34.92499999999997584, -21.76999999999999247, -40.00000000000000000 ) ) ;
#129498 = DIRECTION ( 'NONE',  ( -1.000000000000000000, 0.000000000000000000, 0.000000000000000000 ) ) ;
#129499 = COLOUR_RGB ( '', 0.66274510, 0.83137255, 0.94901961) ;
#129500 = AXIS2_PLACEMENT_3D ( 'NONE', #29642, #118056, #19495 ) ;
#129501 = EDGE_LOOP ( 'NONE', ( #106337, #52700, #17944, #64448 ) ) ;
#129502 = VERTEX_POINT ( 'NONE', #55673 ) ;
#129503 = VECTOR ( 'NONE', #69483, 1000.000000000000000 ) ;
#129504 = DIRECTION ( 'NONE',  ( -0.000000000000000000, -0.3543493200069152693, 0.9351131265310292928 ) ) ;
#129505 = CARTESIAN_POINT ( 'NONE',  ( 180.9587832221920110, -48.83231052142031814, 38.98973348322100918 ) ) ;
#129506 = CARTESIAN_POINT ( 'NONE',  ( 12.48921356237309155, -27.52281430457064104, 5.000000000000000000 ) ) ;
#129507 = FILL_AREA_STYLE_COLOUR ( '', #37421 ) ;
#129508 = AXIS2_PLACEMENT_3D ( 'NONE', #16567, #28187, #114461 ) ;
#129509 = DIRECTION ( 'NONE',  ( -0.7071067811865486830, -0.7071067811865464625, 0.000000000000000000 ) ) ;
#129510 = FACE_OUTER_BOUND ( 'NONE', #3401, .T. ) ;
#129511 = FILL_AREA_STYLE_COLOUR ( '', #33112 ) ;
#129512 = VERTEX_POINT ( 'NONE', #99873 ) ;
#129513 = VECTOR ( 'NONE', #126058, 1000.000000000000227 ) ;
#129514 = VERTEX_POINT ( 'NONE', #539 ) ;
#129515 = VERTEX_POINT ( 'NONE', #44834 ) ;
#129516 = VERTEX_POINT ( 'NONE', #89024 ) ;
#129517 = VECTOR ( 'NONE', #6361, 1000.000000000000000 ) ;
#129518 = VECTOR ( 'NONE', #110382, 999.9999999999998863 ) ;
#129519 = CARTESIAN_POINT ( 'NONE',  ( 183.6085471140771403, -52.10163751122425424, 40.43817685074128576 ) ) ;
#129520 = DIRECTION ( 'NONE',  ( 1.000000000000000000, 0.000000000000000000, 0.000000000000000000 ) ) ;
#129521 = CIRCLE ( 'NONE', #104053, 2.500000000000000444 ) ;
#129522 = DIRECTION ( 'NONE',  ( 0.7071067811865486830, -0.7071067811865464625, -0.000000000000000000 ) ) ;
#129523 = VERTEX_POINT ( 'NONE', #22986 ) ;
#129524 = CARTESIAN_POINT ( 'NONE',  ( 19.17183060077633883, 15.75929247661555976, 4.000000000000000000 ) ) ;
#129525 = CARTESIAN_POINT ( 'NONE',  ( 10.77958563595370833, -2.500000000000000000, 3.061616997868383634E-16 ) ) ;
#129527 = EDGE_CURVE ( 'NONE', #18713, #82210, #102214, .T. ) ;
#129526 = LINE ( 'NONE', #73059, #112823 ) ;
#129528 = FACE_OUTER_BOUND ( 'NONE', #127027, .T. ) ;
#129529 = VECTOR ( 'NONE', #97963, 1000.000000000000000 ) ;
#129530 = DIRECTION ( 'NONE',  ( 0.7071067811865487940, 0.7071067811865463515, -0.000000000000000000 ) ) ;
#129531 = ORIENTED_EDGE ( 'NONE', *, *, #57651, .F. ) ;
#129532 = VECTOR ( 'NONE', #114649, 1000.000000000000000 ) ;
#129533 = CARTESIAN_POINT ( 'NONE',  ( 17.27718569542927796, -21.72500000000000142, 5.000000000000000000 ) ) ;
#129534 = CARTESIAN_POINT ( 'NONE',  ( 9.994118527364397764, 0.000000000000000000, 2.500000000000000444 ) ) ;
#129535 = AXIS2_PLACEMENT_3D ( 'NONE', #69754, #3698, #327 ) ;
#129536 = VERTEX_POINT ( 'NONE', #67257 ) ;
#129537 = CARTESIAN_POINT ( 'NONE',  ( -48.29974487139158867, -27.71228299555239971, 4.000000000000000000 ) ) ;
#129538 = ORIENTED_EDGE ( 'NONE', *, *, #71564, .F. ) ;
#129539 = ADVANCED_FACE ( 'NONE', ( #56421 ), #100604, .F. ) ;
#129540 = EDGE_CURVE ( 'NONE', #129197, #2861, #123069, .T. ) ;
#129541 = FACE_OUTER_BOUND ( 'NONE', #73737, .T. ) ;
#129542 = ORIENTED_EDGE ( 'NONE', *, *, #136579, .F. ) ;
#129544 = AXIS2_PLACEMENT_3D ( 'NONE', #137340, #72839, #17660 ) ;
#129543 = CARTESIAN_POINT ( 'NONE',  ( 65.18793019189811844, 6.110000000000002984, -1.637169565754156730 ) ) ;
#129545 = ORIENTED_EDGE ( 'NONE', *, *, #106837, .F. ) ;
#129546 = ORIENTED_EDGE ( 'NONE', *, *, #54549, .T. ) ;
#129547 = ADVANCED_FACE ( 'NONE', ( #59266 ), #1937, .F. ) ;
#129548 = EDGE_CURVE ( 'NONE', #12163, #60612, #137512, .T. ) ;
#129549 = LINE ( 'NONE', #139756, #18794 ) ;
#129551 = ADVANCED_FACE ( 'NONE', ( #70155 ), #134672, .F. ) ;
#129550 = FACE_OUTER_BOUND ( 'NONE', #95557, .T. ) ;
#129552 = CARTESIAN_POINT ( 'NONE',  ( 95.66709685856477563, -3.055000000000000160, -5.291415217122921177 ) ) ;
#129553 = CARTESIAN_POINT ( 'NONE',  ( -34.42500000000001137, 7.541399257801932876, 5.000000000000000000 ) ) ;
#129554 = EDGE_CURVE ( 'NONE', #25495, #131632, #48350, .T. ) ;
#129555 = LINE ( 'NONE', #95499, #51355 ) ;
#129556 = PLANE ( 'NONE',  #81106 ) ;
#129557 = AXIS2_PLACEMENT_3D ( 'NONE', #107691, #9811, #141034 ) ;
#129558 = DIRECTION ( 'NONE',  ( -0.7071067811865486830, -0.7071067811865464625, 0.000000000000000000 ) ) ;
#129559 = EDGE_CURVE ( 'NONE', #28420, #7787, #78860, .T. ) ;
#129560 = FACE_OUTER_BOUND ( 'NONE', #77843, .T. ) ;
#129561 = FACE_OUTER_BOUND ( 'NONE', #9429, .T. ) ;
#129562 = CARTESIAN_POINT ( 'NONE',  ( 48.18398860626899705, 28.73617430169820608, 5.000000000000000000 ) ) ;
#129563 = EDGE_CURVE ( 'NONE', #101765, #121732, #76767, .T. ) ;
#129564 = ORIENTED_EDGE ( 'NONE', *, *, #138720, .T. ) ;
#129565 = ADVANCED_BREP_SHAPE_REPRESENTATION ( '', ( #92605, #127880 ), #130349 ) ;
#129566 = ORIENTED_EDGE ( 'NONE', *, *, #68285, .T. ) ;
#129567 = EDGE_LOOP ( 'NONE', ( #106596, #1323, #63626, #50909 ) ) ;
#129568 = ORIENTED_EDGE ( 'NONE', *, *, #66299, .T. ) ;
#129569 = VERTEX_POINT ( 'NONE', #79609 ) ;
#129570 = DIRECTION ( 'NONE',  ( -0.7071067811865486830, -0.7071067811865464625, -0.000000000000000000 ) ) ;
#129571 = CARTESIAN_POINT ( 'NONE',  ( -54.29974487139159578, -27.71228299555243879, 4.000000000000000000 ) ) ;
#129572 = EDGE_CURVE ( 'NONE', #138304, #104351, #112887, .T. ) ;
#129573 = DIRECTION ( 'NONE',  ( 0.000000000000000000, 0.000000000000000000, 1.000000000000000000 ) ) ;
#129574 = VERTEX_POINT ( 'NONE', #92539 ) ;
#129575 = CARTESIAN_POINT ( 'NONE',  ( 0.000000000000000000, -14.29000000000013593, -12.70000000000045404 ) ) ;
#129576 = VERTEX_POINT ( 'NONE', #113591 ) ;
#129577 = ADVANCED_FACE ( 'NONE', ( #136067 ), #103419, .T. ) ;
#129578 = CARTESIAN_POINT ( 'NONE',  ( 5.666236474768552078, 7.934999999999990727, -1.457635852685135314E-15 ) ) ;
#129579 = CARTESIAN_POINT ( 'NONE',  ( 31.92500000000001492, -6.269999999999992468, -37.00000000000000000 ) ) ;
#129580 = CARTESIAN_POINT ( 'NONE',  ( 51.48921356237309510, -27.52281430457091460, 5.000000000000000000 ) ) ;
#129581 = EDGE_LOOP ( 'NONE', ( #54116, #28174, #19133, #118821, #84139, #126226 ) ) ;
#129582 = EDGE_LOOP ( 'NONE', ( #24269, #132545, #103324, #43126 ) ) ;
#129584 = ORIENTED_EDGE ( 'NONE', *, *, #37156, .F. ) ;
#129583 = ADVANCED_FACE ( 'NONE', ( #36067 ), #80991, .F. ) ;
#129585 = DIRECTION ( 'NONE',  ( -1.000000000000000000, -1.224606353822377258E-16, -0.000000000000000000 ) ) ;
#129586 = DIRECTION ( 'NONE',  ( 0.7071067811865487940, 0.7071067811865463515, 0.000000000000000000 ) ) ;
#129587 = DIRECTION ( 'NONE',  ( 0.7071067811865487940, 0.7071067811865463515, 0.000000000000000000 ) ) ;
#129588 = FACE_OUTER_BOUND ( 'NONE', #104563, .T. ) ;
#129589 = FACE_OUTER_BOUND ( 'NONE', #39625, .T. ) ;
#129590 = ADVANCED_FACE ( 'NONE', ( #58575 ), #80291, .F. ) ;
#129591 = FACE_OUTER_BOUND ( 'NONE', #79110, .T. ) ;
#129592 = CARTESIAN_POINT ( 'NONE',  ( 33.10459685856476852, 1.637169565754164946, -6.109999999999999432 ) ) ;
#129593 = CYLINDRICAL_SURFACE ( 'NONE', #90722, 2.247899999999996901 ) ;
#129594 = DIRECTION ( 'NONE',  ( 0.000000000000000000, 0.000000000000000000, 1.000000000000000000 ) ) ;
#129595 = EDGE_CURVE ( 'NONE', #3062, #84892, #49088, .T. ) ;
#129596 = ORIENTED_EDGE ( 'NONE', *, *, #116977, .T. ) ;
#129597 = DIRECTION ( 'NONE',  ( 0.000000000000000000, 0.000000000000000000, -1.000000000000000000 ) ) ;
#129598 = AXIS2_PLACEMENT_3D ( 'NONE', #67683, #111870, #56812 ) ;
#129599 = AXIS2_PLACEMENT_3D ( 'NONE', #2232, #121184, #134227 ) ;
#129600 = CIRCLE ( 'NONE', #67128, 5.968999999999998529 ) ;
#129601 = AXIS2_PLACEMENT_3D ( 'NONE', #68833, #2816, #123920 ) ;
#129602 = CARTESIAN_POINT ( 'NONE',  ( 33.48921356237309510, -27.52281430457078670, 5.000000000000000000 ) ) ;
#129603 = ORIENTED_EDGE ( 'NONE', *, *, #32806, .T. ) ;
#129605 = EDGE_CURVE ( 'NONE', #1952, #27121, #70842, .T. ) ;
#129604 =( BOUNDED_CURVE ( )  B_SPLINE_CURVE ( 3, ( #81124, #26719, #4918, #49215 ),
 .UNSPECIFIED., .F., .T. ) 
 B_SPLINE_CURVE_WITH_KNOTS ( ( 4, 4 ),
 ( 3.995629653766860301, 4.163580865291908850 ),
 .UNSPECIFIED. ) 
 CURVE ( )  GEOMETRIC_REPRESENTATION_ITEM ( )  RATIONAL_B_SPLINE_CURVE ( ( 1.000000000000000000, 0.9976507469244630943, 0.9976507469244630943, 1.000000000000000000 ) ) 
 REPRESENTATION_ITEM ( '' )  );
#129606 = EDGE_CURVE ( 'NONE', #90821, #32697, #15670, .T. ) ;
#129607 = AXIS2_PLACEMENT_3D ( 'NONE', #97442, #99576, #32958 ) ;
#129608 = CARTESIAN_POINT ( 'NONE',  ( -6.489213562373093325, -27.52281430457059841, 5.000000000000000000 ) ) ;
#129610 = ORIENTED_EDGE ( 'NONE', *, *, #57102, .T. ) ;
#129609 = CARTESIAN_POINT ( 'NONE',  ( 56.62524208092768419, -47.99115898044231443, -37.22402166429051817 ) ) ;
#129611 = DIRECTION ( 'NONE',  ( -0.7071067811865486830, 0.7071067811865464625, 0.000000000000000000 ) ) ;
#129612 = SURFACE_STYLE_USAGE ( .BOTH. , #63685 ) ;
#129613 = EDGE_LOOP ( 'NONE', ( #139266, #110498, #1475, #42169 ) ) ;
#129614 = DIRECTION ( 'NONE',  ( -0.7071067811865486830, -0.7071067811865464625, 0.000000000000000000 ) ) ;
#129615 = VECTOR ( 'NONE', #64222, 1000.000000000000000 ) ;
#129616 = ORIENTED_EDGE ( 'NONE', *, *, #40070, .T. ) ;
#129617 = DIRECTION ( 'NONE',  ( -0.6830127018922181881, 0.6830127018922202975, -0.2588190451025214056 ) ) ;
#129618 = CARTESIAN_POINT ( 'NONE',  ( 119.2250270504628986, 5.819803920172573086, -5.819803920172572198 ) ) ;
#129619 = CARTESIAN_POINT ( 'NONE',  ( 50.24586038379622011, 3.974999999999996980, 6.884901960086287964 ) ) ;
#129620 = CARTESIAN_POINT ( 'NONE',  ( 10.77958563595370833, 2.500000000000000444, 0.000000000000000000 ) ) ;
#129621 = EDGE_CURVE ( 'NONE', #133913, #37030, #23746, .T. ) ;
#129622 = DIRECTION ( 'NONE',  ( -0.6830127018922180770, -0.6830127018922204085, -0.2588190451025213501 ) ) ;
#129623 = CARTESIAN_POINT ( 'NONE',  ( 9.183988606268997046, 28.73617430169793607, 5.000000000000000000 ) ) ;
#129624 = CARTESIAN_POINT ( 'NONE',  ( 4.375000000000000000, -6.094999999999989981, 3.732111120401553285E-16 ) ) ;
#129626 = VECTOR ( 'NONE', #54440, 1000.000000000000000 ) ;
#129625 = CARTESIAN_POINT ( 'NONE',  ( 15.29123647476855297, -9.717572351234235426E-16, -7.934999999999990727 ) ) ;
#129627 = VECTOR ( 'NONE', #29854, 999.9999999999998863 ) ;
#129628 = CARTESIAN_POINT ( 'NONE',  ( 63.48921356237309510, -27.52281430457099631, 5.000000000000000000 ) ) ;
#129629 = DIRECTION ( 'NONE',  ( 0.7071067811865486830, -0.7071067811865464625, -0.000000000000000000 ) ) ;
#129630 = ORIENTED_EDGE ( 'NONE', *, *, #93280, .F. ) ;
#129631 = ORIENTED_EDGE ( 'NONE', *, *, #11820, .F. ) ;
#129632 = VECTOR ( 'NONE', #26442, 1000.000000000000000 ) ;
#129633 = CARTESIAN_POINT ( 'NONE',  ( 27.00000000000000355, 0.000000000000000000, 0.000000000000000000 ) ) ;
#129634 = ORIENTED_EDGE ( 'NONE', *, *, #31880, .F. ) ;
#129635 = EDGE_CURVE ( 'NONE', #38115, #139654, #12841, .T. ) ;
#129636 = DIRECTION ( 'NONE',  ( 0.6830127018922180770, -0.6830127018922204085, -0.2588190451025213501 ) ) ;
#129637 = DIRECTION ( 'NONE',  ( -1.000000000000000000, -0.000000000000000000, -0.000000000000000000 ) ) ;
#129638 = DIRECTION ( 'NONE',  ( -0.3543493200069162685, -0.000000000000000000, -0.9351131265310288487 ) ) ;
#129639 = FACE_OUTER_BOUND ( 'NONE', #73221, .T. ) ;
#129640 = ORIENTED_EDGE ( 'NONE', *, *, #90642, .T. ) ;
#129641 = CIRCLE ( 'NONE', #99516, 6.000000000000001776 ) ;
#129642 = DIRECTION ( 'NONE',  ( 0.7071067811865486830, -0.7071067811865464625, -0.000000000000000000 ) ) ;
#129643 = DIRECTION ( 'NONE',  ( -1.000000000000000000, -0.000000000000000000, -0.000000000000000000 ) ) ;
#129644 = CARTESIAN_POINT ( 'NONE',  ( 39.48921356237310221, -27.52281430457082934, 5.000000000000000000 ) ) ;
#129645 = EDGE_CURVE ( 'NONE', #82515, #100683, #117153, .T. ) ;
#129646 = AXIS2_PLACEMENT_3D ( 'NONE', #136095, #66575, #90460 ) ;
#129647 = LINE ( 'NONE', #7859, #33270 ) ;
#129649 = ORIENTED_EDGE ( 'NONE', *, *, #97458, .F. ) ;
#129648 = DIRECTION ( 'NONE',  ( 0.7071067811865487940, 0.7071067811865463515, 0.000000000000000000 ) ) ;
#129650 = CARTESIAN_POINT ( 'NONE',  ( 2.999999999999999112, -1.600000000000055600, -28.92500000000001492 ) ) ;
#129651 = VECTOR ( 'NONE', #138234, 1000.000000000000000 ) ;
#129652 =( LENGTH_UNIT ( ) NAMED_UNIT ( * ) SI_UNIT ( .MILLI., .METRE. ) );
#129653 = FACE_OUTER_BOUND ( 'NONE', #137291, .T. ) ;
#129654 = CARTESIAN_POINT ( 'NONE',  ( -68.99451991528748351, 28.92564299267986172, 4.000000000000000000 ) ) ;
#129655 = CARTESIAN_POINT ( 'NONE',  ( 17.99999999999987566, -10.77435723561694125, -9.972017380717273838 ) ) ;
#129656 = ORIENTED_EDGE ( 'NONE', *, *, #2911, .F. ) ;
#129657 = EDGE_LOOP ( 'NONE', ( #107711, #133558, #60392, #48212 ) ) ;
#129658 = ORIENTED_EDGE ( 'NONE', *, *, #139313, .F. ) ;
#129659 = CARTESIAN_POINT ( 'NONE',  ( 102.9587635252314470, 0.000000000000000000, -6.110000000000001208 ) ) ;
#129660 = MECHANICAL_DESIGN_GEOMETRIC_PRESENTATION_REPRESENTATION (  '', ( #27840 ), #55593 ) ;
#129661 = EDGE_LOOP ( 'NONE', ( #115103, #102177, #3270, #75454, #117412, #114315 ) ) ;
#129662 = CARTESIAN_POINT ( 'NONE',  ( 127.0485559394950457, -49.69743550128772824, 36.79359617903031676 ) ) ;
#129663 = VECTOR ( 'NONE', #42301, 1000.000000000000227 ) ;
#129664 = CARTESIAN_POINT ( 'NONE',  ( 11.20710678118647152, -20.24070752338407431, 5.000000000000000000 ) ) ;
#129665 = ORIENTED_EDGE ( 'NONE', *, *, #34650, .F. ) ;
#129666 = CARTESIAN_POINT ( 'NONE',  ( 74.50000000000000000, 0.000000000000000000, -7.950000000000000178 ) ) ;
#129668 = EDGE_CURVE ( 'NONE', #90821, #41872, #38904, .T. ) ;
#129667 = DIRECTION ( 'NONE',  ( 0.000000000000000000, -1.000000000000000000, -1.286409696682840916E-16 ) ) ;
#129669 = CARTESIAN_POINT ( 'NONE',  ( 99.07876352523145158, -7.482591942790325086E-16, 6.109999999999998543 ) ) ;
#129670 = EDGE_CURVE ( 'NONE', #91137, #3249, #41044, .T. ) ;
#129671 = VERTEX_POINT ( 'NONE', #17153 ) ;
#129672 = CARTESIAN_POINT ( 'NONE',  ( 6.489213562373093325, -27.52281430457059841, 5.000000000000000000 ) ) ;
#129673 = DIRECTION ( 'NONE',  ( 0.7071067811865487940, 0.7071067811865463515, 0.000000000000000000 ) ) ;
#129674 = CARTESIAN_POINT ( 'NONE',  ( 16.49999999999988987, 9.431123077392092213, 4.000000000000000000 ) ) ;
#129675 = AXIS2_PLACEMENT_3D ( 'NONE', #57393, #132097, #46545 ) ;
#129676 = DIRECTION ( 'NONE',  ( -0.000000000000000000, 0.3543493200069153248, 0.9351131265310292928 ) ) ;
#129677 = ORIENTED_EDGE ( 'NONE', *, *, #55938, .T. ) ;
#129678 = VERTEX_POINT ( 'NONE', #38205 ) ;
#129679 = VERTEX_POINT ( 'NONE', #128761 ) ;
#129680 = LINE ( 'NONE', #20191, #44584 ) ;
#129681 = ADVANCED_FACE ( 'NONE', ( #40359 ), #60702, .T. ) ;
#129682 = DIRECTION ( 'NONE',  ( -0.6830127018922181881, 0.6830127018922202975, -0.2588190451025214056 ) ) ;
#129683 = CARTESIAN_POINT ( 'NONE',  ( 20.19206980810188767, -7.934999999999990727, -2.126176841940955242 ) ) ;
#129684 = CARTESIAN_POINT ( 'NONE',  ( 22.75000000000000355, -7.464222240803106570E-16, -6.094999999999989981 ) ) ;
#129685 = SURFACE_STYLE_USAGE ( .BOTH. , #137012 ) ;
#129686 = EDGE_LOOP ( 'NONE', ( #124075, #43309, #120756, #42623 ) ) ;
#129687 = ORIENTED_EDGE ( 'NONE', *, *, #64760, .F. ) ;
#129688 = CARTESIAN_POINT ( 'NONE',  ( 39.48921356237310221, -27.52281430457082934, 5.000000000000000000 ) ) ;
#129689 = ORIENTED_EDGE ( 'NONE', *, *, #119384, .T. ) ;
#129690 = ORIENTED_EDGE ( 'NONE', *, *, #22626, .F. ) ;
#129691 = VECTOR ( 'NONE', #28881, 1000.000000000000000 ) ;
#129692 = STYLED_ITEM ( 'NONE', ( #16450 ), #116432 ) ;
#129693 = AXIS2_PLACEMENT_3D ( 'NONE', #127442, #28141, #139048 ) ;
#129694 = DIRECTION ( 'NONE',  ( -0.7071067811865486830, -0.7071067811865464625, 0.000000000000000000 ) ) ;
#129695 = FACE_OUTER_BOUND ( 'NONE', #102681, .T. ) ;
#129696 = ORIENTED_EDGE ( 'NONE', *, *, #70567, .F. ) ;
#129697 = CARTESIAN_POINT ( 'NONE',  ( 8.897059064271770623, 4.202752102959690472E-16, 0.000000000000000000 ) ) ;
#129698 = DIRECTION ( 'NONE',  ( 0.000000000000000000, 1.000000000000000000, 0.000000000000000000 ) ) ;
#129699 = EDGE_CURVE ( 'NONE', #106533, #117346, #6223, .T. ) ;
#129700 = CARTESIAN_POINT ( 'NONE',  ( -3.280019679894024875, 0.7592924766157104211, 14.27032725228008125 ) ) ;
#129701 = CARTESIAN_POINT ( 'NONE',  ( 60.48921356237309510, -27.52281430457097500, 5.000000000000000000 ) ) ;
#129702 = COLOUR_RGB ( '', 0.40784314, 0.44705882, 0.49803922) ;
#129703 = AXIS2_PLACEMENT_3D ( 'NONE', #65999, #55100, #31911 ) ;
#129704 = PRESENTATION_LAYER_ASSIGNMENT (  '', '', ( #37206 ) ) ;
#129705 = ORIENTED_EDGE ( 'NONE', *, *, #91884, .T. ) ;
#129706 = VECTOR ( 'NONE', #32413, 1000.000000000000000 ) ;
#129707 = FACE_OUTER_BOUND ( 'NONE', #57384, .T. ) ;
#129708 = CARTESIAN_POINT ( 'NONE',  ( 0.000000000000000000, 0.000000000000000000, 4.000000000000000000 ) ) ;
#129709 = VERTEX_POINT ( 'NONE', #82417 ) ;
#129710 = CARTESIAN_POINT ( 'NONE',  ( 25.40000000000000568, 3.273809073538042291, -7.239615486481085327 ) ) ;
#129711 = DIRECTION ( 'NONE',  ( 0.3543493200069162685, -0.000000000000000000, -0.9351131265310288487 ) ) ;
#129712 = FACE_OUTER_BOUND ( 'NONE', #17785, .T. ) ;
#129714 = ORIENTED_EDGE ( 'NONE', *, *, #136019, .T. ) ;
#129713 = EDGE_CURVE ( 'NONE', #73159, #44574, #96119, .T. ) ;
#129715 = DIRECTION ( 'NONE',  ( -0.7071067811865486830, -0.7071067811865464625, 0.000000000000000000 ) ) ;
#129716 = ORIENTED_EDGE ( 'NONE', *, *, #62506, .T. ) ;
#129717 = ORIENTED_EDGE ( 'NONE', *, *, #65306, .T. ) ;
#129718 = AXIS2_PLACEMENT_3D ( 'NONE', #119633, #76176, #21056 ) ;
#129719 = ORIENTED_EDGE ( 'NONE', *, *, #85898, .T. ) ;
#129720 = EDGE_CURVE ( 'NONE', #59677, #43567, #8370, .T. ) ;
#129721 = CARTESIAN_POINT ( 'NONE',  ( 26.59959685856477307, -6.109999999999997655, -1.637169565754160283 ) ) ;
#129722 = SURFACE_SIDE_STYLE ('',( #120240 ) ) ;
#129724 = ADVANCED_FACE ( 'NONE', ( #50498 ), #117851, .F. ) ;
#129723 = DIRECTION ( 'NONE',  ( 0.7071067811865487940, 0.7071067811865463515, 0.000000000000000000 ) ) ;
#129725 = CARTESIAN_POINT ( 'NONE',  ( 127.3129301918981042, -1.637169565754159617, -6.110000000000001208 ) ) ;
#129726 = CARTESIAN_POINT ( 'NONE',  ( 6.328169399223481761, -18.74070752338408852, 4.000000000000000000 ) ) ;
#129727 = EDGE_CURVE ( 'NONE', #71286, #31203, #138218, .T. ) ;
#129728 = LINE ( 'NONE', #106524, #133929 ) ;
#129729 = DIRECTION ( 'NONE',  ( -1.000000000000000000, -1.224606353822377258E-16, -0.000000000000000000 ) ) ;
#129730 = AXIS2_PLACEMENT_3D ( 'NONE', #63707, #63001, #7851 ) ;
#129731 = EDGE_CURVE ( 'NONE', #102139, #91497, #96534, .T. ) ;
#129732 = LINE ( 'NONE', #140604, #35409 ) ;
#129733 = VECTOR ( 'NONE', #125607, 1000.000000000000000 ) ;
#129734 = LINE ( 'NONE', #64488, #122287 ) ;
#129735 = VECTOR ( 'NONE', #134941, 1000.000000000000000 ) ;
#129736 = CARTESIAN_POINT ( 'NONE',  ( -29.99999999999978684, 13.55218569542902429, 5.000000000000000000 ) ) ;
#129737 = DIRECTION ( 'NONE',  ( -0.7071067811865487940, 0.7071067811865463515, -0.000000000000000000 ) ) ;
#129738 = EDGE_CURVE ( 'NONE', #132753, #8318, #116031, .T. ) ;
#129739 = VERTEX_POINT ( 'NONE', #73003 ) ;
#129740 = AXIS2_PLACEMENT_3D ( 'NONE', #46442, #55871, #45715 ) ;
#129741 = VERTEX_POINT ( 'NONE', #107003 ) ;
#129742 = ORIENTED_EDGE ( 'NONE', *, *, #16485, .F. ) ;
#129743 = ORIENTED_EDGE ( 'NONE', *, *, #132226, .T. ) ;
#129744 = FACE_OUTER_BOUND ( 'NONE', #51735, .T. ) ;
#129745 = ORIENTED_EDGE ( 'NONE', *, *, #11960, .F. ) ;
#129746 = CIRCLE ( 'NONE', #85764, 2.500000000000000888 ) ;
#129747 = ORIENTED_EDGE ( 'NONE', *, *, #99694, .F. ) ;
#129748 = LINE ( 'NONE', #40621, #116190 ) ;
#129749 = DIRECTION ( 'NONE',  ( -0.000000000000000000, 0.000000000000000000, 1.000000000000000000 ) ) ;
#129750 = EDGE_CURVE ( 'NONE', #28995, #116794, #6934, .T. ) ;
#129751 = EDGE_CURVE ( 'NONE', #83991, #18685, #51221, .T. ) ;
#129752 = AXIS2_PLACEMENT_3D ( 'NONE', #1203, #88251, #119410 ) ;
#129753 = CARTESIAN_POINT ( 'NONE',  ( -6.299744871391586898, -27.71228299555210484, 4.000000000000000000 ) ) ;
#129754 = ORIENTED_EDGE ( 'NONE', *, *, #98178, .F. ) ;
#129755 = LINE ( 'NONE', #9367, #141376 ) ;
#129756 = ORIENTED_EDGE ( 'NONE', *, *, #7281, .F. ) ;
#129757 = EDGE_CURVE ( 'NONE', #4199, #126328, #95416, .T. ) ;
#129758 = PLANE ( 'NONE',  #104652 ) ;
#129759 = DIRECTION ( 'NONE',  ( -0.7071067811865487940, 0.7071067811865463515, -0.000000000000000000 ) ) ;
#129760 = CARTESIAN_POINT ( 'NONE',  ( 14.21290314143522160, 3.967499999999992699, -6.871911579029513994 ) ) ;
#129761 = ORIENTED_EDGE ( 'NONE', *, *, #126139, .T. ) ;
#129762 = CARTESIAN_POINT ( 'NONE',  ( 92.80793019189812298, -6.109999999999999432, 1.637169565754158507 ) ) ;
#129763 = CARTESIAN_POINT ( 'NONE',  ( 0.000000000000000000, 0.000000000000000000, 6.750000000000000888 ) ) ;
#129764 = LINE ( 'NONE', #30465, #16598 ) ;
#129765 = LINE ( 'NONE', #33361, #11815 ) ;
#129766 = ORIENTED_EDGE ( 'NONE', *, *, #76253, .T. ) ;
#129767 = VERTEX_POINT ( 'NONE', #130935 ) ;
#129768 = DIRECTION ( 'NONE',  ( -0.000000000000000000, 0.000000000000000000, 1.000000000000000000 ) ) ;
#129769 = PRESENTATION_LAYER_ASSIGNMENT (  '', '', ( #14065 ) ) ;
#129770 = ORIENTED_EDGE ( 'NONE', *, *, #12373, .T. ) ;
#129771 = PLANE ( 'NONE',  #4541 ) ;
#129772 = CARTESIAN_POINT ( 'NONE',  ( -2.277185695429367662, -21.72499999999999432, 5.000000000000000000 ) ) ;
#129773 = FACE_OUTER_BOUND ( 'NONE', #27537, .T. ) ;
#129774 = DIRECTION ( 'NONE',  ( -0.6830127018922181881, 0.6830127018922202975, -0.2588190451025214056 ) ) ;
#129775 = CARTESIAN_POINT ( 'NONE',  ( 184.1499999999998067, -47.62213595499957819, -36.92499999999998295 ) ) ;
#129776 = ORIENTED_EDGE ( 'NONE', *, *, #93032, .F. ) ;
#129777 = DIRECTION ( 'NONE',  ( -0.6830127018922180770, -0.6830127018922204085, -0.2588190451025213501 ) ) ;
#129778 = CARTESIAN_POINT ( 'NONE',  ( -20.99451991528748707, 28.92564299267952777, 4.000000000000000000 ) ) ;
#129779 = DIRECTION ( 'NONE',  ( 0.000000000000000000, 0.000000000000000000, 1.000000000000000000 ) ) ;
#129780 = ADVANCED_FACE ( 'NONE', ( #109866 ), #142517, .T. ) ;
#129781 = ORIENTED_EDGE ( 'NONE', *, *, #99435, .F. ) ;
#129782 = CARTESIAN_POINT ( 'NONE',  ( -12.29974487139158512, -27.71228299555214747, 4.000000000000000000 ) ) ;
#129783 = VECTOR ( 'NONE', #83416, 999.9999999999998863 ) ;
#129784 = DIRECTION ( 'NONE',  ( -0.3543493200069162685, -0.000000000000000000, -0.9351131265310288487 ) ) ;
#129785 = ORIENTED_EDGE ( 'NONE', *, *, #91007, .F. ) ;
#129787 = ORIENTED_EDGE ( 'NONE', *, *, #103126, .T. ) ;
#129786 = PLANE ( 'NONE',  #106498 ) ;
#129788 = EDGE_LOOP ( 'NONE', ( #18127, #89274, #13587, #97488 ) ) ;
#129789 = LINE ( 'NONE', #141384, #16969 ) ;
#129790 = FACE_OUTER_BOUND ( 'NONE', #59340, .T. ) ;
#129792 = ORIENTED_EDGE ( 'NONE', *, *, #133421, .T. ) ;
#129791 = AXIS2_PLACEMENT_3D ( 'NONE', #13360, #111251, #90972 ) ;
#129793 = FACE_OUTER_BOUND ( 'NONE', #18470, .T. ) ;
#129794 = VECTOR ( 'NONE', #130516, 1000.000000000000000 ) ;
#129795 = EDGE_CURVE ( 'NONE', #107648, #58396, #121449, .T. ) ;
#129796 = CARTESIAN_POINT ( 'NONE',  ( -8.590119451170131981, -22.22500000000000142, -4.979270689482284240 ) ) ;
#129797 = DIRECTION ( 'NONE',  ( 0.7071067811865487940, 0.7071067811865463515, 0.000000000000000000 ) ) ;
#129798 = DIRECTION ( 'NONE',  ( 0.000000000000000000, -1.000000000000000000, 0.000000000000000000 ) ) ;
#129799 = CARTESIAN_POINT ( 'NONE',  ( 0.1600000000000005862, -5.232655156125630924, -5.974607078898705126 ) ) ;
#129800 = EDGE_CURVE ( 'NONE', #29397, #4732, #120731, .T. ) ;
#129801 = CARTESIAN_POINT ( 'NONE',  ( -8.999999999999941380, 2.342191155542440395, -5.001666872980064404 ) ) ;
#129802 = CARTESIAN_POINT ( 'NONE',  ( 46.79166666666666430, 3.975000000000003642, -6.884901960086285300 ) ) ;
#129803 = PLANE ( 'NONE',  #102125 ) ;
#129804 = CARTESIAN_POINT ( 'NONE',  ( 8.282422613574265569, -21.73023691814493219, 5.000000000000000888 ) ) ;
#129805 = FACE_OUTER_BOUND ( 'NONE', #111058, .T. ) ;
#129806 = LINE ( 'NONE', #77601, #64568 ) ;
#129807 = CIRCLE ( 'NONE', #127421, 2.500000000000000888 ) ;
#129808 = LINE ( 'NONE', #75447, #11754 ) ;
#129809 = PLANE ( 'NONE',  #31564 ) ;
#129810 = ORIENTED_EDGE ( 'NONE', *, *, #58193, .F. ) ;
#129811 = ORIENTED_EDGE ( 'NONE', *, *, #89094, .F. ) ;
#129812 = ORIENTED_EDGE ( 'NONE', *, *, #54489, .T. ) ;
#129813 = CIRCLE ( 'NONE', #25591, 2.500000000000002220 ) ;
#129814 = CARTESIAN_POINT ( 'NONE',  ( 108.7708333333333286, -7.949999999999999289, -2.130196079827426203 ) ) ;
#129815 = AXIS2_PLACEMENT_3D ( 'NONE', #33622, #66941, #12541 ) ;
#129816 = ORIENTED_EDGE ( 'NONE', *, *, #117503, .F. ) ;
#129817 = EDGE_LOOP ( 'NONE', ( #139900, #83653, #139943, #98080 ) ) ;
#129818 = EDGE_CURVE ( 'NONE', #8776, #95615, #30597, .T. ) ;
#129819 = VERTEX_POINT ( 'NONE', #33069 ) ;
#129820 = DIRECTION ( 'NONE',  ( -0.7071067811865486830, -0.7071067811865464625, 0.000000000000000000 ) ) ;
#129821 = CARTESIAN_POINT ( 'NONE',  ( 89.08333333333332860, 6.884901960086290629, -3.974999999999994316 ) ) ;
#129822 = AXIS2_PLACEMENT_3D ( 'NONE', #75589, #96571, #19760 ) ;
#129823 =( GEOMETRIC_REPRESENTATION_CONTEXT ( 3 ) GLOBAL_UNCERTAINTY_ASSIGNED_CONTEXT ( ( #22943 ) ) GLOBAL_UNIT_ASSIGNED_CONTEXT ( ( #114451, #15120, #23897 ) ) REPRESENTATION_CONTEXT ( 'NONE', 'WORKASPACE' ) );
#129824 = AXIS2_PLACEMENT_3D ( 'NONE', #116585, #94104, #138345 ) ;
#129825 = VECTOR ( 'NONE', #10487, 1000.000000000000000 ) ;
#129826 = ORIENTED_EDGE ( 'NONE', *, *, #22985, .F. ) ;
#129827 = LINE ( 'NONE', #76912, #69455 ) ;
#129828 = MECHANICAL_DESIGN_GEOMETRIC_PRESENTATION_REPRESENTATION (  '', ( #9438 ), #122895 ) ;
#129829 = CARTESIAN_POINT ( 'NONE',  ( -19.49999999999986500, -10.04351517176479192, -1.623559851933870757 ) ) ;
#129830 = DIRECTION ( 'NONE',  ( -0.000000000000000000, -0.3543493200069152693, 0.9351131265310292928 ) ) ;
#129831 = DIRECTION ( 'NONE',  ( -0.000000000000000000, 0.000000000000000000, 1.000000000000000000 ) ) ;
#129832 = CARTESIAN_POINT ( 'NONE',  ( 103.3962635252314328, 4.472830434245840259, -4.472830434245839371 ) ) ;
#129833 = EDGE_CURVE ( 'NONE', #96844, #126104, #11228, .T. ) ;
#129834 = ORIENTED_EDGE ( 'NONE', *, *, #96381, .F. ) ;
#129835 = LINE ( 'NONE', #30538, #51120 ) ;
#129836 = CARTESIAN_POINT ( 'NONE',  ( -2.999999999999975131, -6.108550654416966097, -3.114665004254973280 ) ) ;
#129837 = VECTOR ( 'NONE', #123804, 1000.000000000000000 ) ;
#129838 = LINE ( 'NONE', #53726, #130358 ) ;
#129839 = CARTESIAN_POINT ( 'NONE',  ( 11.30840764549667554, 9.139736423841732040E-16, 0.000000000000000000 ) ) ;
#129840 = DIRECTION ( 'NONE',  ( 0.6830127018922180770, -0.6830127018922204085, -0.2588190451025213501 ) ) ;
#129841 = CARTESIAN_POINT ( 'NONE',  ( -36.48921356237310221, -27.52281430457080802, 5.000000000000000000 ) ) ;
#129842 = DIRECTION ( 'NONE',  ( 0.3543493200069162685, -0.000000000000000000, -0.9351131265310288487 ) ) ;
#129843 = LINE ( 'NONE', #19648, #72362 ) ;
#129844 = ORIENTED_EDGE ( 'NONE', *, *, #101061, .T. ) ;
#129845 = ORIENTED_EDGE ( 'NONE', *, *, #46790, .F. ) ;
#129846 = CARTESIAN_POINT ( 'NONE',  ( 31.47916666666665364, -7.950000000000001066, 2.130196079827424427 ) ) ;
#129847 = EDGE_LOOP ( 'NONE', ( #94669, #117822, #124752, #128432 ) ) ;
#129848 = VECTOR ( 'NONE', #79113, 1000.000000000000000 ) ;
#129849 = CARTESIAN_POINT ( 'NONE',  ( -48.48921356237309510, -27.52281430457089328, 5.000000000000000000 ) ) ;
#129850 = AXIS2_PLACEMENT_3D ( 'NONE', #12103, #22249, #68666 ) ;
#129851 = CARTESIAN_POINT ( 'NONE',  ( -29.99999999999979039, -13.06887692260767331, 4.000000000000000000 ) ) ;
#129852 = FACE_OUTER_BOUND ( 'NONE', #104437, .T. ) ;
#129853 = CARTESIAN_POINT ( 'NONE',  ( -22.49999999999984013, -7.533600742197664069, 5.000000000000000000 ) ) ;
#129854 = CARTESIAN_POINT ( 'NONE',  ( -2.510786437626908008, -27.52281430457053446, 5.000000000000000000 ) ) ;
#129855 = MECHANICAL_DESIGN_GEOMETRIC_PRESENTATION_REPRESENTATION (  '', ( #113699 ), #51220 ) ;
#129856 = VECTOR ( 'NONE', #54631, 1000.000000000000000 ) ;
#129857 = CARTESIAN_POINT ( 'NONE',  ( 126.6412635252314516, 4.472830434245836706, 4.472830434245840259 ) ) ;
#129858 = EDGE_CURVE ( 'NONE', #130889, #13355, #64956, .T. ) ;
#129859 = EDGE_LOOP ( 'NONE', ( #102803, #51023, #34914, #32846 ) ) ;
#129860 = VECTOR ( 'NONE', #17231, 1000.000000000000000 ) ;
#129861 = DIRECTION ( 'NONE',  ( 0.7071067811865486830, -0.7071067811865464625, -0.000000000000000000 ) ) ;
#129862 = ORIENTED_EDGE ( 'NONE', *, *, #10926, .F. ) ;
#129863 = DIRECTION ( 'NONE',  ( -0.000000000000000000, -0.3543493200069152693, 0.9351131265310292928 ) ) ;
#129864 = VECTOR ( 'NONE', #34978, 1000.000000000000000 ) ;
#129865 = DIRECTION ( 'NONE',  ( 0.7071067811865487940, 0.7071067811865463515, 0.000000000000000000 ) ) ;
#129866 = FACE_OUTER_BOUND ( 'NONE', #34373, .T. ) ;
#129867 = CARTESIAN_POINT ( 'NONE',  ( -14.29289321881336505, -0.7407075233842874695, 5.000000000000000000 ) ) ;
#129868 = ORIENTED_EDGE ( 'NONE', *, *, #57047, .F. ) ;
#129869 = CARTESIAN_POINT ( 'NONE',  ( 43.75043019189810423, 3.055000000000002824, -5.291415217122919401 ) ) ;
#129870 = ORIENTED_EDGE ( 'NONE', *, *, #11969, .F. ) ;
#129871 = VECTOR ( 'NONE', #56209, 999.9999999999998863 ) ;
#129872 = CARTESIAN_POINT ( 'NONE',  ( 54.29974487139159578, -27.71228299555243879, 4.000000000000000000 ) ) ;
#129873 = ADVANCED_FACE ( 'NONE', ( #131633 ), #55506, .T. ) ;
#129874 = CARTESIAN_POINT ( 'NONE',  ( 152.4000000000000057, 25.96999999999993847, 0.000000000000000000 ) ) ;
#129875 = CARTESIAN_POINT ( 'NONE',  ( -10.49999999999991829, -8.947814304570735899, 5.000000000000000000 ) ) ;
#129876 = DIRECTION ( 'NONE',  ( 0.7071067811865487940, 0.7071067811865463515, 0.000000000000000000 ) ) ;
#129877 = AXIS2_PLACEMENT_3D ( 'NONE', #94733, #3442, #136117 ) ;
#129878 = CARTESIAN_POINT ( 'NONE',  ( 41.18293019189811588, -1.637169565754158951, -6.109999999999998543 ) ) ;
#129879 = VERTEX_POINT ( 'NONE', #76550 ) ;
#129880 = CARTESIAN_POINT ( 'NONE',  ( -13.49999999999990763, -20.56887692260760758, 4.000000000000000000 ) ) ;
#129881 = VERTEX_POINT ( 'NONE', #44660 ) ;
#129882 = ORIENTED_EDGE ( 'NONE', *, *, #33473, .F. ) ;
#129883 = AXIS2_PLACEMENT_3D ( 'NONE', #105568, #31612, #119999 ) ;
#129884 = EDGE_LOOP ( 'NONE', ( #78411, #60208, #6254, #101937 ) ) ;
#129885 = AXIS2_PLACEMENT_3D ( 'NONE', #21009, #6520, #50806 ) ;
#129886 = ADVANCED_FACE ( 'NONE', ( #54104 ), #141055, .F. ) ;
#129887 = LINE ( 'NONE', #30593, #125517 ) ;
#129888 = ORIENTED_EDGE ( 'NONE', *, *, #64950, .F. ) ;
#129889 = CARTESIAN_POINT ( 'NONE',  ( -18.18398860626898994, 28.73617430169800002, 5.000000000000000000 ) ) ;
#129890 = LINE ( 'NONE', #48960, #50566 ) ;
#129891 = DIRECTION ( 'NONE',  ( 0.000000000000000000, 0.000000000000000000, 1.000000000000000000 ) ) ;
#129892 = FACE_BOUND ( 'NONE', #138862, .T. ) ;
#129893 = ORIENTED_EDGE ( 'NONE', *, *, #8245, .F. ) ;
#129894 = DIRECTION ( 'NONE',  ( 0.6830127018922181881, 0.6830127018922202975, -0.2588190451025214056 ) ) ;
#129895 = LINE ( 'NONE', #73393, #46777 ) ;
#129896 = LINE ( 'NONE', #119014, #81027 ) ;
#129897 = ORIENTED_EDGE ( 'NONE', *, *, #52401, .F. ) ;
#129898 = PLANE ( 'NONE',  #119874 ) ;
#129899 = ORIENTED_EDGE ( 'NONE', *, *, #73757, .F. ) ;
#129900 = ORIENTED_EDGE ( 'NONE', *, *, #75739, .F. ) ;
#129901 = AXIS2_PLACEMENT_3D ( 'NONE', #63881, #17490, #85594 ) ;
#129902 = CARTESIAN_POINT ( 'NONE',  ( 15.20840764549667767, 2.500000000000000888, 3.061616997868383141E-16 ) ) ;
#129903 = ORIENTED_EDGE ( 'NONE', *, *, #89026, .F. ) ;
#129904 = EDGE_CURVE ( 'NONE', #1343, #128385, #132372, .T. ) ;
#129905 = CARTESIAN_POINT ( 'NONE',  ( 59.99543019189810877, 5.291415217122916737, 3.055000000000001936 ) ) ;
#129906 = VERTEX_POINT ( 'NONE', #133080 ) ;
#129907 = CARTESIAN_POINT ( 'NONE',  ( 21.29177708983034378, -15.74070752338412760, 19.73771281079102735 ) ) ;
#129908 = EDGE_CURVE ( 'NONE', #128301, #66309, #65704, .T. ) ;
#129909 = CARTESIAN_POINT ( 'NONE',  ( -6.640000000000001457, -34.64999999999999147, -40.00000000000000000 ) ) ;
#129910 = ORIENTED_EDGE ( 'NONE', *, *, #70019, .F. ) ;
#129911 = EDGE_CURVE ( 'NONE', #3561, #118497, #9834, .T. ) ;
#129912 = DIRECTION ( 'NONE',  ( 0.7071067811865486830, -0.7071067811865464625, -0.000000000000000000 ) ) ;
#129913 = FACE_OUTER_BOUND ( 'NONE', #143512, .T. ) ;
#129914 = VECTOR ( 'NONE', #139250, 1000.000000000000000 ) ;
#129915 = ADVANCED_FACE ( 'NONE', ( #143209 ), #97552, .F. ) ;
#129916 = AXIS2_PLACEMENT_3D ( 'NONE', #118495, #127985, #62723 ) ;
#129917 = AXIS2_PLACEMENT_3D ( 'NONE', #113644, #34681, #47040 ) ;
#129918 = DIRECTION ( 'NONE',  ( -0.7071067811865486830, -0.7071067811865464625, -0.000000000000000000 ) ) ;
#129919 = LINE ( 'NONE', #130657, #80681 ) ;
#129920 = LINE ( 'NONE', #17568, #85231 ) ;
#129921 = DIRECTION ( 'NONE',  ( 0.6830127018922181881, 0.6830127018922202975, -0.2588190451025214056 ) ) ;
#129922 = CARTESIAN_POINT ( 'NONE',  ( 0.2997448713915885632, -27.71228299555206220, 4.000000000000000000 ) ) ;
#129923 = VERTEX_POINT ( 'NONE', #41760 ) ;
#129924 = VECTOR ( 'NONE', #140646, 1000.000000000000000 ) ;
#129925 = AXIS2_PLACEMENT_3D ( 'NONE', #87207, #129264, #29951 ) ;
#129926 = AXIS2_PLACEMENT_3D ( 'NONE', #28359, #95005, #137115 ) ;
#129927 = ORIENTED_EDGE ( 'NONE', *, *, #8309, .F. ) ;
#129928 = VECTOR ( 'NONE', #98479, 1000.000000000000114 ) ;
#129929 = LINE ( 'NONE', #40101, #49661 ) ;
#129930 = CARTESIAN_POINT ( 'NONE',  ( 0.000000000000000000, 0.000000000000000000, 5.000000000000000000 ) ) ;
#129931 = EDGE_LOOP ( 'NONE', ( #92719, #82376, #127674, #82392 ) ) ;
#129932 = AXIS2_PLACEMENT_3D ( 'NONE', #58323, #3831, #12607 ) ;
#129933 = ORIENTED_EDGE ( 'NONE', *, *, #8768, .F. ) ;
#129934 = ORIENTED_EDGE ( 'NONE', *, *, #49502, .F. ) ;
#129935 = CARTESIAN_POINT ( 'NONE',  ( -26.47599861414532185, 22.03583458319438293, 4.979811245910090278 ) ) ;
#129937 = EDGE_CURVE ( 'NONE', #122378, #39664, #33765, .T. ) ;
#129936 = DIRECTION ( 'NONE',  ( -0.7071067811865486830, -0.7071067811865464625, 0.000000000000000000 ) ) ;
#129938 = ADVANCED_FACE ( 'NONE', ( #130211 ), #56253, .F. ) ;
#129939 = CARTESIAN_POINT ( 'NONE',  ( 39.29974487139159578, -27.71228299555233576, 4.000000000000000000 ) ) ;
#129940 = ORIENTED_EDGE ( 'NONE', *, *, #113890, .F. ) ;
#129941 = AXIS2_PLACEMENT_3D ( 'NONE', #57670, #2510, #121457 ) ;
#129942 = CARTESIAN_POINT ( 'NONE',  ( 4.499999999999968914, 16.18958161055402911, -11.56426086740810355 ) ) ;
#129943 = EDGE_CURVE ( 'NONE', #2836, #55005, #108391, .T. ) ;
#129944 = DIRECTION ( 'NONE',  ( -0.7071067811865486830, -0.7071067811865464625, -0.000000000000000000 ) ) ;
#129945 = CARTESIAN_POINT ( 'NONE',  ( 22.96290314143522338, -3.967499999999994476, 6.871911579029513106 ) ) ;
#129946 = CARTESIAN_POINT ( 'NONE',  ( 9.591592354503321260, 2.500000000000001776, 0.000000000000000000 ) ) ;
#129947 = EDGE_LOOP ( 'NONE', ( #93611, #85895, #42640, #45412 ) ) ;
#129948 = CARTESIAN_POINT ( 'NONE',  ( 120.9537635252314658, -6.109999999999999432, -3.741295971395163529E-16 ) ) ;
#129949 = VECTOR ( 'NONE', #90302, 1000.000000000000227 ) ;
#129950 = FACE_OUTER_BOUND ( 'NONE', #29882, .T. ) ;
#129951 = PLANE ( 'NONE',  #44947 ) ;
#129952 = EDGE_CURVE ( 'NONE', #142336, #143446, #42503, .T. ) ;
#129954 = EDGE_LOOP ( 'NONE', ( #125402, #129467, #36146, #2317, #93336, #65523 ) ) ;
#129953 = DIRECTION ( 'NONE',  ( 1.000000000000000000, 0.000000000000000000, -0.000000000000000000 ) ) ;
#129955 = PLANE ( 'NONE',  #122564 ) ;
#129956 = VERTEX_POINT ( 'NONE', #47519 ) ;
#129957 = CARTESIAN_POINT ( 'NONE',  ( -22.88901570796818774, -1.420450978533076114, 4.272001239691292085 ) ) ;
#129958 = CARTESIAN_POINT ( 'NONE',  ( 1.500000000000000000, 0.000000000000000000, 0.000000000000000000 ) ) ;
#129959 = CARTESIAN_POINT ( 'NONE',  ( -1.828169399223511071, -2.240707523384262601, 4.000000000000000000 ) ) ;
#129960 = EDGE_LOOP ( 'NONE', ( #102410, #57299, #74695, #114499 ) ) ;
#129961 = VECTOR ( 'NONE', #112599, 1000.000000000000000 ) ;
#129962 = VECTOR ( 'NONE', #65899, 1000.000000000000000 ) ;
#129963 = AXIS2_PLACEMENT_3D ( 'NONE', #34715, #78954, #59347 ) ;
#129964 = DIRECTION ( 'NONE',  ( 0.000000000000000000, 0.000000000000000000, 1.000000000000000000 ) ) ;
#129965 = CARTESIAN_POINT ( 'NONE',  ( 4.288407645496676857, 9.139736423841732040E-16, 0.000000000000000000 ) ) ;
#129966 = EDGE_CURVE ( 'NONE', #6240, #115863, #35636, .T. ) ;
#129967 = ORIENTED_EDGE ( 'NONE', *, *, #59800, .T. ) ;
#129968 = CARTESIAN_POINT ( 'NONE',  ( 1.499999999999994449, -11.56887692260769818, 4.000000000000000000 ) ) ;
#129969 = AXIS2_PLACEMENT_3D ( 'NONE', #14284, #23740, #2678 ) ;
#129970 = CARTESIAN_POINT ( 'NONE',  ( 0.7175773864256688173, -21.73023691814493219, 5.000000000000000888 ) ) ;
#129971 = CARTESIAN_POINT ( 'NONE',  ( 7.939999999999994174, -60.26999999999998892, -7.752100000000003099 ) ) ;
#129972 = VERTEX_POINT ( 'NONE', #1768 ) ;
#129973 = VECTOR ( 'NONE', #43683, 1000.000000000000000 ) ;
#129974 = ORIENTED_EDGE ( 'NONE', *, *, #30439, .F. ) ;
#129975 = FACE_OUTER_BOUND ( 'NONE', #58315, .T. ) ;
#129976 = LINE ( 'NONE', #52397, #45956 ) ;
#129977 = EDGE_CURVE ( 'NONE', #54208, #92653, #69980, .T. ) ;
#129978 = CARTESIAN_POINT ( 'NONE',  ( 13.54123647476855474, 0.000000000000000000, 7.934999999999990727 ) ) ;
#129979 = CARTESIAN_POINT ( 'NONE',  ( -7.499999999999944045, 6.052185695429099788, 5.000000000000000000 ) ) ;
#129980 = CARTESIAN_POINT ( 'NONE',  ( 5.510786437626906675, -27.52281430457051314, 5.000000000000000000 ) ) ;
#129981 = CARTESIAN_POINT ( 'NONE',  ( 0.000000000000000000, -39.92999999999999261, -39.50000000000000000 ) ) ;
#129982 = EDGE_LOOP ( 'NONE', ( #112851, #86032, #50042, #60474 ) ) ;
#129983 = DIRECTION ( 'NONE',  ( -0.6830127018922180770, -0.6830127018922204085, -0.2588190451025213501 ) ) ;
#129984 = PLANE ( 'NONE',  #69903 ) ;
#129985 = CONICAL_SURFACE ( 'NONE', #53623, 2.055000000000000604, 0.9599310885968764806 ) ;
#129986 = LINE ( 'NONE', #51004, #139702 ) ;
#129987 = CARTESIAN_POINT ( 'NONE',  ( 34.18293019189809456, -1.637169565754159173, -6.109999999999999432 ) ) ;
#129988 = LINE ( 'NONE', #29940, #108925 ) ;
#129989 = ORIENTED_EDGE ( 'NONE', *, *, #119407, .F. ) ;
#129990 = LINE ( 'NONE', #139480, #18702 ) ;
#129991 = ORIENTED_EDGE ( 'NONE', *, *, #111905, .T. ) ;
#129992 = ADVANCED_FACE ( 'NONE', ( #1080 ), #25703, .F. ) ;
#129993 = ORIENTED_EDGE ( 'NONE', *, *, #103498, .F. ) ;
#129994 = VECTOR ( 'NONE', #74346, 999.9999999999998863 ) ;
#129995 = DIRECTION ( 'NONE',  ( -0.7071067811865487940, 0.7071067811865463515, -0.000000000000000000 ) ) ;
#129996 = LINE ( 'NONE', #142319, #143403 ) ;
#129997 = ORIENTED_EDGE ( 'NONE', *, *, #75247, .T. ) ;
#129998 = FACE_OUTER_BOUND ( 'NONE', #89938, .T. ) ;
#129999 = DIRECTION ( 'NONE',  ( -0.000000000000000000, -0.000000000000000000, 1.000000000000000000 ) ) ;
#130000 = FACE_OUTER_BOUND ( 'NONE', #2821, .T. ) ;
#130001 = CARTESIAN_POINT ( 'NONE',  ( 81.49999999999998579, 0.000000000000000000, -7.950000000000000178 ) ) ;
#130002 = CARTESIAN_POINT ( 'NONE',  ( 17.39159235450332019, 2.500000000000001776, 0.000000000000000000 ) ) ;
#130003 = ADVANCED_FACE ( 'NONE', ( #2497 ), #79438, .F. ) ;
#130004 = VERTEX_POINT ( 'NONE', #58398 ) ;
#130005 = DIRECTION ( 'NONE',  ( 0.7071067811865487940, 0.7071067811865463515, 0.000000000000000000 ) ) ;
#130006 = CARTESIAN_POINT ( 'NONE',  ( 3.000000000000000000, -4.600000000000055600, -28.92500000000000071 ) ) ;
#130008 = AXIS2_PLACEMENT_3D ( 'NONE', #55508, #90248, #47521 ) ;
#130007 = CARTESIAN_POINT ( 'NONE',  ( 0.5685132242927012358, 0.3999999999999995226, 2.467792535850613866 ) ) ;
#130009 = DIRECTION ( 'NONE',  ( 0.7071067811865487940, 0.7071067811865463515, 0.000000000000000000 ) ) ;
#130010 = CARTESIAN_POINT ( 'NONE',  ( 23.36654548503486950, 7.297668562427137573, 4.000000000000000000 ) ) ;
#130011 = CARTESIAN_POINT ( 'NONE',  ( 11.64065804060707165, 22.22500000000000142, 22.64546854729260161 ) ) ;
#130012 = CARTESIAN_POINT ( 'NONE',  ( 54.47502705046288440, -5.819803920172572198, 5.819803920172572198 ) ) ;
#130013 = DIRECTION ( 'NONE',  ( -1.000000000000000000, -0.000000000000000000, -0.000000000000000000 ) ) ;
#130014 = ORIENTED_EDGE ( 'NONE', *, *, #63275, .T. ) ;
#130015 = ORIENTED_EDGE ( 'NONE', *, *, #20592, .F. ) ;
#130016 = CARTESIAN_POINT ( 'NONE',  ( 57.72916666666665719, 7.950000000000001954, -2.130196079827421762 ) ) ;
#130017 = DIRECTION ( 'NONE',  ( -0.000000000000000000, 0.000000000000000000, 1.000000000000000000 ) ) ;
#130018 = DIRECTION ( 'NONE',  ( -0.000000000000000000, -0.3543493200069152693, 0.9351131265310292928 ) ) ;
#130019 = CARTESIAN_POINT ( 'NONE',  ( 7.139999999999991687, -35.76999999999998892, -12.10072711459627293 ) ) ;
#130020 = VERTEX_POINT ( 'NONE', #36578 ) ;
#130021 = AXIS2_PLACEMENT_3D ( 'NONE', #9022, #51169, #119250 ) ;
#130022 = STYLED_ITEM ( 'NONE', ( #35828 ), #131026 ) ;
#130023 =( BOUNDED_CURVE ( )  B_SPLINE_CURVE ( 3, ( #85574, #120317, #131239, #42825 ),
 .UNSPECIFIED., .F., .F. ) 
 B_SPLINE_CURVE_WITH_KNOTS ( ( 4, 4 ),
 ( 1.864375635226932504, 1.933014472006540752 ),
 .UNSPECIFIED. ) 
 CURVE ( )  GEOMETRIC_REPRESENTATION_ITEM ( )  RATIONAL_B_SPLINE_CURVE ( ( 1.000000000000000000, 0.9996074310407765395, 0.9996074310407765395, 1.000000000000000000 ) ) 
 REPRESENTATION_ITEM ( '' )  );
#130024 = PLANE ( 'NONE',  #111708 ) ;
#130025 = VECTOR ( 'NONE', #97253, 999.9999999999998863 ) ;
#130026 = AXIS2_PLACEMENT_3D ( 'NONE', #137389, #38081, #51097 ) ;
#130027 = CARTESIAN_POINT ( 'NONE',  ( 45.06293019189811844, 1.637169565754157174, 6.110000000000002984 ) ) ;
#130028 = EDGE_CURVE ( 'NONE', #38008, #36502, #130146, .T. ) ;
#130029 = VERTEX_POINT ( 'NONE', #35910 ) ;
#130030 = LINE ( 'NONE', #43036, #8524 ) ;
#130031 = ORIENTED_EDGE ( 'NONE', *, *, #127289, .F. ) ;
#130033 = ORIENTED_EDGE ( 'NONE', *, *, #107919, .T. ) ;
#130032 = VECTOR ( 'NONE', #17801, 999.9999999999998863 ) ;
#130034 = AXIS2_PLACEMENT_3D ( 'NONE', #86154, #84041, #7848 ) ;
#130035 = VECTOR ( 'NONE', #99855, 1000.000000000000000 ) ;
#130036 = VECTOR ( 'NONE', #3425, 999.9999999999998863 ) ;
#130037 = DIRECTION ( 'NONE',  ( -1.000000000000000000, -0.000000000000000000, -0.000000000000000000 ) ) ;
#130039 = CARTESIAN_POINT ( 'NONE',  ( 34.92499999999998295, 22.22500000000000142, 4.500000000000000888 ) ) ;
#130038 = VECTOR ( 'NONE', #139724, 1000.000000000000000 ) ;
#130040 = CARTESIAN_POINT ( 'NONE',  ( -33.48921356237309510, -27.52281430457078670, 5.000000000000000000 ) ) ;
#130042 = EDGE_CURVE ( 'NONE', #122443, #99871, #78675, .T. ) ;
#130041 = ORIENTED_EDGE ( 'NONE', *, *, #46206, .F. ) ;
#130043 = DIRECTION ( 'NONE',  ( 1.000000000000000000, 0.000000000000000000, 0.000000000000000000 ) ) ;
#130044 = LINE ( 'NONE', #74234, #32707 ) ;
#130046 = ORIENTED_EDGE ( 'NONE', *, *, #45995, .F. ) ;
#130045 = CARTESIAN_POINT ( 'NONE',  ( 9.670806282870438864, -3.047499999999997211, -5.278424836066143655 ) ) ;
#130047 = CARTESIAN_POINT ( 'NONE',  ( 84.43793019189810423, -6.110000000000001208, 1.637169565754158951 ) ) ;
#130048 = ADVANCED_FACE ( 'NONE', ( #69235 ), #125020, .T. ) ;
#130049 = DIRECTION ( 'NONE',  ( -0.3543493200069162685, -0.000000000000000000, -0.9351131265310288487 ) ) ;
#130050 = CARTESIAN_POINT ( 'NONE',  ( -30.79289321881324071, -2.240707523384262601, 5.000000000000000000 ) ) ;
#130051 = CARTESIAN_POINT ( 'NONE',  ( -11.99999999999991296, -19.06887692260762179, 4.000000000000000000 ) ) ;
#130052 =( GEOMETRIC_REPRESENTATION_CONTEXT ( 3 ) GLOBAL_UNCERTAINTY_ASSIGNED_CONTEXT ( ( #82381 ) ) GLOBAL_UNIT_ASSIGNED_CONTEXT ( ( #24133, #35031, #90083 ) ) REPRESENTATION_CONTEXT ( 'NONE', 'WORKASPACE' ) );
#130053 = CARTESIAN_POINT ( 'NONE',  ( 1.734723475976807094E-15, -9.033600742197645417, 5.000000000000000000 ) ) ;
#130054 = ORIENTED_EDGE ( 'NONE', *, *, #11053, .T. ) ;
#130055 = ADVANCED_FACE ( 'NONE', ( #24288 ), #81555, .F. ) ;
#130056 =( NAMED_UNIT ( * ) PLANE_ANGLE_UNIT ( ) SI_UNIT ( $, .RADIAN. ) );
#130057 = CARTESIAN_POINT ( 'NONE',  ( 69.18293019189809456, -1.637169565754158951, -6.109999999999998543 ) ) ;
#130058 = FACE_OUTER_BOUND ( 'NONE', #76611, .T. ) ;
#130059 = DIRECTION ( 'NONE',  ( 0.7071067811865487940, 0.7071067811865463515, 0.000000000000000000 ) ) ;
#130060 = CARTESIAN_POINT ( 'NONE',  ( 8.207106781186489286, 9.759292476615614831, 5.000000000000000000 ) ) ;
#130061 = VERTEX_POINT ( 'NONE', #100431 ) ;
#130062 = ORIENTED_EDGE ( 'NONE', *, *, #142889, .F. ) ;
#130063 = FACE_OUTER_BOUND ( 'NONE', #122058, .T. ) ;
#130064 = DIRECTION ( 'NONE',  ( 0.7071067811865486830, -0.7071067811865464625, -0.000000000000000000 ) ) ;
#130065 = ORIENTED_EDGE ( 'NONE', *, *, #101234, .F. ) ;
#130066 = EDGE_CURVE ( 'NONE', #35104, #17758, #3230, .T. ) ;
#130067 = VECTOR ( 'NONE', #100128, 1000.000000000000227 ) ;
#130068 = ORIENTED_EDGE ( 'NONE', *, *, #37538, .T. ) ;
#130069 = AXIS2_PLACEMENT_3D ( 'NONE', #39504, #29309, #127193 ) ;
#130070 = CARTESIAN_POINT ( 'NONE',  ( -8.999999999999937828, 7.588810512006198827, -3.013526669885207898 ) ) ;
#130071 = VERTEX_POINT ( 'NONE', #89539 ) ;
#130072 = VECTOR ( 'NONE', #38646, 1000.000000000000000 ) ;
#130073 = CARTESIAN_POINT ( 'NONE',  ( 13.10332671766740020, 3.690788593506699300, 4.000000000000000000 ) ) ;
#130074 = CARTESIAN_POINT ( 'NONE',  ( 27.48921356237309155, -27.52281430457074762, 5.000000000000000000 ) ) ;
#130075 = AXIS2_PLACEMENT_3D ( 'NONE', #24445, #57823, #76353 ) ;
#130076 = LINE ( 'NONE', #30774, #90536 ) ;
#130077 = FACE_BOUND ( 'NONE', #68611, .T. ) ;
#130078 = DIRECTION ( 'NONE',  ( -0.000000000000000000, 0.000000000000000000, 1.000000000000000000 ) ) ;
#130079 = DIRECTION ( 'NONE',  ( 0.7071067811865487940, -0.7071067811865463515, 0.000000000000000000 ) ) ;
#130080 = CARTESIAN_POINT ( 'NONE',  ( -34.49999999999975131, -4.535744391599457082, 4.994342998332168548 ) ) ;
#130082 = ORIENTED_EDGE ( 'NONE', *, *, #44003, .F. ) ;
#130081 = CARTESIAN_POINT ( 'NONE',  ( 30.79289321881325137, -8.240707523384195099, 5.000000000000000000 ) ) ;
#130083 = DIRECTION ( 'NONE',  ( -0.7071067811865487940, 0.7071067811865463515, 0.000000000000000000 ) ) ;
#130084 = ITEM_DEFINED_TRANSFORMATION ( 'NONE', 'NONE', #16921,  #127880 ) ;
#130085 = ORIENTED_EDGE ( 'NONE', *, *, #87878, .T. ) ;
#130087 = ORIENTED_EDGE ( 'NONE', *, *, #134937, .F. ) ;
#130086 = EDGE_CURVE ( 'NONE', #93963, #117180, #90998, .T. ) ;
#130088 = CARTESIAN_POINT ( 'NONE',  ( 81.28709685856478018, 3.054999999999997495, 5.291415217122919401 ) ) ;
#130089 = ORIENTED_EDGE ( 'NONE', *, *, #11156, .F. ) ;
#130090 = CARTESIAN_POINT ( 'NONE',  ( -2.999999999999981792, -11.35517001088072853, -1.126524801160114109 ) ) ;
#130091 = CARTESIAN_POINT ( 'NONE',  ( 12.32816939922344979, -3.740707523384244837, 4.000000000000000000 ) ) ;
#130092 = ADVANCED_FACE ( 'NONE', ( #59103 ), #90247, .F. ) ;
#130093 = VECTOR ( 'NONE', #136101, 1000.000000000000000 ) ;
#130094 = VERTEX_POINT ( 'NONE', #3908 ) ;
#130095 = CARTESIAN_POINT ( 'NONE',  ( 19.88840764549667384, 9.139736423841732040E-16, 0.000000000000000000 ) ) ;
#130096 = VECTOR ( 'NONE', #63859, 1000.000000000000000 ) ;
#130097 = EDGE_CURVE ( 'NONE', #48100, #99232, #68535, .T. ) ;
#130098 = EDGE_CURVE ( 'NONE', #127446, #27313, #135222, .T. ) ;
#130099 = LINE ( 'NONE', #32952, #3093 ) ;
#130100 = CARTESIAN_POINT ( 'NONE',  ( 5.999999999999959144, -15.03360074219758324, 5.000000000000000000 ) ) ;
#130101 = CARTESIAN_POINT ( 'NONE',  ( 2.207106781186531475, -14.24070752338414358, 5.000000000000000000 ) ) ;
#130102 = PLANE ( 'NONE',  #99154 ) ;
#130103 = PLANE ( 'NONE',  #77444 ) ;
#130104 = CARTESIAN_POINT ( 'NONE',  ( 1.499999999999992673, 21.05218569542895679, 5.000000000000000000 ) ) ;
#130105 = DIRECTION ( 'NONE',  ( 0.6830127018922180770, -0.6830127018922204085, -0.2588190451025213501 ) ) ;
#130106 = ORIENTED_EDGE ( 'NONE', *, *, #64477, .T. ) ;
#130107 = VECTOR ( 'NONE', #137279, 1000.000000000000000 ) ;
#130108 =( LENGTH_UNIT ( ) NAMED_UNIT ( * ) SI_UNIT ( .MILLI., .METRE. ) );
#130109 = ORIENTED_EDGE ( 'NONE', *, *, #39764, .F. ) ;
#130110 = CARTESIAN_POINT ( 'NONE',  ( 123.8916937171299253, 2.130196079822641142, 7.950000000002760636 ) ) ;
#130111 = DIRECTION ( 'NONE',  ( 1.734723475976806848E-16, -1.000000000000000000, 0.000000000000000000 ) ) ;
#130112 = ORIENTED_EDGE ( 'NONE', *, *, #71815, .F. ) ;
#130113 = EDGE_LOOP ( 'NONE', ( #132660, #102739, #80809, #37925 ) ) ;
#130114 = EDGE_CURVE ( 'NONE', #88778, #64888, #24978, .T. ) ;
#130116 = ORIENTED_EDGE ( 'NONE', *, *, #53574, .T. ) ;
#130115 = EDGE_CURVE ( 'NONE', #58061, #66948, #56950, .T. ) ;
#130117 = CARTESIAN_POINT ( 'NONE',  ( 35.29209685856476852, -5.291415217122921177, 3.054999999999999272 ) ) ;
#130118 = AXIS2_PLACEMENT_3D ( 'NONE', #126597, #137507, #71540 ) ;
#130119 = ORIENTED_EDGE ( 'NONE', *, *, #52347, .T. ) ;
#130120 = CARTESIAN_POINT ( 'NONE',  ( 45.91666666666666430, -6.884901960086287076, -3.975000000000000977 ) ) ;
#130121 = CARTESIAN_POINT ( 'NONE',  ( 25.56663961620377634, 1.633150327867695095, 6.094999999999988205 ) ) ;
#130122 = CARTESIAN_POINT ( 'NONE',  ( 7.354306473674146361, 12.49300487098931001, -25.30134302938294155 ) ) ;
#130123 = EDGE_CURVE ( 'NONE', #44265, #125649, #85084, .T. ) ;
#130124 = ORIENTED_EDGE ( 'NONE', *, *, #69041, .T. ) ;
#130125 = LINE ( 'NONE', #73599, #101317 ) ;
#130126 = ORIENTED_EDGE ( 'NONE', *, *, #27004, .T. ) ;
#130127 = LINE ( 'NONE', #118512, #51094 ) ;
#130128 = LINE ( 'NONE', #30828, #52139 ) ;
#130130 = EDGE_CURVE ( 'NONE', #24067, #117097, #116286, .T. ) ;
#130129 = VECTOR ( 'NONE', #105356, 999.9999999999998863 ) ;
#130131 = AXIS2_PLACEMENT_3D ( 'NONE', #130677, #33511, #100176 ) ;
#130133 = EDGE_LOOP ( 'NONE', ( #29599, #99151, #69778, #68712 ) ) ;
#130132 = DIRECTION ( 'NONE',  ( -0.7071067811865487940, 0.7071067811865463515, -0.000000000000000000 ) ) ;
#130134 = VECTOR ( 'NONE', #18035, 1000.000000000000000 ) ;
#130135 = ORIENTED_EDGE ( 'NONE', *, *, #98030, .F. ) ;
#130136 = CARTESIAN_POINT ( 'NONE',  ( -31.49999999999977973, 6.431123077392124188, 4.000000000000000000 ) ) ;
#130137 = VECTOR ( 'NONE', #64675, 1000.000000000000227 ) ;
#130138 = LINE ( 'NONE', #43832, #100366 ) ;
#130140 = ORIENTED_EDGE ( 'NONE', *, *, #60384, .F. ) ;
#130139 = AXIS2_PLACEMENT_3D ( 'NONE', #72722, #116874, #97986 ) ;
#130141 = CARTESIAN_POINT ( 'NONE',  ( 156.1499999999997783, -57.14999999999999147, -34.92499999999975557 ) ) ;
#130142 = VERTEX_POINT ( 'NONE', #138050 ) ;
#130143 = ORIENTED_EDGE ( 'NONE', *, *, #21656, .F. ) ;
#130144 = VERTEX_POINT ( 'NONE', #51045 ) ;
#130145 = LINE ( 'NONE', #142449, #5466 ) ;
#130146 = CIRCLE ( 'NONE', #109327, 2.500000000000000444 ) ;
#130147 = EDGE_CURVE ( 'NONE', #9910, #83102, #27849, .T. ) ;
#130148 = VECTOR ( 'NONE', #133916, 1000.000000000000000 ) ;
#130149 = PLANE ( 'NONE',  #106318 ) ;
#130150 = CARTESIAN_POINT ( 'NONE',  ( -3.183988606268992161, 28.73617430169789699, 5.000000000000000000 ) ) ;
#130151 = CARTESIAN_POINT ( 'NONE',  ( -1.410090645198307291, 9.759292476615618384, 11.28811694763778561 ) ) ;
#130152 = LINE ( 'NONE', #75073, #74933 ) ;
#130153 = CARTESIAN_POINT ( 'NONE',  ( -34.75611968250421313, 19.70565069852387197, 4.955485411084898040 ) ) ;
#130154 = ORIENTED_EDGE ( 'NONE', *, *, #60631, .F. ) ;
#130155 = CARTESIAN_POINT ( 'NONE',  ( -5.292893218813413903, -12.74070752338415247, 5.000000000000000000 ) ) ;
#130156 = VERTEX_POINT ( 'NONE', #4600 ) ;
#130157 = EDGE_CURVE ( 'NONE', #83079, #96308, #30965, .T. ) ;
#130158 = DIRECTION ( 'NONE',  ( 0.7071067811865487940, 0.7071067811865463515, -0.000000000000000000 ) ) ;
#130159 = EDGE_CURVE ( 'NONE', #77789, #66568, #66108, .T. ) ;
#130160 = CARTESIAN_POINT ( 'NONE',  ( 33.81206980810188156, 7.934999999999993392, 2.126176841940951689 ) ) ;
#130161 = EDGE_LOOP ( 'NONE', ( #126705, #367, #109189, #104153 ) ) ;
#130162 = CARTESIAN_POINT ( 'NONE',  ( -36.18398860626899705, 28.73617430169812437, 5.000000000000000000 ) ) ;
#130163 = FACE_OUTER_BOUND ( 'NONE', #64201, .T. ) ;
#130164 = ORIENTED_EDGE ( 'NONE', *, *, #103369, .T. ) ;
#130165 = ORIENTED_EDGE ( 'NONE', *, *, #118347, .F. ) ;
#130166 = CARTESIAN_POINT ( 'NONE',  ( 52.51281677483339649, -49.11905619111360721, 40.21880474160332142 ) ) ;
#130167 = CARTESIAN_POINT ( 'NONE',  ( 113.0000000000000000, 0.000000000000000000, -7.950000000000000178 ) ) ;
#130168 = FACE_OUTER_BOUND ( 'NONE', #13635, .T. ) ;
#130169 = CARTESIAN_POINT ( 'NONE',  ( 48.48921356237309510, -27.52281430457089328, 5.000000000000000000 ) ) ;
#130170 = EDGE_CURVE ( 'NONE', #143133, #112059, #6762, .T. ) ;
#130171 = CARTESIAN_POINT ( 'NONE',  ( 67.28709685856478018, 3.054999999999997939, 5.291415217122920289 ) ) ;
#130172 = VECTOR ( 'NONE', #115771, 1000.000000000000000 ) ;
#130173 = LINE ( 'NONE', #75097, #104269 ) ;
#130174 = AXIS2_PLACEMENT_3D ( 'NONE', #46498, #134918, #35611 ) ;
#130175 = LINE ( 'NONE', #40326, #41383 ) ;
#130176 = FACE_OUTER_BOUND ( 'NONE', #125181, .T. ) ;
#130177 = DIRECTION ( 'NONE',  ( -0.000000000000000000, -1.000000000000000000, -0.000000000000000000 ) ) ;
#130178 = VECTOR ( 'NONE', #70266, 1000.000000000000000 ) ;
#130179 = VERTEX_POINT ( 'NONE', #106821 ) ;
#130180 = CARTESIAN_POINT ( 'NONE',  ( 32.99451991528749062, 28.92564299267960948, 4.000000000000000000 ) ) ;
#130181 = ORIENTED_EDGE ( 'NONE', *, *, #95323, .F. ) ;
#130182 = CARTESIAN_POINT ( 'NONE',  ( -42.29974487139158157, -27.71228299555235708, 4.000000000000000000 ) ) ;
#130184 = CIRCLE ( 'NONE', #5114, 2.500000000000000444 ) ;
#130183 = DIRECTION ( 'NONE',  ( -0.6830127018922180770, -0.6830127018922204085, -0.2588190451025213501 ) ) ;
#130185 = EDGE_LOOP ( 'NONE', ( #120788, #29079, #40109, #138934 ) ) ;
#130186 = CARTESIAN_POINT ( 'NONE',  ( 6.229065384000522343, 3.821174125832445049E-16, 0.000000000000000000 ) ) ;
#130188 = ORIENTED_EDGE ( 'NONE', *, *, #77234, .F. ) ;
#130187 = DIRECTION ( 'NONE',  ( 0.7071067811865487940, 0.7071067811865463515, 0.000000000000000000 ) ) ;
#130189 = CARTESIAN_POINT ( 'NONE',  ( 106.5833333333333286, 6.884901960086290629, -3.974999999999994316 ) ) ;
#130190 = CARTESIAN_POINT ( 'NONE',  ( 34.92499999999998295, -21.18334561358932433, 4.500000000000000888 ) ) ;
#130191 = LINE ( 'NONE', #109844, #72707 ) ;
#130192 = VERTEX_POINT ( 'NONE', #127152 ) ;
#130193 = EDGE_LOOP ( 'NONE', ( #115912, #66091, #114835, #100194 ) ) ;
#130194 = DIRECTION ( 'NONE',  ( 0.7071067811865487940, -0.7071067811865463515, 0.000000000000000000 ) ) ;
#130195 = DIRECTION ( 'NONE',  ( -0.000000000000000000, 0.3543493200069153248, 0.9351131265310292928 ) ) ;
#130196 = UNCERTAINTY_MEASURE_WITH_UNIT (LENGTH_MEASURE( 1.000000000000000082E-05 ), #96070, 'distance_accuracy_value', 'NONE');
#130197 = AXIS2_PLACEMENT_3D ( 'NONE', #115244, #49363, #37015 ) ;
#130198 = DIRECTION ( 'NONE',  ( -0.7071067811865486830, -0.7071067811865464625, -0.000000000000000000 ) ) ;
#130199 = CARTESIAN_POINT ( 'NONE',  ( 80.72502705046289861, 5.819803920172573086, -5.819803920172572198 ) ) ;
#130200 = LINE ( 'NONE', #118583, #55553 ) ;
#130201 = DIRECTION ( 'NONE',  ( -0.3543493200069162685, -0.000000000000000000, -0.9351131265310288487 ) ) ;
#130202 = ORIENTED_EDGE ( 'NONE', *, *, #38945, .F. ) ;
#130203 =( BOUNDED_CURVE ( )  B_SPLINE_CURVE ( 3, ( #83421, #38481, #94971, #116012 ),
 .UNSPECIFIED., .F., .T. ) 
 B_SPLINE_CURVE_WITH_KNOTS ( ( 4, 4 ),
 ( 5.920967161967927161, 7.341195215986599187 ),
 .UNSPECIFIED. ) 
 CURVE ( )  GEOMETRIC_REPRESENTATION_ITEM ( )  RATIONAL_B_SPLINE_CURVE ( ( 1.000000000000000000, 0.8388583629366698213, 0.8388583629366698213, 1.000000000000000000 ) ) 
 REPRESENTATION_ITEM ( '' )  );
#130204 = DIRECTION ( 'NONE',  ( 0.7071067811865487940, 0.7071067811865463515, -0.000000000000000000 ) ) ;
#130205 = EDGE_CURVE ( 'NONE', #107763, #118405, #50330, .T. ) ;
#130206 = CARTESIAN_POINT ( 'NONE',  ( 12.39635797468499590, -22.22500000000000142, -12.93183150186171027 ) ) ;
#130208 = AXIS2_PLACEMENT_3D ( 'NONE', #82992, #115562, #62670 ) ;
#130207 = CARTESIAN_POINT ( 'NONE',  ( 33.54166666666667140, 3.047499999999993214, -5.278424836066146320 ) ) ;
#130209 = AXIS2_PLACEMENT_3D ( 'NONE', #56586, #134841, #698 ) ;
#130210 = ORIENTED_EDGE ( 'NONE', *, *, #68484, .F. ) ;
#130211 = FACE_OUTER_BOUND ( 'NONE', #124098, .T. ) ;
#130212 = ORIENTED_EDGE ( 'NONE', *, *, #2155, .T. ) ;
#130213 = CARTESIAN_POINT ( 'NONE',  ( 72.77126352523144703, 4.472830434245839371, 4.472830434245842035 ) ) ;
#130214 = LINE ( 'NONE', #85980, #103286 ) ;
#130216 = AXIS2_PLACEMENT_3D ( 'NONE', #131945, #32634, #99265 ) ;
#130215 = LINE ( 'NONE', #73680, #44802 ) ;
#130217 = ORIENTED_EDGE ( 'NONE', *, *, #40337, .T. ) ;
#130218 = VECTOR ( 'NONE', #10043, 1000.000000000000000 ) ;
#130219 = PLANE ( 'NONE',  #97466 ) ;
#130220 = CARTESIAN_POINT ( 'NONE',  ( 14.51078643762690490, -27.52281430457045275, 5.000000000000000000 ) ) ;
#130221 = CARTESIAN_POINT ( 'NONE',  ( -41.99451991528749062, 28.92564299267967343, 4.000000000000000000 ) ) ;
#130222 = ADVANCED_FACE ( 'NONE', ( #17665 ), #139511, .F. ) ;
#130223 = CARTESIAN_POINT ( 'NONE',  ( -11.20710678118646442, -5.240707523384228850, 5.000000000000000000 ) ) ;
#130225 = ORIENTED_EDGE ( 'NONE', *, *, #67773, .F. ) ;
#130224 = CARTESIAN_POINT ( 'NONE',  ( -14.58437909282842249, -0.7858193515946169105, 4.111732654926457009 ) ) ;
#130226 = ADVANCED_FACE ( 'NONE', ( #82261 ), #104693, .F. ) ;
#130227 = CARTESIAN_POINT ( 'NONE',  ( 128.7663314791150242, -49.19090614205754974, -40.79110616923124866 ) ) ;
#130228 = LINE ( 'NONE', #30917, #26784 ) ;
#130229 = VECTOR ( 'NONE', #7321, 1000.000000000000000 ) ;
#130230 =( BOUNDED_CURVE ( )  B_SPLINE_CURVE ( 3, ( #50013, #26112, #36968, #139169 ),
 .UNSPECIFIED., .F., .T. ) 
 B_SPLINE_CURVE_WITH_KNOTS ( ( 4, 4 ),
 ( 1.864375635226925398, 1.933014472006533868 ),
 .UNSPECIFIED. ) 
 CURVE ( )  GEOMETRIC_REPRESENTATION_ITEM ( )  RATIONAL_B_SPLINE_CURVE ( ( 1.000000000000000000, 0.9996074310407765395, 0.9996074310407765395, 1.000000000000000000 ) ) 
 REPRESENTATION_ITEM ( '' )  );
#130231 = CARTESIAN_POINT ( 'NONE',  ( 59.33333333333333570, -6.884901960086287964, 3.974999999999998312 ) ) ;
#130232 = EDGE_CURVE ( 'NONE', #117708, #2398, #51766, .T. ) ;
#130233 = ORIENTED_EDGE ( 'NONE', *, *, #119531, .T. ) ;
#130234 = ORIENTED_EDGE ( 'NONE', *, *, #121360, .F. ) ;
#130235 = CARTESIAN_POINT ( 'NONE',  ( 61.25043019189810423, 3.055000000000002824, -5.291415217122919401 ) ) ;
#130236 = ORIENTED_EDGE ( 'NONE', *, *, #20453, .T. ) ;
#130237 = ADVANCED_FACE ( 'NONE', ( #84402 ), #117676, .F. ) ;
#130238 = DIRECTION ( 'NONE',  ( 0.000000000000000000, 0.000000000000000000, 1.000000000000000000 ) ) ;
#130239 = DIRECTION ( 'NONE',  ( -0.000000000000000000, -0.3543493200069152693, 0.9351131265310292928 ) ) ;
#130240 = DIRECTION ( 'NONE',  ( -0.7071067811865486830, -0.7071067811865464625, 0.000000000000000000 ) ) ;
#130241 = DIRECTION ( 'NONE',  ( -0.3543493200069162685, -0.000000000000000000, -0.9351131265310288487 ) ) ;
#130242 = ORIENTED_EDGE ( 'NONE', *, *, #13438, .F. ) ;
#130243 = VECTOR ( 'NONE', #45643, 999.9999999999998863 ) ;
#130244 = AXIS2_PLACEMENT_3D ( 'NONE', #47035, #59311, #136111 ) ;
#130245 = LINE ( 'NONE', #64992, #95498 ) ;
#130246 = LINE ( 'NONE', #22156, #23542 ) ;
#130247 = VECTOR ( 'NONE', #10462, 1000.000000000000000 ) ;
#130248 = ADVANCED_FACE ( 'NONE', ( #94516 ), #39465, .T. ) ;
#130249 =( GEOMETRIC_REPRESENTATION_CONTEXT ( 3 ) GLOBAL_UNCERTAINTY_ASSIGNED_CONTEXT ( ( #137840 ) ) GLOBAL_UNIT_ASSIGNED_CONTEXT ( ( #139915, #131154, #31147 ) ) REPRESENTATION_CONTEXT ( 'NONE', 'WORKASPACE' ) );
#130250 = ORIENTED_EDGE ( 'NONE', *, *, #7836, .T. ) ;
#130251 = CARTESIAN_POINT ( 'NONE',  ( -18.24525979340076276, 9.091288135747575438, 4.682346157478786353 ) ) ;
#130253 = LINE ( 'NONE', #74445, #128904 ) ;
#130252 = AXIS2_PLACEMENT_3D ( 'NONE', #75485, #21079, #85614 ) ;
#130254 = CARTESIAN_POINT ( 'NONE',  ( 34.49999999999976552, 0.05432934483094861711, 4.994342998332161443 ) ) ;
#130255 = AXIS2_PLACEMENT_3D ( 'NONE', #24803, #4410, #81366 ) ;
#130256 = ADVANCED_FACE ( 'NONE', ( #44474 ), #64774, .T. ) ;
#130257 = ORIENTED_EDGE ( 'NONE', *, *, #110437, .T. ) ;
#130258 = ORIENTED_EDGE ( 'NONE', *, *, #2060, .T. ) ;
#130259 = PLANE ( 'NONE',  #52307 ) ;
#130260 = DIRECTION ( 'NONE',  ( -0.7071067811865486830, 0.7071067811865464625, 0.000000000000000000 ) ) ;
#130261 = FACE_OUTER_BOUND ( 'NONE', #66059, .T. ) ;
#130262 = DIRECTION ( 'NONE',  ( -0.3543493200069163240, -0.000000000000000000, 0.9351131265310288487 ) ) ;
#130263 = EDGE_CURVE ( 'NONE', #89689, #26788, #21965, .T. ) ;
#130264 = EDGE_CURVE ( 'NONE', #36236, #12429, #53155, .T. ) ;
#130265 = CARTESIAN_POINT ( 'NONE',  ( -23.20710678118637915, -2.240707523384254163, 5.000000000000000000 ) ) ;
#130266 = FACE_OUTER_BOUND ( 'NONE', #58192, .T. ) ;
#130267 = ORIENTED_EDGE ( 'NONE', *, *, #87523, .F. ) ;
#130268 = AXIS2_PLACEMENT_3D ( 'NONE', #54753, #101082, #110511 ) ;
#130269 = ORIENTED_EDGE ( 'NONE', *, *, #83510, .F. ) ;
#130270 = EDGE_LOOP ( 'NONE', ( #97479, #86895, #113539, #40576 ) ) ;
#130271 = ORIENTED_EDGE ( 'NONE', *, *, #42451, .T. ) ;
#130272 = EDGE_CURVE ( 'NONE', #80773, #71223, #107546, .T. ) ;
#130273 = PRESENTATION_STYLE_ASSIGNMENT (( #87473 ) ) ;
#130274 = AXIS2_PLACEMENT_3D ( 'NONE', #18434, #81625, #28663 ) ;
#130275 = CARTESIAN_POINT ( 'NONE',  ( -7.499999999999944045, 4.466399257802216027, 5.000000000000000000 ) ) ;
#130276 = EDGE_CURVE ( 'NONE', #13057, #126336, #32881, .T. ) ;
#130277 = ADVANCED_FACE ( 'NONE', ( #74961 ), #10364, .T. ) ;
#130278 = DIRECTION ( 'NONE',  ( 0.000000000000000000, 0.3543493200069153248, 0.9351131265310291818 ) ) ;
#130279 = ORIENTED_EDGE ( 'NONE', *, *, #105019, .T. ) ;
#130280 = CARTESIAN_POINT ( 'NONE',  ( 1.499999999999990896, -17.56887692260763956, 4.000000000000000000 ) ) ;
#130281 = DIRECTION ( 'NONE',  ( -0.7071067811865486830, -0.7071067811865464625, 0.000000000000000000 ) ) ;
#130282 = VECTOR ( 'NONE', #107808, 1000.000000000000114 ) ;
#130283 = CARTESIAN_POINT ( 'NONE',  ( 58.55836038379621300, -7.949999999999996625, -2.130196079827426203 ) ) ;
#130284 = PLANE ( 'NONE',  #143384 ) ;
#130285 = AXIS2_PLACEMENT_3D ( 'NONE', #60525, #96642, #16991 ) ;
#130286 = COLOUR_RGB ( '', 0.31764706, 0.68627451, 0.89019608) ;
#130287 = CARTESIAN_POINT ( 'NONE',  ( -56.99451991528749062, 28.92564299267978001, 4.000000000000000000 ) ) ;
#130288 = ORIENTED_EDGE ( 'NONE', *, *, #139627, .T. ) ;
#130289 = EDGE_CURVE ( 'NONE', #86768, #116904, #77796, .T. ) ;
#130290 = CARTESIAN_POINT ( 'NONE',  ( 15.79289321881334907, 15.75929247661555443, 5.000000000000000000 ) ) ;
#130291 = DIRECTION ( 'NONE',  ( 0.000000000000000000, -1.000000000000000000, 0.000000000000000000 ) ) ;
#130292 = ORIENTED_EDGE ( 'NONE', *, *, #47915, .T. ) ;
#130293 = PLANE ( 'NONE',  #41248 ) ;
#130294 = ORIENTED_EDGE ( 'NONE', *, *, #36511, .T. ) ;
#130295 = EDGE_CURVE ( 'NONE', #60012, #106911, #63378, .T. ) ;
#130296 = ORIENTED_EDGE ( 'NONE', *, *, #1188, .F. ) ;
#130297 = ORIENTED_EDGE ( 'NONE', *, *, #10569, .T. ) ;
#130298 = CARTESIAN_POINT ( 'NONE',  ( 66.20876352523144703, -7.482591942790329030E-16, 6.110000000000001208 ) ) ;
#130299 = ORIENTED_EDGE ( 'NONE', *, *, #89395, .F. ) ;
#130300 = ORIENTED_EDGE ( 'NONE', *, *, #124518, .F. ) ;
#130301 = CARTESIAN_POINT ( 'NONE',  ( 31.92500000000001492, -6.269999999999992468, -40.00000000000000000 ) ) ;
#130302 = CARTESIAN_POINT ( 'NONE',  ( 97.70876352523144703, -7.482591942790329030E-16, 6.110000000000001208 ) ) ;
#130303 = CARTESIAN_POINT ( 'NONE',  ( 31.11017322888190151, -22.22500000000000497, 4.785647885939355639 ) ) ;
#130304 = EDGE_CURVE ( 'NONE', #29361, #109641, #55330, .T. ) ;
#130306 = LINE ( 'NONE', #42595, #79008 ) ;
#130305 = VECTOR ( 'NONE', #90109, 1000.000000000000000 ) ;
#130307 = ORIENTED_EDGE ( 'NONE', *, *, #25019, .F. ) ;
#130308 = CARTESIAN_POINT ( 'NONE',  ( 27.68840764549667455, -2.499999999999996003, 0.000000000000000000 ) ) ;
#130309 = CIRCLE ( 'NONE', #67836, 2.500000000000000444 ) ;
#130310 = EDGE_CURVE ( 'NONE', #39023, #37409, #95452, .T. ) ;
#130311 = CARTESIAN_POINT ( 'NONE',  ( 22.82816939922335919, -14.24070752338414714, 4.000000000000000000 ) ) ;
#130312 = CARTESIAN_POINT ( 'NONE',  ( -14.81601139373099585, 28.73617430169776910, 5.000000000000000000 ) ) ;
#130313 = LINE ( 'NONE', #73085, #28968 ) ;
#130314 = ORIENTED_EDGE ( 'NONE', *, *, #63495, .T. ) ;
#130315 = VERTEX_POINT ( 'NONE', #143039 ) ;
#130316 = EDGE_LOOP ( 'NONE', ( #80710, #97728, #103159, #72800 ) ) ;
#130317 = ORIENTED_EDGE ( 'NONE', *, *, #53495, .T. ) ;
#130318 = CARTESIAN_POINT ( 'NONE',  ( 120.2245968585647944, -1.637169565754160949, 6.109999999999997655 ) ) ;
#130320 = ORIENTED_EDGE ( 'NONE', *, *, #55759, .T. ) ;
#130319 = AXIS2_PLACEMENT_3D ( 'NONE', #5576, #94718, #117879 ) ;
#130321 = CARTESIAN_POINT ( 'NONE',  ( 0.1839886062690032631, 28.73617430169787568, 5.000000000000000000 ) ) ;
#130322 = DIRECTION ( 'NONE',  ( -0.6830127018922180770, -0.6830127018922204085, -0.2588190451025213501 ) ) ;
#130323 = FACE_OUTER_BOUND ( 'NONE', #80335, .T. ) ;
#130324 = ORIENTED_EDGE ( 'NONE', *, *, #86590, .T. ) ;
#130325 = VECTOR ( 'NONE', #4246, 1000.000000000000000 ) ;
#130326 = ORIENTED_EDGE ( 'NONE', *, *, #11165, .F. ) ;
#130327 = CARTESIAN_POINT ( 'NONE',  ( 2.312069808101886448, 7.934999999999993392, 2.126176841940951689 ) ) ;
#130328 = DIRECTION ( 'NONE',  ( 0.000000000000000000, 1.000000000000000000, 0.000000000000000000 ) ) ;
#130329 = PLANE ( 'NONE',  #108463 ) ;
#130330 = CARTESIAN_POINT ( 'NONE',  ( 12.27285362782770761, -8.650847453065608761, -3.927786684156754582 ) ) ;
#130331 = EDGE_LOOP ( 'NONE', ( #96907, #99817, #20943, #36609 ) ) ;
#130332 = VERTEX_POINT ( 'NONE', #8205 ) ;
#130333 = VERTEX_POINT ( 'NONE', #97360 ) ;
#130334 = LINE ( 'NONE', #74533, #26410 ) ;
#130335 = LINE ( 'NONE', #109276, #101987 ) ;
#130336 = VECTOR ( 'NONE', #45833, 1000.000000000000000 ) ;
#130337 = CARTESIAN_POINT ( 'NONE',  ( -8.999999999999932498, -8.151047557385073361, -8.977947279169777417 ) ) ;
#130338 = CARTESIAN_POINT ( 'NONE',  ( -24.79289321881328689, -17.24070752338410628, 5.000000000000000000 ) ) ;
#130339 = DIRECTION ( 'NONE',  ( 0.000000000000000000, 0.000000000000000000, 1.000000000000000000 ) ) ;
#130340 = AXIS2_PLACEMENT_3D ( 'NONE', #83768, #28661, #27197 ) ;
#130341 = DIRECTION ( 'NONE',  ( 0.7071067811865487940, 0.7071067811865463515, 0.000000000000000000 ) ) ;
#130342 = CARTESIAN_POINT ( 'NONE',  ( 27.56293019189811133, 1.637169565754157174, 6.110000000000002984 ) ) ;
#130343 = SURFACE_STYLE_FILL_AREA ( #106386 ) ;
#130344 = SURFACE_STYLE_FILL_AREA ( #94809 ) ;
#130345 = VERTEX_POINT ( 'NONE', #108224 ) ;
#130346 = DIRECTION ( 'NONE',  ( 0.7071067811865487940, 0.7071067811865463515, -0.000000000000000000 ) ) ;
#130347 = AXIS2_PLACEMENT_3D ( 'NONE', #116578, #15781, #62940 ) ;
#130348 = AXIS2_PLACEMENT_3D ( 'NONE', #137877, #104504, #126270 ) ;
#130349 =( GEOMETRIC_REPRESENTATION_CONTEXT ( 3 ) GLOBAL_UNCERTAINTY_ASSIGNED_CONTEXT ( ( #114015 ) ) GLOBAL_UNIT_ASSIGNED_CONTEXT ( ( #4844, #96160, #73045 ) ) REPRESENTATION_CONTEXT ( 'NONE', 'WORKASPACE' ) );
#130350 = DIRECTION ( 'NONE',  ( -0.5735764363510501562, 0.8191520442889890230, 1.003171929053521419E-16 ) ) ;
#130351 = VERTEX_POINT ( 'NONE', #96634 ) ;
#130352 = LINE ( 'NONE', #7819, #32079 ) ;
#130354 = ORIENTED_EDGE ( 'NONE', *, *, #43473, .F. ) ;
#130353 = DIRECTION ( 'NONE',  ( -0.6830127018922181881, 0.6830127018922202975, -0.2588190451025214056 ) ) ;
#130355 = CARTESIAN_POINT ( 'NONE',  ( 13.64840764549667540, 3.061616997868380183E-16, -2.500000000000001332 ) ) ;
#130356 = ORIENTED_EDGE ( 'NONE', *, *, #56437, .T. ) ;
#130357 = CARTESIAN_POINT ( 'NONE',  ( 34.92500000000001847, 1.088194295437629318E-14, -40.00000000000000000 ) ) ;
#130358 = VECTOR ( 'NONE', #19643, 1000.000000000000000 ) ;
#130359 = ORIENTED_EDGE ( 'NONE', *, *, #36259, .F. ) ;
#130360 = CARTESIAN_POINT ( 'NONE',  ( 30.32816939922330945, -6.740707523384223521, 4.000000000000000000 ) ) ;
#130361 = UNCERTAINTY_MEASURE_WITH_UNIT (LENGTH_MEASURE( 1.000000000000000082E-05 ), #90232, 'distance_accuracy_value', 'NONE');
#130362 = EDGE_LOOP ( 'NONE', ( #139588, #26898, #140009, #8774 ) ) ;
#130363 = CARTESIAN_POINT ( 'NONE',  ( 94.28752705046289861, 0.000000000000000000, -7.949999999999998401 ) ) ;
#130364 = CARTESIAN_POINT ( 'NONE',  ( 109.4541937171295558, 6.884901960086283523, 3.975000000000002753 ) ) ;
#130365 = PLANE ( 'NONE',  #34648 ) ;
#130366 = VECTOR ( 'NONE', #107508, 1000.000000000000000 ) ;
#130367 = DIRECTION ( 'NONE',  ( 0.7071067811865487940, 0.7071067811865463515, 0.000000000000000000 ) ) ;
#130368 = FACE_BOUND ( 'NONE', #71768, .T. ) ;
#130369 = LINE ( 'NONE', #41930, #42526 ) ;
#130370 = CARTESIAN_POINT ( 'NONE',  ( -24.79289321881328334, -11.24070752338417556, 5.000000000000000000 ) ) ;
#130371 = CARTESIAN_POINT ( 'NONE',  ( 7.145833333333333925, -1.633150327867689988, 6.094999999999989981 ) ) ;
#130372 = CARTESIAN_POINT ( 'NONE',  ( 16.74956980810188867, 3.967499999999998916, 6.871911579029510442 ) ) ;
#130373 = LINE ( 'NONE', #39813, #44415 ) ;
#130374 = DIRECTION ( 'NONE',  ( -0.6830127018922181881, 0.6830127018922202975, -0.2588190451025214056 ) ) ;
#130375 = ORIENTED_EDGE ( 'NONE', *, *, #28708, .T. ) ;
#130376 = VECTOR ( 'NONE', #96204, 1000.000000000000000 ) ;
#130377 = VERTEX_POINT ( 'NONE', #20515 ) ;
#130378 = DIRECTION ( 'NONE',  ( -0.000000000000000000, 0.3543493200069153248, 0.9351131265310292928 ) ) ;
#130379 = ORIENTED_EDGE ( 'NONE', *, *, #130170, .F. ) ;
#130380 = VECTOR ( 'NONE', #59735, 1000.000000000000227 ) ;
#130381 = ADVANCED_FACE ( 'NONE', ( #140872 ), #130024, .F. ) ;
#130382 = CARTESIAN_POINT ( 'NONE',  ( 91.51669371712954160, 7.950000000000000178, -2.130196079827421318 ) ) ;
#130383 = CARTESIAN_POINT ( 'NONE',  ( 0.2997448713915885632, -27.71228299555206220, 4.000000000000000000 ) ) ;
#130384 =( LENGTH_UNIT ( ) NAMED_UNIT ( * ) SI_UNIT ( .MILLI., .METRE. ) );
#130385 = ORIENTED_EDGE ( 'NONE', *, *, #38549, .F. ) ;
#130386 = CARTESIAN_POINT ( 'NONE',  ( 17.99999999999987566, -6.033600742197667621, 5.000000000000000000 ) ) ;
#130387 = EDGE_CURVE ( 'NONE', #54291, #31488, #8887, .T. ) ;
#130388 = CARTESIAN_POINT ( 'NONE',  ( -57.18398860626899705, 28.73617430169827358, 5.000000000000000000 ) ) ;
#130389 = EDGE_CURVE ( 'NONE', #122295, #52699, #66210, .T. ) ;
#130390 = EDGE_CURVE ( 'NONE', #98689, #49293, #66949, .T. ) ;
#130391 = CARTESIAN_POINT ( 'NONE',  ( 0.2535635638417512716, -51.76057561339555946, 38.69631370864701836 ) ) ;
#130393 = ORIENTED_EDGE ( 'NONE', *, *, #125978, .T. ) ;
#130392 = DIRECTION ( 'NONE',  ( -0.6830127018922180770, -0.6830127018922204085, -0.2588190451025213501 ) ) ;
#130394 = CARTESIAN_POINT ( 'NONE',  ( 28.82816939922332722, 0.7592924766157104211, 4.000000000000000000 ) ) ;
#130395 = DIRECTION ( 'NONE',  ( -1.000000000000000000, -0.000000000000000000, -0.000000000000000000 ) ) ;
#130396 = DIRECTION ( 'NONE',  ( -1.000000000000000000, -0.000000000000000000, -0.000000000000000000 ) ) ;
#130397 = CARTESIAN_POINT ( 'NONE',  ( 81.48921356237309510, -27.52281430457112066, 5.000000000000000000 ) ) ;
#130398 = DIRECTION ( 'NONE',  ( -0.000000000000000000, 2.242629915582283412E-16, -1.000000000000000000 ) ) ;
#130400 = EDGE_CURVE ( 'NONE', #89147, #771, #86536, .T. ) ;
#130399 = AXIS2_PLACEMENT_3D ( 'NONE', #129072, #65285, #106580 ) ;
#130402 = EDGE_CURVE ( 'NONE', #80109, #51668, #178, .T. ) ;
#130401 = ORIENTED_EDGE ( 'NONE', *, *, #69236, .T. ) ;
#130403 = ORIENTED_EDGE ( 'NONE', *, *, #81037, .T. ) ;
#130404 = ORIENTED_EDGE ( 'NONE', *, *, #135461, .F. ) ;
#130405 = CARTESIAN_POINT ( 'NONE',  ( 105.2920968585647756, -5.291415217122921177, 3.054999999999999272 ) ) ;
#130406 = AXIS2_PLACEMENT_3D ( 'NONE', #69183, #90197, #123587 ) ;
#130407 = EDGE_LOOP ( 'NONE', ( #95627, #80501, #1351, #72790 ) ) ;
#130408 = ADVANCED_FACE ( 'NONE', ( #32135 ), #90827, .T. ) ;
#130409 = FACE_OUTER_BOUND ( 'NONE', #136819, .T. ) ;
#130410 = VECTOR ( 'NONE', #87230, 1000.000000000000227 ) ;
#130411 = FACE_OUTER_BOUND ( 'NONE', #54961, .T. ) ;
#130412 = EDGE_LOOP ( 'NONE', ( #7260, #19537, #92083, #47689 ) ) ;
#130413 = CARTESIAN_POINT ( 'NONE',  ( -19.49999999999986144, -10.53360074219763121, 5.000000000000000000 ) ) ;
#130414 = LINE ( 'NONE', #31802, #25714 ) ;
#130415 = EDGE_CURVE ( 'NONE', #74972, #84117, #133608, .T. ) ;
#130416 = CARTESIAN_POINT ( 'NONE',  ( 98.20376352523145158, 6.109999999999998543, 1.122388791418548911E-15 ) ) ;
#130417 = ORIENTED_EDGE ( 'NONE', *, *, #75456, .T. ) ;
#130418 = PLANE ( 'NONE',  #253 ) ;
#130419 = DIRECTION ( 'NONE',  ( -0.3543493200069162685, -0.000000000000000000, -0.9351131265310288487 ) ) ;
#130420 = AXIS2_PLACEMENT_3D ( 'NONE', #38776, #59826, #60563 ) ;
#130421 = CARTESIAN_POINT ( 'NONE',  ( 115.4791666666666572, -7.950000000000000178, 2.130196079827424427 ) ) ;
#130422 = CARTESIAN_POINT ( 'NONE',  ( 9.208651418775088970, -2.500000000000000444, 3.061616997868384127E-16 ) ) ;
#130423 = VERTEX_POINT ( 'NONE', #135060 ) ;
#130424 = VERTEX_POINT ( 'NONE', #102422 ) ;
#130425 = ORIENTED_EDGE ( 'NONE', *, *, #30027, .T. ) ;
#130426 = DIRECTION ( 'NONE',  ( 1.000000000000000000, 0.000000000000000000, 0.000000000000000000 ) ) ;
#130427 = CARTESIAN_POINT ( 'NONE',  ( -25.39999999999996305, 0.000000000000000000, 0.000000000000000000 ) ) ;
#130428 = CARTESIAN_POINT ( 'NONE',  ( 19.60873647476855197, -5.808823158059033709, 5.808823158059035485 ) ) ;
#130429 = VECTOR ( 'NONE', #101139, 999.9999999999998863 ) ;
#130430 = ADVANCED_FACE ( 'NONE', ( #79972 ), #92209, .F. ) ;
#130431 = CARTESIAN_POINT ( 'NONE',  ( 14.70025512860841133, -27.71228299555195917, 4.000000000000000000 ) ) ;
#130432 = CARTESIAN_POINT ( 'NONE',  ( 34.49999999999975842, 12.05432934483081908, 4.994342998332162331 ) ) ;
#130433 =( NAMED_UNIT ( * ) SI_UNIT ( $, .STERADIAN. ) SOLID_ANGLE_UNIT ( ) );
#130434 = VERTEX_POINT ( 'NONE', #111852 ) ;
#130435 = VERTEX_POINT ( 'NONE', #113982 ) ;
#130436 = CARTESIAN_POINT ( 'NONE',  ( 24.48921356237309510, -27.52281430457072631, 5.000000000000000000 ) ) ;
#130437 = EDGE_LOOP ( 'NONE', ( #97879, #75664, #142770, #84212 ) ) ;
#130438 = EDGE_LOOP ( 'NONE', ( #15012, #58094, #57293, #119370 ) ) ;
#130439 = EDGE_CURVE ( 'NONE', #39023, #86810, #58955, .T. ) ;
#130440 = AXIS2_PLACEMENT_3D ( 'NONE', #94815, #117984, #115848 ) ;
#130441 = VECTOR ( 'NONE', #40612, 999.9999999999998863 ) ;
#130442 = ADVANCED_FACE ( 'NONE', ( #66914 ), #67777, .T. ) ;
#130443 = CARTESIAN_POINT ( 'NONE',  ( 18.37500000000000355, -6.094999999999989981, 3.732111120401553285E-16 ) ) ;
#130444 = CARTESIAN_POINT ( 'NONE',  ( -11.01844734635663769, 18.75929247661552424, 20.33588619593445301 ) ) ;
#130445 = ORIENTED_EDGE ( 'NONE', *, *, #129527, .F. ) ;
#130446 = CARTESIAN_POINT ( 'NONE',  ( 25.49999999999982947, -4.533600742197692490, 5.000000000000000000 ) ) ;
#130447 = CARTESIAN_POINT ( 'NONE',  ( 18.79289321881333308, -14.24070752338413826, 5.000000000000000000 ) ) ;
#130448 = EDGE_CURVE ( 'NONE', #99882, #2363, #79263, .T. ) ;
#130449 = CARTESIAN_POINT ( 'NONE',  ( -13.49999999999991118, -7.420205493532915142, -2.617629953481283245 ) ) ;
#130450 = AXIS2_PLACEMENT_3D ( 'NONE', #37152, #5911, #61107 ) ;
#130451 = AXIS2_PLACEMENT_3D ( 'NONE', #944, #67694, #16643 ) ;
#130452 = DIRECTION ( 'NONE',  ( -0.7071067811865486830, 0.7071067811865464625, 0.000000000000000000 ) ) ;
#130453 = CARTESIAN_POINT ( 'NONE',  ( 1.748455871324237965, -11.24070752338417201, 10.39518518046008744 ) ) ;
#130454 = ORIENTED_EDGE ( 'NONE', *, *, #77253, .T. ) ;
#130455 = EDGE_CURVE ( 'NONE', #89594, #116711, #24828, .T. ) ;
#130456 = EDGE_LOOP ( 'NONE', ( #95785, #119875, #53686, #86266, #10774 ) ) ;
#130457 = DIRECTION ( 'NONE',  ( -0.7071067811865487940, 0.7071067811865463515, -0.000000000000000000 ) ) ;
#130458 = CARTESIAN_POINT ( 'NONE',  ( -13.49999999999990052, 13.56627193232213813, -10.57019076586071904 ) ) ;
#130459 = ORIENTED_EDGE ( 'NONE', *, *, #11276, .F. ) ;
#130460 = DIRECTION ( 'NONE',  ( -0.7071067811865487940, 0.7071067811865463515, 0.000000000000000000 ) ) ;
#130461 = VERTEX_POINT ( 'NONE', #124855 ) ;
#130462 = FACE_OUTER_BOUND ( 'NONE', #121005, .T. ) ;
#130463 = ORIENTED_EDGE ( 'NONE', *, *, #8888, .F. ) ;
#130464 = ORIENTED_EDGE ( 'NONE', *, *, #109273, .F. ) ;
#130466 = EDGE_CURVE ( 'NONE', #38343, #1788, #34283, .T. ) ;
#130465 = VECTOR ( 'NONE', #91245, 1000.000000000000000 ) ;
#130467 = VERTEX_POINT ( 'NONE', #135744 ) ;
#130468 = CARTESIAN_POINT ( 'NONE',  ( 29.80793019189811588, -6.109999999999998543, 1.637169565754158507 ) ) ;
#130469 = DIRECTION ( 'NONE',  ( -1.000000000000000000, -0.000000000000000000, -0.000000000000000000 ) ) ;
#130470 = DIRECTION ( 'NONE',  ( -1.000000000000000000, -1.224606353822377258E-16, -0.000000000000000000 ) ) ;
#130471 = DIRECTION ( 'NONE',  ( 0.000000000000000000, -0.000000000000000000, -1.000000000000000000 ) ) ;
#130472 = CARTESIAN_POINT ( 'NONE',  ( 2.111623618947573888, 9.759292476615621936, 17.35367589129212362 ) ) ;
#130473 = ADVANCED_FACE ( 'NONE', ( #45195 ), #101667, .F. ) ;
#130474 = CARTESIAN_POINT ( 'NONE',  ( 54.48921356237310221, -27.52281430457093236, 5.000000000000000000 ) ) ;
#130476 = CARTESIAN_POINT ( 'NONE',  ( -17.21837311707493257, 21.74787736706806385, 4.999607392498047531 ) ) ;
#130475 = DIRECTION ( 'NONE',  ( -0.7071067811865486830, 0.7071067811865464625, 0.000000000000000000 ) ) ;
#130478 = CARTESIAN_POINT ( 'NONE',  ( 17.99999999999987566, -3.412538124160721331, 4.000000000000000000 ) ) ;
#130477 = VECTOR ( 'NONE', #119917, 1000.000000000000000 ) ;
#130479 = LINE ( 'NONE', #41294, #32082 ) ;
#130480 = FACE_OUTER_BOUND ( 'NONE', #120236, .T. ) ;
#130481 = VECTOR ( 'NONE', #143137, 999.9999999999998863 ) ;
#130482 = CARTESIAN_POINT ( 'NONE',  ( 14.86920357848291196, 3.821174125832445049E-16, 0.000000000000000000 ) ) ;
#130483 = ORIENTED_EDGE ( 'NONE', *, *, #25078, .T. ) ;
#130484 = VERTEX_POINT ( 'NONE', #25532 ) ;
#130485 = ORIENTED_EDGE ( 'NONE', *, *, #46505, .F. ) ;
#130486 = ORIENTED_EDGE ( 'NONE', *, *, #23338, .T. ) ;
#130487 = CARTESIAN_POINT ( 'NONE',  ( -0.6643196045778319014, 1.144798890742325881, 3.945116340096009644 ) ) ;
#130488 = ORIENTED_EDGE ( 'NONE', *, *, #96906, .F. ) ;
#130489 =( BOUNDED_CURVE ( )  B_SPLINE_CURVE ( 3, ( #58528, #59911, #47635, #91796 ),
 .UNSPECIFIED., .F., .T. ) 
 B_SPLINE_CURVE_WITH_KNOTS ( ( 4, 4 ),
 ( 5.043186909253404515, 5.074607125596347856 ),
 .UNSPECIFIED. ) 
 CURVE ( )  GEOMETRIC_REPRESENTATION_ITEM ( )  RATIONAL_B_SPLINE_CURVE ( ( 1.000000000000000000, 0.9999177325257868620, 0.9999177325257868620, 1.000000000000000000 ) ) 
 REPRESENTATION_ITEM ( '' )  );
#130490 = VECTOR ( 'NONE', #71784, 1000.000000000000227 ) ;
#130491 = EDGE_LOOP ( 'NONE', ( #851, #27863, #26164, #85437 ) ) ;
#130492 = DIRECTION ( 'NONE',  ( -0.7071067811865486830, -0.7071067811865464625, 0.000000000000000000 ) ) ;
#130493 = DIRECTION ( 'NONE',  ( 0.7071067811865487940, 0.7071067811865463515, -0.000000000000000000 ) ) ;
#130494 = EDGE_CURVE ( 'NONE', #10056, #23517, #22648, .T. ) ;
#130495 = CARTESIAN_POINT ( 'NONE',  ( -44.99451991528749772, 28.92564299267969474, 4.000000000000000000 ) ) ;
#130496 = ORIENTED_EDGE ( 'NONE', *, *, #33259, .T. ) ;
#130497 = LINE ( 'NONE', #107283, #111244 ) ;
#130498 = ORIENTED_EDGE ( 'NONE', *, *, #61549, .T. ) ;
#130500 = VECTOR ( 'NONE', #83021, 1000.000000000000227 ) ;
#130499 = LINE ( 'NONE', #19567, #113979 ) ;
#130501 = ADVANCED_FACE ( 'NONE', ( #67661 ), #90070, .F. ) ;
#130502 = LINE ( 'NONE', #74700, #61302 ) ;
#130503 = AXIS2_PLACEMENT_3D ( 'NONE', #133339, #78974, #89806 ) ;
#130504 = CARTESIAN_POINT ( 'NONE',  ( 9.254569808101885897, -6.871911579029512218, 3.967499999999996252 ) ) ;
#130505 = ORIENTED_EDGE ( 'NONE', *, *, #118440, .T. ) ;
#130506 = CARTESIAN_POINT ( 'NONE',  ( 96.01626352523143737, -4.472830434245839371, 4.472830434245839371 ) ) ;
#130507 = CARTESIAN_POINT ( 'NONE',  ( 9.174743583335013497, -8.505992269982375120, -4.231105565351911402 ) ) ;
#130508 = CARTESIAN_POINT ( 'NONE',  ( 26.99451991528749417, 28.92564299267956685, 4.000000000000000000 ) ) ;
#130509 = LINE ( 'NONE', #32621, #109100 ) ;
#130510 = ORIENTED_EDGE ( 'NONE', *, *, #115391, .F. ) ;
#130511 = ORIENTED_EDGE ( 'NONE', *, *, #102636, .T. ) ;
#130512 = DIRECTION ( 'NONE',  ( -1.000000000000000000, -1.224606353822377258E-16, -0.000000000000000000 ) ) ;
#130513 = ORIENTED_EDGE ( 'NONE', *, *, #118601, .F. ) ;
#130515 = VECTOR ( 'NONE', #99887, 999.9999999999998863 ) ;
#130514 = CARTESIAN_POINT ( 'NONE',  ( -27.70710678118634007, 2.259292476615696099, 5.000000000000000000 ) ) ;
#130516 = DIRECTION ( 'NONE',  ( 0.7071067811865487940, 0.7071067811865463515, -0.000000000000000000 ) ) ;
#130517 = DIRECTION ( 'NONE',  ( 0.3543493200069162685, -0.000000000000000000, -0.9351131265310288487 ) ) ;
#130518 = CARTESIAN_POINT ( 'NONE',  ( 184.0821179325846515, -51.13011358081446645, -36.94363806876467748 ) ) ;
#130519 = ORIENTED_EDGE ( 'NONE', *, *, #102074, .F. ) ;
#130520 = PLANE ( 'NONE',  #117779 ) ;
#130521 = EDGE_CURVE ( 'NONE', #28286, #99726, #56069, .T. ) ;
#130522 = CARTESIAN_POINT ( 'NONE',  ( 0.8365287112654871127, 15.75929247661555443, 9.299976744542924223 ) ) ;
#130523 = DIRECTION ( 'NONE',  ( -0.7071067811865486830, 0.7071067811865464625, 0.000000000000000000 ) ) ;
#130524 = ORIENTED_EDGE ( 'NONE', *, *, #80551, .F. ) ;
#130525 = DIRECTION ( 'NONE',  ( -1.000000000000000000, -1.224606353822377258E-16, -0.000000000000000000 ) ) ;
#130526 = LINE ( 'NONE', #143515, #72523 ) ;
#130527 = ORIENTED_EDGE ( 'NONE', *, *, #52981, .T. ) ;
#130529 = ORIENTED_EDGE ( 'NONE', *, *, #74032, .T. ) ;
#130528 = LINE ( 'NONE', #7268, #74160 ) ;
#130530 = ORIENTED_EDGE ( 'NONE', *, *, #132635, .F. ) ;
#130531 = ADVANCED_FACE ( 'NONE', ( #48037 ), #36429, .T. ) ;
#130532 = AXIS2_PLACEMENT_3D ( 'NONE', #107899, #18028, #61612 ) ;
#130533 = PLANE ( 'NONE',  #7622 ) ;
#130534 = DIRECTION ( 'NONE',  ( -0.000000000000000000, 0.3543493200069153248, 0.9351131265310292928 ) ) ;
#130535 = ORIENTED_EDGE ( 'NONE', *, *, #142821, .F. ) ;
#130536 = DIRECTION ( 'NONE',  ( 1.000000000000000000, 0.000000000000000000, 0.000000000000000000 ) ) ;
#130537 = CARTESIAN_POINT ( 'NONE',  ( 27.12608002228219206, 1.810106405120792683, 7.950000000000001954 ) ) ;
#130538 = CYLINDRICAL_SURFACE ( 'NONE', #41554, 3.000000000000002665 ) ;
#130539 = CARTESIAN_POINT ( 'NONE',  ( 36.48921356237310221, -27.52281430457080802, 5.000000000000000000 ) ) ;
#130540 = CARTESIAN_POINT ( 'NONE',  ( -5.816011393731002066, 28.73617430169783304, 5.000000000000000000 ) ) ;
#130541 = DIRECTION ( 'NONE',  ( 0.000000000000000000, 0.000000000000000000, 1.000000000000000000 ) ) ;
#130542 = CARTESIAN_POINT ( 'NONE',  ( -15.18398860626900237, 28.73617430169797871, 5.000000000000000000 ) ) ;
#130543 = CARTESIAN_POINT ( 'NONE',  ( -25.39999999999996305, 0.000000000000000000, 2.500000000000000000 ) ) ;
#130544 = CARTESIAN_POINT ( 'NONE',  ( 18.95159235450331892, 9.902892378096218942E-16, 0.000000000000000000 ) ) ;
#130545 = DIRECTION ( 'NONE',  ( -0.000000000000000000, -0.3543493200069152693, 0.9351131265310292928 ) ) ;
#130546 = CARTESIAN_POINT ( 'NONE',  ( -42.48921356237308800, -27.52281430457085065, 5.000000000000000000 ) ) ;
#130547 = PLANE ( 'NONE',  #74304 ) ;
#130548 = VERTEX_POINT ( 'NONE', #3071 ) ;
#130549 = AXIS2_PLACEMENT_3D ( 'NONE', #4855, #136845, #81794 ) ;
#130550 = VERTEX_POINT ( 'NONE', #2325 ) ;
#130551 = ORIENTED_EDGE ( 'NONE', *, *, #134834, .T. ) ;
#130552 = CARTESIAN_POINT ( 'NONE',  ( 115.4791666666666572, -7.950000000000001066, 2.130196079827424427 ) ) ;
#130554 = EDGE_CURVE ( 'NONE', #24092, #120463, #912, .T. ) ;
#130553 = ORIENTED_EDGE ( 'NONE', *, *, #96005, .T. ) ;
#130555 = VERTEX_POINT ( 'NONE', #68376 ) ;
#130556 = VERTEX_POINT ( 'NONE', #112554 ) ;
#130557 = DIRECTION ( 'NONE',  ( 1.000000000000000000, 0.000000000000000000, 0.000000000000000000 ) ) ;
#130558 = CARTESIAN_POINT ( 'NONE',  ( 0.000000000000000000, 0.000000000000000000, 5.000000000000000000 ) ) ;
#130559 = VERTEX_POINT ( 'NONE', #13214 ) ;
#130560 = CARTESIAN_POINT ( 'NONE',  ( 6.471592354503322042, 2.500000000000001776, 0.000000000000000000 ) ) ;
#130561 = EDGE_CURVE ( 'NONE', #73050, #112438, #86263, .T. ) ;
#130562 = DIRECTION ( 'NONE',  ( -0.6830127018922180770, -0.6830127018922204085, -0.2588190451025213501 ) ) ;
#130563 = DIRECTION ( 'NONE',  ( -0.9743982503113671756, -0.2248289345038712306, 0.000000000000000000 ) ) ;
#130564 = LINE ( 'NONE', #31249, #69704 ) ;
#130565 = CARTESIAN_POINT ( 'NONE',  ( 99.60459685856476142, 1.637169565754164946, -6.109999999999999432 ) ) ;
#130566 = ORIENTED_EDGE ( 'NONE', *, *, #32912, .T. ) ;
#130568 = EDGE_CURVE ( 'NONE', #94977, #45414, #106644, .T. ) ;
#130567 = EDGE_CURVE ( 'NONE', #2768, #113494, #72675, .T. ) ;
#130569 = CARTESIAN_POINT ( 'NONE',  ( 12.83744844559187293, 6.995917548256143981, -30.85333074290490529 ) ) ;
#130570 = DIRECTION ( 'NONE',  ( 1.000000000000000000, 0.000000000000000000, 0.000000000000000000 ) ) ;
#130571 = VECTOR ( 'NONE', #6130, 999.9999999999998863 ) ;
#130572 = DIRECTION ( 'NONE',  ( -0.3543493200069162685, -0.000000000000000000, -0.9351131265310288487 ) ) ;
#130573 = CARTESIAN_POINT ( 'NONE',  ( 0.000000000000000000, 0.000000000000000000, 5.000000000000000000 ) ) ;
#130574 = FACE_OUTER_BOUND ( 'NONE', #97495, .T. ) ;
#130575 = CARTESIAN_POINT ( 'NONE',  ( 13.49159235450332162, -3.851859888774471706E-31, 2.500000000000001332 ) ) ;
#130576 = DIRECTION ( 'NONE',  ( 1.000000000000000000, 0.000000000000000000, 0.000000000000000000 ) ) ;
#130577 = EDGE_CURVE ( 'NONE', #54392, #77801, #50167, .T. ) ;
#130578 = ADVANCED_FACE ( 'NONE', ( #49481 ), #18196, .F. ) ;
#130579 = VECTOR ( 'NONE', #6744, 1000.000000000000227 ) ;
#130580 = VERTEX_POINT ( 'NONE', #5895 ) ;
#130581 = EDGE_LOOP ( 'NONE', ( #56179, #64392, #37677, #32545 ) ) ;
#130582 = CARTESIAN_POINT ( 'NONE',  ( 28.99999999999999645, 0.000000000000000000, -7.950000000000000178 ) ) ;
#130583 = EDGE_CURVE ( 'NONE', #143522, #131909, #88547, .T. ) ;
#130584 = ORIENTED_EDGE ( 'NONE', *, *, #71464, .T. ) ;
#130585 = DIRECTION ( 'NONE',  ( 0.000000000000000000, -1.000000000000000000, 0.000000000000000000 ) ) ;
#130586 = ADVANCED_FACE ( 'NONE', ( #62469 ), #140039, .F. ) ;
#130587 = CARTESIAN_POINT ( 'NONE',  ( 7.014532492589830248, 3.821174125832445049E-16, 0.000000000000000000 ) ) ;
#130588 = EDGE_CURVE ( 'NONE', #131428, #134578, #72341, .T. ) ;
#130589 = CARTESIAN_POINT ( 'NONE',  ( 14.99999999999989164, -22.06887692260759692, 4.000000000000000000 ) ) ;
#130590 = AXIS2_PLACEMENT_3D ( 'NONE', #134242, #112480, #34935 ) ;
#130591 = PLANE ( 'NONE',  #130252 ) ;
#130592 = CARTESIAN_POINT ( 'NONE',  ( 149.2199999999997999, -3.180000000000061444, 31.92499999999998295 ) ) ;
#130593 = LINE ( 'NONE', #21808, #16372 ) ;
#130594 = EDGE_CURVE ( 'NONE', #83105, #89365, #137177, .T. ) ;
#130595 = CARTESIAN_POINT ( 'NONE',  ( 119.3495968585647944, 6.109999999999996767, 1.637169565754163836 ) ) ;
#130596 = VECTOR ( 'NONE', #106566, 1000.000000000000000 ) ;
#130597 = ORIENTED_EDGE ( 'NONE', *, *, #72661, .T. ) ;
#130598 = AXIS2_PLACEMENT_3D ( 'NONE', #122715, #135751, #103117 ) ;
#130599 = CARTESIAN_POINT ( 'NONE',  ( -24.18398860626899705, 28.73617430169804265, 5.000000000000000000 ) ) ;
#130600 = VERTEX_POINT ( 'NONE', #139339 ) ;
#130601 = CARTESIAN_POINT ( 'NONE',  ( 0.000000000000000000, 0.000000000000000000, 5.000000000000000000 ) ) ;
#130602 = CARTESIAN_POINT ( 'NONE',  ( -17.99999999999987566, -2.904428200921318481, -6.989807076074900039 ) ) ;
#130603 = CARTESIAN_POINT ( 'NONE',  ( 11.51078643762690490, -27.52281430457047406, 5.000000000000000000 ) ) ;
#130604 = AXIS2_PLACEMENT_3D ( 'NONE', #59743, #72065, #117628 ) ;
#130605 = EDGE_CURVE ( 'NONE', #80902, #141246, #27672, .T. ) ;
#130606 = CARTESIAN_POINT ( 'NONE',  ( 39.29974487139159578, -27.71228299555233576, 4.000000000000000000 ) ) ;
#130607 = ORIENTED_EDGE ( 'NONE', *, *, #115866, .T. ) ;
#130608 = CARTESIAN_POINT ( 'NONE',  ( 48.27126352523143993, 4.472830434245839371, 4.472830434245842035 ) ) ;
#130609 = VECTOR ( 'NONE', #62562, 1000.000000000000000 ) ;
#130610 = VERTEX_POINT ( 'NONE', #81390 ) ;
#130611 = CARTESIAN_POINT ( 'NONE',  ( 8.510786437626906675, -27.52281430457049183, 5.000000000000000000 ) ) ;
#130612 = CARTESIAN_POINT ( 'NONE',  ( -30.18398860626900060, 28.73617430169808173, 5.000000000000000000 ) ) ;
#130613 = LINE ( 'NONE', #18967, #54842 ) ;
#130614 =( NAMED_UNIT ( * ) SI_UNIT ( $, .STERADIAN. ) SOLID_ANGLE_UNIT ( ) );
#130615 = EDGE_CURVE ( 'NONE', #132730, #24067, #114678, .T. ) ;
#130616 = VECTOR ( 'NONE', #101738, 1000.000000000000227 ) ;
#130617 = VECTOR ( 'NONE', #103191, 999.9999999999998863 ) ;
#130618 =( BOUNDED_SURFACE ( )  B_SPLINE_SURFACE ( 3, 2, ( 
 ( #135882, #36562, #28563 ),
 ( #27107, #80805, #37288 ),
 ( #81536, #26416, #53898 ),
 ( #40853, #96610, #140852 ) ),
 .UNSPECIFIED., .F., .F., .F. ) 
 B_SPLINE_SURFACE_WITH_KNOTS ( ( 4, 4 ),
 ( 3, 3 ),
 ( 0.000000000000000000, 0.001630001914283312967 ),
 ( 0.000000000000000000, 1.000000000000000000 ),
 .UNSPECIFIED. ) 
 GEOMETRIC_REPRESENTATION_ITEM ( )  RATIONAL_B_SPLINE_SURFACE ( (
 ( 1.000000000000000000, 0.7180326832784529323, 1.000000000000000000),
 ( 1.000000000000000000, 0.7157206429707735351, 1.000000000000000000),
 ( 1.000000000000000000, 0.7121002461815040263, 1.000000000000000000),
 ( 1.000000000000000000, 0.7071067811865475727, 1.000000000000000000) ) ) 
 REPRESENTATION_ITEM ( '' )  SURFACE ( )  );
#130619 = CARTESIAN_POINT ( 'NONE',  ( 36.07876352523144448, -7.482591942790325086E-16, 6.109999999999998543 ) ) ;
#130620 = VERTEX_POINT ( 'NONE', #59634 ) ;
#130621 = CARTESIAN_POINT ( 'NONE',  ( -25.36246187583883582, 22.22500000000000853, 4.000000000000000000 ) ) ;
#130622 = ORIENTED_EDGE ( 'NONE', *, *, #115857, .F. ) ;
#130623 = EDGE_LOOP ( 'NONE', ( #57422, #133465, #94599, #8600 ) ) ;
#130624 = VECTOR ( 'NONE', #37468, 999.9999999999998863 ) ;
#130625 = VERTEX_POINT ( 'NONE', #17511 ) ;
#130626 = CIRCLE ( 'NONE', #127736, 1.000000000000000888 ) ;
#130627 = FACE_OUTER_BOUND ( 'NONE', #59653, .T. ) ;
#130628 = CARTESIAN_POINT ( 'NONE',  ( -25.49999999999982236, 7.466399257802184053, 5.000000000000000000 ) ) ;
#130629 = ORIENTED_EDGE ( 'NONE', *, *, #56423, .T. ) ;
#130630 = CARTESIAN_POINT ( 'NONE',  ( -27.18398860626900060, 28.73617430169806042, 5.000000000000000000 ) ) ;
#130631 = ADVANCED_FACE ( 'NONE', ( #103789 ), #104526, .F. ) ;
#130632 = FACE_OUTER_BOUND ( 'NONE', #450, .T. ) ;
#130633 = VECTOR ( 'NONE', #3509, 1000.000000000000114 ) ;
#130634 = CARTESIAN_POINT ( 'NONE',  ( 22.22840764549667725, 3.061616997868380183E-16, -2.500000000000001332 ) ) ;
#130635 = ADVANCED_FACE ( 'NONE', ( #137893 ), #82109, .F. ) ;
#130636 = DIRECTION ( 'NONE',  ( 1.000000000000000000, 0.000000000000000000, 0.000000000000000000 ) ) ;
#130637 = FACE_BOUND ( 'NONE', #25760, .T. ) ;
#130638 = VERTEX_POINT ( 'NONE', #63899 ) ;
#130639 =( NAMED_UNIT ( * ) SI_UNIT ( $, .STERADIAN. ) SOLID_ANGLE_UNIT ( ) );
#130640 = DIRECTION ( 'NONE',  ( -0.3543493200069163240, 0.000000000000000000, 0.9351131265310288487 ) ) ;
#130641 = EDGE_LOOP ( 'NONE', ( #61763, #89641, #30036, #131803 ) ) ;
#130642 = DIRECTION ( 'NONE',  ( 1.000000000000000000, 0.000000000000000000, 0.000000000000000000 ) ) ;
#130643 = VERTEX_POINT ( 'NONE', #96471 ) ;
#130644 = ORIENTED_EDGE ( 'NONE', *, *, #83954, .T. ) ;
#130645 = CARTESIAN_POINT ( 'NONE',  ( -17.67183060077635304, 14.25929247661557753, 4.000000000000000000 ) ) ;
#130646 = EDGE_CURVE ( 'NONE', #73032, #129071, #140714, .T. ) ;
#130647 = ORIENTED_EDGE ( 'NONE', *, *, #53, .F. ) ;
#130648 = CARTESIAN_POINT ( 'NONE',  ( 55.18293019189812298, -1.637169565754158951, -6.109999999999998543 ) ) ;
#130649 = ORIENTED_EDGE ( 'NONE', *, *, #72208, .T. ) ;
#130650 = CARTESIAN_POINT ( 'NONE',  ( -31.49999999999978684, -4.216083040037277740, -7.486842126848585188 ) ) ;
#130651 = CARTESIAN_POINT ( 'NONE',  ( -11.99999999999991296, 16.93112307739200872, 4.000000000000000000 ) ) ;
#130652 = EDGE_CURVE ( 'NONE', #105689, #81537, #31969, .T. ) ;
#130653 = ORIENTED_EDGE ( 'NONE', *, *, #135623, .F. ) ;
#130654 = DIRECTION ( 'NONE',  ( 0.7071067811865487940, 0.7071067811865463515, -0.000000000000000000 ) ) ;
#130655 = FACE_OUTER_BOUND ( 'NONE', #7416, .T. ) ;
#130656 = DIRECTION ( 'NONE',  ( 0.7071067811865487940, -0.7071067811865463515, 0.000000000000000000 ) ) ;
#130657 = CARTESIAN_POINT ( 'NONE',  ( -48.48921356237309510, -27.52281430457089328, 5.000000000000000000 ) ) ;
#130658 = LINE ( 'NONE', #21864, #13399 ) ;
#130659 = FACE_OUTER_BOUND ( 'NONE', #105980, .T. ) ;
#130660 = DIRECTION ( 'NONE',  ( -1.000000000000000000, 0.000000000000000000, 0.000000000000000000 ) ) ;
#130661 = ORIENTED_EDGE ( 'NONE', *, *, #128065, .T. ) ;
#130662 = VERTEX_POINT ( 'NONE', #42873 ) ;
#130663 = ORIENTED_EDGE ( 'NONE', *, *, #14888, .F. ) ;
#130664 = CARTESIAN_POINT ( 'NONE',  ( 18.71247294953710494, 0.000000000000000000, 6.094999999999989981 ) ) ;
#130665 = PLANE ( 'NONE',  #44363 ) ;
#130666 = ORIENTED_EDGE ( 'NONE', *, *, #113853, .F. ) ;
#130667 = ORIENTED_EDGE ( 'NONE', *, *, #6976, .T. ) ;
#130668 = ORIENTED_EDGE ( 'NONE', *, *, #119827, .T. ) ;
#130669 = DIRECTION ( 'NONE',  ( -0.7071067811865487940, 0.7071067811865463515, -0.000000000000000000 ) ) ;
#130670 = CARTESIAN_POINT ( 'NONE',  ( 18.95159235450331892, 9.902892378096218942E-16, 0.000000000000000000 ) ) ;
#130671 = ADVANCED_FACE ( 'NONE', ( #54465 ), #130591, .F. ) ;
#130672 = ADVANCED_FACE ( 'NONE', ( #87779 ), #119655, .F. ) ;
#130673 = DIRECTION ( 'NONE',  ( 0.6830127018922180770, -0.6830127018922204085, -0.2588190451025213501 ) ) ;
#130674 = ORIENTED_EDGE ( 'NONE', *, *, #36217, .F. ) ;
#130675 = DIRECTION ( 'NONE',  ( 1.000000000000000000, 0.000000000000000000, 0.000000000000000000 ) ) ;
#130676 = VECTOR ( 'NONE', #32780, 1000.000000000000000 ) ;
#130677 = CARTESIAN_POINT ( 'NONE',  ( -21.48921356237309155, -27.52281430457070499, 5.000000000000000000 ) ) ;
#130678 = AXIS2_PLACEMENT_3D ( 'NONE', #109510, #110203, #72642 ) ;
#130679 = CARTESIAN_POINT ( 'NONE',  ( 16.69206980810189123, -7.934999999999991616, -2.126176841940955242 ) ) ;
#130680 = DIRECTION ( 'NONE',  ( 0.7071067811865487940, -0.7071067811865463515, 0.000000000000000000 ) ) ;
#130681 = VERTEX_POINT ( 'NONE', #129853 ) ;
#130682 = CARTESIAN_POINT ( 'NONE',  ( 120.6620968585647802, -5.291415217122919401, 3.054999999999998384 ) ) ;
#130683 = ADVANCED_FACE ( 'NONE', ( #29812 ), #108063, .F. ) ;
#130684 = VECTOR ( 'NONE', #77264, 1000.000000000000227 ) ;
#130685 = CARTESIAN_POINT ( 'NONE',  ( -36.48921356237310221, -27.52281430457080802, 5.000000000000000000 ) ) ;
#130686 = CARTESIAN_POINT ( 'NONE',  ( -30.49816348513938280, -17.24070752338409918, 8.407044977365297100 ) ) ;
#130688 = ORIENTED_EDGE ( 'NONE', *, *, #78074, .T. ) ;
#130687 = CARTESIAN_POINT ( 'NONE',  ( 9.516654386410381861, 22.22500000000000142, 4.500000000000000888 ) ) ;
#130689 = CARTESIAN_POINT ( 'NONE',  ( 67.60002705046288440, 5.819803920172570422, 5.819803920172575751 ) ) ;
#130690 = ORIENTED_EDGE ( 'NONE', *, *, #107411, .T. ) ;
#130691 = CARTESIAN_POINT ( 'NONE',  ( 10.49999999999991829, 16.18958161055403622, -11.56426086740808934 ) ) ;
#130692 = CARTESIAN_POINT ( 'NONE',  ( 152.4000000000000057, -16.48000000000005016, -12.70000000000045404 ) ) ;
#130693 = EDGE_CURVE ( 'NONE', #83571, #115863, #63209, .T. ) ;
#130694 = PLANE ( 'NONE',  #3166 ) ;
#130696 = EDGE_CURVE ( 'NONE', #111034, #37058, #86366, .T. ) ;
#130695 = EDGE_LOOP ( 'NONE', ( #44720, #72840, #16868 ) ) ;
#130697 = EDGE_CURVE ( 'NONE', #137066, #124568, #116365, .T. ) ;
#130698 = AXIS2_PLACEMENT_3D ( 'NONE', #99830, #496, #44790 ) ;
#130699 = VECTOR ( 'NONE', #62476, 1000.000000000000000 ) ;
#130700 = DIRECTION ( 'NONE',  ( -0.6830127018922180770, -0.6830127018922204085, -0.2588190451025213501 ) ) ;
#130701 = DIRECTION ( 'NONE',  ( 0.000000000000000000, 1.000000000000000000, 0.000000000000000000 ) ) ;
#130702 = ORIENTED_EDGE ( 'NONE', *, *, #125536, .F. ) ;
#130703 = FACE_OUTER_BOUND ( 'NONE', #70236, .T. ) ;
#130704 = CARTESIAN_POINT ( 'NONE',  ( 34.92499999999998295, 22.22500000000000142, 4.500000000000000888 ) ) ;
#130705 = EDGE_LOOP ( 'NONE', ( #128601, #120986, #76988, #44237 ) ) ;
#130706 = CARTESIAN_POINT ( 'NONE',  ( 5.250000000000000000, -7.464222240803106570E-16, -6.094999999999989981 ) ) ;
#130707 = PLANE ( 'NONE',  #69269 ) ;
#130708 = AXIS2_PLACEMENT_3D ( 'NONE', #101962, #1191, #112140 ) ;
#130709 = EDGE_LOOP ( 'NONE', ( #89338, #82869, #83732, #77660 ) ) ;
#130710 = EDGE_CURVE ( 'NONE', #40283, #18415, #87067, .T. ) ;
#130711 = EDGE_LOOP ( 'NONE', ( #43678, #100818, #30872, #44784 ) ) ;
#130712 = CARTESIAN_POINT ( 'NONE',  ( 31.92500000000001492, -6.269999999999992468, -37.00000000000000000 ) ) ;
#130713 = CARTESIAN_POINT ( 'NONE',  ( 7.771493228613311821, 20.25929247661551358, 7.808871592221786173 ) ) ;
#130714 = AXIS2_PLACEMENT_3D ( 'NONE', #87494, #8451, #43995 ) ;
#130715 = CARTESIAN_POINT ( 'NONE',  ( 27.68840764549667455, 9.139736423841732040E-16, 0.000000000000000000 ) ) ;
#130716 = VECTOR ( 'NONE', #68756, 1000.000000000000000 ) ;
#130717 =( GEOMETRIC_REPRESENTATION_CONTEXT ( 3 ) GLOBAL_UNCERTAINTY_ASSIGNED_CONTEXT ( ( #76682 ) ) GLOBAL_UNIT_ASSIGNED_CONTEXT ( ( #58354, #124261, #89488 ) ) REPRESENTATION_CONTEXT ( 'NONE', 'WORKASPACE' ) );
#130718 = LINE ( 'NONE', #64720, #76144 ) ;
#130719 = CARTESIAN_POINT ( 'NONE',  ( 39.49999999999999289, 0.000000000000000000, -7.950000000000000178 ) ) ;
#130720 = ORIENTED_EDGE ( 'NONE', *, *, #104835, .F. ) ;
#130721 = CARTESIAN_POINT ( 'NONE',  ( 152.4000000000000057, 7.919999999999947526, 19.12499999999998224 ) ) ;
#130722 = CARTESIAN_POINT ( 'NONE',  ( -14.99999999999989697, 16.93112307739200872, 4.000000000000000000 ) ) ;
#130723 = DIRECTION ( 'NONE',  ( -0.7071067811865486830, 0.7071067811865464625, 0.000000000000000000 ) ) ;
#130724 = CARTESIAN_POINT ( 'NONE',  ( 127.0000000000000000, -4.017717506652945580, -5.045834523320674059 ) ) ;
#130725 = CARTESIAN_POINT ( 'NONE',  ( 33.45376352523145158, -6.109999999999999432, -3.741295971395163529E-16 ) ) ;
#130726 = CARTESIAN_POINT ( 'NONE',  ( -21.77004279457778324, 21.73644205237997795, 5.000000000000000888 ) ) ;
#130727 = VECTOR ( 'NONE', #71440, 999.9999999999998863 ) ;
#130728 = ORIENTED_EDGE ( 'NONE', *, *, #94677, .T. ) ;
#130729 = ORIENTED_EDGE ( 'NONE', *, *, #56373, .T. ) ;
#130730 = DIRECTION ( 'NONE',  ( 1.000000000000000000, 0.000000000000000000, 0.000000000000000000 ) ) ;
#130731 = EDGE_LOOP ( 'NONE', ( #98526, #29081, #94002, #70069 ) ) ;
#130732 = EDGE_LOOP ( 'NONE', ( #78518, #110796, #7510 ) ) ;
#130733 = FACE_OUTER_BOUND ( 'NONE', #9520, .T. ) ;
#130734 = DIRECTION ( 'NONE',  ( 1.000000000000000000, 0.000000000000000000, 0.000000000000000000 ) ) ;
#130735 = EDGE_LOOP ( 'NONE', ( #27713, #141165, #131180 ) ) ;
#130736 = CARTESIAN_POINT ( 'NONE',  ( -60.48921356237309510, -27.52281430457097500, 5.000000000000000000 ) ) ;
#130737 = DIRECTION ( 'NONE',  ( -0.000000000000000000, -0.3543493200069152693, 0.9351131265310292928 ) ) ;
#130738 = LINE ( 'NONE', #40850, #97243 ) ;
#130739 = DIRECTION ( 'NONE',  ( 0.6830127018922181881, 0.6830127018922202975, -0.2588190451025214056 ) ) ;
#130740 = CARTESIAN_POINT ( 'NONE',  ( 50.99451991528749062, 28.92564299267973738, 4.000000000000000000 ) ) ;
#130741 = EDGE_LOOP ( 'NONE', ( #36210, #23193, #13528, #127831 ) ) ;
#130742 = DIRECTION ( 'NONE',  ( -0.7071067811865486830, -0.7071067811865464625, 0.000000000000000000 ) ) ;
#130743 = DIRECTION ( 'NONE',  ( -0.7071067811865487940, 0.7071067811865463515, 0.000000000000000000 ) ) ;
#130744 = CARTESIAN_POINT ( 'NONE',  ( -7.171830600776419651, 9.759292476615614831, 4.000000000000000000 ) ) ;
#130745 = FACE_OUTER_BOUND ( 'NONE', #113611, .T. ) ;
#130746 = LINE ( 'NONE', #6747, #72867 ) ;
#130747 = FILL_AREA_STYLE_COLOUR ( '', #93060 ) ;
#130748 = DIRECTION ( 'NONE',  ( -0.000000000000000000, 0.3543493200069153248, 0.9351131265310292928 ) ) ;
#130749 = CARTESIAN_POINT ( 'NONE',  ( 53.60002705046289861, 5.819803920172570422, 5.819803920172574863 ) ) ;
#130750 = EDGE_CURVE ( 'NONE', #22993, #30236, #76196, .T. ) ;
#130751 = DIRECTION ( 'NONE',  ( 0.3543493200069162685, -0.000000000000000000, -0.9351131265310288487 ) ) ;
#130752 = ORIENTED_EDGE ( 'NONE', *, *, #39546, .F. ) ;
#130753 = ORIENTED_EDGE ( 'NONE', *, *, #90844, .F. ) ;
#130754 = CARTESIAN_POINT ( 'NONE',  ( 53.79166666666667140, 3.975000000000003642, -6.884901960086285300 ) ) ;
#130755 = CARTESIAN_POINT ( 'NONE',  ( 127.0000000000000000, 1.564650039245123914, 6.154215649023822010 ) ) ;
#130756 = EDGE_CURVE ( 'NONE', #31572, #70129, #20352, .T. ) ;
#130757 = EDGE_CURVE ( 'NONE', #48106, #132436, #118968, .T. ) ;
#130758 = DIRECTION ( 'NONE',  ( 0.000000000000000000, 0.000000000000000000, 1.000000000000000000 ) ) ;
#130759 = ADVANCED_FACE ( 'NONE', ( #97943 ), #127448, .F. ) ;
#130760 = DIRECTION ( 'NONE',  ( -0.7071067811865486830, -0.7071067811865464625, 0.000000000000000000 ) ) ;
#130761 = ORIENTED_EDGE ( 'NONE', *, *, #25009, .T. ) ;
#130762 = EDGE_CURVE ( 'NONE', #102338, #16517, #137637, .T. ) ;
#130763 = LINE ( 'NONE', #136788, #17746 ) ;
#130764 = CIRCLE ( 'NONE', #35878, 3.000000000000002665 ) ;
#130765 = CARTESIAN_POINT ( 'NONE',  ( 13.20450575203696886, 4.382956123802139281, 4.000000000000000000 ) ) ;
#130766 = CARTESIAN_POINT ( 'NONE',  ( 43.60459685856476852, 1.637169565754164946, -6.109999999999999432 ) ) ;
#130768 = EDGE_CURVE ( 'NONE', #15864, #62440, #52044, .T. ) ;
#130767 = ORIENTED_EDGE ( 'NONE', *, *, #16654, .T. ) ;
#130769 = CYLINDRICAL_SURFACE ( 'NONE', #31662, 2.500000000000000444 ) ;
#130770 = ORIENTED_EDGE ( 'NONE', *, *, #124018, .F. ) ;
#130771 = ORIENTED_EDGE ( 'NONE', *, *, #138003, .T. ) ;
#130772 = FACE_OUTER_BOUND ( 'NONE', #105341, .T. ) ;
#130773 = LINE ( 'NONE', #54627, #114815 ) ;
#130774 = LINE ( 'NONE', #84412, #351 ) ;
#130775 = EDGE_CURVE ( 'NONE', #56766, #26207, #115110, .T. ) ;
#130776 = LINE ( 'NONE', #52457, #30 ) ;
#130777 = ORIENTED_EDGE ( 'NONE', *, *, #60540, .F. ) ;
#130779 = EDGE_CURVE ( 'NONE', #8157, #64105, #26302, .T. ) ;
#130778 = CARTESIAN_POINT ( 'NONE',  ( -23.28769006033954980, -21.73547319004781286, 4.999917730833664642 ) ) ;
#130780 = LINE ( 'NONE', #31444, #51223 ) ;
#130782 = EDGE_LOOP ( 'NONE', ( #89455, #2665, #1867, #61928 ) ) ;
#130781 = CARTESIAN_POINT ( 'NONE',  ( -19.17183060077634238, -11.24070752338416490, 4.000000000000000000 ) ) ;
#130783 = CARTESIAN_POINT ( 'NONE',  ( 84.72959685856476142, -6.110000000000000320, -1.637169565754161393 ) ) ;
#130784 = LINE ( 'NONE', #9669, #106329 ) ;
#130785 = CARTESIAN_POINT ( 'NONE',  ( 7.000000000000000888, 0.000000000000000000, 6.094999999999989981 ) ) ;
#130786 = DIRECTION ( 'NONE',  ( 1.000000000000000000, -0.000000000000000000, 0.000000000000000000 ) ) ;
#130787 = CARTESIAN_POINT ( 'NONE',  ( 30.32816939922332367, -21.74070752338405654, 4.000000000000000000 ) ) ;
#130788 = CARTESIAN_POINT ( 'NONE',  ( -2.671830600776449405, -3.740707523384251942, 4.000000000000000000 ) ) ;
#130789 = EDGE_CURVE ( 'NONE', #115093, #104746, #88647, .T. ) ;
#130790 = VECTOR ( 'NONE', #34642, 1000.000000000000000 ) ;
#130791 = ORIENTED_EDGE ( 'NONE', *, *, #17404, .F. ) ;
#130792 = PLANE ( 'NONE',  #77791 ) ;
#130793 = CARTESIAN_POINT ( 'NONE',  ( 71.80793019189812298, -6.109999999999998543, 1.637169565754158063 ) ) ;
#130794 = AXIS2_PLACEMENT_3D ( 'NONE', #64755, #132897, #893 ) ;
#130795 = DIRECTION ( 'NONE',  ( -0.6830127018922181881, 0.6830127018922202975, -0.2588190451025214056 ) ) ;
#130796 = LINE ( 'NONE', #20550, #124166 ) ;
#130797 = EDGE_LOOP ( 'NONE', ( #97695, #69638, #60876, #115439 ) ) ;
#130799 = EDGE_CURVE ( 'NONE', #103522, #137089, #39760, .T. ) ;
#130798 = VERTEX_POINT ( 'NONE', #29551 ) ;
#130800 = CARTESIAN_POINT ( 'NONE',  ( 20.99999999999983658, -13.39766691384881803, -10.96608748226470986 ) ) ;
#130801 = VERTEX_POINT ( 'NONE', #60077 ) ;
#130802 = EDGE_LOOP ( 'NONE', ( #55914, #3725, #139060, #104585 ) ) ;
#130803 = AXIS2_PLACEMENT_3D ( 'NONE', #96079, #94648, #51175 ) ;
#130804 = CARTESIAN_POINT ( 'NONE',  ( -5.510786437626906675, -27.52281430457051314, 5.000000000000000000 ) ) ;
#130805 = ORIENTED_EDGE ( 'NONE', *, *, #55010, .T. ) ;
#130806 = DIRECTION ( 'NONE',  ( -0.6830127018922180770, -0.6830127018922204085, -0.2588190451025213501 ) ) ;
#130807 = DIRECTION ( 'NONE',  ( 0.7071067811865487940, 0.7071067811865463515, -0.000000000000000000 ) ) ;
#130808 = EDGE_CURVE ( 'NONE', #132249, #139004, #117259, .T. ) ;
#130809 = CARTESIAN_POINT ( 'NONE',  ( -0.5116860592843074373, 6.759292476615660128, 16.35960578974469826 ) ) ;
#130810 = FACE_BOUND ( 'NONE', #88645, .T. ) ;
#130811 = DIRECTION ( 'NONE',  ( -0.7071067811865486830, 0.7071067811865464625, 0.000000000000000000 ) ) ;
#130812 = CARTESIAN_POINT ( 'NONE',  ( 9.279999999999999361, 2.055000000000001492, 0.000000000000000000 ) ) ;
#130813 = FACE_OUTER_BOUND ( 'NONE', #4271, .T. ) ;
#130815 = ORIENTED_EDGE ( 'NONE', *, *, #76140, .T. ) ;
#130814 = LINE ( 'NONE', #110434, #24990 ) ;
#130816 = PLANE ( 'NONE',  #83422 ) ;
#130817 = ITEM_DEFINED_TRANSFORMATION ( 'NONE', 'NONE', #53995,  #127880 ) ;
#130818 = VECTOR ( 'NONE', #98625, 1000.000000000000000 ) ;
#130819 = ORIENTED_EDGE ( 'NONE', *, *, #118328, .F. ) ;
#130820 = AXIS2_PLACEMENT_3D ( 'NONE', #83046, #127246, #81646 ) ;
#130822 = ORIENTED_EDGE ( 'NONE', *, *, #29621, .F. ) ;
#130821 = AXIS2_PLACEMENT_3D ( 'NONE', #102128, #5625, #28128 ) ;
#130823 = CARTESIAN_POINT ( 'NONE',  ( 82.30793019189809456, -6.109999999999998543, 1.637169565754158507 ) ) ;
#130824 = ORIENTED_EDGE ( 'NONE', *, *, #94255, .F. ) ;
#130825 = VECTOR ( 'NONE', #77503, 999.9999999999998863 ) ;
#130826 = LINE ( 'NONE', #143098, #88362 ) ;
#130827 = EDGE_CURVE ( 'NONE', #47269, #49530, #61524, .T. ) ;
#130828 = EDGE_LOOP ( 'NONE', ( #134196, #6959, #21138, #90077 ) ) ;
#130829 = DIRECTION ( 'NONE',  ( -1.000000000000000000, -0.000000000000000000, -0.000000000000000000 ) ) ;
#130830 = CARTESIAN_POINT ( 'NONE',  ( 8.111591955682463606, -2.055000000000000160, 2.789133085058097101E-16 ) ) ;
#130831 = DIRECTION ( 'NONE',  ( -0.000000000000000000, 0.3543493200069153248, 0.9351131265310292928 ) ) ;
#130832 = DIRECTION ( 'NONE',  ( -0.1737853339090456306, -0.1737853339090452420, 0.9693282805305142302 ) ) ;
#130833 = EDGE_CURVE ( 'NONE', #78861, #112275, #140462, .T. ) ;
#130834 = DIRECTION ( 'NONE',  ( -1.000000000000000000, 0.000000000000000000, 0.000000000000000000 ) ) ;
#130835 = CARTESIAN_POINT ( 'NONE',  ( 10.49999999999993250, -5.568876922607757685, 4.000000000000000000 ) ) ;
#130836 = PLANE ( 'NONE',  #14528 ) ;
#130837 = DIRECTION ( 'NONE',  ( -0.3543493200069162685, -0.000000000000000000, -0.9351131265310288487 ) ) ;
#130838 = VERTEX_POINT ( 'NONE', #83988 ) ;
#130839 = PLANE ( 'NONE',  #74718 ) ;
#130840 = ORIENTED_EDGE ( 'NONE', *, *, #9171, .F. ) ;
#130841 = CARTESIAN_POINT ( 'NONE',  ( 122.8708603837962272, 6.884901960086289741, -3.974999999999993427 ) ) ;
#130842 = LINE ( 'NONE', #109040, #97608 ) ;
#130843 = VERTEX_POINT ( 'NONE', #104246 ) ;
#130844 = ORIENTED_EDGE ( 'NONE', *, *, #2628, .F. ) ;
#130845 = EDGE_CURVE ( 'NONE', #52797, #70280, #41153, .T. ) ;
#130846 = ORIENTED_EDGE ( 'NONE', *, *, #99306, .T. ) ;
#130847 = EDGE_CURVE ( 'NONE', #115630, #35253, #91093, .T. ) ;
#130848 = CARTESIAN_POINT ( 'NONE',  ( 35.58376352523143282, -6.110000000000001208, -3.741295971395164515E-16 ) ) ;
#130849 = ORIENTED_EDGE ( 'NONE', *, *, #27402, .F. ) ;
#130850 = CARTESIAN_POINT ( 'NONE',  ( 46.35416666666667851, -2.130196079827349376, -7.950000000000045475 ) ) ;
#130851 = CARTESIAN_POINT ( 'NONE',  ( 90.05836038379621300, -7.949999999999996625, -2.130196079827426203 ) ) ;
#130852 = CARTESIAN_POINT ( 'NONE',  ( 22.79580628287044064, -5.278424836066144543, 3.047499999999995879 ) ) ;
#130853 = CARTESIAN_POINT ( 'NONE',  ( 8.331076807256511785, 12.11968929156625308, -25.56276712144670427 ) ) ;
#130854 = ORIENTED_EDGE ( 'NONE', *, *, #34176, .T. ) ;
#130855 = DIRECTION ( 'NONE',  ( -1.000000000000000000, -1.224606353822377258E-16, -0.000000000000000000 ) ) ;
#130856 = VERTEX_POINT ( 'NONE', #28865 ) ;
#130857 = FILL_AREA_STYLE_COLOUR ( '', #28004 ) ;
#130858 = DIRECTION ( 'NONE',  ( -0.7071067811865486830, -0.7071067811865464625, -0.000000000000000000 ) ) ;
#130860 = ORIENTED_EDGE ( 'NONE', *, *, #93534, .T. ) ;
#130859 = CARTESIAN_POINT ( 'NONE',  ( -26.99451991528749417, 28.92564299267956685, 4.000000000000000000 ) ) ;
#130861 = VERTEX_POINT ( 'NONE', #49209 ) ;
#130862 = CARTESIAN_POINT ( 'NONE',  ( 35.99451991528749772, 28.92564299267963079, 4.000000000000000000 ) ) ;
#130863 = CARTESIAN_POINT ( 'NONE',  ( 15.18398860626900237, 28.73617430169797871, 5.000000000000000000 ) ) ;
#130864 = DIRECTION ( 'NONE',  ( 1.000000000000000000, 0.000000000000000000, 0.000000000000000000 ) ) ;
#130865 = ORIENTED_EDGE ( 'NONE', *, *, #65, .T. ) ;
#130866 = CARTESIAN_POINT ( 'NONE',  ( 108.7250270504628844, 5.819803920172573974, -5.819803920172573086 ) ) ;
#130867 = EDGE_LOOP ( 'NONE', ( #50958, #93634, #7560, #13884 ) ) ;
#130869 = EDGE_LOOP ( 'NONE', ( #30284, #122214, #56282, #51463, #85404 ) ) ;
#130868 = ADVANCED_FACE ( 'NONE', ( #51336 ), #95524, .F. ) ;
#130870 = ORIENTED_EDGE ( 'NONE', *, *, #10782, .T. ) ;
#130871 = CARTESIAN_POINT ( 'NONE',  ( 30.18398860626900060, 28.73617430169808173, 5.000000000000000000 ) ) ;
#130872 = LINE ( 'NONE', #96743, #29976 ) ;
#130873 = CARTESIAN_POINT ( 'NONE',  ( 34.49999999999975842, -8.945670655168960650, 4.994342998332163219 ) ) ;
#130874 = LINE ( 'NONE', #62755, #19074 ) ;
#130876 = EDGE_CURVE ( 'NONE', #24466, #125243, #38315, .T. ) ;
#130875 = LINE ( 'NONE', #96746, #95690 ) ;
#130877 = CARTESIAN_POINT ( 'NONE',  ( 27.99999999999996803, -49.14999999999999147, 49.92499999999997584 ) ) ;
#130878 = EDGE_LOOP ( 'NONE', ( #1903, #13429, #72550, #66075 ) ) ;
#130879 = EDGE_CURVE ( 'NONE', #4040, #30662, #115825, .T. ) ;
#130880 = CARTESIAN_POINT ( 'NONE',  ( -30.18398860626900060, 28.73617430169808173, 5.000000000000000000 ) ) ;
#130881 = ORIENTED_EDGE ( 'NONE', *, *, #56479, .T. ) ;
#130882 = CARTESIAN_POINT ( 'NONE',  ( -41.99451991528749062, 28.92564299267967343, 4.000000000000000000 ) ) ;
#130883 = AXIS2_PLACEMENT_3D ( 'NONE', #109337, #112211, #143388 ) ;
#130884 = VERTEX_POINT ( 'NONE', #5646 ) ;
#130885 = DIRECTION ( 'NONE',  ( 1.000000000000000000, 0.000000000000000000, 0.000000000000000000 ) ) ;
#130886 = FACE_OUTER_BOUND ( 'NONE', #113706, .T. ) ;
#130887 = ORIENTED_EDGE ( 'NONE', *, *, #102832, .F. ) ;
#130888 = VECTOR ( 'NONE', #142678, 1000.000000000000000 ) ;
#130889 = VERTEX_POINT ( 'NONE', #83242 ) ;
#130890 = DIRECTION ( 'NONE',  ( -0.7071067811865487940, 0.7071067811865463515, -0.000000000000000000 ) ) ;
#130891 = LINE ( 'NONE', #117808, #122893 ) ;
#130892 = LINE ( 'NONE', #142472, #111731 ) ;
#130893 = CARTESIAN_POINT ( 'NONE',  ( 52.62499999999999289, -7.950000000000000178, -4.867971026610729436E-16 ) ) ;
#130894 = CARTESIAN_POINT ( 'NONE',  ( -7.499999999999951150, -12.08601207473289740, -10.46905243149092612 ) ) ;
#130895 = CARTESIAN_POINT ( 'NONE',  ( 64.51626352523143737, -4.472830434245839371, 4.472830434245839371 ) ) ;
#130896 = EDGE_CURVE ( 'NONE', #83228, #140445, #111373, .T. ) ;
#130897 =( BOUNDED_CURVE ( )  B_SPLINE_CURVE ( 3, ( #119850, #19146, #127930, #75681 ),
 .UNSPECIFIED., .F., .F. ) 
 B_SPLINE_CURVE_WITH_KNOTS ( ( 4, 4 ),
 ( 5.106027341939290309, 6.645403452391245303 ),
 .UNSPECIFIED. ) 
 CURVE ( )  GEOMETRIC_REPRESENTATION_ITEM ( )  RATIONAL_B_SPLINE_CURVE ( ( 1.000000000000000000, 0.8120851936182301722, 0.8120851936182301722, 1.000000000000000000 ) ) 
 REPRESENTATION_ITEM ( '' )  );
#130898 = DIRECTION ( 'NONE',  ( 1.000000000000000000, 0.000000000000000000, 0.000000000000000000 ) ) ;
#130899 = CARTESIAN_POINT ( 'NONE',  ( -7.828169399223472880, -20.24070752338407075, 4.000000000000000000 ) ) ;
#130900 = VECTOR ( 'NONE', #57270, 1000.000000000000000 ) ;
#130901 = CARTESIAN_POINT ( 'NONE',  ( 65.99451991528749772, 28.92564299267984396, 4.000000000000000000 ) ) ;
#130902 = DIRECTION ( 'NONE',  ( -0.7071067811865487940, 0.7071067811865463515, 0.000000000000000000 ) ) ;
#130903 = EDGE_LOOP ( 'NONE', ( #13132, #103265, #67668, #81000 ) ) ;
#130904 = DIRECTION ( 'NONE',  ( 1.000000000000000000, 0.000000000000000000, 0.000000000000000000 ) ) ;
#130905 = VERTEX_POINT ( 'NONE', #272 ) ;
#130906 = DIRECTION ( 'NONE',  ( 0.7071067811865487940, -0.7071067811865463515, 0.000000000000000000 ) ) ;
#130907 = DIRECTION ( 'NONE',  ( -0.000000000000000000, 0.000000000000000000, 1.000000000000000000 ) ) ;
#130908 = ORIENTED_EDGE ( 'NONE', *, *, #138064, .T. ) ;
#130909 = DIRECTION ( 'NONE',  ( -1.000000000000000000, -1.224606353822377258E-16, -0.000000000000000000 ) ) ;
#130911 = VERTEX_POINT ( 'NONE', #33677 ) ;
#130910 = FACE_OUTER_BOUND ( 'NONE', #74426, .T. ) ;
#130912 = CARTESIAN_POINT ( 'NONE',  ( -9.722814304570524868, -21.72500000000000497, 5.000000000000000000 ) ) ;
#130913 = FACE_OUTER_BOUND ( 'NONE', #51252, .T. ) ;
#130914 = CARTESIAN_POINT ( 'NONE',  ( -27.48921356237309155, -27.52281430457074762, 5.000000000000000000 ) ) ;
#130915 = VERTEX_POINT ( 'NONE', #141711 ) ;
#130916 = ORIENTED_EDGE ( 'NONE', *, *, #63346, .T. ) ;
#130917 = CARTESIAN_POINT ( 'NONE',  ( 0.000000000000000000, 0.000000000000000000, 7.950000000000000178 ) ) ;
#130918 = PLANE ( 'NONE',  #95352 ) ;
#130919 = CARTESIAN_POINT ( 'NONE',  ( -33.78162688292469795, 21.74787736706806740, 4.999607392498048419 ) ) ;
#130920 = LINE ( 'NONE', #22112, #34355 ) ;
#130921 = CARTESIAN_POINT ( 'NONE',  ( 84.80836038379621300, 7.949999999999997513, 2.130196079827431088 ) ) ;
#130922 = DIRECTION ( 'NONE',  ( -0.7071067811865486830, -0.7071067811865464625, 0.000000000000000000 ) ) ;
#130924 = EDGE_CURVE ( 'NONE', #126257, #40492, #54007, .T. ) ;
#130923 = VECTOR ( 'NONE', #14116, 1000.000000000000000 ) ;
#130925 = CARTESIAN_POINT ( 'NONE',  ( 25.39999999999999858, 1.126161369193132478, 16.41140641659140798 ) ) ;
#130926 = EDGE_LOOP ( 'NONE', ( #58601, #83206, #45764 ) ) ;
#130927 = VECTOR ( 'NONE', #119002, 1000.000000000000000 ) ;
#130928 = CARTESIAN_POINT ( 'NONE',  ( 6.489213562373093325, -27.52281430457059841, 5.000000000000000000 ) ) ;
#130929 = EDGE_CURVE ( 'NONE', #29058, #9428, #42415, .T. ) ;
#130930 = DIRECTION ( 'NONE',  ( -0.7071067811865486830, -0.7071067811865464625, 0.000000000000000000 ) ) ;
#130931 = CARTESIAN_POINT ( 'NONE',  ( 28.87500000000000000, -6.094999999999989981, 3.732111120401553285E-16 ) ) ;
#130932 = EDGE_LOOP ( 'NONE', ( #113640, #81938, #140013, #70368, #278, #124504 ) ) ;
#130933 = EDGE_CURVE ( 'NONE', #45676, #46507, #22041, .T. ) ;
#130934 = EDGE_CURVE ( 'NONE', #132567, #37221, #131538, .T. ) ;
#130935 = CARTESIAN_POINT ( 'NONE',  ( -21.70612307739179769, 22.22500000000000142, 4.000000000000000000 ) ) ;
#130936 = EDGE_LOOP ( 'NONE', ( #88532, #87981, #130668, #131815 ) ) ;
#130937 = CARTESIAN_POINT ( 'NONE',  ( 77.14626352523143282, -4.472830434245840259, 4.472830434245839371 ) ) ;
#130938 = SURFACE_SIDE_STYLE ('',( #42506 ) ) ;
#130939 = CARTESIAN_POINT ( 'NONE',  ( 2.510786437626908008, -27.52281430457053446, 5.000000000000000000 ) ) ;
#130940 = ORIENTED_EDGE ( 'NONE', *, *, #57603, .T. ) ;
#130941 = CARTESIAN_POINT ( 'NONE',  ( 0.000000000000000000, 0.000000000000000000, 5.000000000000000000 ) ) ;
#130942 = LINE ( 'NONE', #7692, #113681 ) ;
#130943 = EDGE_CURVE ( 'NONE', #66659, #24466, #66296, .T. ) ;
#130944 = DIRECTION ( 'NONE',  ( 0.3543493200069162685, -0.000000000000000000, -0.9351131265310288487 ) ) ;
#130945 = ADVANCED_FACE ( 'NONE', ( #11139 ), #86627, .F. ) ;
#130946 = CARTESIAN_POINT ( 'NONE',  ( 0.000000000000000000, 0.000000000000000000, 7.950000000000000178 ) ) ;
#130948 = ORIENTED_EDGE ( 'NONE', *, *, #116370, .T. ) ;
#130947 = CARTESIAN_POINT ( 'NONE',  ( 19.41999999999999815, 9.521314400968980422E-16, 0.000000000000000000 ) ) ;
#130949 = CARTESIAN_POINT ( 'NONE',  ( 131.6371832251712135, -49.11905619111362142, -40.21880474160340668 ) ) ;
#130950 = FACE_OUTER_BOUND ( 'NONE', #112983, .T. ) ;
#130951 = CARTESIAN_POINT ( 'NONE',  ( 76.97916666666665719, -7.950000000000000178, 2.130196079827424427 ) ) ;
#130952 = ORIENTED_EDGE ( 'NONE', *, *, #7377, .T. ) ;
#130953 = EDGE_CURVE ( 'NONE', #128691, #3502, #132997, .T. ) ;
#130954 = ORIENTED_EDGE ( 'NONE', *, *, #93425, .F. ) ;
#130955 = CARTESIAN_POINT ( 'NONE',  ( 67.95876352523144703, 0.000000000000000000, -6.110000000000001208 ) ) ;
#130956 = VERTEX_POINT ( 'NONE', #44571 ) ;
#130957 = CARTESIAN_POINT ( 'NONE',  ( -54.18398860626899705, 28.73617430169825226, 5.000000000000000000 ) ) ;
#130958 = LINE ( 'NONE', #31630, #103586 ) ;
#130959 = LINE ( 'NONE', #7708, #6343 ) ;
#130960 = PLANE ( 'NONE',  #40953 ) ;
#130961 = ORIENTED_EDGE ( 'NONE', *, *, #107708, .T. ) ;
#130962 = EDGE_CURVE ( 'NONE', #44496, #94791, #98202, .T. ) ;
#130963 = LINE ( 'NONE', #20736, #9830 ) ;
#130964 = ORIENTED_EDGE ( 'NONE', *, *, #41060, .F. ) ;
#130965 = DIRECTION ( 'NONE',  ( -0.7071067811865487940, 0.7071067811865463515, -0.000000000000000000 ) ) ;
#130966 = LINE ( 'NONE', #129497, #103440 ) ;
#130967 = EDGE_CURVE ( 'NONE', #28081, #124509, #143122, .T. ) ;
#130968 = LINE ( 'NONE', #30941, #72503 ) ;
#130969 = ORIENTED_EDGE ( 'NONE', *, *, #116236, .F. ) ;
#130970 = ORIENTED_EDGE ( 'NONE', *, *, #118170, .T. ) ;
#130971 = FACE_BOUND ( 'NONE', #95038, .T. ) ;
#130972 = PLANE ( 'NONE',  #13067 ) ;
#130973 = ADVANCED_FACE ( 'NONE', ( #75737 ), #119909, .F. ) ;
#130974 = CARTESIAN_POINT ( 'NONE',  ( 42.29974487139158157, -27.71228299555235708, 4.000000000000000000 ) ) ;
#130975 = DIRECTION ( 'NONE',  ( -0.7071067811865487940, 0.7071067811865463515, 0.000000000000000000 ) ) ;
#130976 = EDGE_CURVE ( 'NONE', #17123, #68874, #32973, .T. ) ;
#130977 = FACE_OUTER_BOUND ( 'NONE', #107016, .T. ) ;
#130978 = DIRECTION ( 'NONE',  ( -0.7071067811865486830, -0.7071067811865464625, -0.000000000000000000 ) ) ;
#130980 = EDGE_CURVE ( 'NONE', #56830, #142885, #20613, .T. ) ;
#130979 =( NAMED_UNIT ( * ) PLANE_ANGLE_UNIT ( ) SI_UNIT ( $, .RADIAN. ) );
#130982 = EDGE_LOOP ( 'NONE', ( #87771, #18010, #12928, #40915 ) ) ;
#130981 = VECTOR ( 'NONE', #108407, 1000.000000000000000 ) ;
#130983 = ORIENTED_EDGE ( 'NONE', *, *, #73754, .F. ) ;
#130984 = CARTESIAN_POINT ( 'NONE',  ( 116.1412635252314374, 4.472830434245835818, 4.472830434245840259 ) ) ;
#130985 = ORIENTED_EDGE ( 'NONE', *, *, #26273, .T. ) ;
#130986 = ORIENTED_EDGE ( 'NONE', *, *, #91994, .F. ) ;
#130987 = CARTESIAN_POINT ( 'NONE',  ( 181.1500000013235478, -47.86718710719740244, 37.19897551713948047 ) ) ;
#130988 = LINE ( 'NONE', #121502, #84815 ) ;
#130989 = FACE_OUTER_BOUND ( 'NONE', #118995, .T. ) ;
#130990 = VERTEX_POINT ( 'NONE', #64868 ) ;
#130991 = CARTESIAN_POINT ( 'NONE',  ( 27.18398860626900060, 28.73617430169806042, 5.000000000000000000 ) ) ;
#130992 = CARTESIAN_POINT ( 'NONE',  ( -63.18398860626900415, 28.73617430169831621, 5.000000000000000000 ) ) ;
#130994 = DIRECTION ( 'NONE',  ( 0.7071067811865487940, -0.7071067811865463515, 0.000000000000000000 ) ) ;
#130993 = CARTESIAN_POINT ( 'NONE',  ( -10.49999999999992539, 1.466399257802250222, 5.000000000000000000 ) ) ;
#130995 = CARTESIAN_POINT ( 'NONE',  ( 9.299744871391588674, -27.71228299555212971, 4.000000000000000000 ) ) ;
#130996 = DIRECTION ( 'NONE',  ( -0.000000000000000000, -0.000000000000000000, -1.000000000000000000 ) ) ;
#130997 = ORIENTED_EDGE ( 'NONE', *, *, #99618, .T. ) ;
#130998 = CARTESIAN_POINT ( 'NONE',  ( -19.99806943317887331, -22.22500000000000142, 4.500000000000000888 ) ) ;
#130999 = CARTESIAN_POINT ( 'NONE',  ( 50.87499999999999289, 7.950000000000000178, 1.460391307983218535E-15 ) ) ;
#131000 = VERTEX_POINT ( 'NONE', #109048 ) ;
#131001 = PLANE ( 'NONE',  #4139 ) ;
#131002 = ORIENTED_EDGE ( 'NONE', *, *, #36055, .F. ) ;
#131003 = EDGE_LOOP ( 'NONE', ( #48139, #105825, #140, #126723 ) ) ;
#131004 = CARTESIAN_POINT ( 'NONE',  ( 59.79209685856477563, -5.291415217122921177, 3.054999999999999272 ) ) ;
#131005 = ORIENTED_EDGE ( 'NONE', *, *, #57746, .F. ) ;
#131006 = AXIS2_PLACEMENT_3D ( 'NONE', #79452, #22140, #101859 ) ;
#131007 = CARTESIAN_POINT ( 'NONE',  ( -0.1839886062690032631, 28.73617430169787568, 5.000000000000000000 ) ) ;
#131008 = CARTESIAN_POINT ( 'NONE',  ( 101.7920968585647756, -5.291415217122921177, 3.054999999999999272 ) ) ;
#131009 = LINE ( 'NONE', #53431, #98033 ) ;
#131010 = AXIS2_PLACEMENT_3D ( 'NONE', #22018, #22704, #132972 ) ;
#131011 = EDGE_CURVE ( 'NONE', #123836, #141489, #87325, .T. ) ;
#131012 = LINE ( 'NONE', #41853, #60592 ) ;
#131013 = ORIENTED_EDGE ( 'NONE', *, *, #49164, .F. ) ;
#131014 = LINE ( 'NONE', #12768, #34957 ) ;
#131015 = CIRCLE ( 'NONE', #93947, 4.582731094065999322 ) ;
#131016 = DIRECTION ( 'NONE',  ( -0.000000000000000000, 0.000000000000000000, 1.000000000000000000 ) ) ;
#131017 = DIRECTION ( 'NONE',  ( -1.000000000000000000, -1.224606353822377258E-16, -0.000000000000000000 ) ) ;
#131018 = CARTESIAN_POINT ( 'NONE',  ( 76.93336038379621300, 2.130196079827431532, -7.949999999999996625 ) ) ;
#131019 = ORIENTED_EDGE ( 'NONE', *, *, #109794, .F. ) ;
#131020 = ORIENTED_EDGE ( 'NONE', *, *, #95599, .T. ) ;
#131021 = ORIENTED_EDGE ( 'NONE', *, *, #32376, .T. ) ;
#131022 = ORIENTED_EDGE ( 'NONE', *, *, #141966, .F. ) ;
#131023 = CARTESIAN_POINT ( 'NONE',  ( 123.4329301918981088, 1.637169565754156508, 6.110000000000000320 ) ) ;
#131024 = EDGE_LOOP ( 'NONE', ( #134958, #3684, #66752 ) ) ;
#131025 = CARTESIAN_POINT ( 'NONE',  ( -11.99451991528749417, 28.92564299267946382, 4.000000000000000000 ) ) ;
#131026 = ADVANCED_FACE ( 'NONE', ( #78590 ), #54708, .F. ) ;
#131027 = PLANE ( 'NONE',  #67214 ) ;
#131028 = VERTEX_POINT ( 'NONE', #36507 ) ;
#131029 = EDGE_CURVE ( 'NONE', #36667, #8819, #35106, .T. ) ;
#131030 = CARTESIAN_POINT ( 'NONE',  ( -42.18398860626899705, 28.73617430169816700, 5.000000000000000000 ) ) ;
#131031 = ORIENTED_EDGE ( 'NONE', *, *, #63525, .F. ) ;
#131032 = CARTESIAN_POINT ( 'NONE',  ( 14.70790314143522082, -6.871911579029513106, -3.967499999999993587 ) ) ;
#131033 = CARTESIAN_POINT ( 'NONE',  ( 32.99999999999977973, -22.06887692260758271, 4.000000000000000000 ) ) ;
#131034 = DIRECTION ( 'NONE',  ( 1.000000000000000000, 0.000000000000000000, 0.000000000000000000 ) ) ;
#131035 = EDGE_CURVE ( 'NONE', #121873, #13630, #59026, .T. ) ;
#131036 = CARTESIAN_POINT ( 'NONE',  ( 6.852250093007166143, -2.500000000000000444, 3.061616997868384127E-16 ) ) ;
#131037 = EDGE_LOOP ( 'NONE', ( #74120, #139115, #36102, #109044 ) ) ;
#131038 = ORIENTED_EDGE ( 'NONE', *, *, #70708, .F. ) ;
#131039 = ORIENTED_EDGE ( 'NONE', *, *, #72659, .F. ) ;
#131040 = CARTESIAN_POINT ( 'NONE',  ( 19.25000000000000355, -7.464222240803106570E-16, -6.094999999999989981 ) ) ;
#131041 = DIRECTION ( 'NONE',  ( -0.000000000000000000, -1.000000000000000000, -0.000000000000000000 ) ) ;
#131042 = CARTESIAN_POINT ( 'NONE',  ( -8.999999999999934275, -21.84840872380825516, 2.849755605029586469 ) ) ;
#131043 = EDGE_CURVE ( 'NONE', #92938, #97574, #102499, .T. ) ;
#131044 = CYLINDRICAL_SURFACE ( 'NONE', #129445, 7.950000000000000178 ) ;
#131045 = CARTESIAN_POINT ( 'NONE',  ( 29.60459685856477563, 1.637169565754164946, -6.109999999999999432 ) ) ;
#131046 = CARTESIAN_POINT ( 'NONE',  ( 29.99999999999980105, -22.06887692260758982, 4.000000000000000000 ) ) ;
#131047 = LINE ( 'NONE', #31731, #113735 ) ;
#131048 = ORIENTED_EDGE ( 'NONE', *, *, #24289, .T. ) ;
#131049 = LINE ( 'NONE', #118728, #136664 ) ;
#131050 = ORIENTED_EDGE ( 'NONE', *, *, #33738, .F. ) ;
#131051 = ADVANCED_FACE ( 'NONE', ( #3147 ), #80747, .F. ) ;
#131052 = DIRECTION ( 'NONE',  ( -0.000000000000000000, -1.000000000000000000, -0.000000000000000000 ) ) ;
#131053 = ORIENTED_EDGE ( 'NONE', *, *, #106699, .F. ) ;
#131054 = CARTESIAN_POINT ( 'NONE',  ( -25.49999999999982236, -13.91253812416061031, 4.000000000000000000 ) ) ;
#131056 = ORIENTED_EDGE ( 'NONE', *, *, #66104, .F. ) ;
#131055 = CARTESIAN_POINT ( 'NONE',  ( 41.54166666666665719, -3.975000000000002753, 6.884901960086286188 ) ) ;
#131057 = CARTESIAN_POINT ( 'NONE',  ( 21.66846741159843859, -18.74070752338408852, 20.73178291233846338 ) ) ;
#131058 = ORIENTED_EDGE ( 'NONE', *, *, #92265, .T. ) ;
#131059 = EDGE_LOOP ( 'NONE', ( #93563, #14443, #30104, #5792 ) ) ;
#131060 = LINE ( 'NONE', #65848, #62892 ) ;
#131061 = VERTEX_POINT ( 'NONE', #135140 ) ;
#131062 =( BOUNDED_CURVE ( )  B_SPLINE_CURVE ( 3, ( #10778, #32580, #85492, #87659 ),
 .UNSPECIFIED., .F., .T. ) 
 B_SPLINE_CURVE_WITH_KNOTS ( ( 4, 4 ),
 ( 5.106027341939297415, 6.645403452391245303 ),
 .UNSPECIFIED. ) 
 CURVE ( )  GEOMETRIC_REPRESENTATION_ITEM ( )  RATIONAL_B_SPLINE_CURVE ( ( 1.000000000000000000, 0.8120851936182316155, 0.8120851936182316155, 1.000000000000000000 ) ) 
 REPRESENTATION_ITEM ( '' )  );
#131063 = VECTOR ( 'NONE', #75326, 1000.000000000000000 ) ;
#131064 = CARTESIAN_POINT ( 'NONE',  ( 115.1416937171295558, -2.130196079827424871, -7.949999999999999289 ) ) ;
#131065 = CARTESIAN_POINT ( 'NONE',  ( 14.51078643762690490, -27.52281430457045275, 5.000000000000000000 ) ) ;
#131066 = DIRECTION ( 'NONE',  ( -0.3543493200069162685, -0.000000000000000000, -0.9351131265310288487 ) ) ;
#131067 = VECTOR ( 'NONE', #45222, 1000.000000000000000 ) ;
#131068 = LINE ( 'NONE', #52081, #109277 ) ;
#131070 = ADVANCED_FACE ( 'NONE', ( #16139 ), #101033, .F. ) ;
#131069 = DIRECTION ( 'NONE',  ( 0.000000000000000000, 0.000000000000000000, -1.000000000000000000 ) ) ;
#131071 = CARTESIAN_POINT ( 'NONE',  ( -26.99999999999981526, 7.007997736742422212, -8.085015511992175163 ) ) ;
#131072 = CARTESIAN_POINT ( 'NONE',  ( 0.8750000000000001110, -6.094999999999989981, 3.732111120401553285E-16 ) ) ;
#131073 = CARTESIAN_POINT ( 'NONE',  ( 20.24956980810188867, 3.967499999999998916, 6.871911579029510442 ) ) ;
#131074 = CARTESIAN_POINT ( 'NONE',  ( -20.41126436577413727, 22.22500000000000142, -0.4997969837368500534 ) ) ;
#131075 = CARTESIAN_POINT ( 'NONE',  ( 18.48921356237309510, -27.52281430457068367, 5.000000000000000000 ) ) ;
#131076 = VERTEX_POINT ( 'NONE', #69153 ) ;
#131078 = ORIENTED_EDGE ( 'NONE', *, *, #143521, .F. ) ;
#131077 = EDGE_CURVE ( 'NONE', #68534, #106183, #136516, .T. ) ;
#131079 = EDGE_CURVE ( 'NONE', #74755, #93941, #45791, .T. ) ;
#131080 = FACE_OUTER_BOUND ( 'NONE', #53116, .T. ) ;
#131081 = EDGE_LOOP ( 'NONE', ( #67266, #142289, #24526, #43562 ) ) ;
#131082 = VECTOR ( 'NONE', #2477, 1000.000000000000000 ) ;
#131083 = DIRECTION ( 'NONE',  ( -0.000000000000000000, 0.3543493200069153248, 0.9351131265310292928 ) ) ;
#131084 = DIRECTION ( 'NONE',  ( -1.000000000000000000, -0.000000000000000000, -0.000000000000000000 ) ) ;
#131085 = DIRECTION ( 'NONE',  ( -0.5735764363510501562, 0.8191520442889890230, 1.003171929053521419E-16 ) ) ;
#131086 = CARTESIAN_POINT ( 'NONE',  ( 128.5279624519184836, -51.91654526992326879, -39.52330221398023014 ) ) ;
#131087 = EDGE_LOOP ( 'NONE', ( #113680, #82721, #101751, #65430, #51448 ) ) ;
#131088 = EDGE_CURVE ( 'NONE', #32610, #136433, #112638, .T. ) ;
#131089 = CARTESIAN_POINT ( 'NONE',  ( -34.92500000000001137, 21.72500000000000142, 5.000000000000000000 ) ) ;
#131090 = PLANE ( 'NONE',  #141362 ) ;
#131091 = CARTESIAN_POINT ( 'NONE',  ( 24.18398860626899705, 28.73617430169804265, 5.000000000000000000 ) ) ;
#131092 = VECTOR ( 'NONE', #90652, 1000.000000000000227 ) ;
#131093 = EDGE_CURVE ( 'NONE', #105033, #131076, #114061, .T. ) ;
#131094 = EDGE_CURVE ( 'NONE', #101036, #40900, #59708, .T. ) ;
#131095 = DIRECTION ( 'NONE',  ( -0.000000000000000000, 0.000000000000000000, 1.000000000000000000 ) ) ;
#131097 = ORIENTED_EDGE ( 'NONE', *, *, #48877, .F. ) ;
#131096 = CARTESIAN_POINT ( 'NONE',  ( 23.63159235450331863, 3.061616997868375253E-16, -2.500000000000001332 ) ) ;
#131098 = CARTESIAN_POINT ( 'NONE',  ( 40.81250000000000000, 5.819803920172571310, 5.819803920172576639 ) ) ;
#131099 = CARTESIAN_POINT ( 'NONE',  ( 69.39583333333332860, -2.130196079827427091, 7.949999999999998401 ) ) ;
#131100 = DIRECTION ( 'NONE',  ( 0.000000000000000000, 0.000000000000000000, -1.000000000000000000 ) ) ;
#131101 = CARTESIAN_POINT ( 'NONE',  ( -26.99999999999980460, -12.41253812416063163, 4.000000000000000000 ) ) ;
#131102 =( GEOMETRIC_REPRESENTATION_CONTEXT ( 3 ) GLOBAL_UNCERTAINTY_ASSIGNED_CONTEXT ( ( #125885 ) ) GLOBAL_UNIT_ASSIGNED_CONTEXT ( ( #196, #54636, #33612 ) ) REPRESENTATION_CONTEXT ( 'NONE', 'WORKASPACE' ) );
#131103 = CARTESIAN_POINT ( 'NONE',  ( 77.99451991528749772, 28.92564299267992567, 4.000000000000000000 ) ) ;
#131104 = CIRCLE ( 'NONE', #68614, 2.500000000000000888 ) ;
#131105 = ORIENTED_EDGE ( 'NONE', *, *, #13047, .T. ) ;
#131106 = EDGE_LOOP ( 'NONE', ( #102755, #118509, #21236, #21517 ) ) ;
#131107 = ORIENTED_EDGE ( 'NONE', *, *, #19930, .T. ) ;
#131108 = VECTOR ( 'NONE', #81913, 1000.000000000000227 ) ;
#131109 = CARTESIAN_POINT ( 'NONE',  ( 95.95876352523144703, 0.000000000000000000, -6.110000000000001208 ) ) ;
#131110 = ORIENTED_EDGE ( 'NONE', *, *, #64502, .T. ) ;
#131111 = EDGE_CURVE ( 'NONE', #49923, #91902, #60431, .T. ) ;
#131112 = AXIS2_PLACEMENT_3D ( 'NONE', #87765, #75473, #21793 ) ;
#131113 = CARTESIAN_POINT ( 'NONE',  ( 125.6094186379952049, -46.07581969935596078, 35.63601533997828597 ) ) ;
#131114 = VECTOR ( 'NONE', #52940, 1000.000000000000000 ) ;
#131115 = CARTESIAN_POINT ( 'NONE',  ( 83.93336038379621300, 2.130196079827431532, -7.949999999999996625 ) ) ;
#131116 = ORIENTED_EDGE ( 'NONE', *, *, #17682, .T. ) ;
#131117 = EDGE_CURVE ( 'NONE', #111746, #133264, #96553, .T. ) ;
#131118 = DIRECTION ( 'NONE',  ( 0.6830127018922181881, 0.6830127018922202975, -0.2588190451025214056 ) ) ;
#131119 = CARTESIAN_POINT ( 'NONE',  ( 48.83333333333332860, -6.884901960086287964, 3.974999999999998312 ) ) ;
#131120 = CARTESIAN_POINT ( 'NONE',  ( 92.51626352523146579, -4.472830434245839371, 4.472830434245839371 ) ) ;
#131121 = VERTEX_POINT ( 'NONE', #140792 ) ;
#131122 = CARTESIAN_POINT ( 'NONE',  ( 0.5741843527964840543, 0.5999999999999987566, -4.263785792382349449 ) ) ;
#131123 = CARTESIAN_POINT ( 'NONE',  ( 0.000000000000000000, 0.000000000000000000, 6.750000000000000888 ) ) ;
#131124 = VERTEX_POINT ( 'NONE', #6681 ) ;
#131125 = VERTEX_POINT ( 'NONE', #41490 ) ;
#131126 = ORIENTED_EDGE ( 'NONE', *, *, #56529, .T. ) ;
#131127 = PLANE ( 'NONE',  #32985 ) ;
#131128 = CARTESIAN_POINT ( 'NONE',  ( 6.604862331875168913, 21.75929247661549937, 21.32995629748185351 ) ) ;
#131129 = CARTESIAN_POINT ( 'NONE',  ( 17.85873647476855197, 5.808823158059031044, -5.808823158059037262 ) ) ;
#131130 = CARTESIAN_POINT ( 'NONE',  ( 11.67183060077639212, -15.74070752338412760, 4.000000000000000000 ) ) ;
#131131 = EDGE_CURVE ( 'NONE', #21371, #131987, #74877, .T. ) ;
#131132 = CARTESIAN_POINT ( 'NONE',  ( 166.7105211023042841, 26.96999999999993491, 32.60830646801873201 ) ) ;
#131133 = CARTESIAN_POINT ( 'NONE',  ( 7.139999999999992575, -35.14999999999999858, -39.50000000000000000 ) ) ;
#131134 = EDGE_CURVE ( 'NONE', #71156, #84656, #85698, .T. ) ;
#131135 = EDGE_CURVE ( 'NONE', #22146, #1800, #74136, .T. ) ;
#131136 = ORIENTED_EDGE ( 'NONE', *, *, #118380, .T. ) ;
#131137 = ORIENTED_EDGE ( 'NONE', *, *, #143348, .F. ) ;
#131138 = LINE ( 'NONE', #110077, #43345 ) ;
#131139 = VERTEX_POINT ( 'NONE', #128521 ) ;
#131140 = VERTEX_POINT ( 'NONE', #39380 ) ;
#131141 = VECTOR ( 'NONE', #55678, 1000.000000000000227 ) ;
#131142 = LINE ( 'NONE', #20207, #33553 ) ;
#131143 = ORIENTED_EDGE ( 'NONE', *, *, #68404, .T. ) ;
#131144 = DIRECTION ( 'NONE',  ( -0.000000000000000000, 0.000000000000000000, 1.000000000000000000 ) ) ;
#131145 = CARTESIAN_POINT ( 'NONE',  ( 13.13598696172163116, 4.584330080086930965E-16, 0.000000000000000000 ) ) ;
#131146 = DIRECTION ( 'NONE',  ( 1.000000000000000000, 0.000000000000000000, -0.000000000000000000 ) ) ;
#131147 = VECTOR ( 'NONE', #66356, 1000.000000000000000 ) ;
#131148 = CARTESIAN_POINT ( 'NONE',  ( -21.48921356237309155, -27.52281430457070499, 5.000000000000000000 ) ) ;
#131149 = ORIENTED_EDGE ( 'NONE', *, *, #89907, .T. ) ;
#131150 = DIRECTION ( 'NONE',  ( -0.7071067811865487940, 0.7071067811865463515, 0.000000000000000000 ) ) ;
#131151 = ORIENTED_EDGE ( 'NONE', *, *, #118601, .T. ) ;
#131152 = LINE ( 'NONE', #63074, #71294 ) ;
#131153 = ORIENTED_EDGE ( 'NONE', *, *, #12082, .T. ) ;
#131154 =( NAMED_UNIT ( * ) PLANE_ANGLE_UNIT ( ) SI_UNIT ( $, .RADIAN. ) );
#131155 = ORIENTED_EDGE ( 'NONE', *, *, #80303, .T. ) ;
#131156 = DIRECTION ( 'NONE',  ( -0.7071067811865487940, 0.7071067811865463515, 0.000000000000000000 ) ) ;
#131157 = ORIENTED_EDGE ( 'NONE', *, *, #33885, .T. ) ;
#131158 = ORIENTED_EDGE ( 'NONE', *, *, #15946, .F. ) ;
#131159 = ORIENTED_EDGE ( 'NONE', *, *, #67809, .F. ) ;
#131160 = VECTOR ( 'NONE', #32954, 1000.000000000000227 ) ;
#131161 = CARTESIAN_POINT ( 'NONE',  ( 14.54487008052911534, -0.7407075233842805861, 4.335043535661647240 ) ) ;
#131162 = PLANE ( 'NONE',  #143319 ) ;
#131163 = CARTESIAN_POINT ( 'NONE',  ( 19.28515664589288292, 1.963325189347669086, -33.49048331797055766 ) ) ;
#131164 = DIRECTION ( 'NONE',  ( 0.000000000000000000, -1.000000000000000000, 0.000000000000000000 ) ) ;
#131165 = LINE ( 'NONE', #142069, #54398 ) ;
#131166 = ADVANCED_FACE ( 'NONE', ( #19031 ), #119051, .F. ) ;
#131167 = DIRECTION ( 'NONE',  ( -0.7071067811865486830, -0.7071067811865464625, -0.000000000000000000 ) ) ;
#131168 = DIRECTION ( 'NONE',  ( -0.7071067811865487940, 0.7071067811865463515, -0.000000000000000000 ) ) ;
#131169 = CARTESIAN_POINT ( 'NONE',  ( 34.49999999999975131, 22.21934299833216642, 4.348028800457638177 ) ) ;
#131170 = PLANE ( 'NONE',  #133907 ) ;
#131171 = LINE ( 'NONE', #64489, #36692 ) ;
#131172 = DIRECTION ( 'NONE',  ( 0.000000000000000000, -1.000000000000000000, 0.000000000000000000 ) ) ;
#131173 = VECTOR ( 'NONE', #31664, 1000.000000000000000 ) ;
#131174 = ORIENTED_EDGE ( 'NONE', *, *, #38660, .T. ) ;
#131175 = ORIENTED_EDGE ( 'NONE', *, *, #138417, .T. ) ;
#131176 = VERTEX_POINT ( 'NONE', #73430 ) ;
#131177 = CARTESIAN_POINT ( 'NONE',  ( -7.940000000000001279, -60.26999999999998892, -8.101350000000007157 ) ) ;
#131178 = ORIENTED_EDGE ( 'NONE', *, *, #23020, .T. ) ;
#131180 = ORIENTED_EDGE ( 'NONE', *, *, #28759, .F. ) ;
#131179 = ADVANCED_FACE ( 'NONE', ( #84325 ), #137973, .F. ) ;
#131181 = DIRECTION ( 'NONE',  ( 0.7071067811865486830, -0.7071067811865464625, -0.000000000000000000 ) ) ;
#131182 = DIRECTION ( 'NONE',  ( 0.7071067811865487940, 0.7071067811865463515, 0.000000000000000000 ) ) ;
#131183 = VECTOR ( 'NONE', #140224, 1000.000000000000000 ) ;
#131184 = EDGE_CURVE ( 'NONE', #54005, #132339, #72028, .T. ) ;
#131185 = ADVANCED_FACE ( 'NONE', ( #38653 ), #72533, .T. ) ;
#131186 = DIRECTION ( 'NONE',  ( -0.6830127018922180770, -0.6830127018922204085, -0.2588190451025213501 ) ) ;
#131187 = ORIENTED_EDGE ( 'NONE', *, *, #59822, .F. ) ;
#131188 = DIRECTION ( 'NONE',  ( -0.7071067811865486830, -0.7071067811865464625, 0.000000000000000000 ) ) ;
#131189 = ORIENTED_EDGE ( 'NONE', *, *, #31581, .F. ) ;
#131190 = VECTOR ( 'NONE', #756, 1000.000000000000227 ) ;
#131193 = ADVANCED_FACE ( 'NONE', ( #117594 ), #95872, .F. ) ;
#131192 = PLANE ( 'NONE',  #35256 ) ;
#131191 = VECTOR ( 'NONE', #57343, 1000.000000000000000 ) ;
#131194 = ADVANCED_FACE ( 'NONE', ( #138694 ), #105320, .T. ) ;
#131195 = CARTESIAN_POINT ( 'NONE',  ( 34.92499999999998295, 5.816654386410395894, 4.500000000000000888 ) ) ;
#131196 = AXIS2_PLACEMENT_3D ( 'NONE', #82800, #38566, #101666 ) ;
#131197 = CARTESIAN_POINT ( 'NONE',  ( 20.77540314143522338, -2.126176841940958351, -7.934999999999989839 ) ) ;
#131198 = ORIENTED_EDGE ( 'NONE', *, *, #3851, .F. ) ;
#131199 = CARTESIAN_POINT ( 'NONE',  ( 94.99543019189812298, 5.291415217122917625, 3.055000000000002380 ) ) ;
#131200 = DIRECTION ( 'NONE',  ( 0.5735764363510444941, 0.8191520442889929088, 0.000000000000000000 ) ) ;
#131201 = EDGE_CURVE ( 'NONE', #101752, #41149, #14320, .T. ) ;
#131202 = CARTESIAN_POINT ( 'NONE',  ( 55.18164086290597226, -52.14999999999999147, -41.64500000000000313 ) ) ;
#131203 = DIRECTION ( 'NONE',  ( 0.000000000000000000, -1.000000000000000000, 0.000000000000000000 ) ) ;
#131204 = ORIENTED_EDGE ( 'NONE', *, *, #98369, .T. ) ;
#131205 = ORIENTED_EDGE ( 'NONE', *, *, #41097, .T. ) ;
#131206 = DIRECTION ( 'NONE',  ( -1.000000000000000000, -1.224606353822377258E-16, -0.000000000000000000 ) ) ;
#131207 = ORIENTED_EDGE ( 'NONE', *, *, #74400, .F. ) ;
#131208 = CARTESIAN_POINT ( 'NONE',  ( -2.526639036357837487, -5.240707523384232402, 16.25846745537495153 ) ) ;
#131209 = VECTOR ( 'NONE', #49962, 999.9999999999998863 ) ;
#131210 = CARTESIAN_POINT ( 'NONE',  ( -11.99999999999991651, -3.033600742197707145, 5.000000000000000000 ) ) ;
#131211 = CARTESIAN_POINT ( 'NONE',  ( 181.1499999999998067, -47.62213595499956398, -36.92499999999996163 ) ) ;
#131212 = EDGE_LOOP ( 'NONE', ( #88975, #4289, #74820, #95531 ) ) ;
#131213 = DIRECTION ( 'NONE',  ( -0.7071067811865486830, -0.7071067811865464625, 0.000000000000000000 ) ) ;
#131214 = ADVANCED_FACE ( 'NONE', ( #77711 ), #120442, .F. ) ;
#131215 = DIRECTION ( 'NONE',  ( 0.000000000000000000, -0.3543493200069152138, 0.9351131265310292928 ) ) ;
#131216 = LINE ( 'NONE', #118162, #76942 ) ;
#131217 = ORIENTED_EDGE ( 'NONE', *, *, #74245, .T. ) ;
#131218 = DIRECTION ( 'NONE',  ( 1.000000000000000000, 1.369518533665899572E-16, 0.000000000000000000 ) ) ;
#131219 = EDGE_CURVE ( 'NONE', #63455, #60759, #9555, .T. ) ;
#131220 = CARTESIAN_POINT ( 'NONE',  ( -14.29289321881335084, -12.74070752338415247, 5.000000000000000000 ) ) ;
#131221 = ORIENTED_EDGE ( 'NONE', *, *, #37149, .T. ) ;
#131223 = ORIENTED_EDGE ( 'NONE', *, *, #140215, .T. ) ;
#131222 = DIRECTION ( 'NONE',  ( -0.7071067811865486830, -0.7071067811865464625, -0.000000000000000000 ) ) ;
#131224 = ORIENTED_EDGE ( 'NONE', *, *, #36486, .T. ) ;
#131225 = DIRECTION ( 'NONE',  ( 0.7071067811865486830, -0.7071067811865464625, -0.000000000000000000 ) ) ;
#131226 = CARTESIAN_POINT ( 'NONE',  ( 34.92499999999998295, -21.72500000000000142, 5.000000000000000000 ) ) ;
#131227 = EDGE_CURVE ( 'NONE', #26091, #135979, #55978, .T. ) ;
#131228 = ORIENTED_EDGE ( 'NONE', *, *, #25740, .T. ) ;
#131229 = LINE ( 'NONE', #74735, #37319 ) ;
#131230 = LINE ( 'NONE', #87728, #33630 ) ;
#131231 = AXIS2_PLACEMENT_3D ( 'NONE', #30272, #52723, #63647 ) ;
#131232 = DIRECTION ( 'NONE',  ( 0.7071067811865486830, -0.7071067811865464625, -0.000000000000000000 ) ) ;
#131233 = PLANE ( 'NONE',  #76275 ) ;
#131234 = CARTESIAN_POINT ( 'NONE',  ( -11.67183060077638856, -12.74070752338415602, 4.000000000000000000 ) ) ;
#131235 = DIRECTION ( 'NONE',  ( 0.7071067811865487940, 0.7071067811865463515, -0.000000000000000000 ) ) ;
#131237 = EDGE_CURVE ( 'NONE', #103116, #44686, #8811, .T. ) ;
#131236 = LINE ( 'NONE', #1404, #56512 ) ;
#131238 = SURFACE_STYLE_FILL_AREA ( #97902 ) ;
#131239 = CARTESIAN_POINT ( 'NONE',  ( -26.22995720542188991, 21.73644205237998150, 5.000000000000000888 ) ) ;
#131241 = AXIS2_PLACEMENT_3D ( 'NONE', #38393, #82609, #39846 ) ;
#131240 = FACE_OUTER_BOUND ( 'NONE', #68161, .T. ) ;
#131242 = DIRECTION ( 'NONE',  ( -0.000000000000000000, -0.3543493200069152693, 0.9351131265310292928 ) ) ;
#131243 = DIRECTION ( 'NONE',  ( 0.7071067811865487940, 0.7071067811865463515, 0.000000000000000000 ) ) ;
#131244 = CARTESIAN_POINT ( 'NONE',  ( -26.20710678118635428, -17.24070752338410273, 5.000000000000000000 ) ) ;
#131245 = VERTEX_POINT ( 'NONE', #31348 ) ;
#131246 = ORIENTED_EDGE ( 'NONE', *, *, #80816, .T. ) ;
#131247 = ORIENTED_EDGE ( 'NONE', *, *, #4013, .F. ) ;
#131248 = EDGE_CURVE ( 'NONE', #57055, #136234, #67658, .T. ) ;
#131249 = CARTESIAN_POINT ( 'NONE',  ( 97.97916666666668561, -7.950000000000001066, 2.130196079827424427 ) ) ;
#131250 = VERTEX_POINT ( 'NONE', #66131 ) ;
#131251 = ORIENTED_EDGE ( 'NONE', *, *, #13851, .F. ) ;
#131252 = EDGE_CURVE ( 'NONE', #126555, #60629, #45112, .T. ) ;
#131253 = ORIENTED_EDGE ( 'NONE', *, *, #72386, .T. ) ;
#131254 = AXIS2_PLACEMENT_3D ( 'NONE', #86505, #9611, #129260 ) ;
#131255 = DIRECTION ( 'NONE',  ( -0.000000000000000000, 0.000000000000000000, 1.000000000000000000 ) ) ;
#131256 = CARTESIAN_POINT ( 'NONE',  ( 89.95833333333332860, 3.974999999999997424, 6.884901960086288852 ) ) ;
#131257 = ORIENTED_EDGE ( 'NONE', *, *, #142063, .T. ) ;
#131258 = LINE ( 'NONE', #87754, #64893 ) ;
#131259 = EDGE_CURVE ( 'NONE', #91901, #26770, #53070, .T. ) ;
#131260 = LINE ( 'NONE', #120335, #60376 ) ;
#131262 = VECTOR ( 'NONE', #76054, 1000.000000000000000 ) ;
#131261 = DIRECTION ( 'NONE',  ( -1.000000000000000000, -1.224606353822377258E-16, -0.000000000000000000 ) ) ;
#131263 = CARTESIAN_POINT ( 'NONE',  ( 4.658131166821905644, 3.061616997868383634E-16, -2.500000000000000444 ) ) ;
#131264 = VERTEX_POINT ( 'NONE', #54541 ) ;
#131265 = DIRECTION ( 'NONE',  ( -1.000000000000000000, -1.224606353822377258E-16, -0.000000000000000000 ) ) ;
#131266 = CARTESIAN_POINT ( 'NONE',  ( 15.79333936457837062, 21.75929247661549937, 4.998822639870715179 ) ) ;
#131267 = CARTESIAN_POINT ( 'NONE',  ( 24.30132219248945447, 6.014229859109025966, 4.331046227559734341 ) ) ;
#131268 = CARTESIAN_POINT ( 'NONE',  ( -75.18398860626899705, 28.73617430169839793, 5.000000000000000000 ) ) ;
#131269 = DIRECTION ( 'NONE',  ( -0.7071067811865487940, 0.7071067811865463515, -0.000000000000000000 ) ) ;
#131270 = CARTESIAN_POINT ( 'NONE',  ( 31.28752705046289151, 0.000000000000000000, -7.949999999999998401 ) ) ;
#131271 = AXIS2_PLACEMENT_3D ( 'NONE', #78396, #132078, #122593 ) ;
#131272 = FACE_OUTER_BOUND ( 'NONE', #125236, .T. ) ;
#131273 = VERTEX_POINT ( 'NONE', #77016 ) ;
#131274 = EDGE_LOOP ( 'NONE', ( #65562, #105138, #102091, #103854 ) ) ;
#131275 = CARTESIAN_POINT ( 'NONE',  ( 117.2504301918981042, 3.055000000000002824, -5.291415217122919401 ) ) ;
#131276 = VECTOR ( 'NONE', #46858, 1000.000000000000000 ) ;
#131277 = ORIENTED_EDGE ( 'NONE', *, *, #127537, .F. ) ;
#131278 = EDGE_CURVE ( 'NONE', #108755, #101225, #98718, .T. ) ;
#131279 = PLANE ( 'NONE',  #15884 ) ;
#131280 = DIRECTION ( 'NONE',  ( 0.000000000000000000, 0.000000000000000000, -1.000000000000000000 ) ) ;
#131281 = DIRECTION ( 'NONE',  ( -1.000000000000000000, -1.224606353822377258E-16, -0.000000000000000000 ) ) ;
#131282 = EDGE_CURVE ( 'NONE', #71076, #47430, #87860, .T. ) ;
#131283 = DIRECTION ( 'NONE',  ( 0.3543493200069162685, -0.000000000000000000, -0.9351131265310288487 ) ) ;
#131284 = DIRECTION ( 'NONE',  ( -0.3543493200069162685, -0.000000000000000000, -0.9351131265310288487 ) ) ;
#131285 = SURFACE_STYLE_USAGE ( .BOTH. , #87069 ) ;
#131286 = CARTESIAN_POINT ( 'NONE',  ( 122.8495968585647518, 6.109999999999996767, 1.637169565754163836 ) ) ;
#131287 = EDGE_LOOP ( 'NONE', ( #102638, #129997, #27436, #55037 ) ) ;
#131288 = ORIENTED_EDGE ( 'NONE', *, *, #125978, .F. ) ;
#131289 = CARTESIAN_POINT ( 'NONE',  ( -25.49999999999982236, -2.568876922607784774, 4.000000000000000000 ) ) ;
#131290 = CARTESIAN_POINT ( 'NONE',  ( 30.18398860626900060, 28.73617430169808173, 5.000000000000000000 ) ) ;
#131291 = LINE ( 'NONE', #122351, #113560 ) ;
#131292 = CARTESIAN_POINT ( 'NONE',  ( -21.29974487139158512, -27.71228299555221142, 4.000000000000000000 ) ) ;
#131293 = ORIENTED_EDGE ( 'NONE', *, *, #71240, .T. ) ;
#131294 = CIRCLE ( 'NONE', #82660, 2.500000000000000888 ) ;
#131295 = CARTESIAN_POINT ( 'NONE',  ( 47.25043019189810423, 3.055000000000002824, -5.291415217122919401 ) ) ;
#131296 = ORIENTED_EDGE ( 'NONE', *, *, #104845, .F. ) ;
#131297 = DIRECTION ( 'NONE',  ( 0.7071067811865487940, 0.7071067811865463515, 0.000000000000000000 ) ) ;
#131298 = CARTESIAN_POINT ( 'NONE',  ( -35.99451991528749772, 28.92564299267963079, 4.000000000000000000 ) ) ;
#131299 = CARTESIAN_POINT ( 'NONE',  ( 33.48921356237309510, -27.52281430457078670, 5.000000000000000000 ) ) ;
#131300 = DIRECTION ( 'NONE',  ( -0.6830127018922181881, 0.6830127018922202975, -0.2588190451025214056 ) ) ;
#131301 = VECTOR ( 'NONE', #66251, 1000.000000000000000 ) ;
#131302 = VECTOR ( 'NONE', #15047, 1000.000000000000000 ) ;
#131303 = ADVANCED_FACE ( 'NONE', ( #21171 ), #78419, .F. ) ;
#131304 = VECTOR ( 'NONE', #133436, 999.9999999999998863 ) ;
#131305 = CARTESIAN_POINT ( 'NONE',  ( 38.41209685856478018, 5.291415217122921177, -3.054999999999994831 ) ) ;
#131306 = ORIENTED_EDGE ( 'NONE', *, *, #88553, .T. ) ;
#131307 = VECTOR ( 'NONE', #45493, 999.9999999999998863 ) ;
#131308 = DIRECTION ( 'NONE',  ( -0.6830127018922181881, 0.6830127018922202975, -0.2588190451025214056 ) ) ;
#131309 = EDGE_LOOP ( 'NONE', ( #54785, #51014, #108375, #138217 ) ) ;
#131310 = EDGE_LOOP ( 'NONE', ( #54075, #28379, #44783, #127505 ) ) ;
#131311 = PRESENTATION_LAYER_ASSIGNMENT (  '', '', ( #115025 ) ) ;
#131312 = ORIENTED_EDGE ( 'NONE', *, *, #77429, .F. ) ;
#131313 = EDGE_CURVE ( 'NONE', #2249, #67897, #32054, .T. ) ;
#131314 = CARTESIAN_POINT ( 'NONE',  ( -34.49999999999976552, 1.464255608400471642, 4.994342998332163219 ) ) ;
#131315 = PLANE ( 'NONE',  #60764 ) ;
#131316 = ORIENTED_EDGE ( 'NONE', *, *, #134896, .F. ) ;
#131317 = CARTESIAN_POINT ( 'NONE',  ( 2.999999999999981792, 14.87792677143809073, -11.06722581663439264 ) ) ;
#131318 = PLANE ( 'NONE',  #32043 ) ;
#131319 =( BOUNDED_CURVE ( )  B_SPLINE_CURVE ( 3, ( #12265, #89138, #101417, #102867 ),
 .UNSPECIFIED., .F., .F. ) 
 B_SPLINE_CURVE_WITH_KNOTS ( ( 4, 4 ),
 ( 4.350170835173029715, 4.500739107949200957 ),
 .UNSPECIFIED. ) 
 CURVE ( )  GEOMETRIC_REPRESENTATION_ITEM ( )  RATIONAL_B_SPLINE_CURVE ( ( 1.000000000000000000, 0.9981116584018959736, 0.9981116584018959736, 1.000000000000000000 ) ) 
 REPRESENTATION_ITEM ( '' )  );
#131320 = CARTESIAN_POINT ( 'NONE',  ( 22.77149322861322034, 20.25929247661551003, 7.808871592221821700 ) ) ;
#131321 = FACE_BOUND ( 'NONE', #11627, .T. ) ;
#131323 = EDGE_CURVE ( 'NONE', #38880, #73106, #10973, .T. ) ;
#131322 = EDGE_LOOP ( 'NONE', ( #14644, #87842, #52574, #138102 ) ) ;
#131324 = DIRECTION ( 'NONE',  ( -0.6830127018922181881, 0.6830127018922202975, -0.2588190451025214056 ) ) ;
#131325 = CARTESIAN_POINT ( 'NONE',  ( -17.70025512860841488, -27.71228299555193786, 4.000000000000000000 ) ) ;
#131326 = FACE_OUTER_BOUND ( 'NONE', #137419, .T. ) ;
#131327 = ORIENTED_EDGE ( 'NONE', *, *, #62906, .F. ) ;
#131328 = CARTESIAN_POINT ( 'NONE',  ( -14.99999999999989519, 11.96639925780214675, 5.000000000000000000 ) ) ;
#131329 = ORIENTED_EDGE ( 'NONE', *, *, #39321, .F. ) ;
#131330 = AXIS2_PLACEMENT_3D ( 'NONE', #29020, #73254, #27570 ) ;
#131331 = ORIENTED_EDGE ( 'NONE', *, *, #142429, .T. ) ;
#131332 = CARTESIAN_POINT ( 'NONE',  ( 10.49999999999992895, -19.91253812416055169, 4.000000000000000000 ) ) ;
#131333 = ORIENTED_EDGE ( 'NONE', *, *, #135003, .F. ) ;
#131334 = CARTESIAN_POINT ( 'NONE',  ( 57.22459685856477307, -1.637169565754160949, 6.109999999999997655 ) ) ;
#131335 = AXIS2_PLACEMENT_3D ( 'NONE', #71673, #94806, #139069 ) ;
#131336 = ORIENTED_EDGE ( 'NONE', *, *, #140735, .F. ) ;
#131337 = DIRECTION ( 'NONE',  ( -0.7071067811865487940, 0.7071067811865463515, 0.000000000000000000 ) ) ;
#131338 = ORIENTED_EDGE ( 'NONE', *, *, #74200, .F. ) ;
#131339 = CARTESIAN_POINT ( 'NONE',  ( -24.32816939922335919, 17.25929247661554555, 4.000000000000000000 ) ) ;
#131340 = LINE ( 'NONE', #142240, #46457 ) ;
#131341 = ORIENTED_EDGE ( 'NONE', *, *, #118575, .T. ) ;
#131342 = LINE ( 'NONE', #87832, #118580 ) ;
#131343 = CARTESIAN_POINT ( 'NONE',  ( -29.99999999999979039, -8.151047557385094677, -8.977947279169729455 ) ) ;
#131344 = AXIS2_PLACEMENT_3D ( 'NONE', #2452, #11911, #57604 ) ;
#131345 = CARTESIAN_POINT ( 'NONE',  ( -63.18398860626900415, 28.73617430169831621, 5.000000000000000000 ) ) ;
#131346 = DIRECTION ( 'NONE',  ( 0.000000000000000000, 0.000000000000000000, -1.000000000000000000 ) ) ;
#131347 = DIRECTION ( 'NONE',  ( 0.7071067811865487940, 0.7071067811865463515, 0.000000000000000000 ) ) ;
#131348 = DIRECTION ( 'NONE',  ( 0.000000000000000000, -1.000000000000000000, 0.000000000000000000 ) ) ;
#131349 = DIRECTION ( 'NONE',  ( 0.6830127018922181881, 0.6830127018922202975, -0.2588190451025214056 ) ) ;
#131350 = EDGE_LOOP ( 'NONE', ( #118012, #2266, #63754, #44440 ) ) ;
#131351 = EDGE_CURVE ( 'NONE', #104048, #78195, #21880, .T. ) ;
#131352 = VECTOR ( 'NONE', #67262, 1000.000000000000000 ) ;
#131353 = ORIENTED_EDGE ( 'NONE', *, *, #54129, .F. ) ;
#131354 = ORIENTED_EDGE ( 'NONE', *, *, #72353, .F. ) ;
#131355 = CARTESIAN_POINT ( 'NONE',  ( 11.70025512860841133, -27.71228299555198049, 4.000000000000000000 ) ) ;
#131356 = DIRECTION ( 'NONE',  ( -0.7071067811865486830, -0.7071067811865464625, 0.000000000000000000 ) ) ;
#131357 = ORIENTED_EDGE ( 'NONE', *, *, #89955, .F. ) ;
#131358 = EDGE_CURVE ( 'NONE', #27120, #27213, #64690, .T. ) ;
#131359 = VERTEX_POINT ( 'NONE', #11687 ) ;
#131360 = CARTESIAN_POINT ( 'NONE',  ( 24.18398860626899705, 28.73617430169804265, 5.000000000000000000 ) ) ;
#131361 = DIRECTION ( 'NONE',  ( 0.7071067811865487940, 0.7071067811865463515, 0.000000000000000000 ) ) ;
#131362 = VECTOR ( 'NONE', #49155, 1000.000000000000000 ) ;
#131363 = ADVANCED_FACE ( 'NONE', ( #44390 ), #97265, .F. ) ;
#131364 = EDGE_CURVE ( 'NONE', #61426, #141239, #95336, .T. ) ;
#131365 = DIRECTION ( 'NONE',  ( 1.000000000000000000, 0.000000000000000000, 0.000000000000000000 ) ) ;
#131366 = ORIENTED_EDGE ( 'NONE', *, *, #10751, .F. ) ;
#131367 = CARTESIAN_POINT ( 'NONE',  ( 12.79289321881337393, -11.24070752338416845, 5.000000000000000000 ) ) ;
#131369 = ADVANCED_FACE ( 'NONE', ( #4342 ), #123369, .F. ) ;
#131368 = DIRECTION ( 'NONE',  ( 1.734723475976806848E-16, -1.000000000000000000, 0.000000000000000000 ) ) ;
#131370 = EDGE_CURVE ( 'NONE', #1453, #38684, #55948, .T. ) ;
#131371 = CARTESIAN_POINT ( 'NONE',  ( 19.46290314143521982, -3.967499999999994476, 6.871911579029513106 ) ) ;
#131372 = LINE ( 'NONE', #75571, #66969 ) ;
#131373 = ADVANCED_FACE ( 'NONE', ( #122616 ), #124060, .T. ) ;
#131374 = ORIENTED_EDGE ( 'NONE', *, *, #11517, .F. ) ;
#131375 = CARTESIAN_POINT ( 'NONE',  ( 124.0162635252314658, -4.472830434245839371, 4.472830434245839371 ) ) ;
#131376 = VECTOR ( 'NONE', #112429, 999.9999999999998863 ) ;
#131377 = STYLED_ITEM ( 'NONE', ( #27475 ), #4147 ) ;
#131378 = EDGE_CURVE ( 'NONE', #132753, #105598, #135547, .T. ) ;
#131379 = CARTESIAN_POINT ( 'NONE',  ( 23.66989781452720365, 17.25929247661554555, 19.83885114516066039 ) ) ;
#131380 = LINE ( 'NONE', #40804, #35730 ) ;
#131382 = ORIENTED_EDGE ( 'NONE', *, *, #106, .T. ) ;
#131381 = DIRECTION ( 'NONE',  ( 0.7071067811865487940, -0.7071067811865463515, 0.000000000000000000 ) ) ;
#131383 = FACE_OUTER_BOUND ( 'NONE', #1750, .T. ) ;
#131384 = ORIENTED_EDGE ( 'NONE', *, *, #98051, .T. ) ;
#131385 = EDGE_CURVE ( 'NONE', #43329, #110223, #56707, .T. ) ;
#131386 = LINE ( 'NONE', #120454, #116821 ) ;
#131387 = LINE ( 'NONE', #66146, #137271 ) ;
#131388 = DIRECTION ( 'NONE',  ( -0.7071067811865486830, -0.7071067811865464625, 0.000000000000000000 ) ) ;
#131389 = ORIENTED_EDGE ( 'NONE', *, *, #30229, .T. ) ;
#131390 = EDGE_CURVE ( 'NONE', #42684, #10551, #113609, .T. ) ;
#131391 = VECTOR ( 'NONE', #69223, 1000.000000000000000 ) ;
#131392 = FACE_OUTER_BOUND ( 'NONE', #126136, .T. ) ;
#131393 = CARTESIAN_POINT ( 'NONE',  ( -1.171830600776458509, -2.240707523384264377, 4.000000000000000000 ) ) ;
#131394 = EDGE_LOOP ( 'NONE', ( #120570, #105721, #16646, #6118 ) ) ;
#131395 = CARTESIAN_POINT ( 'NONE',  ( -4.499999999999962697, 9.052185695429074030, 5.000000000000000000 ) ) ;
#131396 = PRESENTATION_LAYER_ASSIGNMENT (  '', '', ( #101571 ) ) ;
#131397 = CARTESIAN_POINT ( 'NONE',  ( -34.49999999999975131, -17.91344420646045421, 1.358650452708383138 ) ) ;
#131398 = ORIENTED_EDGE ( 'NONE', *, *, #126904, .F. ) ;
#131399 = EDGE_CURVE ( 'NONE', #62769, #98772, #36343, .T. ) ;
#131400 = VECTOR ( 'NONE', #43958, 1000.000000000000000 ) ;
#131401 = DIRECTION ( 'NONE',  ( 0.7071067811865486830, -0.7071067811865464625, -0.000000000000000000 ) ) ;
#131403 = EDGE_LOOP ( 'NONE', ( #91878, #58431, #61618, #50721, #33766, #104842 ) ) ;
#131402 = CARTESIAN_POINT ( 'NONE',  ( 0.1839886062690032631, 28.73617430169787568, 5.000000000000000000 ) ) ;
#131404 = ORIENTED_EDGE ( 'NONE', *, *, #103539, .T. ) ;
#131405 = LINE ( 'NONE', #42982, #114323 ) ;
#131406 = DIRECTION ( 'NONE',  ( 0.3543493200069163240, -0.000000000000000000, -0.9351131265310288487 ) ) ;
#131407 = EDGE_CURVE ( 'NONE', #132567, #131487, #101573, .T. ) ;
#131408 = AXIS2_PLACEMENT_3D ( 'NONE', #118187, #52935, #74745 ) ;
#131409 = ORIENTED_EDGE ( 'NONE', *, *, #142272, .T. ) ;
#131410 = STYLED_ITEM ( 'NONE', ( #119016 ), #137587 ) ;
#131411 = LINE ( 'NONE', #32827, #101507 ) ;
#131412 = VECTOR ( 'NONE', #6962, 1000.000000000000000 ) ;
#131413 = DIRECTION ( 'NONE',  ( -1.000000000000000000, -0.000000000000000000, -0.000000000000000000 ) ) ;
#131414 = DIRECTION ( 'NONE',  ( -8.673617379884034239E-17, 1.000000000000000000, 0.000000000000000000 ) ) ;
#131415 = EDGE_LOOP ( 'NONE', ( #29504, #62239, #133567, #59847 ) ) ;
#131416 = CARTESIAN_POINT ( 'NONE',  ( -57.18398860626899705, 28.73617430169827358, 5.000000000000000000 ) ) ;
#131417 = CARTESIAN_POINT ( 'NONE',  ( 42.29974487139158157, -27.71228299555235708, 4.000000000000000000 ) ) ;
#131418 = CARTESIAN_POINT ( 'NONE',  ( -24.48921356237309510, -27.52281430457072631, 5.000000000000000000 ) ) ;
#131419 = AXIS2_PLACEMENT_3D ( 'NONE', #54131, #142543, #51963 ) ;
#131420 = CARTESIAN_POINT ( 'NONE',  ( -14.99451991528749595, 28.92564299267948513, 4.000000000000000000 ) ) ;
#131421 = CARTESIAN_POINT ( 'NONE',  ( 39.87043019189810877, -3.055000000000001936, 5.291415217122918513 ) ) ;
#131422 = DIRECTION ( 'NONE',  ( 0.7071067811865487940, 0.7071067811865463515, 0.000000000000000000 ) ) ;
#131423 = ORIENTED_EDGE ( 'NONE', *, *, #50499, .F. ) ;
#131424 = ORIENTED_EDGE ( 'NONE', *, *, #65527, .F. ) ;
#131425 = EDGE_CURVE ( 'NONE', #35489, #11869, #79167, .T. ) ;
#131426 = EDGE_LOOP ( 'NONE', ( #4332, #115547, #8743, #7722 ) ) ;
#131427 = EDGE_CURVE ( 'NONE', #133121, #82135, #13123, .T. ) ;
#131428 = VERTEX_POINT ( 'NONE', #57394 ) ;
#131429 = LINE ( 'NONE', #54591, #64096 ) ;
#131430 = LINE ( 'NONE', #74929, #87834 ) ;
#131431 = ORIENTED_EDGE ( 'NONE', *, *, #17851, .T. ) ;
#131432 = EDGE_CURVE ( 'NONE', #140149, #124115, #12025, .T. ) ;
#131433 = LINE ( 'NONE', #21232, #13823 ) ;
#131434 = CARTESIAN_POINT ( 'NONE',  ( -15.32816939922341959, -21.74070752338406365, 4.000000000000000000 ) ) ;
#131435 = CARTESIAN_POINT ( 'NONE',  ( 12.69999999999999574, -25.83999999999998565, 2.999999999999999112 ) ) ;
#131436 = DIRECTION ( 'NONE',  ( 0.000000000000000000, -1.000000000000000000, 0.000000000000000000 ) ) ;
#131437 = CYLINDRICAL_SURFACE ( 'NONE', #73245, 2.500000000000000000 ) ;
#131438 = ORIENTED_EDGE ( 'NONE', *, *, #15984, .F. ) ;
#131439 = LINE ( 'NONE', #32118, #102022 ) ;
#131440 = CARTESIAN_POINT ( 'NONE',  ( 152.4000000000000057, 7.919999999999947526, -18.97500000000001918 ) ) ;
#131441 = VECTOR ( 'NONE', #48831, 1000.000000000000000 ) ;
#131442 = LINE ( 'NONE', #85067, #98169 ) ;
#131443 = DIRECTION ( 'NONE',  ( 0.7071067811865486830, -0.7071067811865464625, -0.000000000000000000 ) ) ;
#131444 = PLANE ( 'NONE',  #123747 ) ;
#131445 = DIRECTION ( 'NONE',  ( -0.6830127018922180770, -0.6830127018922204085, -0.2588190451025213501 ) ) ;
#131446 = DIRECTION ( 'NONE',  ( -0.6830127018922181881, 0.6830127018922202975, -0.2588190451025214056 ) ) ;
#131447 = CARTESIAN_POINT ( 'NONE',  ( 57.97502705046289151, -5.819803920172572198, 5.819803920172572198 ) ) ;
#131448 = AXIS2_PLACEMENT_3D ( 'NONE', #127463, #48477, #103551 ) ;
#131449 = CARTESIAN_POINT ( 'NONE',  ( -15.18398860626900237, 28.73617430169797871, 5.000000000000000000 ) ) ;
#131450 = ORIENTED_EDGE ( 'NONE', *, *, #21329, .T. ) ;
#131451 = VERTEX_POINT ( 'NONE', #37041 ) ;
#131452 =( BOUNDED_CURVE ( )  B_SPLINE_CURVE ( 3, ( #103720, #82041, #116763, #137827 ),
 .UNSPECIFIED., .F., .T. ) 
 B_SPLINE_CURVE_WITH_KNOTS ( ( 4, 4 ),
 ( 1.570796326794896558, 3.141592653589793116 ),
 .UNSPECIFIED. ) 
 CURVE ( )  GEOMETRIC_REPRESENTATION_ITEM ( )  RATIONAL_B_SPLINE_CURVE ( ( 1.000000000000000000, 0.8047378541243649375, 0.8047378541243649375, 1.000000000000000000 ) ) 
 REPRESENTATION_ITEM ( '' )  );
#131453 = CARTESIAN_POINT ( 'NONE',  ( 55.68749999999999289, -5.819803920172573086, 5.819803920172572198 ) ) ;
#131454 = LINE ( 'NONE', #111660, #109488 ) ;
#131455 = ADVANCED_FACE ( 'NONE', ( #80571 ), #2237, .F. ) ;
#131456 = LINE ( 'NONE', #120530, #27730 ) ;
#131457 = DIRECTION ( 'NONE',  ( -0.6830127018922180770, -0.6830127018922204085, -0.2588190451025213501 ) ) ;
#131458 = EDGE_LOOP ( 'NONE', ( #51604, #56763, #44168, #23535 ) ) ;
#131459 = DIRECTION ( 'NONE',  ( -1.000000000000000000, -1.224606353822377258E-16, -0.000000000000000000 ) ) ;
#131460 = DIRECTION ( 'NONE',  ( 0.3543493200069162685, -0.000000000000000000, -0.9351131265310288487 ) ) ;
#131461 = CARTESIAN_POINT ( 'NONE',  ( 44.04209685856477563, 5.291415217122923842, -3.054999999999996163 ) ) ;
#131462 = EDGE_CURVE ( 'NONE', #116321, #2713, #58859, .T. ) ;
#131463 = ORIENTED_EDGE ( 'NONE', *, *, #70324, .F. ) ;
#131464 = CARTESIAN_POINT ( 'NONE',  ( -32.99999999999975842, 2.587461875839218273, 4.000000000000000000 ) ) ;
#131465 = ORIENTED_EDGE ( 'NONE', *, *, #68544, .F. ) ;
#131466 = ORIENTED_EDGE ( 'NONE', *, *, #13972, .F. ) ;
#131467 = DIRECTION ( 'NONE',  ( -0.6830127018922181881, 0.6830127018922202975, -0.2588190451025214056 ) ) ;
#131468 = DIRECTION ( 'NONE',  ( 0.000000000000000000, 1.000000000000000000, 0.000000000000000000 ) ) ;
#131469 = LINE ( 'NONE', #140202, #136865 ) ;
#131470 = DIRECTION ( 'NONE',  ( -0.6830127018922181881, 0.6830127018922202975, -0.2588190451025214056 ) ) ;
#131471 = VERTEX_POINT ( 'NONE', #2975 ) ;
#131472 = ADVANCED_FACE ( 'NONE', ( #25438 ), #42079, .T. ) ;
#131473 = LINE ( 'NONE', #8218, #4787 ) ;
#131475 = ORIENTED_EDGE ( 'NONE', *, *, #65362, .T. ) ;
#131474 = LINE ( 'NONE', #113089, #15135 ) ;
#131476 = CARTESIAN_POINT ( 'NONE',  ( 80.20876352523143282, -7.482591942790329030E-16, 6.110000000000001208 ) ) ;
#131477 = LINE ( 'NONE', #19834, #94751 ) ;
#131478 = SURFACE_STYLE_FILL_AREA ( #42345 ) ;
#131479 = EDGE_CURVE ( 'NONE', #69258, #129709, #50431, .T. ) ;
#131480 = ORIENTED_EDGE ( 'NONE', *, *, #121577, .F. ) ;
#131481 = AXIS2_PLACEMENT_3D ( 'NONE', #106161, #115589, #40261 ) ;
#131482 = CARTESIAN_POINT ( 'NONE',  ( 0.000000000000000000, -22.26999999999999247, -40.00000000000000000 ) ) ;
#131483 = CARTESIAN_POINT ( 'NONE',  ( 70.49543019189810877, 5.291415217122916737, 3.055000000000001936 ) ) ;
#131484 = DIRECTION ( 'NONE',  ( 0.7071067811865487940, 0.7071067811865463515, 0.000000000000000000 ) ) ;
#131485 = LINE ( 'NONE', #68405, #29259 ) ;
#131486 = DIRECTION ( 'NONE',  ( -0.7071067811865486830, -0.7071067811865464625, 0.000000000000000000 ) ) ;
#131487 = VERTEX_POINT ( 'NONE', #26180 ) ;
#131488 = EDGE_LOOP ( 'NONE', ( #30811, #26119, #47984, #75646 ) ) ;
#131489 = FACE_OUTER_BOUND ( 'NONE', #113945, .T. ) ;
#131490 = LINE ( 'NONE', #62671, #120911 ) ;
#131491 = ORIENTED_EDGE ( 'NONE', *, *, #88741, .F. ) ;
#131492 = EDGE_CURVE ( 'NONE', #97655, #141246, #75414, .T. ) ;
#131493 = ORIENTED_EDGE ( 'NONE', *, *, #46296, .F. ) ;
#131494 = AXIS2_PLACEMENT_3D ( 'NONE', #3733, #82093, #111839 ) ;
#131495 = EDGE_CURVE ( 'NONE', #32915, #135400, #94271, .T. ) ;
#131496 = LINE ( 'NONE', #33631, #136996 ) ;
#131497 = VERTEX_POINT ( 'NONE', #39938 ) ;
#131498 = CARTESIAN_POINT ( 'NONE',  ( -48.18398860626899705, 28.73617430169820608, 5.000000000000000000 ) ) ;
#131499 = DIRECTION ( 'NONE',  ( -0.7071067811865486830, 0.7071067811865464625, 0.000000000000000000 ) ) ;
#131500 = MECHANICAL_DESIGN_GEOMETRIC_PRESENTATION_REPRESENTATION (  '', ( #103629 ), #138433 ) ;
#131501 = DIRECTION ( 'NONE',  ( -0.7071067811865486830, -0.7071067811865464625, -0.000000000000000000 ) ) ;
#131502 = VECTOR ( 'NONE', #116877, 1000.000000000000000 ) ;
#131503 = FACE_BOUND ( 'NONE', #68135, .T. ) ;
#131504 = EDGE_CURVE ( 'NONE', #37411, #87872, #84155, .T. ) ;
#131505 = DIRECTION ( 'NONE',  ( -0.3543493200069162685, -0.000000000000000000, -0.9351131265310288487 ) ) ;
#131506 = DIRECTION ( 'NONE',  ( -0.7071067811865487940, 0.7071067811865463515, -0.000000000000000000 ) ) ;
#131507 = CARTESIAN_POINT ( 'NONE',  ( -8.671830600776413434, 11.25929247661560240, 4.000000000000000000 ) ) ;
#131509 = ORIENTED_EDGE ( 'NONE', *, *, #63356, .F. ) ;
#131508 = CARTESIAN_POINT ( 'NONE',  ( 52.14169371712954870, -2.130196079827424871, -7.949999999999998401 ) ) ;
#131510 = AXIS2_PLACEMENT_3D ( 'NONE', #71277, #47422, #16122 ) ;
#131511 = VECTOR ( 'NONE', #91924, 1000.000000000000000 ) ;
#131512 = CARTESIAN_POINT ( 'NONE',  ( 23.78840764549667597, 9.139736423841732040E-16, 0.000000000000000000 ) ) ;
#131513 = VERTEX_POINT ( 'NONE', #40630 ) ;
#131514 = ORIENTED_EDGE ( 'NONE', *, *, #91107, .T. ) ;
#131515 = CARTESIAN_POINT ( 'NONE',  ( 88.28709685856478018, 3.054999999999997495, 5.291415217122919401 ) ) ;
#131516 = EDGE_LOOP ( 'NONE', ( #76413, #76901, #111309, #59436 ) ) ;
#131517 = CARTESIAN_POINT ( 'NONE',  ( -7.499999999999945821, 15.05218569542901896, 5.000000000000000000 ) ) ;
#131518 = VERTEX_POINT ( 'NONE', #17423 ) ;
#131519 = LINE ( 'NONE', #117052, #100289 ) ;
#131520 = CARTESIAN_POINT ( 'NONE',  ( -1.499999999999990896, -2.173586137069142499, -4.605770156576112662 ) ) ;
#131521 = DIRECTION ( 'NONE',  ( 0.7071067811865486830, -0.7071067811865464625, -0.000000000000000000 ) ) ;
#131522 = CARTESIAN_POINT ( 'NONE',  ( -13.49999999999990941, 12.05218569542904561, 5.000000000000000000 ) ) ;
#131523 = CARTESIAN_POINT ( 'NONE',  ( 2.999999999999985345, 8.587461875839158765, 4.000000000000000000 ) ) ;
#131524 = DIRECTION ( 'NONE',  ( -0.7071067811865486830, 0.7071067811865464625, 0.000000000000000000 ) ) ;
#131525 = FACE_OUTER_BOUND ( 'NONE', #97851, .T. ) ;
#131526 = EDGE_LOOP ( 'NONE', ( #109200, #97171, #43263, #40598 ) ) ;
#131527 = FILL_AREA_STYLE_COLOUR ( '', #127902 ) ;
#131528 = ORIENTED_EDGE ( 'NONE', *, *, #66457, .T. ) ;
#131529 = DIRECTION ( 'NONE',  ( 0.7071067811865487940, 0.7071067811865463515, 0.000000000000000000 ) ) ;
#131530 = CARTESIAN_POINT ( 'NONE',  ( 6.989119713460463679, -22.02621442084248216, 4.990779571109220214 ) ) ;
#131531 = MECHANICAL_DESIGN_GEOMETRIC_PRESENTATION_REPRESENTATION (  '', ( #8833 ), #108401 ) ;
#131532 = VERTEX_POINT ( 'NONE', #116743 ) ;
#131533 = ORIENTED_EDGE ( 'NONE', *, *, #38948, .F. ) ;
#131534 = CARTESIAN_POINT ( 'NONE',  ( 38.06293019189810423, 1.637169565754157174, 6.110000000000002984 ) ) ;
#131535 =( GEOMETRIC_REPRESENTATION_CONTEXT ( 3 ) GLOBAL_UNCERTAINTY_ASSIGNED_CONTEXT ( ( #69193 ) ) GLOBAL_UNIT_ASSIGNED_CONTEXT ( ( #102998, #60223, #137051 ) ) REPRESENTATION_CONTEXT ( 'NONE', 'WORKASPACE' ) );
#131536 = EDGE_LOOP ( 'NONE', ( #52738, #60131, #127234, #57230 ) ) ;
#131537 = CARTESIAN_POINT ( 'NONE',  ( 72.48921356237309510, -27.52281430457106026, 5.000000000000000000 ) ) ;
#131538 = LINE ( 'NONE', #88768, #118729 ) ;
#131539 = ADVANCED_FACE ( 'NONE', ( #7960 ), #126200, .T. ) ;
#131540 = CARTESIAN_POINT ( 'NONE',  ( 22.94163961620376568, -6.094999999999989093, 1.633150327867691765 ) ) ;
#131541 = CARTESIAN_POINT ( 'NONE',  ( 7.109511292951834704, 11.08337169632131669, -28.03137008052015133 ) ) ;
#131542 = EDGE_CURVE ( 'NONE', #47759, #130435, #115268, .T. ) ;
#131543 = ORIENTED_EDGE ( 'NONE', *, *, #30395, .T. ) ;
#131544 = CYLINDRICAL_SURFACE ( 'NONE', #34168, 7.950000000000000178 ) ;
#131546 = VERTEX_POINT ( 'NONE', #49388 ) ;
#131545 = EDGE_CURVE ( 'NONE', #137465, #96120, #139954, .T. ) ;
#131547 = CARTESIAN_POINT ( 'NONE',  ( 19.89359858452208130, 4.202752102959690472E-16, 0.000000000000000000 ) ) ;
#131548 = DIRECTION ( 'NONE',  ( -0.7071067811865486830, -0.7071067811865464625, 0.000000000000000000 ) ) ;
#131549 = VECTOR ( 'NONE', #125292, 1000.000000000000114 ) ;
#131551 = VERTEX_POINT ( 'NONE', #96386 ) ;
#131550 = DIRECTION ( 'NONE',  ( 0.6830127018922181881, 0.6830127018922202975, -0.2588190451025214056 ) ) ;
#131552 = ORIENTED_EDGE ( 'NONE', *, *, #81995, .T. ) ;
#131553 = ADVANCED_FACE ( 'NONE', ( #83418 ), #16716, .F. ) ;
#131554 = PLANE ( 'NONE',  #45057 ) ;
#131555 = CARTESIAN_POINT ( 'NONE',  ( 14.81601139373099585, 28.73617430169776910, 5.000000000000000000 ) ) ;
#131556 = VECTOR ( 'NONE', #137305, 1000.000000000000000 ) ;
#131557 = CARTESIAN_POINT ( 'NONE',  ( 33.52400138585425537, 22.03583458319438648, 4.979811245910084949 ) ) ;
#131558 = ORIENTED_EDGE ( 'NONE', *, *, #113604, .F. ) ;
#131559 = VERTEX_POINT ( 'NONE', #127634 ) ;
#131560 = VERTEX_POINT ( 'NONE', #105153 ) ;
#131561 = VERTEX_POINT ( 'NONE', #71845 ) ;
#131562 = EDGE_CURVE ( 'NONE', #36893, #4917, #29713, .T. ) ;
#131563 = DIRECTION ( 'NONE',  ( -0.7071067811865486830, -0.7071067811865464625, 0.000000000000000000 ) ) ;
#131564 = LINE ( 'NONE', #132306, #125059 ) ;
#131565 = CARTESIAN_POINT ( 'NONE',  ( 9.748407645496676821, 3.061616997868380183E-16, -2.500000000000001332 ) ) ;
#131566 = DIRECTION ( 'NONE',  ( -0.6830127018922180770, -0.6830127018922204085, -0.2588190451025213501 ) ) ;
#131567 = DIRECTION ( 'NONE',  ( 0.7071067811865487940, -0.7071067811865463515, 0.000000000000000000 ) ) ;
#131568 = EDGE_CURVE ( 'NONE', #62743, #6620, #126883, .T. ) ;
#131569 = DIRECTION ( 'NONE',  ( -0.6830127018922180770, -0.6830127018922204085, -0.2588190451025213501 ) ) ;
#131570 = CARTESIAN_POINT ( 'NONE',  ( -24.29974487139158867, -27.71228299555223273, 4.000000000000000000 ) ) ;
#131571 = EDGE_CURVE ( 'NONE', #116882, #77069, #16577, .T. ) ;
#131572 = VERTEX_POINT ( 'NONE', #27578 ) ;
#131573 = LINE ( 'NONE', #85916, #81397 ) ;
#131574 = ORIENTED_EDGE ( 'NONE', *, *, #30389, .T. ) ;
#131575 = CARTESIAN_POINT ( 'NONE',  ( 27.48921356237309155, -27.52281430457074762, 5.000000000000000000 ) ) ;
#131576 = EDGE_CURVE ( 'NONE', #106729, #131264, #71125, .T. ) ;
#131577 = CARTESIAN_POINT ( 'NONE',  ( 24.48921356237309510, -27.52281430457072631, 5.000000000000000000 ) ) ;
#131578 = SPHERICAL_SURFACE ( 'NONE', #129455, 0.5000000000000000000 ) ;
#131579 = ORIENTED_EDGE ( 'NONE', *, *, #118122, .T. ) ;
#131580 = PLANE ( 'NONE',  #113147 ) ;
#131581 = VECTOR ( 'NONE', #255, 1000.000000000000227 ) ;
#131582 = LINE ( 'NONE', #7069, #48814 ) ;
#131583 = DIRECTION ( 'NONE',  ( -0.000000000000000000, 0.000000000000000000, 1.000000000000000000 ) ) ;
#131584 = ORIENTED_EDGE ( 'NONE', *, *, #48950, .F. ) ;
#131585 = ORIENTED_EDGE ( 'NONE', *, *, #90309, .F. ) ;
#131586 = CARTESIAN_POINT ( 'NONE',  ( 52.40027281129884784, -49.14999999999999147, 40.57187971031920171 ) ) ;
#131587 = DIRECTION ( 'NONE',  ( -0.3543493200069162685, -0.000000000000000000, -0.9351131265310288487 ) ) ;
#131588 = DIRECTION ( 'NONE',  ( -0.7071067811865486830, -0.7071067811865464625, 0.000000000000000000 ) ) ;
#131589 = CARTESIAN_POINT ( 'NONE',  ( 10.17183060077640455, 9.759292476615618384, 4.000000000000000000 ) ) ;
#131590 = DIRECTION ( 'NONE',  ( -0.7071067811865487940, 0.7071067811865463515, 0.000000000000000000 ) ) ;
#131591 = CARTESIAN_POINT ( 'NONE',  ( 63.93293019189812298, 1.637169565754156730, 6.110000000000001208 ) ) ;
#131592 = DIRECTION ( 'NONE',  ( -0.7071067811865486830, -0.7071067811865464625, 0.000000000000000000 ) ) ;
#131593 = LINE ( 'NONE', #65670, #120199 ) ;
#131594 = PLANE ( 'NONE',  #113620 ) ;
#131595 = CARTESIAN_POINT ( 'NONE',  ( 23.29289321881329045, 20.25929247661551358, 5.000000000000000000 ) ) ;
#131596 = ORIENTED_EDGE ( 'NONE', *, *, #26008, .T. ) ;
#131597 = LINE ( 'NONE', #142483, #30288 ) ;
#131598 = EDGE_CURVE ( 'NONE', #127400, #116795, #60252, .T. ) ;
#131599 = VERTEX_POINT ( 'NONE', #73264 ) ;
#131600 = CARTESIAN_POINT ( 'NONE',  ( -22.26506670282036993, 12.75929247661558286, 18.34774599283961294 ) ) ;
#131601 =( NAMED_UNIT ( * ) PLANE_ANGLE_UNIT ( ) SI_UNIT ( $, .RADIAN. ) );
#131602 = VERTEX_POINT ( 'NONE', #117427 ) ;
#131603 = VECTOR ( 'NONE', #42732, 1000.000000000000000 ) ;
#131604 = COLOUR_RGB ( '', 0.08235294, 0.09019608, 0.10196078) ;
#131605 = CARTESIAN_POINT ( 'NONE',  ( 0.000000000000000000, 0.000000000000000000, 5.000000000000000000 ) ) ;
#131606 = LINE ( 'NONE', #10509, #37318 ) ;
#131607 = AXIS2_PLACEMENT_3D ( 'NONE', #88176, #143256, #54841 ) ;
#131608 = DIRECTION ( 'NONE',  ( 0.000000000000000000, 0.000000000000000000, 1.000000000000000000 ) ) ;
#131609 = DIRECTION ( 'NONE',  ( 0.7071067811865487940, 0.7071067811865463515, -0.000000000000000000 ) ) ;
#131610 = AXIS2_PLACEMENT_3D ( 'NONE', #63666, #40482, #18676 ) ;
#131611 = DIRECTION ( 'NONE',  ( -0.6830127018922181881, 0.6830127018922202975, -0.2588190451025214056 ) ) ;
#131612 = VERTEX_POINT ( 'NONE', #5805 ) ;
#131613 = ORIENTED_EDGE ( 'NONE', *, *, #32136, .F. ) ;
#131614 = LINE ( 'NONE', #130917, #141226 ) ;
#131615 = DIRECTION ( 'NONE',  ( -0.7071067811865486830, -0.7071067811865464625, 0.000000000000000000 ) ) ;
#131616 = UNCERTAINTY_MEASURE_WITH_UNIT (LENGTH_MEASURE( 1.000000000000000082E-05 ), #85109, 'distance_accuracy_value', 'NONE');
#131617 = CONICAL_SURFACE ( 'NONE', #108379, 2.500000000000000888, 0.9599310885968822538 ) ;
#131618 = VECTOR ( 'NONE', #26839, 1000.000000000000000 ) ;
#131619 = CARTESIAN_POINT ( 'NONE',  ( -28.17183060077627488, -20.24070752338407431, 4.000000000000000000 ) ) ;
#131620 = EDGE_CURVE ( 'NONE', #39821, #141489, #18104, .T. ) ;
#131621 = LINE ( 'NONE', #112014, #27388 ) ;
#131622 = CARTESIAN_POINT ( 'NONE',  ( 88.89169371712954160, 2.130196079827421762, 7.950000000000001066 ) ) ;
#131623 = DIRECTION ( 'NONE',  ( 0.000000000000000000, -1.000000000000000000, 0.000000000000000000 ) ) ;
#131624 = DIRECTION ( 'NONE',  ( 0.000000000000000000, -1.137193330093851115E-16, 1.000000000000000000 ) ) ;
#131625 = ORIENTED_EDGE ( 'NONE', *, *, #58049, .T. ) ;
#131626 = CARTESIAN_POINT ( 'NONE',  ( 85.43750000000001421, 5.819803920172573974, -5.819803920172572198 ) ) ;
#131627 = CARTESIAN_POINT ( 'NONE',  ( 30.18398860626900060, 28.73617430169808173, 5.000000000000000000 ) ) ;
#131628 = EDGE_CURVE ( 'NONE', #103228, #67897, #50081, .T. ) ;
#131629 = FACE_OUTER_BOUND ( 'NONE', #133175, .T. ) ;
#131630 = DIRECTION ( 'NONE',  ( -0.7071067811865486830, -0.7071067811865464625, -0.000000000000000000 ) ) ;
#131631 =( GEOMETRIC_REPRESENTATION_CONTEXT ( 3 ) GLOBAL_UNCERTAINTY_ASSIGNED_CONTEXT ( ( #26044 ) ) GLOBAL_UNIT_ASSIGNED_CONTEXT ( ( #139461, #60466, #127853 ) ) REPRESENTATION_CONTEXT ( 'NONE', 'WORKASPACE' ) );
#131632 = VERTEX_POINT ( 'NONE', #51508 ) ;
#131633 = FACE_OUTER_BOUND ( 'NONE', #82974, .T. ) ;
#131634 = ORIENTED_EDGE ( 'NONE', *, *, #22351, .T. ) ;
#131635 = VECTOR ( 'NONE', #61560, 1000.000000000000227 ) ;
#131636 = EDGE_CURVE ( 'NONE', #57761, #73971, #7235, .T. ) ;
#131637 = CARTESIAN_POINT ( 'NONE',  ( 79.33376352523144703, 6.110000000000001208, 1.122388791418549305E-15 ) ) ;
#131639 = VERTEX_POINT ( 'NONE', #119570 ) ;
#131638 = AXIS2_PLACEMENT_3D ( 'NONE', #90603, #55846, #47154 ) ;
#131640 = LINE ( 'NONE', #76560, #2565 ) ;
#131641 = VECTOR ( 'NONE', #88992, 1000.000000000000000 ) ;
#131642 = CARTESIAN_POINT ( 'NONE',  ( -34.92500000000001137, -0.2815095627957688307, 4.759050581649336920 ) ) ;
#131643 = CARTESIAN_POINT ( 'NONE',  ( -57.48921356237308800, -27.52281430457095368, 5.000000000000000000 ) ) ;
#131644 = VECTOR ( 'NONE', #25988, 1000.000000000000000 ) ;
#131645 = CARTESIAN_POINT ( 'NONE',  ( 0.1161069444170877152, -0.3999999999999998002, -2.220360628129161906 ) ) ;
#131646 = EDGE_CURVE ( 'NONE', #107864, #112008, #77553, .T. ) ;
#131647 = CARTESIAN_POINT ( 'NONE',  ( -0.4892135623730947680, -27.52281430457055578, 5.000000000000000000 ) ) ;
#131649 = ORIENTED_EDGE ( 'NONE', *, *, #82503, .T. ) ;
#131648 = CARTESIAN_POINT ( 'NONE',  ( 29.20710678118634718, -20.24070752338407075, 5.000000000000000000 ) ) ;
#131650 = FACE_OUTER_BOUND ( 'NONE', #126841, .T. ) ;
#131651 = DIRECTION ( 'NONE',  ( 0.000000000000000000, -1.000000000000000000, 0.000000000000000000 ) ) ;
#131652 = CARTESIAN_POINT ( 'NONE',  ( 0.000000000000000000, 0.000000000000000000, 5.000000000000000000 ) ) ;
#131653 = VECTOR ( 'NONE', #83285, 1000.000000000000000 ) ;
#131654 = LINE ( 'NONE', #133788, #101677 ) ;
#131655 = ORIENTED_EDGE ( 'NONE', *, *, #126955, .T. ) ;
#131656 = ORIENTED_EDGE ( 'NONE', *, *, #6913, .F. ) ;
#131657 = CARTESIAN_POINT ( 'NONE',  ( 62.41709685856476852, 3.054999999999998828, 5.291415217122922066 ) ) ;
#131658 = EDGE_LOOP ( 'NONE', ( #17371, #112044, #41399, #85277 ) ) ;
#131659 = DIRECTION ( 'NONE',  ( 0.6830127018922181881, 0.6830127018922202975, -0.2588190451025214056 ) ) ;
#131660 = DIRECTION ( 'NONE',  ( 1.000000000000000000, 0.000000000000000000, 0.000000000000000000 ) ) ;
#131661 = LINE ( 'NONE', #96836, #75854 ) ;
#131662 = SURFACE_STYLE_USAGE ( .BOTH. , #109179 ) ;
#131663 = ORIENTED_EDGE ( 'NONE', *, *, #138401, .F. ) ;
#131664 = VERTEX_POINT ( 'NONE', #88423 ) ;
#131665 = VECTOR ( 'NONE', #51881, 999.9999999999998863 ) ;
#131666 = CARTESIAN_POINT ( 'NONE',  ( 9.005480084712511157, 28.92564299267931816, 4.000000000000000000 ) ) ;
#131667 = LINE ( 'NONE', #107740, #4974 ) ;
#131668 = VECTOR ( 'NONE', #56754, 1000.000000000000000 ) ;
#131669 = ORIENTED_EDGE ( 'NONE', *, *, #6168, .F. ) ;
#131670 = EDGE_CURVE ( 'NONE', #28630, #46262, #20266, .T. ) ;
#131671 = LINE ( 'NONE', #11269, #2644 ) ;
#131672 = CARTESIAN_POINT ( 'NONE',  ( -3.299744871391591339, -27.71228299555208352, 4.000000000000000000 ) ) ;
#131673 = DIRECTION ( 'NONE',  ( -0.3543493200069163240, -0.000000000000000000, 0.9351131265310288487 ) ) ;
#131674 = ORIENTED_EDGE ( 'NONE', *, *, #44004, .F. ) ;
#131675 = ADVANCED_FACE ( 'NONE', ( #8646 ), #42065, .F. ) ;
#131676 = FACE_BOUND ( 'NONE', #48763, .T. ) ;
#131677 = EDGE_CURVE ( 'NONE', #135110, #35704, #5182, .T. ) ;
#131678 = CARTESIAN_POINT ( 'NONE',  ( 181.1391930515558215, -48.09618305010690875, 37.50858089739960377 ) ) ;
#131679 = CARTESIAN_POINT ( 'NONE',  ( 20.67183060077633883, 20.25929247661551713, 4.000000000000000000 ) ) ;
#131680 = CARTESIAN_POINT ( 'NONE',  ( 0.000000000000000000, 0.000000000000000000, 5.000000000000000000 ) ) ;
#131681 = CARTESIAN_POINT ( 'NONE',  ( 184.1500000000000057, -57.15000000000003411, -15.92500000000064730 ) ) ;
#131682 = PLANE ( 'NONE',  #23378 ) ;
#131683 = VERTEX_POINT ( 'NONE', #66663 ) ;
#131684 = ORIENTED_EDGE ( 'NONE', *, *, #128938, .F. ) ;
#131685 = CARTESIAN_POINT ( 'NONE',  ( 109.8704301918981230, -3.055000000000001492, 5.291415217122917625 ) ) ;
#131686 = ORIENTED_EDGE ( 'NONE', *, *, #142147, .T. ) ;
#131687 = ORIENTED_EDGE ( 'NONE', *, *, #36918, .F. ) ;
#131688 = CARTESIAN_POINT ( 'NONE',  ( -16.00193056682086379, -22.22500000000000142, 4.500000000000000888 ) ) ;
#131689 = ADVANCED_FACE ( 'NONE', ( #110131 ), #53644, .T. ) ;
#131690 = CARTESIAN_POINT ( 'NONE',  ( 21.00548008471250938, 28.92564299267923644, 4.000000000000000000 ) ) ;
#131691 = CARTESIAN_POINT ( 'NONE',  ( -51.18398860626899705, 28.73617430169823095, 5.000000000000000000 ) ) ;
#131692 = ORIENTED_EDGE ( 'NONE', *, *, #9062, .F. ) ;
#131693 = DIRECTION ( 'NONE',  ( 0.3543493200069162685, -0.000000000000000000, -0.9351131265310288487 ) ) ;
#131694 = CARTESIAN_POINT ( 'NONE',  ( 7.720000000000001528, -2.055000000000000160, 0.000000000000000000 ) ) ;
#131696 = LINE ( 'NONE', #86772, #126786 ) ;
#131695 = DIRECTION ( 'NONE',  ( 1.000000000000000000, 0.000000000000000000, 0.000000000000000000 ) ) ;
#131697 = LINE ( 'NONE', #108461, #50772 ) ;
#131698 = VECTOR ( 'NONE', #79503, 1000.000000000000000 ) ;
#131699 = AXIS2_PLACEMENT_3D ( 'NONE', #64906, #40997, #118542 ) ;
#131700 = CARTESIAN_POINT ( 'NONE',  ( 31.49999999999977263, 19.08746187583906462, 4.000000000000000000 ) ) ;
#131701 = VECTOR ( 'NONE', #125444, 1000.000000000000227 ) ;
#131702 = ORIENTED_EDGE ( 'NONE', *, *, #28622, .F. ) ;
#131703 = CARTESIAN_POINT ( 'NONE',  ( -8.994519915287490619, 28.92564299267944250, 4.000000000000000000 ) ) ;
#131704 = FACE_OUTER_BOUND ( 'NONE', #108034, .T. ) ;
#131705 = ORIENTED_EDGE ( 'NONE', *, *, #75562, .T. ) ;
#131706 = ORIENTED_EDGE ( 'NONE', *, *, #131542, .T. ) ;
#131707 = VERTEX_POINT ( 'NONE', #86972 ) ;
#131708 = CARTESIAN_POINT ( 'NONE',  ( 64.89626352523143282, 4.472830434245840259, -4.472830434245838482 ) ) ;
#131709 = CONICAL_SURFACE ( 'NONE', #43428, 2.055000000000000604, 0.9599310885968764806 ) ;
#131710 = ORIENTED_EDGE ( 'NONE', *, *, #51179, .T. ) ;
#131711 = VECTOR ( 'NONE', #136554, 1000.000000000000000 ) ;
#131712 = CARTESIAN_POINT ( 'NONE',  ( -23.99999999999983302, 13.55218569542903317, 5.000000000000000000 ) ) ;
#131713 = ADVANCED_FACE ( 'NONE', ( #86277 ), #131192, .F. ) ;
#131714 = CARTESIAN_POINT ( 'NONE',  ( 17.53719725875415847, 4.202752102959690472E-16, 0.000000000000000000 ) ) ;
#131715 = CARTESIAN_POINT ( 'NONE',  ( 95.52126352523141861, -4.472830434245838482, -4.472830434245840259 ) ) ;
#131716 = DIRECTION ( 'NONE',  ( -0.3543493200069162685, -0.000000000000000000, -0.9351131265310288487 ) ) ;
#131717 = ADVANCED_FACE ( 'NONE', ( #85519, #110828 ), #129758, .F. ) ;
#131718 = DIRECTION ( 'NONE',  ( -0.7071067811865487940, 0.7071067811865463515, -0.000000000000000000 ) ) ;
#131719 = ORIENTED_EDGE ( 'NONE', *, *, #81179, .F. ) ;
#131720 = FACE_OUTER_BOUND ( 'NONE', #76522, .T. ) ;
#131721 = AXIS2_PLACEMENT_3D ( 'NONE', #113924, #125532, #126235 ) ;
#131722 = FACE_OUTER_BOUND ( 'NONE', #61290, .T. ) ;
#131723 = EDGE_CURVE ( 'NONE', #46898, #67112, #130499, .T. ) ;
#131724 = EDGE_CURVE ( 'NONE', #91593, #143231, #76102, .T. ) ;
#131725 =( BOUNDED_CURVE ( )  B_SPLINE_CURVE ( 2, ( #21624, #120924, #54980, #52791, #87591, #120174, #76001, #65880, #75305, #63718, #20886, #131099, #64406 ),
 .UNSPECIFIED., .F., .F. ) 
 B_SPLINE_CURVE_WITH_KNOTS ( ( 3, 2, 2, 2, 2, 2, 3 ),
 ( 0.5333333333333334370, 0.5361111111111112049, 0.5388888888888889728, 0.5416666666666667407, 0.5444444444444443976, 0.5472222222222222765, 0.5500000000000000444 ),
 .UNSPECIFIED. ) 
 CURVE ( )  GEOMETRIC_REPRESENTATION_ITEM ( )  RATIONAL_B_SPLINE_CURVE ( ( 0.9999999999999986677, 0.9659258262890696445, 1.000000000000000000, 0.9659258262890683122, 1.000000000000000000, 0.9659258262890683122, 1.000000000000000000, 0.9659258262890683122, 1.000000000000000000, 0.9659258262890683122, 1.000000000000000000, 0.9659258262890683122, 1.000000000000000000 ) ) 
 REPRESENTATION_ITEM ( '' )  );
#131726 = DIRECTION ( 'NONE',  ( -0.3543493200069162685, -0.000000000000000000, -0.9351131265310288487 ) ) ;
#131727 = CARTESIAN_POINT ( 'NONE',  ( 14.20710678118644132, -11.24070752338417023, 5.000000000000000000 ) ) ;
#131728 = ORIENTED_EDGE ( 'NONE', *, *, #100503, .F. ) ;
#131729 = AXIS2_PLACEMENT_3D ( 'NONE', #1070, #122874, #14094 ) ;
#131730 = LINE ( 'NONE', #140446, #106210 ) ;
#131731 = ORIENTED_EDGE ( 'NONE', *, *, #24083, .F. ) ;
#131732 = ORIENTED_EDGE ( 'NONE', *, *, #135573, .T. ) ;
#131733 = ORIENTED_EDGE ( 'NONE', *, *, #882, .T. ) ;
#131734 = CARTESIAN_POINT ( 'NONE',  ( 126.6412635252314516, 4.472830434245835818, 4.472830434245840259 ) ) ;
#131735 = ORIENTED_EDGE ( 'NONE', *, *, #112036, .T. ) ;
#131736 = VECTOR ( 'NONE', #26448, 1000.000000000000000 ) ;
#131737 =( BOUNDED_CURVE ( )  B_SPLINE_CURVE ( 2, ( #121796, #1437, #66735, #78328, #47180, #91362, #110911, #11594, #56620, #55878, #100079, #89203, #122519 ),
 .UNSPECIFIED., .F., .T. ) 
 B_SPLINE_CURVE_WITH_KNOTS ( ( 3, 2, 2, 2, 2, 2, 3 ),
 ( 0.4000000000000000222, 0.4027777777777777901, 0.4055555555555555580, 0.4083333333333333259, 0.4111111111111110938, 0.4138888888888888618, 0.4166666666666666852 ),
 .UNSPECIFIED. ) 
 CURVE ( )  GEOMETRIC_REPRESENTATION_ITEM ( )  RATIONAL_B_SPLINE_CURVE ( ( 1.000000000000000000, 0.9659258262890683122, 1.000000000000000000, 0.9659258262890683122, 1.000000000000000000, 0.9659258262890683122, 1.000000000000000000, 0.9659258262890683122, 1.000000000000000000, 0.9659258262890683122, 1.000000000000000000, 0.9659258262890683122, 1.000000000000000000 ) ) 
 REPRESENTATION_ITEM ( '' )  );
#131738 = MECHANICAL_DESIGN_GEOMETRIC_PRESENTATION_REPRESENTATION (  '', ( #97015 ), #6669 ) ;
#131739 = DIRECTION ( 'NONE',  ( -0.7071067811865486830, 0.7071067811865464625, 0.000000000000000000 ) ) ;
#131740 = AXIS2_PLACEMENT_3D ( 'NONE', #105530, #114281, #70807 ) ;
#131741 = ADVANCED_FACE ( 'NONE', ( #109434 ), #43471, .F. ) ;
#131742 = DIRECTION ( 'NONE',  ( -0.5735764363510503783, -0.8191520442889886899, 0.000000000000000000 ) ) ;
#131743 = ADVANCED_FACE ( 'NONE', ( #26009 ), #57236, .F. ) ;
#131744 = ORIENTED_EDGE ( 'NONE', *, *, #8875, .F. ) ;
#131745 = LINE ( 'NONE', #9188, #39575 ) ;
#131746 = ORIENTED_EDGE ( 'NONE', *, *, #31755, .T. ) ;
#131747 = VECTOR ( 'NONE', #45691, 1000.000000000000000 ) ;
#131748 = ADVANCED_FACE ( 'NONE', ( #663 ), #36863, .T. ) ;
#131749 = CARTESIAN_POINT ( 'NONE',  ( 16.45790314143522082, 6.871911579029515771, 3.967499999999989146 ) ) ;
#131750 = FACE_OUTER_BOUND ( 'NONE', #82046, .T. ) ;
#131751 = B_SPLINE_CURVE_WITH_KNOTS ( 'NONE', 1,
 ( #68922, #123302 ),
 .UNSPECIFIED., .F., .F.,
 ( 2, 2 ),
 ( 0.000000000000000000, 0.1304347826086980078 ),
 .UNSPECIFIED. ) ;
#131752 = PLANE ( 'NONE',  #138641 ) ;
#131753 = CARTESIAN_POINT ( 'NONE',  ( 37.74999999999999289, -9.735942053221458872E-16, 7.950000000000000178 ) ) ;
#131754 = ORIENTED_EDGE ( 'NONE', *, *, #96192, .F. ) ;
#131755 = VERTEX_POINT ( 'NONE', #111580 ) ;
#131756 = VERTEX_POINT ( 'NONE', #47791 ) ;
#131757 = CARTESIAN_POINT ( 'NONE',  ( 58.02083333333332149, 7.949999999999998401, 2.130196079827431532 ) ) ;
#131758 = UNCERTAINTY_MEASURE_WITH_UNIT (LENGTH_MEASURE( 1.000000000000000082E-05 ), #50087, 'distance_accuracy_value', 'NONE');
#131759 = EDGE_CURVE ( 'NONE', #56470, #26097, #78986, .T. ) ;
#131760 = VECTOR ( 'NONE', #70635, 1000.000000000000000 ) ;
#131761 = DIRECTION ( 'NONE',  ( -0.000000000000000000, -0.3543493200069152693, 0.9351131265310292928 ) ) ;
#131762 = PLANE ( 'NONE',  #140892 ) ;
#131763 = CARTESIAN_POINT ( 'NONE',  ( -48.29974487139158867, -27.71228299555239971, 4.000000000000000000 ) ) ;
#131764 = CARTESIAN_POINT ( 'NONE',  ( 32.22959685856477563, -6.110000000000000320, -1.637169565754161393 ) ) ;
#131765 = DIRECTION ( 'NONE',  ( 0.3543493200069162685, -0.000000000000000000, -0.9351131265310288487 ) ) ;
#131766 = CARTESIAN_POINT ( 'NONE',  ( 19.05000000000000071, 3.174999999999997158, 4.000000000000000000 ) ) ;
#131767 = ORIENTED_EDGE ( 'NONE', *, *, #95558, .F. ) ;
#131768 = PLANE ( 'NONE',  #90533 ) ;
#131769 = EDGE_CURVE ( 'NONE', #42960, #116177, #23867, .T. ) ;
#131770 = ORIENTED_EDGE ( 'NONE', *, *, #26089, .F. ) ;
#131771 = CARTESIAN_POINT ( 'NONE',  ( -1.179999999999999938, 6.391994993740214959, 10.00000000000000000 ) ) ;
#131772 = EDGE_LOOP ( 'NONE', ( #51539, #87295, #67522, #3260 ) ) ;
#131773 = CARTESIAN_POINT ( 'NONE',  ( 18.71247294953710494, 0.000000000000000000, 6.094999999999989981 ) ) ;
#131775 = VERTEX_POINT ( 'NONE', #114429 ) ;
#131774 = DIRECTION ( 'NONE',  ( -0.6830127018922181881, 0.6830127018922202975, -0.2588190451025214056 ) ) ;
#131776 = CARTESIAN_POINT ( 'NONE',  ( -9.792893218813391698, -20.24070752338407431, 5.000000000000000000 ) ) ;
#131777 = EDGE_CURVE ( 'NONE', #113899, #76633, #34042, .T. ) ;
#131778 = ORIENTED_EDGE ( 'NONE', *, *, #38243, .T. ) ;
#131779 = DIRECTION ( 'NONE',  ( -0.6830127018922180770, 0.6830127018922202975, -0.2588190451025213501 ) ) ;
#131780 = ORIENTED_EDGE ( 'NONE', *, *, #73052, .T. ) ;
#131781 = DIRECTION ( 'NONE',  ( -0.6830127018922180770, -0.6830127018922204085, -0.2588190451025213501 ) ) ;
#131782 = EDGE_LOOP ( 'NONE', ( #106696, #40294, #103207, #37088 ) ) ;
#131783 = CARTESIAN_POINT ( 'NONE',  ( 59.99451991528749772, 28.92564299267980132, 4.000000000000000000 ) ) ;
#131784 = ADVANCED_FACE ( 'NONE', ( #36178 ), #125318, .F. ) ;
#131785 = CARTESIAN_POINT ( 'NONE',  ( 110.1833603837962130, -2.130196079827426203, 7.949999999999997513 ) ) ;
#131786 = CARTESIAN_POINT ( 'NONE',  ( 2.613322195557305605, 4.202752102959690472E-16, 0.000000000000000000 ) ) ;
#131787 = CYLINDRICAL_SURFACE ( 'NONE', #27384, 3.000000000000002665 ) ;
#131788 = CARTESIAN_POINT ( 'NONE',  ( 71.99451991528749772, 28.92564299267988304, 4.000000000000000000 ) ) ;
#131789 = DIRECTION ( 'NONE',  ( 0.000000000000000000, -1.000000000000000000, 0.000000000000000000 ) ) ;
#131790 = LINE ( 'NONE', #32479, #83209 ) ;
#131791 = CARTESIAN_POINT ( 'NONE',  ( 5.250000000000000000, -7.464222240803106570E-16, -6.094999999999989981 ) ) ;
#131792 = CARTESIAN_POINT ( 'NONE',  ( 16.60373647476855297, 5.808823158059035485, 5.808823158059032821 ) ) ;
#131793 = CARTESIAN_POINT ( 'NONE',  ( 7.637717201596474048, 4.584330080086930965E-16, 0.000000000000000000 ) ) ;
#131794 = FACE_OUTER_BOUND ( 'NONE', #86221, .T. ) ;
#131795 = VERTEX_POINT ( 'NONE', #59375 ) ;
#131796 = VERTEX_POINT ( 'NONE', #113722 ) ;
#131797 = DIRECTION ( 'NONE',  ( 1.000000000000000000, 0.000000000000000000, 0.000000000000000000 ) ) ;
#131798 = ORIENTED_EDGE ( 'NONE', *, *, #5153, .T. ) ;
#131799 = EDGE_CURVE ( 'NONE', #70593, #20021, #44954, .T. ) ;
#131800 = CARTESIAN_POINT ( 'NONE',  ( 5.443598275411213550, 2.500000000000000444, 3.061616997868383634E-16 ) ) ;
#131801 = CARTESIAN_POINT ( 'NONE',  ( 0.000000000000000000, -22.26999999999999247, -0.5000000000000004441 ) ) ;
#131802 = CARTESIAN_POINT ( 'NONE',  ( 131.5423521607622774, -49.05583548141699168, -39.86617647058817226 ) ) ;
#131803 = ORIENTED_EDGE ( 'NONE', *, *, #1762, .F. ) ;
#131804 = VECTOR ( 'NONE', #74873, 1000.000000000000000 ) ;
#131805 = VECTOR ( 'NONE', #125453, 1000.000000000000227 ) ;
#131806 = AXIS2_PLACEMENT_3D ( 'NONE', #56968, #134512, #102600 ) ;
#131807 = PRESENTATION_STYLE_ASSIGNMENT (( #28397 ) ) ;
#131808 = CARTESIAN_POINT ( 'NONE',  ( 8.510786437626906675, -27.52281430457049183, 5.000000000000000000 ) ) ;
#131809 = VECTOR ( 'NONE', #128139, 999.9999999999998863 ) ;
#131810 = DIRECTION ( 'NONE',  ( -0.000000000000000000, 0.3543493200069153248, 0.9351131265310292928 ) ) ;
#131811 = CARTESIAN_POINT ( 'NONE',  ( 0.1839886062690032631, 28.73617430169787568, 5.000000000000000000 ) ) ;
#131812 = EDGE_CURVE ( 'NONE', #137018, #100179, #102151, .T. ) ;
#131813 = SURFACE_STYLE_FILL_AREA ( #107184 ) ;
#131815 = ORIENTED_EDGE ( 'NONE', *, *, #140213, .F. ) ;
#131814 = DIRECTION ( 'NONE',  ( 0.7071067811865487940, -0.7071067811865463515, 0.000000000000000000 ) ) ;
#131816 = DIRECTION ( 'NONE',  ( -0.000000000000000000, -0.3543493200069152693, 0.9351131265310292928 ) ) ;
#131817 = FACE_OUTER_BOUND ( 'NONE', #128533, .T. ) ;
#131818 = PLANE ( 'NONE',  #71101 ) ;
#131819 = VECTOR ( 'NONE', #41352, 1000.000000000000000 ) ;
#131820 = CARTESIAN_POINT ( 'NONE',  ( 34.42499999999998295, -4.458600742197917910, 5.000000000000000000 ) ) ;
#131821 = EDGE_LOOP ( 'NONE', ( #137537, #37835, #87645, #128840 ) ) ;
#131822 = ORIENTED_EDGE ( 'NONE', *, *, #6039, .T. ) ;
#131823 = ORIENTED_EDGE ( 'NONE', *, *, #96957, .F. ) ;
#131824 = CARTESIAN_POINT ( 'NONE',  ( 95.52126352523141861, -4.472830434245839371, -4.472830434245840259 ) ) ;
#131825 = ORIENTED_EDGE ( 'NONE', *, *, #27747, .F. ) ;
#131826 = EDGE_CURVE ( 'NONE', #23670, #489, #112310, .T. ) ;
#131827 = CARTESIAN_POINT ( 'NONE',  ( 128.6786164994711044, -49.14501756083436845, 40.36361034346624876 ) ) ;
#131828 = VECTOR ( 'NONE', #117293, 1000.000000000000227 ) ;
#131829 = VECTOR ( 'NONE', #108951, 999.9999999999998863 ) ;
#131830 = CARTESIAN_POINT ( 'NONE',  ( -7.499999999999944045, 3.052185695429140200, 5.000000000000000000 ) ) ;
#131831 = ORIENTED_EDGE ( 'NONE', *, *, #100741, .T. ) ;
#131832 = CARTESIAN_POINT ( 'NONE',  ( 183.3316408629058287, -52.14999999999999147, 41.64499999999997470 ) ) ;
#131833 = DIRECTION ( 'NONE',  ( -1.000000000000000000, -0.000000000000000000, -0.000000000000000000 ) ) ;
#131834 = STYLED_ITEM ( 'NONE', ( #14662 ), #96714 ) ;
#131835 = CARTESIAN_POINT ( 'NONE',  ( 83.03709685856478018, -3.054999999999998828, -5.291415217122919401 ) ) ;
#131836 = VERTEX_POINT ( 'NONE', #12258 ) ;
#131837 = EDGE_CURVE ( 'NONE', #66659, #130638, #124599, .T. ) ;
#131838 = CARTESIAN_POINT ( 'NONE',  ( 54.18398860626899705, 28.73617430169825226, 5.000000000000000000 ) ) ;
#131839 = LINE ( 'NONE', #20184, #130218 ) ;
#131840 = CONICAL_SURFACE ( 'NONE', #87849, 2.500000000000000888, 0.9599310885968822538 ) ;
#131841 = VECTOR ( 'NONE', #37825, 1000.000000000000227 ) ;
#131842 = ORIENTED_EDGE ( 'NONE', *, *, #132137, .F. ) ;
#131843 = EDGE_LOOP ( 'NONE', ( #131754, #8915, #61929, #60204 ) ) ;
#131844 = EDGE_CURVE ( 'NONE', #73748, #36255, #23106, .T. ) ;
#131845 = ORIENTED_EDGE ( 'NONE', *, *, #29236, .F. ) ;
#131846 = CARTESIAN_POINT ( 'NONE',  ( 28.49999999999980105, 18.43112307739199451, 4.000000000000000000 ) ) ;
#131848 = EDGE_CURVE ( 'NONE', #131518, #50635, #89133, .T. ) ;
#131847 = VECTOR ( 'NONE', #78342, 1000.000000000000227 ) ;
#131849 = CARTESIAN_POINT ( 'NONE',  ( -26.99999999999980815, -21.41253812416053748, 4.000000000000000000 ) ) ;
#131850 = CARTESIAN_POINT ( 'NONE',  ( 0.4892135623730947680, -27.52281430457055578, 5.000000000000000000 ) ) ;
#131851 = AXIS2_PLACEMENT_3D ( 'NONE', #58566, #135382, #111446 ) ;
#131852 = AXIS2_PLACEMENT_3D ( 'NONE', #111762, #79890, #54544 ) ;
#131853 = CARTESIAN_POINT ( 'NONE',  ( 166.8257598198775895, 26.96999999999993847, 32.27759070793130292 ) ) ;
#131854 = PLANE ( 'NONE',  #25633 ) ;
#131855 =( LENGTH_UNIT ( ) NAMED_UNIT ( * ) SI_UNIT ( .MILLI., .METRE. ) );
#131856 = ORIENTED_EDGE ( 'NONE', *, *, #102114, .F. ) ;
#131858 = VERTEX_POINT ( 'NONE', #135495 ) ;
#131857 = EDGE_CURVE ( 'NONE', #69033, #96928, #79724, .T. ) ;
#131859 = DIRECTION ( 'NONE',  ( -0.7071067811865486830, -0.7071067811865464625, 0.000000000000000000 ) ) ;
#131860 = ORIENTED_EDGE ( 'NONE', *, *, #138090, .F. ) ;
#131861 = VERTEX_POINT ( 'NONE', #25274 ) ;
#131862 = VECTOR ( 'NONE', #123942, 1000.000000000000000 ) ;
#131863 = EDGE_CURVE ( 'NONE', #49923, #134381, #78258, .T. ) ;
#131864 = DIRECTION ( 'NONE',  ( -0.7071067811865487940, 0.7071067811865463515, -0.000000000000000000 ) ) ;
#131865 = EDGE_LOOP ( 'NONE', ( #112648, #60378, #73721, #3792 ) ) ;
#131866 = LINE ( 'NONE', #8592, #25084 ) ;
#131867 = CARTESIAN_POINT ( 'NONE',  ( 14.42840764549667476, 9.139736423841732040E-16, 0.000000000000000000 ) ) ;
#131868 = DIRECTION ( 'NONE',  ( -0.7071067811865486830, -0.7071067811865464625, -0.000000000000000000 ) ) ;
#131869 = LINE ( 'NONE', #45600, #11304 ) ;
#131870 = DIRECTION ( 'NONE',  ( -0.7071067811865487940, 0.7071067811865463515, -0.000000000000000000 ) ) ;
#131871 = ORIENTED_EDGE ( 'NONE', *, *, #131826, .F. ) ;
#131872 = CARTESIAN_POINT ( 'NONE',  ( 18.01107201284014536, 3.821174125832445049E-16, 0.000000000000000000 ) ) ;
#131873 = ORIENTED_EDGE ( 'NONE', *, *, #10218, .F. ) ;
#131874 = LINE ( 'NONE', #130458, #20228 ) ;
#131875 = EDGE_LOOP ( 'NONE', ( #21730, #31627, #115418, #74461 ) ) ;
#131876 = SURFACE_STYLE_USAGE ( .BOTH. , #87649 ) ;
#131877 = VERTEX_POINT ( 'NONE', #69533 ) ;
#131878 =( REPRESENTATION_RELATIONSHIP ('NONE','NONE', #69070, #428 ) REPRESENTATION_RELATIONSHIP_WITH_TRANSFORMATION ( #20581 )SHAPE_REPRESENTATION_RELATIONSHIP( ) );
#131879 = DIRECTION ( 'NONE',  ( 0.7071067811865487940, 0.7071067811865463515, -0.000000000000000000 ) ) ;
#131880 = ORIENTED_EDGE ( 'NONE', *, *, #66124, .T. ) ;
#131881 = ORIENTED_EDGE ( 'NONE', *, *, #104399, .T. ) ;
#131882 = VERTEX_POINT ( 'NONE', #14412 ) ;
#131883 = CARTESIAN_POINT ( 'NONE',  ( -57.29974487139158157, -27.71228299555246011, 4.000000000000000000 ) ) ;
#131884 = EDGE_CURVE ( 'NONE', #72729, #142002, #37616, .T. ) ;
#131885 = PLANE ( 'NONE',  #87766 ) ;
#131886 = CARTESIAN_POINT ( 'NONE',  ( -2.816011393730999401, 28.73617430169785436, 5.000000000000000000 ) ) ;
#131887 = SURFACE_STYLE_USAGE ( .BOTH. , #141319 ) ;
#131888 = DIRECTION ( 'NONE',  ( -0.000000000000000000, 0.3543493200069153248, 0.9351131265310292928 ) ) ;
#131889 = EDGE_CURVE ( 'NONE', #71084, #83494, #89819, .T. ) ;
#131890 = FACE_OUTER_BOUND ( 'NONE', #119772, .T. ) ;
#131892 = CARTESIAN_POINT ( 'NONE',  ( 24.48921356237309510, -27.52281430457072631, 5.000000000000000000 ) ) ;
#131891 = CARTESIAN_POINT ( 'NONE',  ( -26.29289321881326913, 14.25929247661557220, 5.000000000000000000 ) ) ;
#131893 = CARTESIAN_POINT ( 'NONE',  ( -34.49999999999975842, 22.01701374228152730, 2.453858888625711110 ) ) ;
#131894 = ADVANCED_FACE ( 'NONE', ( #97485 ), #30092, .F. ) ;
#131895 = EDGE_CURVE ( 'NONE', #46307, #141426, #52562, .T. ) ;
#131896 = FILL_AREA_STYLE ('',( #111557 ) ) ;
#131897 = CARTESIAN_POINT ( 'NONE',  ( 24.48921356237309510, -27.52281430457072631, 5.000000000000000000 ) ) ;
#131898 = CARTESIAN_POINT ( 'NONE',  ( 4.499999999999968914, 9.052185695429077583, 5.000000000000000000 ) ) ;
#131899 = VERTEX_POINT ( 'NONE', #4908 ) ;
#131900 = ORIENTED_EDGE ( 'NONE', *, *, #115152, .F. ) ;
#131901 = AXIS2_PLACEMENT_3D ( 'NONE', #26643, #38951, #93328 ) ;
#131902 = ORIENTED_EDGE ( 'NONE', *, *, #89445, .T. ) ;
#131903 = CARTESIAN_POINT ( 'NONE',  ( -8.292893218813384593, -15.74070752338412049, 5.000000000000000000 ) ) ;
#131904 = VECTOR ( 'NONE', #50777, 1000.000000000000000 ) ;
#131905 = ORIENTED_EDGE ( 'NONE', *, *, #61781, .T. ) ;
#131906 = VECTOR ( 'NONE', #97383, 999.9999999999998863 ) ;
#131907 = EDGE_CURVE ( 'NONE', #57945, #63482, #118533, .T. ) ;
#131909 = VERTEX_POINT ( 'NONE', #48463 ) ;
#131908 = AXIS2_PLACEMENT_3D ( 'NONE', #72194, #93887, #17055 ) ;
#131910 = CARTESIAN_POINT ( 'NONE',  ( 42.18398860626899705, 28.73617430169816700, 5.000000000000000000 ) ) ;
#131911 = CARTESIAN_POINT ( 'NONE',  ( 0.000000000000000000, -30.18000000000009564, 15.92499999999935945 ) ) ;
#131912 = ADVANCED_FACE ( 'NONE', ( #92664 ), #49207, .F. ) ;
#131913 = EDGE_CURVE ( 'NONE', #38574, #18661, #20639, .T. ) ;
#131914 = DIRECTION ( 'NONE',  ( 0.3543493200069162685, -0.000000000000000000, -0.9351131265310288487 ) ) ;
#131915 = ORIENTED_EDGE ( 'NONE', *, *, #21447, .T. ) ;
#131916 = FACE_OUTER_BOUND ( 'NONE', #67944, .T. ) ;
#131918 = ORIENTED_EDGE ( 'NONE', *, *, #101427, .T. ) ;
#131917 = MECHANICAL_DESIGN_GEOMETRIC_PRESENTATION_REPRESENTATION (  '', ( #57851 ), #9224 ) ;
#131919 =( BOUNDED_CURVE ( )  B_SPLINE_CURVE ( 2, ( #112168, #67229, #45503, #21581, #33208, #78828, #77419, #46216, #120870, #123038, #87546, #54241, #131773 ),
 .UNSPECIFIED., .F., .T. ) 
 B_SPLINE_CURVE_WITH_KNOTS ( ( 3, 2, 2, 2, 2, 2, 3 ),
 ( 0.5500000000000001554, 0.5583333333333334592, 0.5666666666666667629, 0.5750000000000000666, 0.5833333333333334814, 0.5916666666666667851, 0.6000000000000000888 ),
 .UNSPECIFIED. ) 
 CURVE ( )  GEOMETRIC_REPRESENTATION_ITEM ( )  RATIONAL_B_SPLINE_CURVE ( ( 0.9999999999999995559, 0.9659258262890687563, 1.000000000000000000, 0.9659258262890683122, 1.000000000000000000, 0.9659258262890683122, 1.000000000000000000, 0.9659258262890683122, 1.000000000000000000, 0.9659258262890683122, 1.000000000000000000, 0.9659258262890678681, 1.000000000000000444 ) ) 
 REPRESENTATION_ITEM ( '' )  );
#131920 = PLANE ( 'NONE',  #35827 ) ;
#131921 = EDGE_CURVE ( 'NONE', #7595, #59056, #130874, .T. ) ;
#131923 = VECTOR ( 'NONE', #102876, 1000.000000000000000 ) ;
#131922 = CARTESIAN_POINT ( 'NONE',  ( 16.25456980810188767, -6.871911579029512218, 3.967499999999996252 ) ) ;
#131924 = ORIENTED_EDGE ( 'NONE', *, *, #84623, .T. ) ;
#131925 = CARTESIAN_POINT ( 'NONE',  ( 92.66209685856479439, -5.291415217122919401, 3.054999999999998384 ) ) ;
#131926 = EDGE_CURVE ( 'NONE', #134787, #68809, #108334, .T. ) ;
#131927 = CARTESIAN_POINT ( 'NONE',  ( 6.342504469876894646, -9.325618364798961224, -1.816862207259552608 ) ) ;
#131928 = CARTESIAN_POINT ( 'NONE',  ( -5.994519915287488843, 28.92564299267942118, 4.000000000000000000 ) ) ;
#131929 = CARTESIAN_POINT ( 'NONE',  ( 0.000000000000000000, 0.000000000000000000, 5.000000000000000000 ) ) ;
#131930 = ORIENTED_EDGE ( 'NONE', *, *, #71435, .F. ) ;
#131931 = ORIENTED_EDGE ( 'NONE', *, *, #9985, .F. ) ;
#131932 = EDGE_LOOP ( 'NONE', ( #73632, #67981, #42830, #84633 ) ) ;
#131934 = VECTOR ( 'NONE', #121946, 1000.000000000000000 ) ;
#131933 = PLANE ( 'NONE',  #35759 ) ;
#131935 = FACE_OUTER_BOUND ( 'NONE', #72083, .T. ) ;
#131937 = DIRECTION ( 'NONE',  ( 0.000000000000000000, 0.000000000000000000, 1.000000000000000000 ) ) ;
#131936 = VECTOR ( 'NONE', #15387, 1000.000000000000000 ) ;
#131938 = EDGE_CURVE ( 'NONE', #116539, #97084, #75072, .T. ) ;
#131939 = CARTESIAN_POINT ( 'NONE',  ( -5.999999999999954703, -0.4125381241607533611, 4.000000000000000000 ) ) ;
#131940 = CARTESIAN_POINT ( 'NONE',  ( 23.67183060077630685, 11.25929247661559884, 4.000000000000000000 ) ) ;
#131941 = ORIENTED_EDGE ( 'NONE', *, *, #24988, .F. ) ;
#131942 = DIRECTION ( 'NONE',  ( 0.7071067811865487940, 0.7071067811865463515, 0.000000000000000000 ) ) ;
#131943 = AXIS2_PLACEMENT_3D ( 'NONE', #73344, #139328, #109335 ) ;
#131944 = FACE_OUTER_BOUND ( 'NONE', #26710, .T. ) ;
#131945 = CARTESIAN_POINT ( 'NONE',  ( -75.18398860626899705, 28.73617430169839793, 5.000000000000000000 ) ) ;
#131946 = ORIENTED_EDGE ( 'NONE', *, *, #28726, .T. ) ;
#131947 = DIRECTION ( 'NONE',  ( -0.5735764363510501562, 0.8191520442889890230, 1.003171929053521419E-16 ) ) ;
#131948 = ADVANCED_FACE ( 'NONE', ( #9008 ), #29374, .F. ) ;
#131949 = VECTOR ( 'NONE', #143223, 1000.000000000000000 ) ;
#131951 = VECTOR ( 'NONE', #40169, 1000.000000000000000 ) ;
#131950 = CARTESIAN_POINT ( 'NONE',  ( -15.79289321881334551, 18.75929247661552424, 5.000000000000000000 ) ) ;
#131952 = ORIENTED_EDGE ( 'NONE', *, *, #92112, .F. ) ;
#131953 = VECTOR ( 'NONE', #30322, 1000.000000000000227 ) ;
#131955 = VERTEX_POINT ( 'NONE', #60074 ) ;
#131954 = CARTESIAN_POINT ( 'NONE',  ( -11.99451991528749417, 28.92564299267946382, 4.000000000000000000 ) ) ;
#131956 = ORIENTED_EDGE ( 'NONE', *, *, #101594, .T. ) ;
#131957 = AXIS2_PLACEMENT_3D ( 'NONE', #27553, #60974, #105133 ) ;
#131958 = DIRECTION ( 'NONE',  ( 1.000000000000000000, 0.000000000000000000, 0.000000000000000000 ) ) ;
#131959 = AXIS2_PLACEMENT_3D ( 'NONE', #52442, #11054, #57482 ) ;
#131960 = CARTESIAN_POINT ( 'NONE',  ( -9.489213562373095101, -27.52281430457062328, 5.000000000000000000 ) ) ;
#131961 = EDGE_LOOP ( 'NONE', ( #42913, #133050, #27516, #137885 ) ) ;
#131962 = DIRECTION ( 'NONE',  ( -0.7071067811865486830, -0.7071067811865464625, 0.000000000000000000 ) ) ;
#131963 = DIRECTION ( 'NONE',  ( 0.000000000000000000, -1.000000000000000000, 0.000000000000000000 ) ) ;
#131964 = EDGE_CURVE ( 'NONE', #118228, #76385, #96057, .T. ) ;
#131965 = PLANE ( 'NONE',  #138755 ) ;
#131966 = CARTESIAN_POINT ( 'NONE',  ( 45.29974487139158867, -27.71228299555237840, 4.000000000000000000 ) ) ;
#131967 = CARTESIAN_POINT ( 'NONE',  ( 31.04166666666666075, -3.975000000000002753, 6.884901960086286188 ) ) ;
#131968 = LINE ( 'NONE', #42822, #130096 ) ;
#131969 = CARTESIAN_POINT ( 'NONE',  ( -13.49999999999991118, -4.796895815301030375, -3.611700055028712164 ) ) ;
#131970 = CYLINDRICAL_SURFACE ( 'NONE', #83110, 7.950000000000000178 ) ;
#131972 = VECTOR ( 'NONE', #17639, 1000.000000000000000 ) ;
#131971 = LINE ( 'NONE', #110179, #103636 ) ;
#131973 = LINE ( 'NONE', #76153, #102401 ) ;
#131974 = DIRECTION ( 'NONE',  ( -0.7071067811865487940, 0.7071067811865463515, 0.000000000000000000 ) ) ;
#131975 = EDGE_CURVE ( 'NONE', #40996, #100682, #85910, .T. ) ;
#131976 = DIRECTION ( 'NONE',  ( 1.000000000000000000, 0.000000000000000000, 0.000000000000000000 ) ) ;
#131977 = CARTESIAN_POINT ( 'NONE',  ( 101.2875270504628986, 0.000000000000000000, -7.949999999999998401 ) ) ;
#131978 = ORIENTED_EDGE ( 'NONE', *, *, #11052, .F. ) ;
#131979 = ORIENTED_EDGE ( 'NONE', *, *, #56680, .F. ) ;
#131980 = CARTESIAN_POINT ( 'NONE',  ( 101.7708333333333428, -7.949999999999999289, -2.130196079827426203 ) ) ;
#131981 = ORIENTED_EDGE ( 'NONE', *, *, #133188, .F. ) ;
#131982 = ORIENTED_EDGE ( 'NONE', *, *, #33590, .T. ) ;
#131983 = EDGE_LOOP ( 'NONE', ( #84542, #77911, #84437, #47012 ) ) ;
#131984 = PLANE ( 'NONE',  #105762 ) ;
#131985 = CARTESIAN_POINT ( 'NONE',  ( 128.5894344200537489, -57.14999999999999147, 39.86617647058822911 ) ) ;
#131986 = VECTOR ( 'NONE', #128518, 1000.000000000000000 ) ;
#131987 = VERTEX_POINT ( 'NONE', #63487 ) ;
#131988 = CARTESIAN_POINT ( 'NONE',  ( -34.49999999999975131, 12.43112307739205846, 4.000000000000000000 ) ) ;
#131989 =( NAMED_UNIT ( * ) SI_UNIT ( $, .STERADIAN. ) SOLID_ANGLE_UNIT ( ) );
#131990 = DIRECTION ( 'NONE',  ( 1.000000000000000000, 0.000000000000000000, 0.000000000000000000 ) ) ;
#131991 = FACE_OUTER_BOUND ( 'NONE', #133612, .T. ) ;
#131992 = ORIENTED_EDGE ( 'NONE', *, *, #53213, .T. ) ;
#131993 = CARTESIAN_POINT ( 'NONE',  ( 9.512856086559503765, 9.797339893906631403, -29.02678346616960425 ) ) ;
#131994 = PLANE ( 'NONE',  #121438 ) ;
#131995 = LINE ( 'NONE', #55143, #28212 ) ;
#131996 = LINE ( 'NONE', #76918, #5847 ) ;
#131997 = PRESENTATION_LAYER_ASSIGNMENT (  '', '', ( #13869 ) ) ;
#131998 = CARTESIAN_POINT ( 'NONE',  ( 39.48921356237310221, -27.52281430457082934, 5.000000000000000000 ) ) ;
#131999 = LINE ( 'NONE', #31957, #54647 ) ;
#132000 = CARTESIAN_POINT ( 'NONE',  ( 27.20419371712955225, -6.884901960086285300, -3.975000000000000089 ) ) ;
#132001 = CARTESIAN_POINT ( 'NONE',  ( 0.000000000000000000, 16.93112307739200872, 4.000000000000000000 ) ) ;
#132002 = ORIENTED_EDGE ( 'NONE', *, *, #4612, .F. ) ;
#132003 = ORIENTED_EDGE ( 'NONE', *, *, #64691, .F. ) ;
#132004 = CARTESIAN_POINT ( 'NONE',  ( 121.7712635252314328, 4.472830434245839371, 4.472830434245842035 ) ) ;
#132005 = ORIENTED_EDGE ( 'NONE', *, *, #108460, .T. ) ;
#132006 = DIRECTION ( 'NONE',  ( -0.000000000000000000, 0.000000000000000000, 1.000000000000000000 ) ) ;
#132007 = EDGE_CURVE ( 'NONE', #94828, #56865, #106941, .T. ) ;
#132008 = CARTESIAN_POINT ( 'NONE',  ( -26.20710678118636139, 12.75929247661559351, 5.000000000000000000 ) ) ;
#132009 = LINE ( 'NONE', #111677, #108182 ) ;
#132010 = DIRECTION ( 'NONE',  ( -1.000000000000000000, -1.224606353822377258E-16, -0.000000000000000000 ) ) ;
#132011 =( NAMED_UNIT ( * ) SI_UNIT ( $, .STERADIAN. ) SOLID_ANGLE_UNIT ( ) );
#132012 = VECTOR ( 'NONE', #141923, 1000.000000000000000 ) ;
#132013 = CARTESIAN_POINT ( 'NONE',  ( 113.5162635252314516, -4.472830434245839371, 4.472830434245839371 ) ) ;
#132014 = ORIENTED_EDGE ( 'NONE', *, *, #46410, .T. ) ;
#132015 = ORIENTED_EDGE ( 'NONE', *, *, #15049, .T. ) ;
#132016 = CARTESIAN_POINT ( 'NONE',  ( 69.78752705046289861, 0.000000000000000000, -7.949999999999998401 ) ) ;
#132017 = VECTOR ( 'NONE', #77898, 999.9999999999998863 ) ;
#132018 = AXIS2_PLACEMENT_3D ( 'NONE', #113017, #58718, #24589 ) ;
#132019 = AXIS2_PLACEMENT_3D ( 'NONE', #7973, #96400, #98568 ) ;
#132020 = DIRECTION ( 'NONE',  ( 1.000000000000000000, 0.000000000000000000, -0.000000000000000000 ) ) ;
#132021 = AXIS2_PLACEMENT_3D ( 'NONE', #43616, #63962, #20420 ) ;
#132022 = VERTEX_POINT ( 'NONE', #26711 ) ;
#132023 = ORIENTED_EDGE ( 'NONE', *, *, #34063, .F. ) ;
#132024 = CARTESIAN_POINT ( 'NONE',  ( 40.68793019189811133, 6.110000000000002984, -1.637169565754156730 ) ) ;
#132025 = EDGE_CURVE ( 'NONE', #56807, #80300, #46677, .T. ) ;
#132026 = ORIENTED_EDGE ( 'NONE', *, *, #25023, .F. ) ;
#132027 = CARTESIAN_POINT ( 'NONE',  ( 15.48921356237309510, -27.52281430457066236, 5.000000000000000000 ) ) ;
#132028 = CARTESIAN_POINT ( 'NONE',  ( 29.90156419391745857, 11.25929247661560240, 10.79108189686413866 ) ) ;
#132029 = LINE ( 'NONE', #99353, #110850 ) ;
#132030 = VECTOR ( 'NONE', #73329, 1000.000000000000000 ) ;
#132031 = EDGE_CURVE ( 'NONE', #55786, #42348, #85181, .T. ) ;
#132032 = EDGE_CURVE ( 'NONE', #132148, #111457, #60732, .T. ) ;
#132033 = CARTESIAN_POINT ( 'NONE',  ( 41.91209685856478728, 5.291415217122921177, -3.054999999999994831 ) ) ;
#132034 = ORIENTED_EDGE ( 'NONE', *, *, #87918, .T. ) ;
#132035 = EDGE_CURVE ( 'NONE', #45162, #22876, #137633, .T. ) ;
#132036 = LINE ( 'NONE', #32727, #115013 ) ;
#132037 = ORIENTED_EDGE ( 'NONE', *, *, #135406, .T. ) ;
#132038 = ORIENTED_EDGE ( 'NONE', *, *, #120399, .F. ) ;
#132039 = VECTOR ( 'NONE', #139811, 1000.000000000000000 ) ;
#132040 = ORIENTED_EDGE ( 'NONE', *, *, #109631, .F. ) ;
#132041 = EDGE_CURVE ( 'NONE', #53146, #24456, #82526, .T. ) ;
#132042 = VECTOR ( 'NONE', #131337, 1000.000000000000000 ) ;
#132043 = DIRECTION ( 'NONE',  ( -0.7071067811865486830, -0.7071067811865464625, 0.000000000000000000 ) ) ;
#132044 = ORIENTED_EDGE ( 'NONE', *, *, #20383, .F. ) ;
#132045 = DIRECTION ( 'NONE',  ( 0.7071067811865487940, 0.7071067811865463515, -0.000000000000000000 ) ) ;
#132046 = VECTOR ( 'NONE', #96102, 1000.000000000000000 ) ;
#132047 = FACE_OUTER_BOUND ( 'NONE', #17064, .T. ) ;
#132048 = SURFACE_STYLE_FILL_AREA ( #100827 ) ;
#132049 = ADVANCED_FACE ( 'NONE', ( #98912 ), #33003, .F. ) ;
#132050 = VECTOR ( 'NONE', #76172, 1000.000000000000000 ) ;
#132051 = CARTESIAN_POINT ( 'NONE',  ( -6.489213562373093325, -27.52281430457059841, 5.000000000000000000 ) ) ;
#132052 = FACE_BOUND ( 'NONE', #86244, .T. ) ;
#132053 = VERTEX_POINT ( 'NONE', #22066 ) ;
#132054 = LINE ( 'NONE', #55926, #75820 ) ;
#132055 = CARTESIAN_POINT ( 'NONE',  ( 11.29289321881338104, -18.74070752338409562, 5.000000000000000000 ) ) ;
#132056 = CARTESIAN_POINT ( 'NONE',  ( 0.000000000000000000, 0.000000000000000000, 5.000000000000000000 ) ) ;
#132057 = ORIENTED_EDGE ( 'NONE', *, *, #58584, .T. ) ;
#132058 = LINE ( 'NONE', #110968, #61987 ) ;
#132059 = ORIENTED_EDGE ( 'NONE', *, *, #123572, .F. ) ;
#132061 = EDGE_LOOP ( 'NONE', ( #106194, #88270, #58505, #67534, #121337 ) ) ;
#132060 = EDGE_CURVE ( 'NONE', #85002, #100524, #65639, .T. ) ;
#132062 = EDGE_CURVE ( 'NONE', #129167, #133316, #133714, .T. ) ;
#132063 = CARTESIAN_POINT ( 'NONE',  ( 19.82816939922339827, -14.24070752338414003, 4.000000000000000000 ) ) ;
#132064 = ORIENTED_EDGE ( 'NONE', *, *, #135614, .F. ) ;
#132065 = CARTESIAN_POINT ( 'NONE',  ( 48.91209685856478018, 5.291415217122921177, -3.054999999999994831 ) ) ;
#132066 = ORIENTED_EDGE ( 'NONE', *, *, #32747, .T. ) ;
#132067 = VECTOR ( 'NONE', #77842, 1000.000000000000000 ) ;
#132068 = CARTESIAN_POINT ( 'NONE',  ( 30.48921356237309510, -27.52281430457076894, 5.000000000000000000 ) ) ;
#132069 = LINE ( 'NONE', #43607, #31101 ) ;
#132070 = CARTESIAN_POINT ( 'NONE',  ( 4.288407645496676857, 9.139736423841732040E-16, 0.000000000000000000 ) ) ;
#132071 = EDGE_CURVE ( 'NONE', #47310, #52143, #100115, .T. ) ;
#132072 = ORIENTED_EDGE ( 'NONE', *, *, #11583, .F. ) ;
#132073 = CARTESIAN_POINT ( 'NONE',  ( 7.499999999999949374, 16.77039438581780217, 0.4657186855307575701 ) ) ;
#132075 = LINE ( 'NONE', #101550, #13425 ) ;
#132074 = VECTOR ( 'NONE', #32680, 1000.000000000000000 ) ;
#132076 = EDGE_CURVE ( 'NONE', #39432, #48488, #90188, .T. ) ;
#132077 = ADVANCED_FACE ( 'NONE', ( #11163 ), #134434, .F. ) ;
#132078 = DIRECTION ( 'NONE',  ( 1.000000000000000000, -0.000000000000000000, -0.000000000000000000 ) ) ;
#132079 = CARTESIAN_POINT ( 'NONE',  ( -34.92500000000001137, -21.72500000000000142, 0.4999999999999995559 ) ) ;
#132080 = LINE ( 'NONE', #75548, #92257 ) ;
#132081 = LINE ( 'NONE', #129187, #28519 ) ;
#132082 = CARTESIAN_POINT ( 'NONE',  ( -48.29974487139158867, -27.71228299555239971, 4.000000000000000000 ) ) ;
#132083 = ORIENTED_EDGE ( 'NONE', *, *, #106068, .F. ) ;
#132084 = VERTEX_POINT ( 'NONE', #111969 ) ;
#132085 = VECTOR ( 'NONE', #31878, 1000.000000000000000 ) ;
#132086 = ORIENTED_EDGE ( 'NONE', *, *, #94870, .F. ) ;
#132087 = DIRECTION ( 'NONE',  ( 0.9707728879609287542, 0.000000000000000000, -0.2399999999999954392 ) ) ;
#132088 = FACE_OUTER_BOUND ( 'NONE', #118059, .T. ) ;
#132089 = ORIENTED_EDGE ( 'NONE', *, *, #108438, .T. ) ;
#132090 = ADVANCED_FACE ( 'NONE', ( #55440 ), #34393, .F. ) ;
#132091 = ORIENTED_EDGE ( 'NONE', *, *, #88206, .F. ) ;
#132092 = SURFACE_SIDE_STYLE ('',( #121880 ) ) ;
#132093 = FACE_OUTER_BOUND ( 'NONE', #18466, .T. ) ;
#132094 = EDGE_CURVE ( 'NONE', #98043, #71394, #143146, .T. ) ;
#132095 = LINE ( 'NONE', #77707, #76447 ) ;
#132096 = ORIENTED_EDGE ( 'NONE', *, *, #127962, .T. ) ;
#132097 = DIRECTION ( 'NONE',  ( 0.6830127018922180770, -0.6830127018922204085, -0.2588190451025213501 ) ) ;
#132098 = VECTOR ( 'NONE', #3886, 1000.000000000000000 ) ;
#132099 = DIRECTION ( 'NONE',  ( -0.7071067811865486830, -0.7071067811865464625, -0.000000000000000000 ) ) ;
#132100 = CARTESIAN_POINT ( 'NONE',  ( 19.90040314143521982, -7.934999999999989839, 2.126176841940957907 ) ) ;
#132101 = LINE ( 'NONE', #35665, #55386 ) ;
#132102 = ORIENTED_EDGE ( 'NONE', *, *, #38428, .F. ) ;
#132103 = CARTESIAN_POINT ( 'NONE',  ( 124.4537635252314516, -6.109999999999999432, -3.741295971395163529E-16 ) ) ;
#132104 = ADVANCED_FACE ( 'NONE', ( #133020 ), #45303, .T. ) ;
#132105 = DIRECTION ( 'NONE',  ( -0.6830127018922181881, 0.6830127018922202975, -0.2588190451025214056 ) ) ;
#132106 = DIRECTION ( 'NONE',  ( 1.000000000000000000, 0.000000000000000000, 0.000000000000000000 ) ) ;
#132108 = ORIENTED_EDGE ( 'NONE', *, *, #101129, .T. ) ;
#132107 = DIRECTION ( 'NONE',  ( -0.000000000000000000, -0.000000000000000000, 1.000000000000000000 ) ) ;
#132109 = PLANE ( 'NONE',  #18435 ) ;
#132110 = ORIENTED_EDGE ( 'NONE', *, *, #119927, .T. ) ;
#132112 = ADVANCED_FACE ( 'NONE', ( #122828 ), #43846, .F. ) ;
#132111 = VECTOR ( 'NONE', #69497, 999.9999999999998863 ) ;
#132113 = FACE_OUTER_BOUND ( 'NONE', #133968, .T. ) ;
#132114 = DIRECTION ( 'NONE',  ( -0.7071067811865486830, -0.7071067811865464625, 0.000000000000000000 ) ) ;
#132115 = ORIENTED_EDGE ( 'NONE', *, *, #42786, .T. ) ;
#132116 = VECTOR ( 'NONE', #50034, 999.9999999999998863 ) ;
#132117 = VECTOR ( 'NONE', #48207, 999.9999999999998863 ) ;
#132118 = CARTESIAN_POINT ( 'NONE',  ( 7.499999999999951150, 5.696342897626511359, -7.587980461218381656 ) ) ;
#132119 = DIRECTION ( 'NONE',  ( -0.3543493200069162685, -0.000000000000000000, -0.9351131265310288487 ) ) ;
#132120 = ORIENTED_EDGE ( 'NONE', *, *, #44034, .F. ) ;
#132121 = VECTOR ( 'NONE', #33533, 1000.000000000000000 ) ;
#132122 = CIRCLE ( 'NONE', #27893, 2.055000000000001048 ) ;
#132123 = CARTESIAN_POINT ( 'NONE',  ( -6.707106781186497280, 17.25929247661554911, 5.000000000000000000 ) ) ;
#132124 = MECHANICAL_DESIGN_GEOMETRIC_PRESENTATION_REPRESENTATION (  '', ( #65069 ), #106611 ) ;
#132125 = CARTESIAN_POINT ( 'NONE',  ( 21.29974487139158512, -27.71228299555221142, 4.000000000000000000 ) ) ;
#132127 = ORIENTED_EDGE ( 'NONE', *, *, #29549, .F. ) ;
#132126 = AXIS2_PLACEMENT_3D ( 'NONE', #6148, #29356, #50425 ) ;
#132128 = CARTESIAN_POINT ( 'NONE',  ( -2.721745484314253005, 8.259292476615630818, 11.78515199841150007 ) ) ;
#132130 = VERTEX_POINT ( 'NONE', #9772 ) ;
#132129 = DIRECTION ( 'NONE',  ( 0.7071067811865486830, -0.7071067811865464625, -0.000000000000000000 ) ) ;
#132131 = EDGE_LOOP ( 'NONE', ( #66271, #77541, #315, #25799 ) ) ;
#132132 = DIRECTION ( 'NONE',  ( 0.7071067811865487940, 0.7071067811865463515, -0.000000000000000000 ) ) ;
#132133 = VECTOR ( 'NONE', #129830, 1000.000000000000000 ) ;
#132134 = CARTESIAN_POINT ( 'NONE',  ( 75.48921356237309510, -27.52281430457107803, 5.000000000000000000 ) ) ;
#132135 = ORIENTED_EDGE ( 'NONE', *, *, #37611, .T. ) ;
#132136 = LINE ( 'NONE', #74912, #73683 ) ;
#132137 = EDGE_CURVE ( 'NONE', #48771, #70033, #88063, .T. ) ;
#132138 = LINE ( 'NONE', #32828, #124765 ) ;
#132139 = FACE_OUTER_BOUND ( 'NONE', #107177, .T. ) ;
#132140 = ORIENTED_EDGE ( 'NONE', *, *, #1244, .T. ) ;
#132141 = DIRECTION ( 'NONE',  ( 0.7071067811865487940, -0.7071067811865463515, 0.000000000000000000 ) ) ;
#132142 = LINE ( 'NONE', #42279, #44436 ) ;
#132143 = DIRECTION ( 'NONE',  ( -0.000000000000000000, 0.000000000000000000, 1.000000000000000000 ) ) ;
#132144 = AXIS2_PLACEMENT_3D ( 'NONE', #64202, #74373, #107682 ) ;
#132145 = CARTESIAN_POINT ( 'NONE',  ( 41.03709685856478728, -3.054999999999999272, -5.291415217122919401 ) ) ;
#132146 = DIRECTION ( 'NONE',  ( 0.000000000000000000, -1.000000000000000000, 0.000000000000000000 ) ) ;
#132147 = AXIS2_PLACEMENT_3D ( 'NONE', #105942, #139352, #115375 ) ;
#132148 = VERTEX_POINT ( 'NONE', #54037 ) ;
#132149 = ORIENTED_EDGE ( 'NONE', *, *, #13494, .T. ) ;
#132150 = CARTESIAN_POINT ( 'NONE',  ( 125.8333333333333286, -6.884901960086287964, 3.974999999999998312 ) ) ;
#132151 = AXIS2_PLACEMENT_3D ( 'NONE', #127039, #105982, #139397 ) ;
#132152 = ORIENTED_EDGE ( 'NONE', *, *, #78802, .T. ) ;
#132153 = AXIS2_PLACEMENT_3D ( 'NONE', #87048, #121791, #33421 ) ;
#132154 = VERTEX_POINT ( 'NONE', #101056 ) ;
#132155 = LINE ( 'NONE', #21935, #110424 ) ;
#132156 = CARTESIAN_POINT ( 'NONE',  ( 18.09667064187394914, -2.240707523384257716, 15.26439735382756346 ) ) ;
#132157 = AXIS2_PLACEMENT_3D ( 'NONE', #24942, #80095, #98938 ) ;
#132158 = ORIENTED_EDGE ( 'NONE', *, *, #71929, .F. ) ;
#132159 = DIRECTION ( 'NONE',  ( -0.7071067811865486830, 0.7071067811865464625, 0.000000000000000000 ) ) ;
#132160 = DIRECTION ( 'NONE',  ( 1.000000000000000000, 0.000000000000000000, 0.000000000000000000 ) ) ;
#132161 = CARTESIAN_POINT ( 'NONE',  ( 8.999999999999941380, 14.96639925780211478, 5.000000000000000000 ) ) ;
#132162 = CARTESIAN_POINT ( 'NONE',  ( 15.29974487139158867, -27.71228299555216879, 4.000000000000000000 ) ) ;
#132163 = CARTESIAN_POINT ( 'NONE',  ( 117.8337635252314470, 6.110000000000001208, 1.122388791418549305E-15 ) ) ;
#132164 = VECTOR ( 'NONE', #116956, 1000.000000000000000 ) ;
#132165 = VERTEX_POINT ( 'NONE', #121386 ) ;
#132166 = CARTESIAN_POINT ( 'NONE',  ( -34.92500000000001137, 7.701930566820932356, 4.500000000000000888 ) ) ;
#132167 = CYLINDRICAL_SURFACE ( 'NONE', #141740, 2.552699999999959779 ) ;
#132168 = CARTESIAN_POINT ( 'NONE',  ( -2.671830600776449405, 2.259292476615697876, 4.000000000000000000 ) ) ;
#132169 = CARTESIAN_POINT ( 'NONE',  ( 18.18398860626898994, 28.73617430169800002, 5.000000000000000000 ) ) ;
#132170 = DIRECTION ( 'NONE',  ( 0.7071067811865486830, -0.7071067811865464625, -0.000000000000000000 ) ) ;
#132171 = CARTESIAN_POINT ( 'NONE',  ( 0.000000000000000000, 0.000000000000000000, -10.00000000000000000 ) ) ;
#132172 = CYLINDRICAL_SURFACE ( 'NONE', #36579, 0.5000000000000004441 ) ;
#132173 = CARTESIAN_POINT ( 'NONE',  ( 55.64169371712955581, -2.130196079827424871, -7.949999999999999289 ) ) ;
#132174 = CARTESIAN_POINT ( 'NONE',  ( 2.999999999999999556, 2.500000000000000000, 0.000000000000000000 ) ) ;
#132175 = CARTESIAN_POINT ( 'NONE',  ( -69.29974487139159578, -27.71228299555254537, 4.000000000000000000 ) ) ;
#132176 = EDGE_LOOP ( 'NONE', ( #85391, #78837, #72318, #93660 ) ) ;
#132177 = ORIENTED_EDGE ( 'NONE', *, *, #51338, .T. ) ;
#132178 = CARTESIAN_POINT ( 'NONE',  ( 48.10416666666665009, 2.130196079827422206, 7.950000000000001954 ) ) ;
#132179 = PLANE ( 'NONE',  #41379 ) ;
#132180 = VECTOR ( 'NONE', #84725, 1000.000000000000000 ) ;
#132181 = CARTESIAN_POINT ( 'NONE',  ( -12.70000000000000995, 12.19802518668052294, 4.711086268963008195 ) ) ;
#132182 = ORIENTED_EDGE ( 'NONE', *, *, #8443, .T. ) ;
#132183 = CARTESIAN_POINT ( 'NONE',  ( -2.345055162546169747, 5.259292476615669010, 12.77922209995893255 ) ) ;
#132184 = DIRECTION ( 'NONE',  ( -0.7071067811865487940, 0.7071067811865463515, -0.000000000000000000 ) ) ;
#132185 = CARTESIAN_POINT ( 'NONE',  ( 44.62543019189810423, 5.291415217122919401, 3.055000000000002824 ) ) ;
#132186 = ORIENTED_EDGE ( 'NONE', *, *, #103576, .F. ) ;
#132187 = EDGE_CURVE ( 'NONE', #45797, #9933, #33700, .T. ) ;
#132188 = ADVANCED_FACE ( 'NONE', ( #88792 ), #46006, .F. ) ;
#132189 = CARTESIAN_POINT ( 'NONE',  ( 0.1600000000000026401, -9.717572351234235426E-16, -7.934999999999990727 ) ) ;
#132190 = ORIENTED_EDGE ( 'NONE', *, *, #110122, .T. ) ;
#132191 = ORIENTED_EDGE ( 'NONE', *, *, #123542, .T. ) ;
#132192 = AXIS2_PLACEMENT_3D ( 'NONE', #108509, #111390, #99815 ) ;
#132193 = DIRECTION ( 'NONE',  ( 0.7071067811865487940, 0.7071067811865463515, 0.000000000000000000 ) ) ;
#132194 = DIRECTION ( 'NONE',  ( 0.000000000000000000, -1.000000000000000000, 0.000000000000000000 ) ) ;
#132195 = CYLINDRICAL_SURFACE ( 'NONE', #9316, 7.950000000000000178 ) ;
#132196 = ADVANCED_FACE ( 'NONE', ( #32257 ), #120659, .F. ) ;
#132197 = PLANE ( 'NONE',  #120388 ) ;
#132198 = VERTEX_POINT ( 'NONE', #54731 ) ;
#132199 = LINE ( 'NONE', #21278, #39647 ) ;
#132200 = EDGE_CURVE ( 'NONE', #44009, #71093, #137287, .T. ) ;
#132201 = EDGE_CURVE ( 'NONE', #78047, #108780, #37980, .T. ) ;
#132203 = VERTEX_POINT ( 'NONE', #136542 ) ;
#132202 = DIRECTION ( 'NONE',  ( -0.7071067811865487940, 0.7071067811865463515, 0.000000000000000000 ) ) ;
#132204 = CARTESIAN_POINT ( 'NONE',  ( 82.39626352523143282, 4.472830434245840259, -4.472830434245838482 ) ) ;
#132205 = FACE_OUTER_BOUND ( 'NONE', #72691, .T. ) ;
#132206 = PRESENTATION_STYLE_ASSIGNMENT (( #88698 ) ) ;
#132207 = DIRECTION ( 'NONE',  ( -1.000000000000000000, -0.000000000000000000, 0.000000000000000000 ) ) ;
#132208 = DIRECTION ( 'NONE',  ( -0.7071067811865487940, 0.7071067811865463515, 0.000000000000000000 ) ) ;
#132209 = CIRCLE ( 'NONE', #85918, 2.500000000000000888 ) ;
#132210 = PLANE ( 'NONE',  #110956 ) ;
#132211 = ADVANCED_FACE ( 'NONE', ( #92315 ), #115473, .T. ) ;
#132212 = EDGE_CURVE ( 'NONE', #140579, #9125, #3850, .T. ) ;
#132213 = VERTEX_POINT ( 'NONE', #26380 ) ;
#132214 = CARTESIAN_POINT ( 'NONE',  ( -11.99999999999992717, 9.631307414974314085, -9.079085613539570332 ) ) ;
#132215 = CARTESIAN_POINT ( 'NONE',  ( 64.95376352523145158, -6.109999999999998543, -3.741295971395162543E-16 ) ) ;
#132216 = DIRECTION ( 'NONE',  ( 0.7071067811865487940, 0.7071067811865463515, 0.000000000000000000 ) ) ;
#132217 = EDGE_CURVE ( 'NONE', #40999, #25787, #38677, .T. ) ;
#132218 = DIRECTION ( 'NONE',  ( 0.3543493200069163240, -0.000000000000000000, -0.9351131265310288487 ) ) ;
#132219 = DIRECTION ( 'NONE',  ( -0.6830127018922181881, 0.6830127018922202975, -0.2588190451025214056 ) ) ;
#132220 = ORIENTED_EDGE ( 'NONE', *, *, #71689, .T. ) ;
#132221 = ORIENTED_EDGE ( 'NONE', *, *, #77418, .F. ) ;
#132223 = AXIS2_PLACEMENT_3D ( 'NONE', #16531, #49920, #4913 ) ;
#132222 =( NAMED_UNIT ( * ) PLANE_ANGLE_UNIT ( ) SI_UNIT ( $, .RADIAN. ) );
#132224 = ORIENTED_EDGE ( 'NONE', *, *, #119757, .F. ) ;
#132225 = AXIS2_PLACEMENT_3D ( 'NONE', #117755, #141703, #108302 ) ;
#132226 = EDGE_CURVE ( 'NONE', #106919, #61275, #78982, .T. ) ;
#132228 = VERTEX_POINT ( 'NONE', #24237 ) ;
#132227 = VECTOR ( 'NONE', #137917, 1000.000000000000000 ) ;
#132229 = CARTESIAN_POINT ( 'NONE',  ( -13.49999999999992184, 10.08746187583916054, 4.000000000000000000 ) ) ;
#132230 = ORIENTED_EDGE ( 'NONE', *, *, #73781, .T. ) ;
#132231 = PLANE ( 'NONE',  #2920 ) ;
#132232 = DIRECTION ( 'NONE',  ( -0.6830127018922180770, -0.6830127018922204085, -0.2588190451025213501 ) ) ;
#132233 = VECTOR ( 'NONE', #34061, 1000.000000000000227 ) ;
#132234 = VECTOR ( 'NONE', #119111, 1000.000000000000000 ) ;
#132235 = CIRCLE ( 'NONE', #28001, 2.500000000000000888 ) ;
#132236 = VECTOR ( 'NONE', #31100, 1000.000000000000227 ) ;
#132237 = VECTOR ( 'NONE', #72032, 1000.000000000000000 ) ;
#132238 = CARTESIAN_POINT ( 'NONE',  ( -8.510786437626906675, -27.52281430457049183, 5.000000000000000000 ) ) ;
#132239 = FACE_BOUND ( 'NONE', #137832, .T. ) ;
#132240 = LINE ( 'NONE', #22004, #112744 ) ;
#132241 = CARTESIAN_POINT ( 'NONE',  ( 41.05836038379621300, -7.949999999999996625, -2.130196079827426203 ) ) ;
#132243 = DIRECTION ( 'NONE',  ( 0.7071067811865486830, -0.7071067811865464625, -0.000000000000000000 ) ) ;
#132242 = VECTOR ( 'NONE', #30911, 999.9999999999998863 ) ;
#132245 = EDGE_LOOP ( 'NONE', ( #11597, #108279, #19942 ) ) ;
#132244 = CARTESIAN_POINT ( 'NONE',  ( 51.99586038379622011, -3.974999999999998312, -6.884901960086286188 ) ) ;
#132246 = EDGE_CURVE ( 'NONE', #21069, #16647, #93769, .T. ) ;
#132247 = PLANE ( 'NONE',  #48647 ) ;
#132248 = CONTEXT_DEPENDENT_SHAPE_REPRESENTATION ( #94790, #74823 ) ;
#132249 = VERTEX_POINT ( 'NONE', #13322 ) ;
#132250 = ORIENTED_EDGE ( 'NONE', *, *, #35562, .F. ) ;
#132251 = CARTESIAN_POINT ( 'NONE',  ( 76.76626352523142316, 4.472830434245838482, -4.472830434245837594 ) ) ;
#132252 = VERTEX_POINT ( 'NONE', #14775 ) ;
#132253 = CARTESIAN_POINT ( 'NONE',  ( 25.34840764549667469, 9.139736423841732040E-16, 0.000000000000000000 ) ) ;
#132254 = AXIS2_PLACEMENT_3D ( 'NONE', #127210, #96014, #19178 ) ;
#132255 = CARTESIAN_POINT ( 'NONE',  ( 24.48921356237309510, -27.52281430457072631, 5.000000000000000000 ) ) ;
#132256 = EDGE_CURVE ( 'NONE', #8597, #137404, #81790, .T. ) ;
#132257 = AXIS2_PLACEMENT_3D ( 'NONE', #63162, #19615, #102552 ) ;
#132258 = VERTEX_POINT ( 'NONE', #48135 ) ;
#132259 = LINE ( 'NONE', #33655, #109262 ) ;
#132260 = VECTOR ( 'NONE', #103821, 1000.000000000000000 ) ;
#132261 = CARTESIAN_POINT ( 'NONE',  ( 22.49999999999984723, -15.29013452822852415, 0.3645803511610861136 ) ) ;
#132262 = ADVANCED_FACE ( 'NONE', ( #24926 ), #113359, .F. ) ;
#132263 = DIRECTION ( 'NONE',  ( 0.6830127018922181881, 0.6830127018922202975, -0.2588190451025214056 ) ) ;
#132264 = AXIS2_PLACEMENT_3D ( 'NONE', #8905, #98818, #53174 ) ;
#132265 = CARTESIAN_POINT ( 'NONE',  ( -23.29289321881329045, 20.25929247661550647, 5.000000000000000000 ) ) ;
#132266 = LINE ( 'NONE', #88015, #138415 ) ;
#132267 = DIRECTION ( 'NONE',  ( -0.7071067811865487940, 0.7071067811865463515, 0.000000000000000000 ) ) ;
#132268 = EDGE_CURVE ( 'NONE', #71833, #8723, #126219, .T. ) ;
#132269 = DIRECTION ( 'NONE',  ( 0.7071067811865487940, 0.7071067811865463515, -0.000000000000000000 ) ) ;
#132270 = LINE ( 'NONE', #119203, #48594 ) ;
#132271 = EDGE_LOOP ( 'NONE', ( #4549, #45269, #98875, #26387 ) ) ;
#132272 = CARTESIAN_POINT ( 'NONE',  ( -4.171830600776440967, 21.75929247661549937, 4.000000000000000000 ) ) ;
#132273 = ORIENTED_EDGE ( 'NONE', *, *, #114544, .F. ) ;
#132274 = VECTOR ( 'NONE', #37833, 999.9999999999998863 ) ;
#132275 = CARTESIAN_POINT ( 'NONE',  ( 27.99999999999999645, -2.055000000000000160, 0.000000000000000000 ) ) ;
#132276 = DIRECTION ( 'NONE',  ( -1.000000000000000000, 0.000000000000000000, 0.000000000000000000 ) ) ;
#132277 = EDGE_CURVE ( 'NONE', #52856, #80457, #60827, .T. ) ;
#132278 = ORIENTED_EDGE ( 'NONE', *, *, #23155, .T. ) ;
#132279 = ORIENTED_EDGE ( 'NONE', *, *, #45952, .F. ) ;
#132280 = DIRECTION ( 'NONE',  ( 0.7071067811865486830, -0.7071067811865464625, -0.000000000000000000 ) ) ;
#132281 = VERTEX_POINT ( 'NONE', #117619 ) ;
#132282 = CARTESIAN_POINT ( 'NONE',  ( -27.08491323193744904, -12.74070752338414891, 18.74364270924348119 ) ) ;
#132283 = EDGE_CURVE ( 'NONE', #91199, #7626, #72417, .T. ) ;
#132284 = DIRECTION ( 'NONE',  ( -0.3543493200069162685, -0.000000000000000000, -0.9351131265310288487 ) ) ;
#132285 = AXIS2_PLACEMENT_3D ( 'NONE', #17876, #137565, #103472 ) ;
#132286 = CARTESIAN_POINT ( 'NONE',  ( 27.75413961620377279, 3.047499999999993214, -5.278424836066146320 ) ) ;
#132287 = CARTESIAN_POINT ( 'NONE',  ( 17.75907150484199448, 4.272537658411479811, -29.62615593856758167 ) ) ;
#132288 = ORIENTED_EDGE ( 'NONE', *, *, #40757, .F. ) ;
#132289 = EDGE_CURVE ( 'NONE', #105795, #7238, #141016, .T. ) ;
#132290 = CARTESIAN_POINT ( 'NONE',  ( 16.61159235450331906, 9.902892378096218942E-16, 0.000000000000000000 ) ) ;
#132291 = ORIENTED_EDGE ( 'NONE', *, *, #121644, .T. ) ;
#132292 = AXIS2_PLACEMENT_3D ( 'NONE', #115710, #94693, #62109 ) ;
#132293 = PLANE ( 'NONE',  #45249 ) ;
#132295 = VERTEX_POINT ( 'NONE', #95900 ) ;
#132294 = CARTESIAN_POINT ( 'NONE',  ( 0.000000000000000000, 4.999999999999998224, 8.040613248383180784E-16 ) ) ;
#132296 = VECTOR ( 'NONE', #36716, 1000.000000000000000 ) ;
#132297 = EDGE_LOOP ( 'NONE', ( #88562, #97926, #31092, #83304 ) ) ;
#132298 = DIRECTION ( 'NONE',  ( 0.000000000000000000, 1.224646799147353454E-16, 1.000000000000000000 ) ) ;
#132299 = DIRECTION ( 'NONE',  ( -0.7071067811865486830, 0.7071067811865464625, 0.000000000000000000 ) ) ;
#132300 = CARTESIAN_POINT ( 'NONE',  ( 36.29974487139159578, -27.71228299555231445, 4.000000000000000000 ) ) ;
#132301 = ORIENTED_EDGE ( 'NONE', *, *, #45421, .T. ) ;
#132302 = ORIENTED_EDGE ( 'NONE', *, *, #21260, .T. ) ;
#132303 = EDGE_CURVE ( 'NONE', #73203, #54989, #39404, .T. ) ;
#132304 = ORIENTED_EDGE ( 'NONE', *, *, #29396, .F. ) ;
#132305 = CARTESIAN_POINT ( 'NONE',  ( -25.39999999999996305, 0.000000000000000000, 0.000000000000000000 ) ) ;
#132306 = CARTESIAN_POINT ( 'NONE',  ( -11.16347128873443850, 15.75929247661555443, 9.299976744542897578 ) ) ;
#132307 = AXIS2_PLACEMENT_3D ( 'NONE', #75078, #43853, #109083 ) ;
#132308 = CARTESIAN_POINT ( 'NONE',  ( -34.92500000000001137, 21.72500000000000142, 0.4999999999999995559 ) ) ;
#132309 =( NAMED_UNIT ( * ) PLANE_ANGLE_UNIT ( ) SI_UNIT ( $, .RADIAN. ) );
#132310 = CARTESIAN_POINT ( 'NONE',  ( 3.083148067729290176, 21.75929247661549937, 7.311836541448058391 ) ) ;
#132311 = PLANE ( 'NONE',  #81876 ) ;
#132312 = DIRECTION ( 'NONE',  ( 1.000000000000000000, -0.000000000000000000, 0.000000000000000000 ) ) ;
#132313 = ORIENTED_EDGE ( 'NONE', *, *, #34017, .T. ) ;
#132314 = DIRECTION ( 'NONE',  ( -0.7071067811865486830, -0.7071067811865464625, 0.000000000000000000 ) ) ;
#132315 = ORIENTED_EDGE ( 'NONE', *, *, #29068, .F. ) ;
#132316 = CARTESIAN_POINT ( 'NONE',  ( -34.42500000000001137, -19.45860074219779534, 5.000000000000000000 ) ) ;
#132317 = CARTESIAN_POINT ( 'NONE',  ( 0.000000000000000000, 0.000000000000000000, 5.000000000000000000 ) ) ;
#132318 = ADVANCED_FACE ( 'NONE', ( #8152 ), #61876, .F. ) ;
#132319 = ORIENTED_EDGE ( 'NONE', *, *, #49699, .T. ) ;
#132320 = DIRECTION ( 'NONE',  ( -0.7071067811865487940, 0.7071067811865463515, -0.000000000000000000 ) ) ;
#132321 =( BOUNDED_CURVE ( )  B_SPLINE_CURVE ( 3, ( #1503, #121864, #56686, #66105 ),
 .UNSPECIFIED., .F., .T. ) 
 B_SPLINE_CURVE_WITH_KNOTS ( ( 4, 4 ),
 ( 2.001653308786173646, 3.503810798801451742 ),
 .UNSPECIFIED. ) 
 CURVE ( )  GEOMETRIC_REPRESENTATION_ITEM ( )  RATIONAL_B_SPLINE_CURVE ( ( 1.000000000000000000, 0.8206354192515249446, 0.8206354192515249446, 1.000000000000000000 ) ) 
 REPRESENTATION_ITEM ( '' )  );
#132322 = FACE_OUTER_BOUND ( 'NONE', #40514, .T. ) ;
#132323 = CARTESIAN_POINT ( 'NONE',  ( -63.18398860626900415, 28.73617430169831621, 5.000000000000000000 ) ) ;
#132324 = ORIENTED_EDGE ( 'NONE', *, *, #72189, .F. ) ;
#132325 = EDGE_CURVE ( 'NONE', #93801, #73090, #74901, .T. ) ;
#132326 = LINE ( 'NONE', #53289, #44095 ) ;
#132327 = FACE_OUTER_BOUND ( 'NONE', #73023, .T. ) ;
#132328 = DIRECTION ( 'NONE',  ( -0.000000000000000000, -1.000000000000000000, -0.000000000000000000 ) ) ;
#132329 =( LENGTH_UNIT ( ) NAMED_UNIT ( * ) SI_UNIT ( .MILLI., .METRE. ) );
#132330 = AXIS2_PLACEMENT_3D ( 'NONE', #116417, #17784, #39589 ) ;
#132331 = CARTESIAN_POINT ( 'NONE',  ( 62.76626352523144448, 4.472830434245839371, -4.472830434245839371 ) ) ;
#132332 = EDGE_CURVE ( 'NONE', #41149, #101752, #51595, .T. ) ;
#132333 = DIRECTION ( 'NONE',  ( 0.000000000000000000, 0.000000000000000000, 1.000000000000000000 ) ) ;
#132334 = VECTOR ( 'NONE', #100335, 1000.000000000000000 ) ;
#132335 = VECTOR ( 'NONE', #135944, 1000.000000000000000 ) ;
#132336 = DIRECTION ( 'NONE',  ( 0.6830127018922180770, -0.6830127018922204085, -0.2588190451025213501 ) ) ;
#132337 = EDGE_CURVE ( 'NONE', #43580, #32625, #119072, .T. ) ;
#132338 = CARTESIAN_POINT ( 'NONE',  ( 83.39583333333334281, -2.130196079827351596, 7.950000000000043698 ) ) ;
#132339 = VERTEX_POINT ( 'NONE', #19057 ) ;
#132340 = CARTESIAN_POINT ( 'NONE',  ( 153.4000000000000057, 26.96999999999993847, 34.92499999999998295 ) ) ;
#132341 = ORIENTED_EDGE ( 'NONE', *, *, #96509, .T. ) ;
#132342 = VECTOR ( 'NONE', #106571, 1000.000000000000000 ) ;
#132343 = TOROIDAL_SURFACE ( 'NONE', #49020, 2.500000000000000000, 0.5000000000000000000 ) ;
#132344 = VECTOR ( 'NONE', #98430, 1000.000000000000000 ) ;
#132345 = LINE ( 'NONE', #77251, #66282 ) ;
#132347 = SURFACE_STYLE_USAGE ( .BOTH. , #9804 ) ;
#132346 = AXIS2_PLACEMENT_3D ( 'NONE', #93315, #62853, #5570 ) ;
#132348 = VECTOR ( 'NONE', #5584, 1000.000000000000000 ) ;
#132349 = LINE ( 'NONE', #77942, #27609 ) ;
#132350 = DIRECTION ( 'NONE',  ( -0.6830127018922181881, 0.6830127018922202975, -0.2588190451025214056 ) ) ;
#132351 = CARTESIAN_POINT ( 'NONE',  ( 0.2997448713915885632, -27.71228299555206220, 4.000000000000000000 ) ) ;
#132352 = ADVANCED_FACE ( 'NONE', ( #72058 ), #6705, .F. ) ;
#132353 = CARTESIAN_POINT ( 'NONE',  ( -31.49999999999977973, -14.94781430457067906, 5.000000000000000000 ) ) ;
#132354 = CARTESIAN_POINT ( 'NONE',  ( 0.000000000000000000, 0.000000000000000000, 5.000000000000000000 ) ) ;
#132355 = ORIENTED_EDGE ( 'NONE', *, *, #112591, .T. ) ;
#132356 = EDGE_LOOP ( 'NONE', ( #108321, #121329, #104465, #21877, #115758 ) ) ;
#132357 = DIRECTION ( 'NONE',  ( 0.000000000000000000, -1.000000000000000000, 0.000000000000000000 ) ) ;
#132358 = PRESENTATION_STYLE_ASSIGNMENT (( #121431 ) ) ;
#132359 = VECTOR ( 'NONE', #77289, 1000.000000000000000 ) ;
#132360 = LINE ( 'NONE', #122137, #33518 ) ;
#132361 = CARTESIAN_POINT ( 'NONE',  ( 3.250000000000000000, 4.999999999999997335, -7.627214432543508948 ) ) ;
#132362 = CARTESIAN_POINT ( 'NONE',  ( 83.35002705046287019, -5.819803920172572198, -5.819803920172572198 ) ) ;
#132363 = LINE ( 'NONE', #33056, #62587 ) ;
#132364 = DIRECTION ( 'NONE',  ( 0.000000000000000000, -1.000000000000000000, 0.000000000000000000 ) ) ;
#132365 = ORIENTED_EDGE ( 'NONE', *, *, #139313, .T. ) ;
#132366 = CARTESIAN_POINT ( 'NONE',  ( 76.54166666666667140, -3.975000000000002753, 6.884901960086286188 ) ) ;
#132367 = AXIS2_PLACEMENT_3D ( 'NONE', #13271, #124915, #57543 ) ;
#132368 = DIRECTION ( 'NONE',  ( 0.6830127018922180770, -0.6830127018922204085, -0.2588190451025213501 ) ) ;
#132369 = PLANE ( 'NONE',  #124802 ) ;
#132370 = CARTESIAN_POINT ( 'NONE',  ( 48.18398860626899705, 28.73617430169820608, 5.000000000000000000 ) ) ;
#132371 = VERTEX_POINT ( 'NONE', #140145 ) ;
#132372 = LINE ( 'NONE', #11965, #125481 ) ;
#132373 = ORIENTED_EDGE ( 'NONE', *, *, #90718, .T. ) ;
#132374 = AXIS2_PLACEMENT_3D ( 'NONE', #125238, #79654, #101339 ) ;
#132375 = DIRECTION ( 'NONE',  ( -0.000000000000000000, 0.3543493200069153248, 0.9351131265310292928 ) ) ;
#132376 = CARTESIAN_POINT ( 'NONE',  ( 71.60459685856477563, 1.637169565754164946, -6.109999999999999432 ) ) ;
#132377 = AXIS2_PLACEMENT_3D ( 'NONE', #14572, #116738, #115260 ) ;
#132378 =( NAMED_UNIT ( * ) SI_UNIT ( $, .STERADIAN. ) SOLID_ANGLE_UNIT ( ) );
#132379 = EDGE_LOOP ( 'NONE', ( #88458, #102236, #63432 ) ) ;
#132380 = EDGE_CURVE ( 'NONE', #86945, #9815, #62580, .T. ) ;
#132381 = AXIS2_PLACEMENT_3D ( 'NONE', #24616, #81902, #25322 ) ;
#132382 = LINE ( 'NONE', #143217, #120639 ) ;
#132383 = PLANE ( 'NONE',  #142505 ) ;
#132384 = DIRECTION ( 'NONE',  ( 0.000000000000000000, 0.000000000000000000, 1.000000000000000000 ) ) ;
#132385 = LINE ( 'NONE', #54113, #13811 ) ;
#132386 = PLANE ( 'NONE',  #6876 ) ;
#132387 = EDGE_CURVE ( 'NONE', #120179, #128174, #96575, .T. ) ;
#132389 = ORIENTED_EDGE ( 'NONE', *, *, #90278, .T. ) ;
#132388 = LINE ( 'NONE', #66394, #59181 ) ;
#132390 = CARTESIAN_POINT ( 'NONE',  ( -54.29974487139159578, -27.71228299555243879, 4.000000000000000000 ) ) ;
#132391 = DIRECTION ( 'NONE',  ( 0.6830127018922180770, -0.6830127018922204085, -0.2588190451025213501 ) ) ;
#132392 = LINE ( 'NONE', #75151, #111898 ) ;
#132393 = VECTOR ( 'NONE', #120605, 1000.000000000000000 ) ;
#132394 = LINE ( 'NONE', #33087, #83167 ) ;
#132395 = ORIENTED_EDGE ( 'NONE', *, *, #107287, .T. ) ;
#132397 = ORIENTED_EDGE ( 'NONE', *, *, #56790, .F. ) ;
#132396 = ADVANCED_FACE ( 'NONE', ( #64000 ), #95180, .T. ) ;
#132398 = EDGE_CURVE ( 'NONE', #123934, #91948, #139453, .T. ) ;
#132399 = CARTESIAN_POINT ( 'NONE',  ( 68.97959685856477563, 6.109999999999999432, 1.637169565754164280 ) ) ;
#132400 = ORIENTED_EDGE ( 'NONE', *, *, #108414, .F. ) ;
#132401 = EDGE_CURVE ( 'NONE', #132873, #128738, #7443, .T. ) ;
#132403 = CARTESIAN_POINT ( 'NONE',  ( 11.51078643762690490, -27.52281430457047406, 5.000000000000000000 ) ) ;
#132402 = PRODUCT_DEFINITION_SHAPE ( 'NONE', 'NONE',  #110370 ) ;
#132404 = LINE ( 'NONE', #77306, #41099 ) ;
#132405 = EDGE_CURVE ( 'NONE', #10056, #18584, #140815, .T. ) ;
#132406 = VECTOR ( 'NONE', #15347, 1000.000000000000000 ) ;
#132407 = PLANE ( 'NONE',  #94359 ) ;
#132408 =( NAMED_UNIT ( * ) PLANE_ANGLE_UNIT ( ) SI_UNIT ( $, .RADIAN. ) );
#132409 = EDGE_LOOP ( 'NONE', ( #31208, #26861, #133243, #62700 ) ) ;
#132410 = ORIENTED_EDGE ( 'NONE', *, *, #19434, .F. ) ;
#132411 = VECTOR ( 'NONE', #111047, 1000.000000000000000 ) ;
#132412 = EDGE_CURVE ( 'NONE', #32103, #52797, #27792, .T. ) ;
#132413 = DIRECTION ( 'NONE',  ( 0.7071067811865487940, 0.7071067811865463515, -0.000000000000000000 ) ) ;
#132414 = DIRECTION ( 'NONE',  ( -1.000000000000000000, -1.224606353822377258E-16, -0.000000000000000000 ) ) ;
#132415 = EDGE_CURVE ( 'NONE', #43467, #115656, #116233, .T. ) ;
#132416 = ORIENTED_EDGE ( 'NONE', *, *, #48597, .T. ) ;
#132417 = CARTESIAN_POINT ( 'NONE',  ( 0.000000000000000000, -9.500000000000000000, 4.000000000000000000 ) ) ;
#132418 = CONICAL_SURFACE ( 'NONE', #79116, 2.500000000000000444, 0.9599310885968830309 ) ;
#132419 = DIRECTION ( 'NONE',  ( -1.000000000000000000, -1.224606353822377258E-16, -0.000000000000000000 ) ) ;
#132420 = CARTESIAN_POINT ( 'NONE',  ( -28.49999999999979750, 18.05218569542898521, 5.000000000000000000 ) ) ;
#132421 = AXIS2_PLACEMENT_3D ( 'NONE', #116934, #114770, #127840 ) ;
#132422 = ORIENTED_EDGE ( 'NONE', *, *, #44124, .T. ) ;
#132423 = EDGE_CURVE ( 'NONE', #110396, #58396, #5999, .T. ) ;
#132424 = EDGE_CURVE ( 'NONE', #138243, #15180, #142288, .T. ) ;
#132425 = CARTESIAN_POINT ( 'NONE',  ( -5.816011393731002066, 28.73617430169783304, 5.000000000000000000 ) ) ;
#132426 = PLANE ( 'NONE',  #70957 ) ;
#132427 = CARTESIAN_POINT ( 'NONE',  ( -34.92500000000001137, -3.183345613589545486, 4.500000000000000888 ) ) ;
#132428 = CARTESIAN_POINT ( 'NONE',  ( -24.88837638105226446, 9.759292476615614831, 17.35367589129218402 ) ) ;
#132429 = VECTOR ( 'NONE', #4601, 1000.000000000000227 ) ;
#132430 = CARTESIAN_POINT ( 'NONE',  ( 8.999999999999941380, 8.587461875839151659, 4.000000000000000000 ) ) ;
#132431 = EDGE_CURVE ( 'NONE', #105156, #86133, #55266, .T. ) ;
#132432 = CARTESIAN_POINT ( 'NONE',  ( 39.18398860626899705, 28.73617430169814568, 5.000000000000000000 ) ) ;
#132433 = ORIENTED_EDGE ( 'NONE', *, *, #44570, .F. ) ;
#132434 = ORIENTED_EDGE ( 'NONE', *, *, #89335, .T. ) ;
#132435 = CARTESIAN_POINT ( 'NONE',  ( 106.5162635252314658, -4.472830434245838482, 4.472830434245838482 ) ) ;
#132436 = VERTEX_POINT ( 'NONE', #32817 ) ;
#132437 = ORIENTED_EDGE ( 'NONE', *, *, #22006, .T. ) ;
#132438 = CARTESIAN_POINT ( 'NONE',  ( 0.000000000000000000, 0.000000000000000000, 0.000000000000000000 ) ) ;
#132439 = AXIS2_PLACEMENT_3D ( 'NONE', #140829, #98068, #142302 ) ;
#132440 = VECTOR ( 'NONE', #121888, 1000.000000000000000 ) ;
#132441 = DIRECTION ( 'NONE',  ( 0.7071067811865487940, -0.7071067811865463515, 0.000000000000000000 ) ) ;
#132442 = AXIS2_PLACEMENT_3D ( 'NONE', #73084, #117237, #17916 ) ;
#132443 = LINE ( 'NONE', #74471, #118880 ) ;
#132444 = VERTEX_POINT ( 'NONE', #56004 ) ;
#132445 = CARTESIAN_POINT ( 'NONE',  ( 30.18398860626900060, 28.73617430169808173, 5.000000000000000000 ) ) ;
#132446 = DIRECTION ( 'NONE',  ( -0.000000000000000000, -0.000000000000000000, 1.000000000000000000 ) ) ;
#132447 = CARTESIAN_POINT ( 'NONE',  ( 36.29166666666666430, 3.975000000000003642, -6.884901960086285300 ) ) ;
#132449 = DIRECTION ( 'NONE',  ( 1.000000000000000000, 0.000000000000000000, 0.000000000000000000 ) ) ;
#132448 = CARTESIAN_POINT ( 'NONE',  ( 27.32816939922334143, -3.740707523384241728, 4.000000000000000000 ) ) ;
#132450 = EDGE_CURVE ( 'NONE', #73694, #52182, #122642, .T. ) ;
#132451 = DIRECTION ( 'NONE',  ( 0.7071067811865487940, 0.7071067811865463515, 0.000000000000000000 ) ) ;
#132452 = AXIS2_PLACEMENT_3D ( 'NONE', #66380, #122149, #88856 ) ;
#132453 = VECTOR ( 'NONE', #142499, 1000.000000000000000 ) ;
#132454 = AXIS2_PLACEMENT_3D ( 'NONE', #107577, #140914, #142377 ) ;
#132455 = DIRECTION ( 'NONE',  ( 0.000000000000000000, -1.000000000000000000, 0.000000000000000000 ) ) ;
#132456 = ORIENTED_EDGE ( 'NONE', *, *, #120073, .T. ) ;
#132457 = CARTESIAN_POINT ( 'NONE',  ( 87.33333333333332860, -6.884901960086287964, 3.974999999999998312 ) ) ;
#132458 = DIRECTION ( 'NONE',  ( -0.7071067811865486830, -0.7071067811865464625, 0.000000000000000000 ) ) ;
#132459 = ORIENTED_EDGE ( 'NONE', *, *, #62615, .F. ) ;
#132460 = VERTEX_POINT ( 'NONE', #54565 ) ;
#132461 = ORIENTED_EDGE ( 'NONE', *, *, #105393, .T. ) ;
#132462 = CARTESIAN_POINT ( 'NONE',  ( 66.64626352523144703, -4.472830434245840259, 4.472830434245838482 ) ) ;
#132463 = EDGE_LOOP ( 'NONE', ( #88986, #58682, #51873, #53210 ) ) ;
#132464 = EDGE_CURVE ( 'NONE', #28318, #11599, #100200, .T. ) ;
#132465 = FACE_OUTER_BOUND ( 'NONE', #131309, .T. ) ;
#132466 = CARTESIAN_POINT ( 'NONE',  ( -0.1000270504628942014, 4.461849672132297329, -4.461849672132302658 ) ) ;
#132467 = CARTESIAN_POINT ( 'NONE',  ( 102.2295968585647614, -6.110000000000000320, -1.637169565754161393 ) ) ;
#132468 = CARTESIAN_POINT ( 'NONE',  ( -18.79333936457834753, 21.75929247661549937, 4.998822639870701856 ) ) ;
#132469 = EDGE_CURVE ( 'NONE', #139589, #49848, #88619, .T. ) ;
#132470 = LINE ( 'NONE', #54191, #24730 ) ;
#132471 = ORIENTED_EDGE ( 'NONE', *, *, #91305, .F. ) ;
#132472 = CARTESIAN_POINT ( 'NONE',  ( -34.92500000000001137, -22.22500000000000142, 4.000000000000000000 ) ) ;
#132473 = DIRECTION ( 'NONE',  ( 0.6830127018922180770, -0.6830127018922204085, -0.2588190451025213501 ) ) ;
#132474 = CARTESIAN_POINT ( 'NONE',  ( -5.999999999999963585, 19.93112307739198386, 4.000000000000000000 ) ) ;
#132475 = AXIS2_PLACEMENT_3D ( 'NONE', #57725, #23646, #136677 ) ;
#132476 = DIRECTION ( 'NONE',  ( -0.3543493200069162685, -0.000000000000000000, -0.9351131265310288487 ) ) ;
#132477 = ORIENTED_EDGE ( 'NONE', *, *, #97475, .T. ) ;
#132478 = CONICAL_SURFACE ( 'NONE', #83836, 2.500000000000000444, 0.9599310885968830309 ) ;
#132479 = CARTESIAN_POINT ( 'NONE',  ( 30.41161490594810601, 22.22500000000000142, 4.777194822843814137 ) ) ;
#132480 = EDGE_CURVE ( 'NONE', #107805, #305, #45136, .T. ) ;
#132481 = ORIENTED_EDGE ( 'NONE', *, *, #123884, .F. ) ;
#132482 = AXIS2_PLACEMENT_3D ( 'NONE', #81107, #13656, #82519 ) ;
#132483 = ORIENTED_EDGE ( 'NONE', *, *, #44684, .F. ) ;
#132484 = ORIENTED_EDGE ( 'NONE', *, *, #104505, .T. ) ;
#132485 = CARTESIAN_POINT ( 'NONE',  ( 120.9537635252314658, -6.109999999999998543, -3.741295971395162543E-16 ) ) ;
#132486 = VECTOR ( 'NONE', #55321, 1000.000000000000000 ) ;
#132487 = LINE ( 'NONE', #54210, #42326 ) ;
#132488 = EDGE_CURVE ( 'NONE', #68848, #91904, #42975, .T. ) ;
#132489 = DIRECTION ( 'NONE',  ( -0.000000000000000000, 0.000000000000000000, 1.000000000000000000 ) ) ;
#132490 = VERTEX_POINT ( 'NONE', #132848 ) ;
#132491 = CARTESIAN_POINT ( 'NONE',  ( 31.58990935480149176, 9.759292476615621936, 11.28811694763786022 ) ) ;
#132492 = ORIENTED_EDGE ( 'NONE', *, *, #69926, .T. ) ;
#132493 = VECTOR ( 'NONE', #130654, 1000.000000000000000 ) ;
#132494 = CARTESIAN_POINT ( 'NONE',  ( 12.22873647476855119, 5.808823158059031044, -5.808823158059038150 ) ) ;
#132495 = ADVANCED_FACE ( 'NONE', ( #21905 ), #66856, .F. ) ;
#132496 = DIRECTION ( 'NONE',  ( 0.000000000000000000, -1.000000000000000000, 0.000000000000000000 ) ) ;
#132497 = LINE ( 'NONE', #20099, #117784 ) ;
#132498 = CARTESIAN_POINT ( 'NONE',  ( 9.370933818357753964, 3.821174125832445049E-16, 0.000000000000000000 ) ) ;
#132499 = ORIENTED_EDGE ( 'NONE', *, *, #123823, .T. ) ;
#132500 = ORIENTED_EDGE ( 'NONE', *, *, #107412, .F. ) ;
#132501 = CONICAL_SURFACE ( 'NONE', #86104, 2.500000000000000888, 0.9599310885968822538 ) ;
#132502 = ORIENTED_EDGE ( 'NONE', *, *, #80980, .F. ) ;
#132503 = LINE ( 'NONE', #33188, #34781 ) ;
#132504 = CARTESIAN_POINT ( 'NONE',  ( -31.92499999999997584, 22.26999999999998181, -14.71147562388301822 ) ) ;
#132505 = VECTOR ( 'NONE', #73830, 1000.000000000000000 ) ;
#132506 = DIRECTION ( 'NONE',  ( 0.7071067811865487940, -0.7071067811865463515, 0.000000000000000000 ) ) ;
#132507 = CARTESIAN_POINT ( 'NONE',  ( -36.29974487139159578, -27.71228299555231445, 4.000000000000000000 ) ) ;
#132508 = EDGE_CURVE ( 'NONE', #93492, #135550, #77038, .T. ) ;
#132509 = CARTESIAN_POINT ( 'NONE',  ( 32.20710678118632586, -2.240707523384269706, 5.000000000000000000 ) ) ;
#132510 = EDGE_CURVE ( 'NONE', #59483, #91502, #121213, .T. ) ;
#132511 = CARTESIAN_POINT ( 'NONE',  ( 29.99451991528749417, 28.92564299267958816, 4.000000000000000000 ) ) ;
#132512 = PLANE ( 'NONE',  #134384 ) ;
#132513 = CARTESIAN_POINT ( 'NONE',  ( 2.816011393730999401, 28.73617430169785436, 5.000000000000000000 ) ) ;
#132514 = ORIENTED_EDGE ( 'NONE', *, *, #41759, .T. ) ;
#132515 = LINE ( 'NONE', #41907, #14022 ) ;
#132516 = VECTOR ( 'NONE', #29049, 1000.000000000000227 ) ;
#132517 = ORIENTED_EDGE ( 'NONE', *, *, #139990, .F. ) ;
#132518 = DIRECTION ( 'NONE',  ( -0.7071067811865486830, 0.7071067811865464625, 0.000000000000000000 ) ) ;
#132519 = VERTEX_POINT ( 'NONE', #89314 ) ;
#132520 = DIRECTION ( 'NONE',  ( 0.7071067811865487940, 0.7071067811865463515, 0.000000000000000000 ) ) ;
#132522 = ORIENTED_EDGE ( 'NONE', *, *, #123395, .T. ) ;
#132521 = CARTESIAN_POINT ( 'NONE',  ( 152.4000000000000057, 7.919999999999947526, -18.97500000000001918 ) ) ;
#132523 = EDGE_CURVE ( 'NONE', #70498, #84616, #110320, .T. ) ;
#132524 = CARTESIAN_POINT ( 'NONE',  ( -10.82816939922345689, 15.75929247661555799, 4.000000000000000000 ) ) ;
#132525 = ORIENTED_EDGE ( 'NONE', *, *, #121789, .F. ) ;
#132526 = DIRECTION ( 'NONE',  ( 0.7071067811865487940, 0.7071067811865463515, 0.000000000000000000 ) ) ;
#132528 = VERTEX_POINT ( 'NONE', #10306 ) ;
#132527 = VECTOR ( 'NONE', #111635, 999.9999999999998863 ) ;
#132529 = LINE ( 'NONE', #1918, #55962 ) ;
#132530 = ORIENTED_EDGE ( 'NONE', *, *, #85365, .T. ) ;
#132531 = CARTESIAN_POINT ( 'NONE',  ( -29.09565676934979450, 22.22500000000000142, 2.791043937613590931 ) ) ;
#132532 = CARTESIAN_POINT ( 'NONE',  ( 113.2458603837962272, 3.974999999999996980, 6.884901960086287964 ) ) ;
#132533 = CARTESIAN_POINT ( 'NONE',  ( -14.20710678118644310, 15.75929247661555443, 5.000000000000000000 ) ) ;
#132534 = DIRECTION ( 'NONE',  ( 0.7071067811865486830, -0.7071067811865464625, -0.000000000000000000 ) ) ;
#132535 = LINE ( 'NONE', #35353, #123171 ) ;
#132536 = CARTESIAN_POINT ( 'NONE',  ( -5.999999999999956479, 17.96639925780208458, 5.000000000000000000 ) ) ;
#132537 = DIRECTION ( 'NONE',  ( 0.6830127018922181881, 0.6830127018922202975, -0.2588190451025214056 ) ) ;
#132538 = CARTESIAN_POINT ( 'NONE',  ( 15.89583333333333393, 1.633150327867687324, -6.094999999999991758 ) ) ;
#132539 = CARTESIAN_POINT ( 'NONE',  ( 16.45790314143522082, 6.871911579029515771, 3.967499999999989146 ) ) ;
#132540 = VECTOR ( 'NONE', #4939, 1000.000000000000000 ) ;
#132541 = VECTOR ( 'NONE', #36531, 1000.000000000000000 ) ;
#132543 = LINE ( 'NONE', #10684, #95287 ) ;
#132542 = VECTOR ( 'NONE', #51438, 1000.000000000000000 ) ;
#132544 = CARTESIAN_POINT ( 'NONE',  ( -20.67183060077632817, -12.74070752338415247, 4.000000000000000000 ) ) ;
#132545 = ORIENTED_EDGE ( 'NONE', *, *, #64471, .T. ) ;
#132546 = ORIENTED_EDGE ( 'NONE', *, *, #105684, .F. ) ;
#132547 = AXIS2_PLACEMENT_3D ( 'NONE', #138871, #70077, #37405 ) ;
#132548 = LINE ( 'NONE', #111456, #334 ) ;
#132549 = EDGE_LOOP ( 'NONE', ( #111929, #3942, #117959, #133963 ) ) ;
#132550 = FACE_OUTER_BOUND ( 'NONE', #111057, .T. ) ;
#132551 = DIRECTION ( 'NONE',  ( 0.3543493200069163240, 0.000000000000000000, -0.9351131265310288487 ) ) ;
#132552 = AXIS2_PLACEMENT_3D ( 'NONE', #54620, #64058, #98804 ) ;
#132553 = DIRECTION ( 'NONE',  ( -0.7071067811865487940, 0.7071067811865463515, -0.000000000000000000 ) ) ;
#132554 = CARTESIAN_POINT ( 'NONE',  ( 128.6723146205780779, -49.13871568196854867, -40.16438383193010964 ) ) ;
#132555 = VERTEX_POINT ( 'NONE', #76308 ) ;
#132556 = PLANE ( 'NONE',  #126207 ) ;
#132557 = DIRECTION ( 'NONE',  ( 3.973028287378889149E-16, -1.000000000000000000, 0.000000000000000000 ) ) ;
#132558 = DIRECTION ( 'NONE',  ( -0.5735764363510507113, 0.8191520442889885789, 1.003171929053520926E-16 ) ) ;
#132559 = CARTESIAN_POINT ( 'NONE',  ( -5.999999999999952927, 11.96639925780214320, 5.000000000000000000 ) ) ;
#132560 = DIRECTION ( 'NONE',  ( 0.000000000000000000, -1.000000000000000000, 0.000000000000000000 ) ) ;
#132562 = EDGE_LOOP ( 'NONE', ( #143278, #92131, #20059, #140942 ) ) ;
#132561 = DIRECTION ( 'NONE',  ( 0.6830127018922181881, 0.6830127018922202975, -0.2588190451025214056 ) ) ;
#132563 = CARTESIAN_POINT ( 'NONE',  ( 34.92499999999998295, -2.143876922607573121, 4.000000000000000000 ) ) ;
#132564 = FACE_OUTER_BOUND ( 'NONE', #97793, .T. ) ;
#132565 = CARTESIAN_POINT ( 'NONE',  ( -12.32816939922344091, 5.259292476615662792, 4.000000000000000000 ) ) ;
#132566 = ORIENTED_EDGE ( 'NONE', *, *, #134580, .T. ) ;
#132567 = VERTEX_POINT ( 'NONE', #34225 ) ;
#132568 = VERTEX_POINT ( 'NONE', #32078 ) ;
#132569 = ADVANCED_FACE ( 'NONE', ( #121913 ), #56733, .F. ) ;
#132570 = CARTESIAN_POINT ( 'NONE',  ( 96.97959685856478984, 6.109999999999999432, 1.637169565754164280 ) ) ;
#132571 = ORIENTED_EDGE ( 'NONE', *, *, #54493, .T. ) ;
#132572 = EDGE_CURVE ( 'NONE', #5121, #18530, #100893, .T. ) ;
#132573 = CARTESIAN_POINT ( 'NONE',  ( 27.29974487139158512, -27.71228299555225405, 4.000000000000000000 ) ) ;
#132574 = EDGE_CURVE ( 'NONE', #104026, #65260, #115, .T. ) ;
#132575 = DIRECTION ( 'NONE',  ( 0.000000000000000000, -1.000000000000000000, 0.000000000000000000 ) ) ;
#132576 = ORIENTED_EDGE ( 'NONE', *, *, #66331, .F. ) ;
#132577 = EDGE_CURVE ( 'NONE', #60780, #97230, #98743, .T. ) ;
#132578 = LINE ( 'NONE', #10036, #93033 ) ;
#132579 = CARTESIAN_POINT ( 'NONE',  ( 49.27083333333333570, -7.949999999999998401, -2.130196079827426203 ) ) ;
#132580 = MECHANICAL_DESIGN_GEOMETRIC_PRESENTATION_REPRESENTATION (  '', ( #51527 ), #63131 ) ;
#132581 = CARTESIAN_POINT ( 'NONE',  ( 82.01626352523142316, -4.472830434245839371, 4.472830434245839371 ) ) ;
#132582 = ORIENTED_EDGE ( 'NONE', *, *, #45723, .T. ) ;
#132583 = CARTESIAN_POINT ( 'NONE',  ( -26.99999999999981171, -8.731860332648864187, -2.120594902707600315 ) ) ;
#132584 = FACE_OUTER_BOUND ( 'NONE', #27886, .T. ) ;
#132585 = VECTOR ( 'NONE', #87594, 999.9999999999998863 ) ;
#132586 = VERTEX_POINT ( 'NONE', #9582 ) ;
#132587 = VERTEX_POINT ( 'NONE', #53855 ) ;
#132588 = EDGE_CURVE ( 'NONE', #95615, #136985, #44695, .T. ) ;
#132589 = ORIENTED_EDGE ( 'NONE', *, *, #137200, .F. ) ;
#132590 = CARTESIAN_POINT ( 'NONE',  ( 0.000000000000000000, 0.000000000000000000, 5.000000000000000000 ) ) ;
#132591 = EDGE_CURVE ( 'NONE', #119532, #67945, #101603, .T. ) ;
#132592 = LINE ( 'NONE', #142716, #124231 ) ;
#132593 = CARTESIAN_POINT ( 'NONE',  ( 57.29974487139158157, -27.71228299555246011, 4.000000000000000000 ) ) ;
#132594 = DIRECTION ( 'NONE',  ( 0.7071067811865487940, 0.7071067811865463515, 0.000000000000000000 ) ) ;
#132595 = EDGE_CURVE ( 'NONE', #73071, #74995, #90009, .T. ) ;
#132596 = LINE ( 'NONE', #33291, #16289 ) ;
#132597 = FACE_OUTER_BOUND ( 'NONE', #97254, .T. ) ;
#132598 = VERTEX_POINT ( 'NONE', #2261 ) ;
#132599 = EDGE_LOOP ( 'NONE', ( #110927, #131149, #119699, #113835 ) ) ;
#132600 = LINE ( 'NONE', #77499, #24811 ) ;
#132601 = ORIENTED_EDGE ( 'NONE', *, *, #91557, .F. ) ;
#132602 = ORIENTED_EDGE ( 'NONE', *, *, #126743, .F. ) ;
#132603 = AXIS2_PLACEMENT_3D ( 'NONE', #51079, #15537, #50363 ) ;
#132604 = EDGE_CURVE ( 'NONE', #138081, #99040, #82045, .T. ) ;
#132605 = VECTOR ( 'NONE', #94678, 999.9999999999998863 ) ;
#132606 =( BOUNDED_CURVE ( )  B_SPLINE_CURVE ( 3, ( #107926, #8595, #89768, #44149 ),
 .UNSPECIFIED., .F., .F. ) 
 B_SPLINE_CURVE_WITH_KNOTS ( ( 4, 4 ),
 ( 0.9743798061614650230, 1.027697802963069229 ),
 .UNSPECIFIED. ) 
 CURVE ( )  GEOMETRIC_REPRESENTATION_ITEM ( )  RATIONAL_B_SPLINE_CURVE ( ( 1.000000000000000000, 0.9997631132982454094, 0.9997631132982454094, 1.000000000000000000 ) ) 
 REPRESENTATION_ITEM ( '' )  );
#132607 = LINE ( 'NONE', #33302, #24217 ) ;
#132608 = ORIENTED_EDGE ( 'NONE', *, *, #130097, .T. ) ;
#132609 = DIRECTION ( 'NONE',  ( -0.6830127018922180770, -0.6830127018922204085, -0.2588190451025213501 ) ) ;
#132610 = DIRECTION ( 'NONE',  ( 1.000000000000000000, 0.000000000000000000, 0.000000000000000000 ) ) ;
#132611 = PLANE ( 'NONE',  #108042 ) ;
#132612 = EDGE_CURVE ( 'NONE', #106069, #123748, #14607, .T. ) ;
#132613 = DIRECTION ( 'NONE',  ( 0.7071067811865487940, -0.7071067811865463515, 0.000000000000000000 ) ) ;
#132614 = VECTOR ( 'NONE', #38237, 1000.000000000000000 ) ;
#132615 =( BOUNDED_CURVE ( )  B_SPLINE_CURVE ( 3, ( #66640, #109414, #86956, #1341 ),
 .UNSPECIFIED., .F., .T. ) 
 B_SPLINE_CURVE_WITH_KNOTS ( ( 4, 4 ),
 ( 5.043186909253412509, 5.074607125596337198 ),
 .UNSPECIFIED. ) 
 CURVE ( )  GEOMETRIC_REPRESENTATION_ITEM ( )  RATIONAL_B_SPLINE_CURVE ( ( 1.000000000000000000, 0.9999177325257868620, 0.9999177325257868620, 1.000000000000000000 ) ) 
 REPRESENTATION_ITEM ( '' )  );
#132616 = CARTESIAN_POINT ( 'NONE',  ( 118.2500000000000000, -9.735942053221458872E-16, 7.950000000000000178 ) ) ;
#132617 = ORIENTED_EDGE ( 'NONE', *, *, #108560, .F. ) ;
#132618 = LINE ( 'NONE', #78942, #2390 ) ;
#132619 = ORIENTED_EDGE ( 'NONE', *, *, #23764, .F. ) ;
#132620 = DIRECTION ( 'NONE',  ( 0.000000000000000000, -1.000000000000000000, 0.000000000000000000 ) ) ;
#132621 = EDGE_LOOP ( 'NONE', ( #82880, #40409, #110388, #61163 ) ) ;
#132622 = CARTESIAN_POINT ( 'NONE',  ( 116.7458603837962272, 3.974999999999996980, 6.884901960086287964 ) ) ;
#132623 = ORIENTED_EDGE ( 'NONE', *, *, #38759, .T. ) ;
#132624 = LINE ( 'NONE', #42747, #22697 ) ;
#132625 = ORIENTED_EDGE ( 'NONE', *, *, #131724, .T. ) ;
#132626 = VERTEX_POINT ( 'NONE', #124792 ) ;
#132627 = AXIS2_PLACEMENT_3D ( 'NONE', #113236, #2312, #123453 ) ;
#132628 = ORIENTED_EDGE ( 'NONE', *, *, #24175, .T. ) ;
#132629 = EDGE_CURVE ( 'NONE', #41252, #135320, #58162, .T. ) ;
#132630 = CARTESIAN_POINT ( 'NONE',  ( 0.1839886062690032631, 28.73617430169787568, 5.000000000000000000 ) ) ;
#132631 = CARTESIAN_POINT ( 'NONE',  ( 30.79289321881324781, -2.240707523384264377, 5.000000000000000000 ) ) ;
#132632 = DIRECTION ( 'NONE',  ( -0.000000000000000000, -0.3543493200069153248, -0.9351131265310292928 ) ) ;
#132633 = FACE_OUTER_BOUND ( 'NONE', #91445, .T. ) ;
#132634 = CARTESIAN_POINT ( 'NONE',  ( 15.00548008471250228, 28.92564299267927552, 4.000000000000000000 ) ) ;
#132635 = EDGE_CURVE ( 'NONE', #89630, #113088, #81318, .T. ) ;
#132636 = DIRECTION ( 'NONE',  ( -0.000000000000000000, 0.000000000000000000, 1.000000000000000000 ) ) ;
#132637 = CARTESIAN_POINT ( 'NONE',  ( -12.20000000000000284, -39.92999999999999261, -40.00000000000000000 ) ) ;
#132638 = VECTOR ( 'NONE', #134256, 1000.000000000000000 ) ;
#132639 = AXIS2_PLACEMENT_3D ( 'NONE', #132590, #33284, #45580 ) ;
#132640 = AXIS2_PLACEMENT_3D ( 'NONE', #101, #42965, #45822 ) ;
#132641 = VECTOR ( 'NONE', #15408, 1000.000000000000000 ) ;
#132642 = DIRECTION ( 'NONE',  ( 0.000000000000000000, 0.000000000000000000, -1.000000000000000000 ) ) ;
#132643 = LINE ( 'NONE', #22378, #113067 ) ;
#132644 = DIRECTION ( 'NONE',  ( -0.7071067811865486830, -0.7071067811865464625, 0.000000000000000000 ) ) ;
#132645 = EDGE_CURVE ( 'NONE', #64888, #28108, #113186, .T. ) ;
#132646 = ORIENTED_EDGE ( 'NONE', *, *, #40430, .F. ) ;
#132647 = EDGE_LOOP ( 'NONE', ( #96075, #58073, #141472, #41564, #6555, #27272 ) ) ;
#132648 = AXIS2_PLACEMENT_3D ( 'NONE', #34370, #55415, #31514 ) ;
#132649 = EDGE_LOOP ( 'NONE', ( #134094, #129126, #99681, #8552 ) ) ;
#132650 = AXIS2_PLACEMENT_3D ( 'NONE', #44086, #117502, #105223 ) ;
#132651 = PRESENTATION_LAYER_ASSIGNMENT (  '', '', ( #26033 ) ) ;
#132652 = CARTESIAN_POINT ( 'NONE',  ( 15.50060776059232559, 22.22500000000000142, -14.10814778869267805 ) ) ;
#132653 = ORIENTED_EDGE ( 'NONE', *, *, #31680, .T. ) ;
#132654 = ORIENTED_EDGE ( 'NONE', *, *, #132325, .T. ) ;
#132655 = CARTESIAN_POINT ( 'NONE',  ( -14.67183060077636547, 14.25929247661557042, 4.000000000000000000 ) ) ;
#132656 = CARTESIAN_POINT ( 'NONE',  ( -6.792893218813409462, 9.759292476615618384, 5.000000000000000000 ) ) ;
#132657 = ADVANCED_FACE ( 'NONE', ( #60279 ), #69738, .F. ) ;
#132658 = CARTESIAN_POINT ( 'NONE',  ( -16.17183060077635659, 21.75929247661549581, 4.000000000000000000 ) ) ;
#132659 = CARTESIAN_POINT ( 'NONE',  ( -33.18398860626899705, 28.73617430169810305, 5.000000000000000000 ) ) ;
#132660 = ORIENTED_EDGE ( 'NONE', *, *, #126330, .F. ) ;
#132661 = CARTESIAN_POINT ( 'NONE',  ( 25.49999999999982947, 15.05218569542901896, 5.000000000000000000 ) ) ;
#132662 = ORIENTED_EDGE ( 'NONE', *, *, #104362, .F. ) ;
#132663 = CARTESIAN_POINT ( 'NONE',  ( -11.81601139373100651, 28.73617430169779041, 5.000000000000000000 ) ) ;
#132664 = CIRCLE ( 'NONE', #19205, 0.5000000000000004441 ) ;
#132665 = CARTESIAN_POINT ( 'NONE',  ( 22.67123647476855552, 0.000000000000000000, 7.934999999999990727 ) ) ;
#132666 = ORIENTED_EDGE ( 'NONE', *, *, #111409, .T. ) ;
#132667 = CARTESIAN_POINT ( 'NONE',  ( 85.07876352523143737, -7.482591942790327058E-16, 6.109999999999999432 ) ) ;
#132668 = CARTESIAN_POINT ( 'NONE',  ( 6.403482346239627532, -9.299335578761299459, 1.960683619075200390 ) ) ;
#132669 = DIRECTION ( 'NONE',  ( -0.7071067811865486830, -0.7071067811865464625, 0.000000000000000000 ) ) ;
#132670 = ADVANCED_FACE ( 'NONE', ( #58888 ), #3686, .T. ) ;
#132671 = ORIENTED_EDGE ( 'NONE', *, *, #19218, .T. ) ;
#132672 = CARTESIAN_POINT ( 'NONE',  ( -4.499999999999968914, 10.94296225409026668, -9.576120664313268804 ) ) ;
#132673 = ORIENTED_EDGE ( 'NONE', *, *, #42022, .F. ) ;
#132674 = ORIENTED_EDGE ( 'NONE', *, *, #97777, .T. ) ;
#132675 = LINE ( 'NONE', #77566, #114359 ) ;
#132676 = CARTESIAN_POINT ( 'NONE',  ( 34.17183060077623225, 15.75929247661556687, 4.000000000000000000 ) ) ;
#132677 = CARTESIAN_POINT ( 'NONE',  ( 16.45742106731621135, 0.9613713492673626737, -33.49048331797055766 ) ) ;
#132678 = DIRECTION ( 'NONE',  ( 0.6830127018922180770, -0.6830127018922204085, -0.2588190451025213501 ) ) ;
#132679 = CARTESIAN_POINT ( 'NONE',  ( 34.82816939922328459, -14.24070752338414714, 4.000000000000000000 ) ) ;
#132680 = VERTEX_POINT ( 'NONE', #47295 ) ;
#132681 = AXIS2_PLACEMENT_3D ( 'NONE', #7030, #18637, #105651 ) ;
#132682 =( NAMED_UNIT ( * ) SI_UNIT ( $, .STERADIAN. ) SOLID_ANGLE_UNIT ( ) );
#132683 = EDGE_CURVE ( 'NONE', #10836, #120276, #71150, .T. ) ;
#132684 = VECTOR ( 'NONE', #143145, 1000.000000000000227 ) ;
#132685 = DIRECTION ( 'NONE',  ( -1.000000000000000000, 0.000000000000000000, 0.000000000000000000 ) ) ;
#132686 = DIRECTION ( 'NONE',  ( 1.000000000000000000, 0.000000000000000000, 0.000000000000000000 ) ) ;
#132687 = ORIENTED_EDGE ( 'NONE', *, *, #133227, .F. ) ;
#132688 = DIRECTION ( 'NONE',  ( -0.000000000000000000, -0.000000000000000000, 1.000000000000000000 ) ) ;
#132689 = AXIS2_PLACEMENT_3D ( 'NONE', #35392, #1956, #15010 ) ;
#132690 = LINE ( 'NONE', #53680, #58670 ) ;
#132691 = ORIENTED_EDGE ( 'NONE', *, *, #134931, .F. ) ;
#132692 = EDGE_CURVE ( 'NONE', #57534, #124891, #3006, .T. ) ;
#132694 = ORIENTED_EDGE ( 'NONE', *, *, #47193, .T. ) ;
#132693 = CARTESIAN_POINT ( 'NONE',  ( -21.29974487139158512, -27.71228299555221142, 4.000000000000000000 ) ) ;
#132695 = EDGE_LOOP ( 'NONE', ( #65898, #45012, #67786, #116799, #120382, #125514 ) ) ;
#132696 = EDGE_CURVE ( 'NONE', #112107, #50934, #92145, .T. ) ;
#132697 = LINE ( 'NONE', #77585, #21522 ) ;
#132698 = CARTESIAN_POINT ( 'NONE',  ( -5.292986735706916690, -21.74070752338406010, 4.999753212805220670 ) ) ;
#132699 = VERTEX_POINT ( 'NONE', #59566 ) ;
#132700 = CARTESIAN_POINT ( 'NONE',  ( 25.39999999999999858, -1.600000000000086020, -34.92499999999998295 ) ) ;
#132701 = VECTOR ( 'NONE', #113751, 1000.000000000000227 ) ;
#132702 = DIRECTION ( 'NONE',  ( 0.6830127018922181881, 0.6830127018922202975, -0.2588190451025214056 ) ) ;
#132703 = DIRECTION ( 'NONE',  ( -0.7071067811865486830, -0.7071067811865464625, 0.000000000000000000 ) ) ;
#132704 = CARTESIAN_POINT ( 'NONE',  ( -18.18398860626898994, 28.73617430169800002, 5.000000000000000000 ) ) ;
#132705 = LINE ( 'NONE', #57278, #81585 ) ;
#132706 = AXIS2_PLACEMENT_3D ( 'NONE', #123689, #55565, #78035 ) ;
#132707 = CARTESIAN_POINT ( 'NONE',  ( 54.18398860626899705, 28.73617430169825226, 5.000000000000000000 ) ) ;
#132708 = CARTESIAN_POINT ( 'NONE',  ( 34.17183060077623225, -11.24070752338416490, 4.000000000000000000 ) ) ;
#132709 = CARTESIAN_POINT ( 'NONE',  ( 16.31206980810189222, 7.934999999999993392, 2.126176841940951689 ) ) ;
#132710 = DIRECTION ( 'NONE',  ( -0.7071067811865487940, 0.7071067811865463515, 0.000000000000000000 ) ) ;
#132711 = AXIS2_PLACEMENT_3D ( 'NONE', #79431, #123628, #80123 ) ;
#132712 = DIRECTION ( 'NONE',  ( -0.7071067811865486830, -0.7071067811865464625, -0.000000000000000000 ) ) ;
#132713 = CARTESIAN_POINT ( 'NONE',  ( -1.889826771117871784, -22.22500000000000142, 4.785647885939354751 ) ) ;
#132714 = PLANE ( 'NONE',  #10623 ) ;
#132715 = VERTEX_POINT ( 'NONE', #137106 ) ;
#132716 = EDGE_CURVE ( 'NONE', #15253, #36181, #26206, .T. ) ;
#132717 = ORIENTED_EDGE ( 'NONE', *, *, #132380, .F. ) ;
#132718 = CARTESIAN_POINT ( 'NONE',  ( 100.1666666666666714, 6.884901960086285300, 3.975000000000003642 ) ) ;
#132719 = ORIENTED_EDGE ( 'NONE', *, *, #107033, .F. ) ;
#132720 = ORIENTED_EDGE ( 'NONE', *, *, #44794, .T. ) ;
#132721 = ORIENTED_EDGE ( 'NONE', *, *, #24336, .F. ) ;
#132722 = LINE ( 'NONE', #58014, #122018 ) ;
#132723 = DIRECTION ( 'NONE',  ( -0.000000000000000000, -0.000000000000000000, 1.000000000000000000 ) ) ;
#132724 = VECTOR ( 'NONE', #136710, 1000.000000000000227 ) ;
#132725 = ORIENTED_EDGE ( 'NONE', *, *, #117639, .T. ) ;
#132726 = LINE ( 'NONE', #121785, #27823 ) ;
#132727 = CARTESIAN_POINT ( 'NONE',  ( 10.15640092694706453, 3.821174125832445049E-16, 0.000000000000000000 ) ) ;
#132728 = FACE_OUTER_BOUND ( 'NONE', #84154, .T. ) ;
#132729 = DIRECTION ( 'NONE',  ( -0.6830127018922181881, 0.6830127018922202975, -0.2588190451025214056 ) ) ;
#132730 = VERTEX_POINT ( 'NONE', #114614 ) ;
#132731 = CARTESIAN_POINT ( 'NONE',  ( 16.15220243791050336, 1.822765899684732238, -33.22366253240541312 ) ) ;
#132732 = LINE ( 'NONE', #100780, #25934 ) ;
#132733 = DIRECTION ( 'NONE',  ( 0.3543493200069163240, -0.000000000000000000, 0.9351131265310288487 ) ) ;
#132734 = CARTESIAN_POINT ( 'NONE',  ( 1.199999999999999956, -0.5999999999999993117, -4.543283425070392845 ) ) ;
#132735 = FACE_OUTER_BOUND ( 'NONE', #71193, .T. ) ;
#132736 = DIRECTION ( 'NONE',  ( -0.7071067811865486830, 0.7071067811865464625, 0.000000000000000000 ) ) ;
#132737 = ORIENTED_EDGE ( 'NONE', *, *, #59381, .F. ) ;
#132738 = ORIENTED_EDGE ( 'NONE', *, *, #44198, .T. ) ;
#132739 = EDGE_CURVE ( 'NONE', #47092, #140803, #79914, .T. ) ;
#132740 = CARTESIAN_POINT ( 'NONE',  ( 120.3129301918980758, -1.637169565754159617, -6.110000000000001208 ) ) ;
#132741 = VERTEX_POINT ( 'NONE', #92871 ) ;
#132742 = EDGE_CURVE ( 'NONE', #79780, #50223, #69008, .T. ) ;
#132743 = CARTESIAN_POINT ( 'NONE',  ( -34.92500000000001137, -16.48753812416032360, 4.000000000000000000 ) ) ;
#132744 = AXIS2_PLACEMENT_3D ( 'NONE', #114449, #48487, #89840 ) ;
#132745 = CARTESIAN_POINT ( 'NONE',  ( 17.99451991528748351, 28.92564299267950645, 4.000000000000000000 ) ) ;
#132746 = EDGE_CURVE ( 'NONE', #139884, #69443, #104456, .T. ) ;
#132747 = EDGE_CURVE ( 'NONE', #136709, #19349, #36369, .T. ) ;
#132748 = DIRECTION ( 'NONE',  ( -0.000000000000000000, -0.3543493200069152693, 0.9351131265310292928 ) ) ;
#132750 = VECTOR ( 'NONE', #49371, 1000.000000000000227 ) ;
#132749 = CARTESIAN_POINT ( 'NONE',  ( 20.67906569311139009, 4.202752102959690472E-16, 0.000000000000000000 ) ) ;
#132751 = CARTESIAN_POINT ( 'NONE',  ( 116.5787635252314516, -7.482591942790325086E-16, 6.109999999999998543 ) ) ;
#132752 = ORIENTED_EDGE ( 'NONE', *, *, #64279, .F. ) ;
#132753 = VERTEX_POINT ( 'NONE', #134991 ) ;
#132754 = VECTOR ( 'NONE', #78521, 1000.000000000000000 ) ;
#132755 = DIRECTION ( 'NONE',  ( -0.7071067811865486830, -0.7071067811865464625, 0.000000000000000000 ) ) ;
#132756 = CARTESIAN_POINT ( 'NONE',  ( 98.27083333333332860, -7.949999999999998401, -2.130196079827426203 ) ) ;
#132757 = CIRCLE ( 'NONE', #70264, 2.000000000000001776 ) ;
#132758 = ORIENTED_EDGE ( 'NONE', *, *, #11227, .F. ) ;
#132759 = ORIENTED_EDGE ( 'NONE', *, *, #8960, .T. ) ;
#132761 = EDGE_CURVE ( 'NONE', #77764, #8795, #80597, .T. ) ;
#132760 = CARTESIAN_POINT ( 'NONE',  ( 39.08376352523143282, -6.110000000000001208, -3.741295971395164515E-16 ) ) ;
#132762 = VERTEX_POINT ( 'NONE', #39222 ) ;
#132763 = CARTESIAN_POINT ( 'NONE',  ( 9.183988606268997046, 28.73617430169793607, 5.000000000000000000 ) ) ;
#132764 = EDGE_CURVE ( 'NONE', #82496, #38440, #50104, .T. ) ;
#132765 = CARTESIAN_POINT ( 'NONE',  ( 34.42499999999998295, -22.22500000000000142, 4.500000000000000888 ) ) ;
#132766 = VECTOR ( 'NONE', #63161, 1000.000000000000227 ) ;
#132767 = EDGE_CURVE ( 'NONE', #69819, #100020, #52225, .T. ) ;
#132768 = CARTESIAN_POINT ( 'NONE',  ( 30.39126352523144448, -4.472830434245839371, -4.472830434245839371 ) ) ;
#132769 = EDGE_LOOP ( 'NONE', ( #55858, #44402, #17288 ) ) ;
#132770 = DIRECTION ( 'NONE',  ( 0.6830127018922180770, -0.6830127018922204085, -0.2588190451025213501 ) ) ;
#132771 = EDGE_LOOP ( 'NONE', ( #17196, #63019, #42810, #115216 ) ) ;
#132772 = ORIENTED_EDGE ( 'NONE', *, *, #77784, .F. ) ;
#132773 = EDGE_CURVE ( 'NONE', #15499, #77121, #105867, .T. ) ;
#132774 = ORIENTED_EDGE ( 'NONE', *, *, #47014, .T. ) ;
#132775 = AXIS2_PLACEMENT_3D ( 'NONE', #34378, #90918, #69160 ) ;
#132776 = DIRECTION ( 'NONE',  ( -1.000000000000000000, 0.000000000000000000, 0.000000000000000000 ) ) ;
#132777 = LINE ( 'NONE', #55916, #92780 ) ;
#132778 = VERTEX_POINT ( 'NONE', #62413 ) ;
#132779 = AXIS2_PLACEMENT_3D ( 'NONE', #137751, #91396, #70388 ) ;
#132780 = CARTESIAN_POINT ( 'NONE',  ( -29.20710678118634007, -2.240707523384255939, 5.000000000000000000 ) ) ;
#132781 = EDGE_CURVE ( 'NONE', #94514, #88116, #72610, .T. ) ;
#132782 = DIRECTION ( 'NONE',  ( -0.000000000000000000, 0.3543493200069153248, 0.9351131265310292928 ) ) ;
#132783 = VECTOR ( 'NONE', #34394, 1000.000000000000227 ) ;
#132784 = FACE_BOUND ( 'NONE', #50131, .T. ) ;
#132785 = ORIENTED_EDGE ( 'NONE', *, *, #82385, .F. ) ;
#132786 = LINE ( 'NONE', #122570, #17907 ) ;
#132787 = DIRECTION ( 'NONE',  ( 0.7071067811865487940, 0.7071067811865463515, -0.000000000000000000 ) ) ;
#132788 = CARTESIAN_POINT ( 'NONE',  ( -21.48921356237309155, -27.52281430457070499, 5.000000000000000000 ) ) ;
#132789 = VERTEX_POINT ( 'NONE', #140650 ) ;
#132790 = ADVANCED_FACE ( 'NONE', ( #74726 ), #63839, .F. ) ;
#132791 = DIRECTION ( 'NONE',  ( 1.000000000000000000, 0.000000000000000000, 0.000000000000000000 ) ) ;
#132792 = VERTEX_POINT ( 'NONE', #96411 ) ;
#132793 = EDGE_CURVE ( 'NONE', #67347, #115536, #29052, .T. ) ;
#132794 = ORIENTED_EDGE ( 'NONE', *, *, #67966, .T. ) ;
#132795 =( BOUNDED_CURVE ( )  B_SPLINE_CURVE ( 3, ( #19446, #22269, #30325, #63695 ),
 .UNSPECIFIED., .F., .T. ) 
 B_SPLINE_CURVE_WITH_KNOTS ( ( 4, 4 ),
 ( 2.001653308786165208, 3.503810798801451742 ),
 .UNSPECIFIED. ) 
 CURVE ( )  GEOMETRIC_REPRESENTATION_ITEM ( )  RATIONAL_B_SPLINE_CURVE ( ( 1.000000000000000000, 0.8206354192515228352, 0.8206354192515228352, 1.000000000000000000 ) ) 
 REPRESENTATION_ITEM ( '' )  );
#132796 = ORIENTED_EDGE ( 'NONE', *, *, #80182, .T. ) ;
#132797 = VECTOR ( 'NONE', #21330, 1000.000000000000000 ) ;
#132798 = EDGE_CURVE ( 'NONE', #5701, #93024, #114175, .T. ) ;
#132799 = CARTESIAN_POINT ( 'NONE',  ( 50.51626352523143737, -4.472830434245838482, 4.472830434245838482 ) ) ;
#132801 = ORIENTED_EDGE ( 'NONE', *, *, #132415, .T. ) ;
#132800 = VECTOR ( 'NONE', #49030, 1000.000000000000000 ) ;
#132802 = AXIS2_PLACEMENT_3D ( 'NONE', #48541, #136978, #16607 ) ;
#132803 = LINE ( 'NONE', #142924, #37136 ) ;
#132804 = DIRECTION ( 'NONE',  ( -0.6830127018922180770, -0.6830127018922204085, -0.2588190451025213501 ) ) ;
#132805 = PLANE ( 'NONE',  #125150 ) ;
#132806 = ORIENTED_EDGE ( 'NONE', *, *, #86213, .T. ) ;
#132807 = DIRECTION ( 'NONE',  ( 1.000000000000000000, 0.000000000000000000, 0.000000000000000000 ) ) ;
#132808 = LINE ( 'NONE', #33489, #119905 ) ;
#132809 = CARTESIAN_POINT ( 'NONE',  ( 152.4000000000000057, 7.919999999999947526, 21.67769999999997310 ) ) ;
#132810 = FACE_OUTER_BOUND ( 'NONE', #79693, .T. ) ;
#132811 = DIRECTION ( 'NONE',  ( -0.6830127018922181881, 0.6830127018922202975, -0.2588190451025214056 ) ) ;
#132812 = DIRECTION ( 'NONE',  ( 1.000000000000000000, 0.000000000000000000, 0.000000000000000000 ) ) ;
#132813 = VERTEX_POINT ( 'NONE', #117458 ) ;
#132815 = VERTEX_POINT ( 'NONE', #137831 ) ;
#132814 = VECTOR ( 'NONE', #128015, 1000.000000000000000 ) ;
#132816 = VERTEX_POINT ( 'NONE', #63141 ) ;
#132817 = DIRECTION ( 'NONE',  ( 0.7071067811865487940, 0.7071067811865463515, 0.000000000000000000 ) ) ;
#132818 = FACE_OUTER_BOUND ( 'NONE', #108038, .T. ) ;
#132819 = ORIENTED_EDGE ( 'NONE', *, *, #138540, .T. ) ;
#132820 = EDGE_LOOP ( 'NONE', ( #123343, #9136, #68282, #84674 ) ) ;
#132821 = CARTESIAN_POINT ( 'NONE',  ( -9.183988606268997046, 28.73617430169793607, 5.000000000000000000 ) ) ;
#132822 = DIRECTION ( 'NONE',  ( -0.000000000000000000, 0.3543493200069153248, 0.9351131265310292928 ) ) ;
#132823 = DIRECTION ( 'NONE',  ( -0.7071067811865486830, -0.7071067811865464625, 0.000000000000000000 ) ) ;
#132824 = VECTOR ( 'NONE', #58416, 1000.000000000000000 ) ;
#132825 = ORIENTED_EDGE ( 'NONE', *, *, #48574, .F. ) ;
#132826 = CARTESIAN_POINT ( 'NONE',  ( -7.499999999999951150, -14.70932175296478128, -11.46312253303835504 ) ) ;
#132827 = DIRECTION ( 'NONE',  ( -0.000000000000000000, 1.000000000000000000, 0.000000000000000000 ) ) ;
#132828 = CARTESIAN_POINT ( 'NONE',  ( 29.37956980810188412, 3.967499999999998916, 6.871911579029510442 ) ) ;
#132829 = VECTOR ( 'NONE', #106349, 1000.000000000000000 ) ;
#132830 = DIRECTION ( 'NONE',  ( 0.000000000000000000, 1.000000000000000000, 0.000000000000000000 ) ) ;
#132831 = VERTEX_POINT ( 'NONE', #27608 ) ;
#132832 = CARTESIAN_POINT ( 'NONE',  ( 107.5370968585647944, -3.054999999999999272, -5.291415217122919401 ) ) ;
#132833 = DIRECTION ( 'NONE',  ( -0.000000000000000000, 0.3543493200069153248, 0.9351131265310292928 ) ) ;
#132834 = DIRECTION ( 'NONE',  ( -0.000000000000000000, 0.3543493200069153248, 0.9351131265310292928 ) ) ;
#132836 = ORIENTED_EDGE ( 'NONE', *, *, #115263, .F. ) ;
#132835 = CARTESIAN_POINT ( 'NONE',  ( 19.05000000000000071, 3.174999999999997158, 5.000000000000000000 ) ) ;
#132837 = LINE ( 'NONE', #121900, #39303 ) ;
#132838 = ORIENTED_EDGE ( 'NONE', *, *, #11756, .F. ) ;
#132839 = LINE ( 'NONE', #54557, #81726 ) ;
#132840 = CARTESIAN_POINT ( 'NONE',  ( -23.99999999999983302, -15.03360074219758502, 5.000000000000000000 ) ) ;
#132842 = ORIENTED_EDGE ( 'NONE', *, *, #53758, .T. ) ;
#132841 = VECTOR ( 'NONE', #142579, 1000.000000000000000 ) ;
#132843 = DIRECTION ( 'NONE',  ( -0.000000000000000000, -0.000000000000000000, 1.000000000000000000 ) ) ;
#132844 = CARTESIAN_POINT ( 'NONE',  ( 11.15159235450332176, -3.851859888774471706E-31, 2.500000000000001332 ) ) ;
#132845 = ORIENTED_EDGE ( 'NONE', *, *, #64784, .T. ) ;
#132846 = PRODUCT_DEFINITION_FORMATION_WITH_SPECIFIED_SOURCE ( 'ANY', '', #7609, .NOT_KNOWN. ) ;
#132847 = CARTESIAN_POINT ( 'NONE',  ( -2.816011393730999401, 28.73617430169785436, 5.000000000000000000 ) ) ;
#132848 = CARTESIAN_POINT ( 'NONE',  ( -5.999999999999950262, 8.966399257802171618, 5.000000000000000000 ) ) ;
#132849 = ORIENTED_EDGE ( 'NONE', *, *, #127156, .F. ) ;
#132850 = LINE ( 'NONE', #22590, #73904 ) ;
#132851 = EDGE_CURVE ( 'NONE', #10224, #85316, #38506, .T. ) ;
#132853 = EDGE_LOOP ( 'NONE', ( #127780, #140610, #96860, #80463 ) ) ;
#132852 = DIRECTION ( 'NONE',  ( 1.000000000000000000, 0.000000000000000000, 0.000000000000000000 ) ) ;
#132855 = ORIENTED_EDGE ( 'NONE', *, *, #21095, .F. ) ;
#132854 = ADVANCED_FACE ( 'NONE', ( #82730 ), #139271, .F. ) ;
#132856 = CARTESIAN_POINT ( 'NONE',  ( 33.51665438641022376, 22.22500000000000142, 4.500000000000000888 ) ) ;
#132857 =( GEOMETRIC_REPRESENTATION_CONTEXT ( 3 ) GLOBAL_UNCERTAINTY_ASSIGNED_CONTEXT ( ( #28896 ) ) GLOBAL_UNIT_ASSIGNED_CONTEXT ( ( #13627, #42916, #76987 ) ) REPRESENTATION_CONTEXT ( 'NONE', 'WORKASPACE' ) );
#132858 = EDGE_LOOP ( 'NONE', ( #105036, #11656, #59866, #5779 ) ) ;
#132859 = CARTESIAN_POINT ( 'NONE',  ( -12.70000000000000817, -1.739288537755694446E-15, -40.00000000000000000 ) ) ;
#132860 = VECTOR ( 'NONE', #140501, 999.9999999999998863 ) ;
#132861 = DIRECTION ( 'NONE',  ( -0.7071067811865486830, -0.7071067811865464625, -0.000000000000000000 ) ) ;
#132862 = CARTESIAN_POINT ( 'NONE',  ( 26.99999999999998579, -7.850927237173508821, -1.251176053402193178 ) ) ;
#132863 = ORIENTED_EDGE ( 'NONE', *, *, #17929, .T. ) ;
#132864 = EDGE_CURVE ( 'NONE', #120303, #59180, #126908, .T. ) ;
#132865 = PLANE ( 'NONE',  #134645 ) ;
#132866 = CARTESIAN_POINT ( 'NONE',  ( -60.48921356237309510, -27.52281430457097500, 5.000000000000000000 ) ) ;
#132867 = CARTESIAN_POINT ( 'NONE',  ( -21.29974487139158512, -27.71228299555221142, 4.000000000000000000 ) ) ;
#132868 = FILL_AREA_STYLE_COLOUR ( '', #45994 ) ;
#132869 = CARTESIAN_POINT ( 'NONE',  ( 26.89126352523144092, -4.472830434245839371, -4.472830434245839371 ) ) ;
#132870 = VECTOR ( 'NONE', #90170, 1000.000000000000000 ) ;
#132871 = DIRECTION ( 'NONE',  ( -0.000000000000000000, -1.000000000000000000, -0.000000000000000000 ) ) ;
#132872 = EDGE_CURVE ( 'NONE', #71242, #105060, #127663, .T. ) ;
#132873 = VERTEX_POINT ( 'NONE', #16743 ) ;
#132874 = EDGE_LOOP ( 'NONE', ( #138705, #122247, #97161, #110293 ) ) ;
#132875 = CARTESIAN_POINT ( 'NONE',  ( 126.1250000000000142, -7.950000000000000178, -4.867971026610729436E-16 ) ) ;
#132876 = VECTOR ( 'NONE', #24052, 1000.000000000000000 ) ;
#132877 = ORIENTED_EDGE ( 'NONE', *, *, #61807, .T. ) ;
#132878 = AXIS2_PLACEMENT_3D ( 'NONE', #98123, #87950, #132193 ) ;
#132879 = ORIENTED_EDGE ( 'NONE', *, *, #58518, .T. ) ;
#132880 = LINE ( 'NONE', #102388, #40921 ) ;
#132881 = CARTESIAN_POINT ( 'NONE',  ( 32.29289321881321939, 11.25929247661560062, 5.000000000000000000 ) ) ;
#132882 = EDGE_CURVE ( 'NONE', #22872, #128013, #18131, .T. ) ;
#132883 = VERTEX_POINT ( 'NONE', #61020 ) ;
#132884 = FACE_OUTER_BOUND ( 'NONE', #92224, .T. ) ;
#132886 = AXIS2_PLACEMENT_3D ( 'NONE', #95902, #105346, #61877 ) ;
#132885 = CARTESIAN_POINT ( 'NONE',  ( 130.7379471109758526, -48.51956544822608208, 36.87500513592861040 ) ) ;
#132887 = DIRECTION ( 'NONE',  ( -0.6830127018922181881, 0.6830127018922202975, -0.2588190451025214056 ) ) ;
#132888 = CIRCLE ( 'NONE', #49589, 0.5000000000000000000 ) ;
#132889 = LINE ( 'NONE', #122679, #102070 ) ;
#132890 = CARTESIAN_POINT ( 'NONE',  ( 122.2087635252314328, -7.482591942790329030E-16, 6.110000000000001208 ) ) ;
#132891 = ORIENTED_EDGE ( 'NONE', *, *, #123643, .T. ) ;
#132892 = CARTESIAN_POINT ( 'NONE',  ( -54.48921356237310221, -27.52281430457093236, 5.000000000000000000 ) ) ;
#132893 = CARTESIAN_POINT ( 'NONE',  ( 13.88982677111779473, -22.22500000000000142, 4.785647885939352086 ) ) ;
#132894 = EDGE_CURVE ( 'NONE', #142445, #7871, #105176, .T. ) ;
#132895 = DIRECTION ( 'NONE',  ( -0.7071067811865487940, 0.7071067811865463515, 0.000000000000000000 ) ) ;
#132896 = CIRCLE ( 'NONE', #84264, 14.46000000000000085 ) ;
#132897 = DIRECTION ( 'NONE',  ( -0.6830127018922181881, 0.6830127018922202975, -0.2588190451025214056 ) ) ;
#132898 = FACE_OUTER_BOUND ( 'NONE', #56499, .T. ) ;
#132899 = DIRECTION ( 'NONE',  ( -0.6830127018922180770, -0.6830127018922204085, -0.2588190451025213501 ) ) ;
#132900 = VECTOR ( 'NONE', #138482, 1000.000000000000000 ) ;
#132901 = CARTESIAN_POINT ( 'NONE',  ( 47.47502705046288440, -5.819803920172572198, 5.819803920172572198 ) ) ;
#132902 = LINE ( 'NONE', #1600, #134752 ) ;
#132903 = AXIS2_PLACEMENT_3D ( 'NONE', #64496, #84821, #116735 ) ;
#132904 = CARTESIAN_POINT ( 'NONE',  ( 42.18398860626899705, 28.73617430169816700, 5.000000000000000000 ) ) ;
#132905 = ORIENTED_EDGE ( 'NONE', *, *, #66737, .F. ) ;
#132906 = ORIENTED_EDGE ( 'NONE', *, *, #4499, .T. ) ;
#132907 = CARTESIAN_POINT ( 'NONE',  ( 47.08333333333332149, 6.884901960086290629, -3.974999999999994316 ) ) ;
#132908 = CARTESIAN_POINT ( 'NONE',  ( 59.99451991528749772, 28.92564299267980132, 4.000000000000000000 ) ) ;
#132909 = EDGE_CURVE ( 'NONE', #111254, #13885, #7265, .T. ) ;
#132910 = AXIS2_PLACEMENT_3D ( 'NONE', #56398, #44813, #25858 ) ;
#132911 = DIRECTION ( 'NONE',  ( -0.7071067811865486830, -0.7071067811865464625, 0.000000000000000000 ) ) ;
#132912 = VERTEX_POINT ( 'NONE', #51538 ) ;
#132913 = CARTESIAN_POINT ( 'NONE',  ( -0.08791674731329272852, -1.320799999999990870, 4.000000000000001776 ) ) ;
#132915 = EDGE_CURVE ( 'NONE', #88412, #60505, #84183, .T. ) ;
#132914 = DIRECTION ( 'NONE',  ( 0.3543493200069163795, -9.265275131829747941E-33, -0.9351131265310288487 ) ) ;
#132916 = ADVANCED_FACE ( 'NONE', ( #107316 ), #7985, .F. ) ;
#132917 = CARTESIAN_POINT ( 'NONE',  ( 37.77126352523144703, 4.472830434245839371, 4.472830434245842035 ) ) ;
#132918 = EDGE_LOOP ( 'NONE', ( #88454, #120940, #26983, #74631 ) ) ;
#132919 = CARTESIAN_POINT ( 'NONE',  ( -34.42500000000001137, -4.458600742197945443, 5.000000000000000000 ) ) ;
#132920 = ORIENTED_EDGE ( 'NONE', *, *, #123194, .T. ) ;
#132921 = ORIENTED_EDGE ( 'NONE', *, *, #33697, .T. ) ;
#132922 = VECTOR ( 'NONE', #79736, 1000.000000000000000 ) ;
#132923 = CARTESIAN_POINT ( 'NONE',  ( 13.98012225071443915, -17.24070752338409918, 20.23474786156472405 ) ) ;
#132924 = EDGE_CURVE ( 'NONE', #33315, #18584, #110854, .T. ) ;
#132925 = FACE_OUTER_BOUND ( 'NONE', #21493, .T. ) ;
#132926 = FACE_OUTER_BOUND ( 'NONE', #125525, .T. ) ;
#132927 = DIRECTION ( 'NONE',  ( 0.7071067811865487940, 0.7071067811865463515, 0.000000000000000000 ) ) ;
#132928 = ORIENTED_EDGE ( 'NONE', *, *, #35190, .F. ) ;
#132929 = ADVANCED_FACE ( 'NONE', ( #54405 ), #87713, .F. ) ;
#132930 = DIRECTION ( 'NONE',  ( 0.7071067811865487940, 0.7071067811865463515, -0.000000000000000000 ) ) ;
#132931 = ORIENTED_EDGE ( 'NONE', *, *, #56539, .T. ) ;
#132932 = CARTESIAN_POINT ( 'NONE',  ( 79.77126352523143282, 4.472830434245838482, 4.472830434245842035 ) ) ;
#132933 = ADVANCED_FACE ( 'NONE', ( #34066 ), #52913, .F. ) ;
#132934 = CARTESIAN_POINT ( 'NONE',  ( -12.70710678118644843, -12.74070752338415602, 5.000000000000000000 ) ) ;
#132935 = DIRECTION ( 'NONE',  ( 0.7071067811865487940, 0.7071067811865463515, 0.000000000000000000 ) ) ;
#132936 = DIRECTION ( 'NONE',  ( -0.7071067811865486830, -0.7071067811865464625, -0.000000000000000000 ) ) ;
#132937 = VERTEX_POINT ( 'NONE', #141377 ) ;
#132938 = AXIS2_PLACEMENT_3D ( 'NONE', #59030, #5977, #38655 ) ;
#132939 = EDGE_CURVE ( 'NONE', #85156, #33404, #44978, .T. ) ;
#132940 = DIRECTION ( 'NONE',  ( -0.7071067811865486830, -0.7071067811865464625, 0.000000000000000000 ) ) ;
#132941 = CARTESIAN_POINT ( 'NONE',  ( 58.53709685856478728, -3.054999999999998828, -5.291415217122919401 ) ) ;
#132942 = DIRECTION ( 'NONE',  ( -0.7071067811865486830, -0.7071067811865464625, 0.000000000000000000 ) ) ;
#132943 = DIRECTION ( 'NONE',  ( 0.7071067811865487940, -0.7071067811865463515, 0.000000000000000000 ) ) ;
#132944 = CARTESIAN_POINT ( 'NONE',  ( -34.42500000000001137, -22.22500000000000142, 5.000000000000000000 ) ) ;
#132945 = ORIENTED_EDGE ( 'NONE', *, *, #113381, .T. ) ;
#132946 = VERTEX_POINT ( 'NONE', #43497 ) ;
#132947 = CYLINDRICAL_SURFACE ( 'NONE', #81678, 0.5000000000000004441 ) ;
#132949 = ADVANCED_FACE ( 'NONE', ( #89152 ), #86997, .F. ) ;
#132948 =( NAMED_UNIT ( * ) PLANE_ANGLE_UNIT ( ) SI_UNIT ( $, .RADIAN. ) );
#132950 = ORIENTED_EDGE ( 'NONE', *, *, #101956, .T. ) ;
#132951 = VECTOR ( 'NONE', #89603, 1000.000000000000000 ) ;
#132952 = LINE ( 'NONE', #119172, #14356 ) ;
#132953 = ORIENTED_EDGE ( 'NONE', *, *, #13063, .T. ) ;
#132954 = LINE ( 'NONE', #9695, #104759 ) ;
#132955 = PLANE ( 'NONE',  #124364 ) ;
#132956 = CARTESIAN_POINT ( 'NONE',  ( 17.99999999999987566, 16.93112307739200872, 4.000000000000000000 ) ) ;
#132957 = FACE_BOUND ( 'NONE', #94879, .T. ) ;
#132958 = DIRECTION ( 'NONE',  ( -0.000000000000000000, 1.000000000000000000, -0.000000000000000000 ) ) ;
#132959 = CARTESIAN_POINT ( 'NONE',  ( 5.816011393731002066, 28.73617430169783304, 5.000000000000000000 ) ) ;
#132960 = DIRECTION ( 'NONE',  ( -0.3543493200069162685, -0.000000000000000000, -0.9351131265310288487 ) ) ;
#132962 = EDGE_LOOP ( 'NONE', ( #81883, #97125, #62195, #42289 ) ) ;
#132961 = FACE_OUTER_BOUND ( 'NONE', #8551, .T. ) ;
#132963 = AXIS2_PLACEMENT_3D ( 'NONE', #96180, #98365, #117920 ) ;
#132964 = LINE ( 'NONE', #100312, #132067 ) ;
#132965 = ORIENTED_EDGE ( 'NONE', *, *, #51233, .F. ) ;
#132966 = EDGE_CURVE ( 'NONE', #84862, #1609, #119596, .T. ) ;
#132967 = EDGE_CURVE ( 'NONE', #57169, #40200, #122465, .T. ) ;
#132968 = VECTOR ( 'NONE', #25144, 999.9999999999998863 ) ;
#132969 = VERTEX_POINT ( 'NONE', #98580 ) ;
#132970 = CARTESIAN_POINT ( 'NONE',  ( 78.51626352523143737, -4.472830434245838482, 4.472830434245838482 ) ) ;
#132971 = VERTEX_POINT ( 'NONE', #42807 ) ;
#132972 = DIRECTION ( 'NONE',  ( 0.7071067811865487940, -0.7071067811865463515, 0.000000000000000000 ) ) ;
#132973 = LINE ( 'NONE', #20586, #44395 ) ;
#132974 = AXIS2_PLACEMENT_3D ( 'NONE', #57098, #101282, #110698 ) ;
#132975 = EDGE_LOOP ( 'NONE', ( #137087, #16548, #48775, #120041 ) ) ;
#132976 = DIRECTION ( 'NONE',  ( -1.000000000000000000, -1.224606353822377258E-16, -0.000000000000000000 ) ) ;
#132977 = LINE ( 'NONE', #58295, #58828 ) ;
#132978 = CARTESIAN_POINT ( 'NONE',  ( 18.48921356237309510, -27.52281430457068367, 5.000000000000000000 ) ) ;
#132979 = CARTESIAN_POINT ( 'NONE',  ( 3.770042794577902256, 21.73644205237997440, 5.000000000000000888 ) ) ;
#132980 = VECTOR ( 'NONE', #53479, 999.9999999999998863 ) ;
#132981 = CARTESIAN_POINT ( 'NONE',  ( -30.29974487139158867, -27.71228299555227537, 4.000000000000000000 ) ) ;
#132982 = DIRECTION ( 'NONE',  ( 0.3543493200069162685, -0.000000000000000000, -0.9351131265310288487 ) ) ;
#132983 = CARTESIAN_POINT ( 'NONE',  ( 15.18398860626900237, 28.73617430169797871, 5.000000000000000000 ) ) ;
#132984 = ORIENTED_EDGE ( 'NONE', *, *, #115152, .T. ) ;
#132985 = LINE ( 'NONE', #36321, #39955 ) ;
#132986 = ORIENTED_EDGE ( 'NONE', *, *, #103889, .F. ) ;
#132987 = LINE ( 'NONE', #43807, #58683 ) ;
#132988 = LINE ( 'NONE', #110458, #28088 ) ;
#132989 = ORIENTED_EDGE ( 'NONE', *, *, #92256, .F. ) ;
#132990 = VERTEX_POINT ( 'NONE', #55824 ) ;
#132991 = VERTEX_POINT ( 'NONE', #131950 ) ;
#132992 = VECTOR ( 'NONE', #69353, 1000.000000000000000 ) ;
#132993 = LINE ( 'NONE', #43813, #4436 ) ;
#132994 = ORIENTED_EDGE ( 'NONE', *, *, #124173, .T. ) ;
#132995 = CARTESIAN_POINT ( 'NONE',  ( 122.6835989386367771, -43.14999999999999147, -34.92499999999998295 ) ) ;
#132996 = AXIS2_PLACEMENT_3D ( 'NONE', #129042, #29714, #73964 ) ;
#132997 = LINE ( 'NONE', #21349, #97952 ) ;
#132998 = AXIS2_PLACEMENT_3D ( 'NONE', #50598, #51323, #43127 ) ;
#132999 = CARTESIAN_POINT ( 'NONE',  ( 31.25413961620377634, 3.047499999999993214, -5.278424836066146320 ) ) ;
#133000 = DIRECTION ( 'NONE',  ( 0.6830127018922181881, 0.6830127018922202975, -0.2588190451025214056 ) ) ;
#133001 = ORIENTED_EDGE ( 'NONE', *, *, #23951, .T. ) ;
#133002 = ORIENTED_EDGE ( 'NONE', *, *, #137186, .F. ) ;
#133003 = LINE ( 'NONE', #109787, #23318 ) ;
#133004 = DIRECTION ( 'NONE',  ( -0.000000000000000000, -0.000000000000000000, 1.000000000000000000 ) ) ;
#133006 = VERTEX_POINT ( 'NONE', #76132 ) ;
#133005 = CARTESIAN_POINT ( 'NONE',  ( 0.005480084712502889671, 28.92564299267938210, 4.000000000000000000 ) ) ;
#133007 = VERTEX_POINT ( 'NONE', #131220 ) ;
#133008 = CARTESIAN_POINT ( 'NONE',  ( 42.29974487139158157, -27.71228299555235708, 4.000000000000000000 ) ) ;
#133009 =( BOUNDED_CURVE ( )  B_SPLINE_CURVE ( 3, ( #58823, #25398, #102291, #47234 ),
 .UNSPECIFIED., .F., .F. ) 
 B_SPLINE_CURVE_WITH_KNOTS ( ( 4, 4 ),
 ( 1.208578181583233491, 1.359146454359404510 ),
 .UNSPECIFIED. ) 
 CURVE ( )  GEOMETRIC_REPRESENTATION_ITEM ( )  RATIONAL_B_SPLINE_CURVE ( ( 1.000000000000000000, 0.9981116584018959736, 0.9981116584018959736, 1.000000000000000000 ) ) 
 REPRESENTATION_ITEM ( '' )  );
#133010 = LINE ( 'NONE', #111197, #90828 ) ;
#133011 = DIRECTION ( 'NONE',  ( 0.7071067811865486830, -0.7071067811865464625, -0.000000000000000000 ) ) ;
#133012 = ORIENTED_EDGE ( 'NONE', *, *, #132939, .T. ) ;
#133013 = CARTESIAN_POINT ( 'NONE',  ( 7.720000000000001528, 2.055000000000001492, 2.516649172247811554E-16 ) ) ;
#133014 = LINE ( 'NONE', #39752, #73403 ) ;
#133015 = ORIENTED_EDGE ( 'NONE', *, *, #55162, .T. ) ;
#133016 = LINE ( 'NONE', #33695, #61128 ) ;
#133017 = LINE ( 'NONE', #3168, #21638 ) ;
#133018 = DIRECTION ( 'NONE',  ( 0.6830127018922181881, 0.6830127018922202975, -0.2588190451025214056 ) ) ;
#133019 = CARTESIAN_POINT ( 'NONE',  ( -4.228506771386627783, 20.25929247661551003, 7.808871592221759528 ) ) ;
#133020 = FACE_OUTER_BOUND ( 'NONE', #125530, .T. ) ;
#133021 = ADVANCED_FACE ( 'NONE', ( #9395 ), #97114, .F. ) ;
#133022 = CARTESIAN_POINT ( 'NONE',  ( 15.65467068707222076, 3.821174125832445049E-16, 0.000000000000000000 ) ) ;
#133023 = DIRECTION ( 'NONE',  ( -0.7071067811865486830, -0.7071067811865464625, -0.000000000000000000 ) ) ;
#133024 = ADVANCED_FACE ( 'NONE', ( #86305 ), #32638, .F. ) ;
#133026 = ORIENTED_EDGE ( 'NONE', *, *, #28065, .F. ) ;
#133025 = EDGE_CURVE ( 'NONE', #115355, #67593, #75423, .T. ) ;
#133027 = ORIENTED_EDGE ( 'NONE', *, *, #107591, .F. ) ;
#133028 = LINE ( 'NONE', #67035, #66476 ) ;
#133029 = CARTESIAN_POINT ( 'NONE',  ( 128.9683591370938416, -52.14999999999999147, -41.64500000000001023 ) ) ;
#133030 = EDGE_CURVE ( 'NONE', #54989, #115943, #130526, .T. ) ;
#133031 = EDGE_CURVE ( 'NONE', #12969, #96758, #44233, .T. ) ;
#133032 = CARTESIAN_POINT ( 'NONE',  ( 18.01107201284014536, 3.821174125832445049E-16, 0.000000000000000000 ) ) ;
#133033 = ORIENTED_EDGE ( 'NONE', *, *, #50225, .T. ) ;
#133034 = DIRECTION ( 'NONE',  ( 0.7071067811865487940, 0.7071067811865463515, -0.000000000000000000 ) ) ;
#133035 = CARTESIAN_POINT ( 'NONE',  ( -12.09843580608229274, 11.25929247661560950, 10.79108189686404096 ) ) ;
#133036 = ORIENTED_EDGE ( 'NONE', *, *, #27711, .T. ) ;
#133037 = EDGE_CURVE ( 'NONE', #133264, #69882, #132690, .T. ) ;
#133038 = DIRECTION ( 'NONE',  ( -1.000000000000000000, -1.224606353822377258E-16, -0.000000000000000000 ) ) ;
#133039 = DIRECTION ( 'NONE',  ( 0.6830127018922180770, -0.6830127018922204085, -0.2588190451025213501 ) ) ;
#133040 = CARTESIAN_POINT ( 'NONE',  ( 20.81601139373100295, 28.73617430169773002, 5.000000000000000000 ) ) ;
#133041 = PRESENTATION_STYLE_ASSIGNMENT (( #44621 ) ) ;
#133042 = DIRECTION ( 'NONE',  ( 0.7071067811865487940, -0.7071067811865463515, 0.000000000000000000 ) ) ;
#133043 = CARTESIAN_POINT ( 'NONE',  ( 54.59959685856476597, -6.109999999999998543, -1.637169565754160727 ) ) ;
#133044 = AXIS2_PLACEMENT_3D ( 'NONE', #30433, #121694, #74667 ) ;
#133045 = LINE ( 'NONE', #90959, #97327 ) ;
#133046 = ADVANCED_FACE ( 'NONE', ( #65997 ), #66687, .F. ) ;
#133047 = CARTESIAN_POINT ( 'NONE',  ( 28.17183060077627488, -20.24070752338407431, 4.000000000000000000 ) ) ;
#133048 = CARTESIAN_POINT ( 'NONE',  ( 32.01669371712954160, 7.950000000000000178, -2.130196079827421318 ) ) ;
#133049 = DIRECTION ( 'NONE',  ( -0.000000000000000000, -0.3543493200069152693, 0.9351131265310292928 ) ) ;
#133050 = ORIENTED_EDGE ( 'NONE', *, *, #14401, .F. ) ;
#133051 = FILL_AREA_STYLE ('',( #90964 ) ) ;
#133052 = ORIENTED_EDGE ( 'NONE', *, *, #100127, .T. ) ;
#133053 = CARTESIAN_POINT ( 'NONE',  ( 17.84387692260747116, -22.22499999999999076, 4.000000000000000000 ) ) ;
#133054 = ADVANCED_FACE ( 'NONE', ( #112330 ), #126066, .F. ) ;
#133055 = CARTESIAN_POINT ( 'NONE',  ( 42.48921356237308800, -27.52281430457085065, 5.000000000000000000 ) ) ;
#133056 = DIRECTION ( 'NONE',  ( 0.6830127018922180770, -0.6830127018922204085, -0.2588190451025213501 ) ) ;
#133057 = SURFACE_STYLE_FILL_AREA ( #43179 ) ;
#133058 = CARTESIAN_POINT ( 'NONE',  ( -34.47516574401893052, 13.49051761211547529, 4.998110765256835286 ) ) ;
#133059 = PLANE ( 'NONE',  #59304 ) ;
#133060 = ORIENTED_EDGE ( 'NONE', *, *, #39427, .F. ) ;
#133061 = ORIENTED_EDGE ( 'NONE', *, *, #75745, .F. ) ;
#133062 = CARTESIAN_POINT ( 'NONE',  ( 5.816011393731002066, 28.73617430169783304, 5.000000000000000000 ) ) ;
#133063 = DIRECTION ( 'NONE',  ( -0.6830127018922181881, 0.6830127018922202975, -0.2588190451025214056 ) ) ;
#133064 = UNCERTAINTY_MEASURE_WITH_UNIT (LENGTH_MEASURE( 1.000000000000000082E-05 ), #114168, 'distance_accuracy_value', 'NONE');
#133066 = EDGE_CURVE ( 'NONE', #63744, #70033, #12981, .T. ) ;
#133065 = CIRCLE ( 'NONE', #123738, 2.500000000000000888 ) ;
#133067 = DIRECTION ( 'NONE',  ( 0.7071067811865487940, -0.7071067811865463515, -0.000000000000000000 ) ) ;
#133068 = DIRECTION ( 'NONE',  ( 0.7071067811865487940, 0.7071067811865463515, 0.000000000000000000 ) ) ;
#133069 = CARTESIAN_POINT ( 'NONE',  ( 81.01669371712955581, 7.950000000000001066, -2.130196079827421318 ) ) ;
#133070 = CARTESIAN_POINT ( 'NONE',  ( -19.82816939922339117, 21.75929247661550647, 4.000000000000000000 ) ) ;
#133071 = LINE ( 'NONE', #101836, #69237 ) ;
#133072 = EDGE_LOOP ( 'NONE', ( #107209, #74026, #104137, #3856, #55797 ) ) ;
#133073 = CARTESIAN_POINT ( 'NONE',  ( 77.41666666666665719, -6.884901960086287076, -3.975000000000000977 ) ) ;
#133074 = CARTESIAN_POINT ( 'NONE',  ( -9.489213562373095101, -27.52281430457062328, 5.000000000000000000 ) ) ;
#133075 = AXIS2_PLACEMENT_3D ( 'NONE', #33051, #38721, #14816 ) ;
#133076 = DIRECTION ( 'NONE',  ( -1.000000000000000000, 0.000000000000000000, 0.000000000000000000 ) ) ;
#133077 = DIRECTION ( 'NONE',  ( 0.7071067811865487940, -0.7071067811865463515, 0.000000000000000000 ) ) ;
#133078 = ADVANCED_FACE ( 'NONE', ( #69560 ), #2833, .F. ) ;
#133079 = VERTEX_POINT ( 'NONE', #124620 ) ;
#133080 = CARTESIAN_POINT ( 'NONE',  ( 27.99999999999996803, -57.14999999999999147, 45.92499999999999005 ) ) ;
#133081 = ADVANCED_FACE ( 'NONE', ( #4195 ), #136925, .F. ) ;
#133082 = ORIENTED_EDGE ( 'NONE', *, *, #92777, .F. ) ;
#133083 = AXIS2_PLACEMENT_3D ( 'NONE', #24412, #4026, #16357 ) ;
#133084 = DIRECTION ( 'NONE',  ( 0.000000000000000000, 1.000000000000000000, 0.000000000000000000 ) ) ;
#133085 = CARTESIAN_POINT ( 'NONE',  ( 67.95876352523144703, 0.000000000000000000, -6.110000000000001208 ) ) ;
#133086 = ADVANCED_FACE ( 'NONE', ( #36886 ), #26034, .T. ) ;
#133087 = DIRECTION ( 'NONE',  ( 0.7071067811865486830, -0.7071067811865464625, -0.000000000000000000 ) ) ;
#133088 = ORIENTED_EDGE ( 'NONE', *, *, #69838, .F. ) ;
#133089 = FACE_OUTER_BOUND ( 'NONE', #23050, .T. ) ;
#133090 = EDGE_CURVE ( 'NONE', #113958, #102574, #57258, .T. ) ;
#133091 = DIRECTION ( 'NONE',  ( -0.000000000000000000, 0.000000000000000000, 1.000000000000000000 ) ) ;
#133092 = LINE ( 'NONE', #99705, #120712 ) ;
#133093 = CARTESIAN_POINT ( 'NONE',  ( 3.469446951953614189E-15, -1.447814304570820276, 5.000000000000000000 ) ) ;
#133094 = DIRECTION ( 'NONE',  ( -0.7071067811865486830, -0.7071067811865464625, 0.000000000000000000 ) ) ;
#133096 = VERTEX_POINT ( 'NONE', #113745 ) ;
#133095 = CARTESIAN_POINT ( 'NONE',  ( 32.99999999999977263, 13.55218569542903140, 5.000000000000000000 ) ) ;
#133097 = DIRECTION ( 'NONE',  ( 0.7071067811865486830, -0.7071067811865464625, -0.000000000000000000 ) ) ;
#133098 = CARTESIAN_POINT ( 'NONE',  ( 3.770729005911382714, 22.22500000000000142, 19.66325824265030775 ) ) ;
#133099 = DIRECTION ( 'NONE',  ( -1.000000000000000000, -0.000000000000000000, 0.000000000000000000 ) ) ;
#133100 = ORIENTED_EDGE ( 'NONE', *, *, #62245, .T. ) ;
#133101 = AXIS2_PLACEMENT_3D ( 'NONE', #13377, #65700, #112717 ) ;
#133102 = VERTEX_POINT ( 'NONE', #101435 ) ;
#133103 = CARTESIAN_POINT ( 'NONE',  ( 68.39626352523141861, 4.472830434245840259, -4.472830434245839371 ) ) ;
#133104 = VECTOR ( 'NONE', #138146, 1000.000000000000000 ) ;
#133105 = ORIENTED_EDGE ( 'NONE', *, *, #77589, .T. ) ;
#133106 = AXIS2_PLACEMENT_3D ( 'NONE', #78203, #67330, #60765 ) ;
#133107 = EDGE_CURVE ( 'NONE', #34133, #60854, #2084, .T. ) ;
#133108 = CARTESIAN_POINT ( 'NONE',  ( -11.81601139373100651, 28.73617430169779041, 5.000000000000000000 ) ) ;
#133109 = CARTESIAN_POINT ( 'NONE',  ( 8.994519915287490619, 28.92564299267944250, 4.000000000000000000 ) ) ;
#133110 = CARTESIAN_POINT ( 'NONE',  ( -36.29974487139159578, -27.71228299555231445, 4.000000000000000000 ) ) ;
#133111 = FACE_OUTER_BOUND ( 'NONE', #52156, .T. ) ;
#133112 = LINE ( 'NONE', #91027, #87210 ) ;
#133113 = ORIENTED_EDGE ( 'NONE', *, *, #119514, .T. ) ;
#133114 = VERTEX_POINT ( 'NONE', #47814 ) ;
#133115 = DIRECTION ( 'NONE',  ( -0.7071067811865486830, -0.7071067811865464625, 0.000000000000000000 ) ) ;
#133116 = VERTEX_POINT ( 'NONE', #80429 ) ;
#133117 = EDGE_CURVE ( 'NONE', #54672, #105689, #46395, .T. ) ;
#133118 = CARTESIAN_POINT ( 'NONE',  ( -0.1839886062690032631, 28.73617430169787568, 5.000000000000000000 ) ) ;
#133119 = CARTESIAN_POINT ( 'NONE',  ( -30.18398860626900060, 28.73617430169808173, 5.000000000000000000 ) ) ;
#133120 = CARTESIAN_POINT ( 'NONE',  ( 5.510786437626906675, -27.52281430457051314, 5.000000000000000000 ) ) ;
#133121 = VERTEX_POINT ( 'NONE', #68843 ) ;
#133122 = FACE_BOUND ( 'NONE', #130331, .T. ) ;
#133123 = CARTESIAN_POINT ( 'NONE',  ( -32.99999999999976552, 5.587461875839186298, 4.000000000000000000 ) ) ;
#133124 = CARTESIAN_POINT ( 'NONE',  ( -60.18398860626900415, 28.73617430169829490, 5.000000000000000000 ) ) ;
#133125 = LINE ( 'NONE', #33803, #117687 ) ;
#133126 = SURFACE_STYLE_USAGE ( .BOTH. , #121492 ) ;
#133127 = CARTESIAN_POINT ( 'NONE',  ( -12.20000000000000462, -21.76999999999999247, 0.000000000000000000 ) ) ;
#133128 =( NAMED_UNIT ( * ) SI_UNIT ( $, .STERADIAN. ) SOLID_ANGLE_UNIT ( ) );
#133129 = VERTEX_POINT ( 'NONE', #100735 ) ;
#133130 = ADVANCED_FACE ( 'NONE', ( #135516 ), #51688, .T. ) ;
#133131 = ORIENTED_EDGE ( 'NONE', *, *, #103718, .F. ) ;
#133132 = CARTESIAN_POINT ( 'NONE',  ( 105.6412635252314516, 4.472830434245835818, 4.472830434245840259 ) ) ;
#133133 = VERTEX_POINT ( 'NONE', #90583 ) ;
#133134 = ADVANCED_FACE ( 'NONE', ( #134820 ), #35516, .T. ) ;
#133135 = CARTESIAN_POINT ( 'NONE',  ( 0.000000000000000000, 0.000000000000000000, 5.000000000000000000 ) ) ;
#133136 = ORIENTED_EDGE ( 'NONE', *, *, #107541, .F. ) ;
#133137 = CARTESIAN_POINT ( 'NONE',  ( -19.05000000000000071, 3.174999999999997158, 4.000000000000000000 ) ) ;
#133138 = CARTESIAN_POINT ( 'NONE',  ( 3.254139616203772345, 3.047499999999993214, -5.278424836066146320 ) ) ;
#133140 = ADVANCED_FACE ( 'NONE', ( #70295 ), #134085, .T. ) ;
#133139 = DIRECTION ( 'NONE',  ( 1.000000000000000000, 0.000000000000000000, 0.000000000000000000 ) ) ;
#133141 = VERTEX_POINT ( 'NONE', #36200 ) ;
#133142 = DIRECTION ( 'NONE',  ( 0.000000000000000000, -1.000000000000000000, 0.000000000000000000 ) ) ;
#133143 = DIRECTION ( 'NONE',  ( 0.6830127018922180770, -0.6830127018922204085, -0.2588190451025213501 ) ) ;
#133144 = DIRECTION ( 'NONE',  ( 0.3543493200069162685, -0.000000000000000000, -0.9351131265310288487 ) ) ;
#133145 = DIRECTION ( 'NONE',  ( -1.000000000000000000, 0.000000000000000000, 0.000000000000000000 ) ) ;
#133147 = DIRECTION ( 'NONE',  ( 0.3543493200069162685, -0.000000000000000000, -0.9351131265310288487 ) ) ;
#133146 = DIRECTION ( 'NONE',  ( 0.7071067811865487940, -0.7071067811865463515, 0.000000000000000000 ) ) ;
#133148 = CARTESIAN_POINT ( 'NONE',  ( 9.712309939660210389, -21.73547319004781997, 4.999917730833664642 ) ) ;
#133149 = CARTESIAN_POINT ( 'NONE',  ( 24.32816939922335919, -12.74070752338415957, 4.000000000000000000 ) ) ;
#133150 = EDGE_LOOP ( 'NONE', ( #54749, #119101, #36433, #120234 ) ) ;
#133151 = CARTESIAN_POINT ( 'NONE',  ( -66.48921356237309510, -27.52281430457101763, 5.000000000000000000 ) ) ;
#133152 = PLANE ( 'NONE',  #81307 ) ;
#133153 = ORIENTED_EDGE ( 'NONE', *, *, #107053, .T. ) ;
#133154 = EDGE_LOOP ( 'NONE', ( #137615, #58454, #84549 ) ) ;
#133155 = ADVANCED_FACE ( 'NONE', ( #79748 ), #123930, .F. ) ;
#133156 = ORIENTED_EDGE ( 'NONE', *, *, #78248, .F. ) ;
#133157 = CARTESIAN_POINT ( 'NONE',  ( 55.12543019189811133, 5.291415217122919401, 3.055000000000002824 ) ) ;
#133158 = ORIENTED_EDGE ( 'NONE', *, *, #6698, .F. ) ;
#133159 = DIRECTION ( 'NONE',  ( 0.000000000000000000, 0.000000000000000000, 1.000000000000000000 ) ) ;
#133160 = AXIS2_PLACEMENT_3D ( 'NONE', #120921, #132561, #77459 ) ;
#133161 = CARTESIAN_POINT ( 'NONE',  ( 1.649972949537105604, -4.461849672132299105, 4.461849672132299993 ) ) ;
#133162 = CARTESIAN_POINT ( 'NONE',  ( 90.56293019189810423, 1.637169565754157174, 6.110000000000002984 ) ) ;
#133163 = FILL_AREA_STYLE ('',( #36663 ) ) ;
#133164 = AXIS2_PLACEMENT_3D ( 'NONE', #95052, #109331, #32499 ) ;
#133165 = VERTEX_POINT ( 'NONE', #57979 ) ;
#133166 = CARTESIAN_POINT ( 'NONE',  ( 22.07159235450331991, 3.061616997868380183E-16, -2.500000000000001332 ) ) ;
#133167 = CARTESIAN_POINT ( 'NONE',  ( -2.994519915287485734, 28.92564299267940342, 4.000000000000000000 ) ) ;
#133168 = VERTEX_POINT ( 'NONE', #102175 ) ;
#133169 = CARTESIAN_POINT ( 'NONE',  ( -2.671830600776449405, 8.259292476615637923, 4.000000000000000000 ) ) ;
#133170 = DIRECTION ( 'NONE',  ( 0.7071067811865486830, -0.7071067811865464625, -0.000000000000000000 ) ) ;
#133171 = ORIENTED_EDGE ( 'NONE', *, *, #13405, .T. ) ;
#133172 = DIRECTION ( 'NONE',  ( -0.000000000000000000, 0.000000000000000000, 1.000000000000000000 ) ) ;
#133173 = VECTOR ( 'NONE', #62249, 1000.000000000000114 ) ;
#133174 = ORIENTED_EDGE ( 'NONE', *, *, #16296, .F. ) ;
#133175 = EDGE_LOOP ( 'NONE', ( #12839, #89942, #9824, #76574 ) ) ;
#133176 = ORIENTED_EDGE ( 'NONE', *, *, #79896, .T. ) ;
#133177 = CARTESIAN_POINT ( 'NONE',  ( 122.9954301918981230, 5.291415217122916737, 3.055000000000001936 ) ) ;
#133178 = EDGE_CURVE ( 'NONE', #88227, #19705, #91311, .T. ) ;
#133179 = DIRECTION ( 'NONE',  ( -0.7071067811865486830, 0.7071067811865464625, 0.000000000000000000 ) ) ;
#133180 = CARTESIAN_POINT ( 'NONE',  ( 2.613322195557305161, 2.055000000000001048, 0.000000000000000000 ) ) ;
#133181 = EDGE_CURVE ( 'NONE', #50175, #9966, #49937, .T. ) ;
#133182 = ADVANCED_FACE ( 'NONE', ( #41172 ), #29574, .T. ) ;
#133183 = ORIENTED_EDGE ( 'NONE', *, *, #50733, .F. ) ;
#133184 = DIRECTION ( 'NONE',  ( -0.3543493200069162685, -0.000000000000000000, -0.9351131265310288487 ) ) ;
#133185 = EDGE_LOOP ( 'NONE', ( #38420, #6106, #13672, #43505 ) ) ;
#133186 = VECTOR ( 'NONE', #41218, 1000.000000000000000 ) ;
#133187 = EDGE_CURVE ( 'NONE', #10027, #66379, #18687, .T. ) ;
#133188 = EDGE_CURVE ( 'NONE', #73197, #98076, #107141, .T. ) ;
#133189 = VECTOR ( 'NONE', #135829, 999.9999999999998863 ) ;
#133190 = CARTESIAN_POINT ( 'NONE',  ( 15.29123647476855297, -9.717572351234235426E-16, -7.934999999999990727 ) ) ;
#133191 = CARTESIAN_POINT ( 'NONE',  ( -3.707013264293017141, -21.74070752338405299, 4.999753212805222446 ) ) ;
#133192 = AXIS2_PLACEMENT_3D ( 'NONE', #83968, #86800, #96903 ) ;
#133193 = EDGE_CURVE ( 'NONE', #86287, #49673, #71682, .T. ) ;
#133194 = DIRECTION ( 'NONE',  ( 0.3543493200069162685, -0.000000000000000000, -0.9351131265310288487 ) ) ;
#133195 = VECTOR ( 'NONE', #8615, 1000.000000000000227 ) ;
#133196 = DIRECTION ( 'NONE',  ( -0.000000000000000000, -0.3543493200069152693, 0.9351131265310292928 ) ) ;
#133197 = ORIENTED_EDGE ( 'NONE', *, *, #1401, .T. ) ;
#133198 = ORIENTED_EDGE ( 'NONE', *, *, #93888, .F. ) ;
#133199 = EDGE_CURVE ( 'NONE', #103464, #16482, #47085, .T. ) ;
#133200 = ORIENTED_EDGE ( 'NONE', *, *, #128837, .T. ) ;
#133201 = DIRECTION ( 'NONE',  ( 0.7071067811865487940, -0.7071067811865463515, 0.000000000000000000 ) ) ;
#133202 = UNCERTAINTY_MEASURE_WITH_UNIT (LENGTH_MEASURE( 1.000000000000000082E-05 ), #108989, 'distance_accuracy_value', 'NONE');
#133203 = EDGE_CURVE ( 'NONE', #106661, #83402, #137659, .T. ) ;
#133204 = DIRECTION ( 'NONE',  ( -1.000000000000000000, 0.000000000000000000, -0.000000000000000000 ) ) ;
#133205 = CARTESIAN_POINT ( 'NONE',  ( -34.92500000000001137, 22.22500000000000142, 4.000000000000000000 ) ) ;
#133206 = ADVANCED_FACE ( 'NONE', ( #84011 ), #85381, .F. ) ;
#133207 = CARTESIAN_POINT ( 'NONE',  ( -24.32816939922335209, 11.25929247661560950, 4.000000000000000000 ) ) ;
#133208 = CARTESIAN_POINT ( 'NONE',  ( 0.000000000000000000, 0.000000000000000000, 0.000000000000000000 ) ) ;
#133209 = DIRECTION ( 'NONE',  ( 0.7071067811865486830, -0.7071067811865464625, -0.000000000000000000 ) ) ;
#133210 = DIRECTION ( 'NONE',  ( 0.5735764363510444941, 0.8191520442889929088, 0.000000000000000000 ) ) ;
#133211 = ORIENTED_EDGE ( 'NONE', *, *, #6457, .F. ) ;
#133212 = CARTESIAN_POINT ( 'NONE',  ( 125.5000000000000000, -3.441786896390352624, 7.166352137582667758 ) ) ;
#133213 = VERTEX_POINT ( 'NONE', #128892 ) ;
#133214 = CARTESIAN_POINT ( 'NONE',  ( 16.63171309283781696, 0.4494914063655743863, -33.70035307763171062 ) ) ;
#133215 = ORIENTED_EDGE ( 'NONE', *, *, #42703, .T. ) ;
#133216 = EDGE_CURVE ( 'NONE', #62934, #101394, #26732, .T. ) ;
#133217 = DIRECTION ( 'NONE',  ( -0.6830127018922181881, 0.6830127018922202975, -0.2588190451025214056 ) ) ;
#133219 = ORIENTED_EDGE ( 'NONE', *, *, #87004, .F. ) ;
#133218 = CARTESIAN_POINT ( 'NONE',  ( 5.999999999999964473, 19.93112307739198386, 4.000000000000000000 ) ) ;
#133220 = FILL_AREA_STYLE_COLOUR ( '', #113435 ) ;
#133221 = CARTESIAN_POINT ( 'NONE',  ( 0.000000000000000000, 0.000000000000000000, 5.000000000000000000 ) ) ;
#133222 = ORIENTED_EDGE ( 'NONE', *, *, #133216, .T. ) ;
#133223 = CARTESIAN_POINT ( 'NONE',  ( -8.648657329869978142E-14, -34.64999999999997726, -40.00000000000000000 ) ) ;
#133224 = ORIENTED_EDGE ( 'NONE', *, *, #40773, .F. ) ;
#133225 = FACE_OUTER_BOUND ( 'NONE', #44568, .T. ) ;
#133226 = ORIENTED_EDGE ( 'NONE', *, *, #95104, .T. ) ;
#133227 = EDGE_CURVE ( 'NONE', #98041, #1156, #70975, .T. ) ;
#133228 = CARTESIAN_POINT ( 'NONE',  ( 0.000000000000000000, 0.000000000000000000, 5.000000000000000000 ) ) ;
#133229 =( BOUNDED_CURVE ( )  B_SPLINE_CURVE ( 3, ( #100889, #134250, #24056, #58151 ),
 .UNSPECIFIED., .F., .T. ) 
 B_SPLINE_CURVE_WITH_KNOTS ( ( 4, 4 ),
 ( 4.712388980384689674, 6.105785702739217058 ),
 .UNSPECIFIED. ) 
 CURVE ( )  GEOMETRIC_REPRESENTATION_ITEM ( )  RATIONAL_B_SPLINE_CURVE ( ( 1.000000000000000000, 0.8446433258982466441, 0.8446433258982466441, 1.000000000000000000 ) ) 
 REPRESENTATION_ITEM ( '' )  );
#133230 = CARTESIAN_POINT ( 'NONE',  ( 114.4125270504628986, -7.949999999999998401, -4.867971026610728450E-16 ) ) ;
#133231 = FACE_OUTER_BOUND ( 'NONE', #117462, .T. ) ;
#133232 = DIRECTION ( 'NONE',  ( -1.000000000000000000, -1.224606353822377258E-16, -0.000000000000000000 ) ) ;
#133233 = SURFACE_STYLE_FILL_AREA ( #110012 ) ;
#133234 = CARTESIAN_POINT ( 'NONE',  ( -23.20710678118637915, -8.240707523384202204, 5.000000000000000000 ) ) ;
#133235 = DIRECTION ( 'NONE',  ( -1.000000000000000000, -1.224606353822377258E-16, -0.000000000000000000 ) ) ;
#133236 = CARTESIAN_POINT ( 'NONE',  ( 18.52083333333333570, -6.094999999999989981, -1.633150327867689100 ) ) ;
#133237 = CARTESIAN_POINT ( 'NONE',  ( 2.994519915287485734, 28.92564299267940342, 4.000000000000000000 ) ) ;
#133238 = PLANE ( 'NONE',  #23469 ) ;
#133239 = DIRECTION ( 'NONE',  ( -0.7071067811865486830, -0.7071067811865464625, 0.000000000000000000 ) ) ;
#133240 = ORIENTED_EDGE ( 'NONE', *, *, #96957, .T. ) ;
#133241 = ORIENTED_EDGE ( 'NONE', *, *, #59534, .T. ) ;
#133242 = DIRECTION ( 'NONE',  ( -1.000000000000000000, -1.224606353822377258E-16, -0.000000000000000000 ) ) ;
#133243 = ORIENTED_EDGE ( 'NONE', *, *, #106707, .F. ) ;
#133244 = CARTESIAN_POINT ( 'NONE',  ( 102.2295968585647614, -6.110000000000000320, -1.637169565754161393 ) ) ;
#133245 = EDGE_CURVE ( 'NONE', #74481, #38431, #60098, .T. ) ;
#133246 = LINE ( 'NONE', #112891, #108134 ) ;
#133247 = CARTESIAN_POINT ( 'NONE',  ( 10.49999999999993250, 3.052185695429136647, 5.000000000000000000 ) ) ;
#133248 = DIRECTION ( 'NONE',  ( -0.7071067811865486830, -0.7071067811865464625, 0.000000000000000000 ) ) ;
#133249 = FACE_OUTER_BOUND ( 'NONE', #76907, .T. ) ;
#133250 = ORIENTED_EDGE ( 'NONE', *, *, #73362, .F. ) ;
#133251 = CARTESIAN_POINT ( 'NONE',  ( 11.99999999999991296, 19.93112307739198386, 4.000000000000000000 ) ) ;
#133252 = DIRECTION ( 'NONE',  ( -1.000000000000000000, -3.115803279706882722E-16, 0.000000000000000000 ) ) ;
#133253 = EDGE_CURVE ( 'NONE', #89658, #59700, #139080, .T. ) ;
#133254 = CARTESIAN_POINT ( 'NONE',  ( -17.28242261357420873, -21.73023691814492864, 5.000000000000000000 ) ) ;
#133255 = SURFACE_SIDE_STYLE ('',( #84234 ) ) ;
#133256 = DIRECTION ( 'NONE',  ( -0.000000000000000000, 0.3543493200069153248, 0.9351131265310292928 ) ) ;
#133258 = ORIENTED_EDGE ( 'NONE', *, *, #78541, .T. ) ;
#133257 = CARTESIAN_POINT ( 'NONE',  ( 23.67183060077630685, -12.74070752338415069, 4.000000000000000000 ) ) ;
#133259 = LINE ( 'NONE', #57140, #10612 ) ;
#133260 = SURFACE_STYLE_USAGE ( .BOTH. , #88321 ) ;
#133261 = LINE ( 'NONE', #80314, #34050 ) ;
#133262 = EDGE_CURVE ( 'NONE', #58070, #88273, #111915, .T. ) ;
#133263 = LINE ( 'NONE', #88324, #111651 ) ;
#133264 = VERTEX_POINT ( 'NONE', #28170 ) ;
#133265 = ORIENTED_EDGE ( 'NONE', *, *, #50871, .F. ) ;
#133266 = VERTEX_POINT ( 'NONE', #16551 ) ;
#133267 = CARTESIAN_POINT ( 'NONE',  ( 90.70876352523143282, -7.482591942790329030E-16, 6.110000000000001208 ) ) ;
#133268 = ORIENTED_EDGE ( 'NONE', *, *, #8714, .F. ) ;
#133269 = PRESENTATION_LAYER_ASSIGNMENT (  '', '', ( #119346 ) ) ;
#133270 = ADVANCED_FACE ( 'NONE', ( #94116 ), #39038, .F. ) ;
#133271 = LINE ( 'NONE', #78892, #50921 ) ;
#133272 = LINE ( 'NONE', #54991, #20174 ) ;
#133273 = CARTESIAN_POINT ( 'NONE',  ( -32.99999999999976552, -13.44781430457069149, 5.000000000000000000 ) ) ;
#133274 = DIRECTION ( 'NONE',  ( 0.7071067811865486830, -0.7071067811865464625, -0.000000000000000000 ) ) ;
#133275 = ORIENTED_EDGE ( 'NONE', *, *, #3543, .F. ) ;
#133276 = LINE ( 'NONE', #78173, #53740 ) ;
#133277 = LINE ( 'NONE', #90467, #88347 ) ;
#133278 = CARTESIAN_POINT ( 'NONE',  ( 81.72459685856476597, -1.637169565754160949, 6.109999999999997655 ) ) ;
#133279 = VECTOR ( 'NONE', #127313, 1000.000000000000000 ) ;
#133280 = ORIENTED_EDGE ( 'NONE', *, *, #112693, .F. ) ;
#133281 = EDGE_CURVE ( 'NONE', #4087, #27739, #116598, .T. ) ;
#133282 = CARTESIAN_POINT ( 'NONE',  ( 26.29289321881327623, 11.25929247661560773, 5.000000000000000000 ) ) ;
#133283 = LINE ( 'NONE', #98485, #42367 ) ;
#133284 = ORIENTED_EDGE ( 'NONE', *, *, #132882, .T. ) ;
#133285 = ORIENTED_EDGE ( 'NONE', *, *, #93534, .F. ) ;
#133286 = EDGE_CURVE ( 'NONE', #142768, #13302, #6353, .T. ) ;
#133287 = CARTESIAN_POINT ( 'NONE',  ( -34.49999999999975842, 16.77039438581775954, 0.4657186855308521056 ) ) ;
#133288 = ADVANCED_FACE ( 'NONE', ( #28885 ), #17960, .F. ) ;
#133289 = CARTESIAN_POINT ( 'NONE',  ( 21.65040314143522693, 7.934999999999988951, -2.126176841940961904 ) ) ;
#133290 = DIRECTION ( 'NONE',  ( 0.7071067811865487940, 0.7071067811865463515, -0.000000000000000000 ) ) ;
#133291 = CARTESIAN_POINT ( 'NONE',  ( -28.49999999999979039, 3.052185695429140200, 5.000000000000000000 ) ) ;
#133292 = VECTOR ( 'NONE', #33084, 1000.000000000000227 ) ;
#133293 = PLANE ( 'NONE',  #97318 ) ;
#133294 = PLANE ( 'NONE',  #96007 ) ;
#133295 = EDGE_CURVE ( 'NONE', #92540, #92320, #141192, .T. ) ;
#133296 = VECTOR ( 'NONE', #135229, 1000.000000000000000 ) ;
#133297 = ORIENTED_EDGE ( 'NONE', *, *, #137656, .F. ) ;
#133299 = VERTEX_POINT ( 'NONE', #54238 ) ;
#133298 = VECTOR ( 'NONE', #93578, 1000.000000000000000 ) ;
#133300 = EDGE_LOOP ( 'NONE', ( #129656, #93338, #139389, #69829 ) ) ;
#133301 = ORIENTED_EDGE ( 'NONE', *, *, #108060, .F. ) ;
#133302 = AXIS2_PLACEMENT_3D ( 'NONE', #65836, #19424, #142639 ) ;
#133303 = EDGE_CURVE ( 'NONE', #129197, #17080, #20119, .T. ) ;
#133305 = EDGE_CURVE ( 'NONE', #86591, #74065, #9213, .T. ) ;
#133304 = DIRECTION ( 'NONE',  ( -0.7071067811865486830, 0.7071067811865464625, 0.000000000000000000 ) ) ;
#133306 = ORIENTED_EDGE ( 'NONE', *, *, #59010, .F. ) ;
#133307 = CARTESIAN_POINT ( 'NONE',  ( 56.07919371712956291, 3.975000000000002753, -6.884901960086283523 ) ) ;
#133308 = CARTESIAN_POINT ( 'NONE',  ( 20.20519093902540320, 4.584330080086930965E-16, 0.000000000000000000 ) ) ;
#133309 = PLANE ( 'NONE',  #64212 ) ;
#133310 = CARTESIAN_POINT ( 'NONE',  ( 34.92499999999998295, 22.22500000000000142, 4.500000000000000888 ) ) ;
#133311 = CARTESIAN_POINT ( 'NONE',  ( 119.7083333333333286, -3.974999999999999201, -6.884901960086287964 ) ) ;
#133312 = ORIENTED_EDGE ( 'NONE', *, *, #57435, .T. ) ;
#133313 = DIRECTION ( 'NONE',  ( -1.000000000000000000, -0.000000000000000000, -0.000000000000000000 ) ) ;
#133314 = VERTEX_POINT ( 'NONE', #99843 ) ;
#133315 = DIRECTION ( 'NONE',  ( -0.3543493200069163240, 4.681814790819596721E-17, -0.9351131265310288487 ) ) ;
#133316 = VERTEX_POINT ( 'NONE', #54928 ) ;
#133317 = CARTESIAN_POINT ( 'NONE',  ( -44.99451991528749772, 28.92564299267969474, 4.000000000000000000 ) ) ;
#133318 = EDGE_CURVE ( 'NONE', #108418, #133114, #131015, .T. ) ;
#133319 = VERTEX_POINT ( 'NONE', #66516 ) ;
#133320 = DIRECTION ( 'NONE',  ( 0.7071067811865486830, -0.7071067811865464625, -0.000000000000000000 ) ) ;
#133321 = EDGE_LOOP ( 'NONE', ( #92498, #141456, #14865, #57292 ) ) ;
#133322 = ORIENTED_EDGE ( 'NONE', *, *, #129245, .T. ) ;
#133323 = EDGE_LOOP ( 'NONE', ( #10637, #115032, #98559, #90039 ) ) ;
#133324 = CARTESIAN_POINT ( 'NONE',  ( 66.29974487139159578, -27.71228299555252406, 4.000000000000000000 ) ) ;
#133325 = CARTESIAN_POINT ( 'NONE',  ( -12.70000000000000817, -1.739288537755694446E-15, -40.00000000000000000 ) ) ;
#133326 = LINE ( 'NONE', #142755, #79725 ) ;
#133327 = CARTESIAN_POINT ( 'NONE',  ( 119.2920968585647756, -5.291415217122921177, 3.054999999999999272 ) ) ;
#133328 = DIRECTION ( 'NONE',  ( 0.7071067811865487940, -0.7071067811865463515, 0.000000000000000000 ) ) ;
#133329 = DIRECTION ( 'NONE',  ( -0.3543493200069162685, -0.000000000000000000, -0.9351131265310288487 ) ) ;
#133330 = DIRECTION ( 'NONE',  ( -0.000000000000000000, 1.000000000000000000, 1.286409696682840916E-16 ) ) ;
#133331 = CARTESIAN_POINT ( 'NONE',  ( 20.51159235450331764, 9.902892378096218942E-16, 0.000000000000000000 ) ) ;
#133332 = ORIENTED_EDGE ( 'NONE', *, *, #111004, .F. ) ;
#133333 = LINE ( 'NONE', #36163, #39091 ) ;
#133334 = DIRECTION ( 'NONE',  ( 0.7071067811865487940, 0.7071067811865463515, -0.000000000000000000 ) ) ;
#133335 = EDGE_LOOP ( 'NONE', ( #97174, #108870, #26141, #79560 ) ) ;
#133336 = ORIENTED_EDGE ( 'NONE', *, *, #88541, .F. ) ;
#133337 = EDGE_CURVE ( 'NONE', #135646, #133878, #33205, .T. ) ;
#133338 = ORIENTED_EDGE ( 'NONE', *, *, #104332, .F. ) ;
#133339 = CARTESIAN_POINT ( 'NONE',  ( 42.18398860626899705, 28.73617430169816700, 5.000000000000000000 ) ) ;
#133340 = VERTEX_POINT ( 'NONE', #109996 ) ;
#133341 = VERTEX_POINT ( 'NONE', #74546 ) ;
#133342 = CARTESIAN_POINT ( 'NONE',  ( -23.99451991528749062, 28.92564299267954908, 4.000000000000000000 ) ) ;
#133343 = CARTESIAN_POINT ( 'NONE',  ( 15.21247294953710671, 0.000000000000000000, 6.094999999999989981 ) ) ;
#133344 = CARTESIAN_POINT ( 'NONE',  ( 28.55334942336764925, 2.259292476615690770, 14.86850063742347849 ) ) ;
#133345 = CARTESIAN_POINT ( 'NONE',  ( -8.292893218813400580, -6.740707523384218192, 5.000000000000000000 ) ) ;
#133346 = ORIENTED_EDGE ( 'NONE', *, *, #38911, .F. ) ;
#133347 = CARTESIAN_POINT ( 'NONE',  ( -50.99451991528749062, 28.92564299267973738, 4.000000000000000000 ) ) ;
#133348 = ORIENTED_EDGE ( 'NONE', *, *, #96638, .F. ) ;
#133349 = DIRECTION ( 'NONE',  ( 0.7071067811865486830, -0.7071067811865464625, -0.000000000000000000 ) ) ;
#133350 = AXIS2_PLACEMENT_3D ( 'NONE', #132425, #141853, #85284 ) ;
#133351 = ADVANCED_FACE ( 'NONE', ( #108535 ), #22252, .F. ) ;
#133352 = CARTESIAN_POINT ( 'NONE',  ( 20.48373647476854842, -5.808823158059035485, -5.808823158059033709 ) ) ;
#133353 = ORIENTED_EDGE ( 'NONE', *, *, #137906, .F. ) ;
#133354 = CARTESIAN_POINT ( 'NONE',  ( 84.05793019189810877, 6.110000000000001208, -1.637169565754156286 ) ) ;
#133355 = EDGE_CURVE ( 'NONE', #13056, #12477, #97699, .T. ) ;
#133356 = PLANE ( 'NONE',  #96775 ) ;
#133357 = VECTOR ( 'NONE', #126823, 999.9999999999998863 ) ;
#133358 = DIRECTION ( 'NONE',  ( -0.7071067811865487940, 0.7071067811865463515, -0.000000000000000000 ) ) ;
#133359 = VERTEX_POINT ( 'NONE', #30303 ) ;
#133360 = ORIENTED_EDGE ( 'NONE', *, *, #88034, .T. ) ;
#133361 = EDGE_CURVE ( 'NONE', #39023, #116419, #61468, .T. ) ;
#133362 = ORIENTED_EDGE ( 'NONE', *, *, #107788, .T. ) ;
#133363 = CARTESIAN_POINT ( 'NONE',  ( 19.05000000000000071, 3.174999999999997158, 4.000000000000000000 ) ) ;
#133364 = FACE_OUTER_BOUND ( 'NONE', #51420, .T. ) ;
#133365 = CARTESIAN_POINT ( 'NONE',  ( -8.816011393731004731, 28.73617430169781173, 5.000000000000000000 ) ) ;
#133366 = CARTESIAN_POINT ( 'NONE',  ( 10.49999999999992539, -15.29013452822853125, 0.3645803511610583580 ) ) ;
#133367 = ADVANCED_FACE ( 'NONE', ( #141953 ), #87543, .F. ) ;
#133368 = PLANE ( 'NONE',  #54231 ) ;
#133369 = EDGE_LOOP ( 'NONE', ( #126751, #53893, #82153 ) ) ;
#133370 = LINE ( 'NONE', #11536, #112916 ) ;
#133372 = EDGE_CURVE ( 'NONE', #125503, #19482, #21578, .T. ) ;
#133371 = VECTOR ( 'NONE', #13065, 1000.000000000000000 ) ;
#133373 = LINE ( 'NONE', #79744, #23430 ) ;
#133374 = DIRECTION ( 'NONE',  ( -1.000000000000000000, -0.000000000000000000, -0.000000000000000000 ) ) ;
#133375 = ORIENTED_EDGE ( 'NONE', *, *, #139142, .T. ) ;
#133376 = DIRECTION ( 'NONE',  ( -0.6830127018922181881, 0.6830127018922202975, -0.2588190451025214056 ) ) ;
#133377 = CARTESIAN_POINT ( 'NONE',  ( -56.99451991528749062, 28.92564299267978001, 4.000000000000000000 ) ) ;
#133378 = ORIENTED_EDGE ( 'NONE', *, *, #53574, .F. ) ;
#133379 = ADVANCED_FACE ( 'NONE', ( #99098 ), #31735, .F. ) ;
#133381 = ORIENTED_EDGE ( 'NONE', *, *, #121780, .F. ) ;
#133380 = CARTESIAN_POINT ( 'NONE',  ( 26.99999999999980105, -16.02097659208070368, -11.96015758381215477 ) ) ;
#133382 = ORIENTED_EDGE ( 'NONE', *, *, #131913, .T. ) ;
#133383 = EDGE_CURVE ( 'NONE', #67347, #21681, #120128, .T. ) ;
#133384 = DIRECTION ( 'NONE',  ( 0.6830127018922181881, 0.6830127018922202975, -0.2588190451025214056 ) ) ;
#133385 = CARTESIAN_POINT ( 'NONE',  ( -0.7928932188134494297, 3.759292476615678336, 5.000000000000000000 ) ) ;
#133386 = ORIENTED_EDGE ( 'NONE', *, *, #38912, .F. ) ;
#133387 = PLANE ( 'NONE',  #67553 ) ;
#133388 = UNCERTAINTY_MEASURE_WITH_UNIT (LENGTH_MEASURE( 1.000000000000000082E-05 ), #5955, 'distance_accuracy_value', 'NONE');
#133389 = EDGE_CURVE ( 'NONE', #70502, #91018, #109289, .T. ) ;
#133390 = FACE_OUTER_BOUND ( 'NONE', #28894, .T. ) ;
#133391 = VECTOR ( 'NONE', #67674, 1000.000000000000000 ) ;
#133392 = DIRECTION ( 'NONE',  ( -0.000000000000000000, 0.000000000000000000, 1.000000000000000000 ) ) ;
#133393 = DIRECTION ( 'NONE',  ( -0.7071067811865486830, -0.7071067811865464625, -0.000000000000000000 ) ) ;
#133395 = VECTOR ( 'NONE', #45721, 1000.000000000000000 ) ;
#133394 = CARTESIAN_POINT ( 'NONE',  ( 57.18398860626899705, 28.73617430169827358, 5.000000000000000000 ) ) ;
#133396 = FACE_OUTER_BOUND ( 'NONE', #80461, .T. ) ;
#133397 = LINE ( 'NONE', #97901, #95782 ) ;
#133398 = DIRECTION ( 'NONE',  ( -1.000000000000000000, -0.000000000000000000, -0.000000000000000000 ) ) ;
#133399 = CARTESIAN_POINT ( 'NONE',  ( 20.24956980810188867, 3.967499999999998916, 6.871911579029510442 ) ) ;
#133400 = DIRECTION ( 'NONE',  ( 0.3543493200069162685, -0.000000000000000000, -0.9351131265310288487 ) ) ;
#133401 = FACE_OUTER_BOUND ( 'NONE', #21705, .T. ) ;
#133402 = AXIS2_PLACEMENT_3D ( 'NONE', #58184, #69763, #103749 ) ;
#133403 = PLANE ( 'NONE',  #53493 ) ;
#133404 = LINE ( 'NONE', #54429, #112588 ) ;
#133405 = ORIENTED_EDGE ( 'NONE', *, *, #131759, .T. ) ;
#133406 = ORIENTED_EDGE ( 'NONE', *, *, #65445, .F. ) ;
#133407 = CARTESIAN_POINT ( 'NONE',  ( 105.5624999999999858, -5.819803920172572198, -5.819803920172573086 ) ) ;
#133408 = VERTEX_POINT ( 'NONE', #9972 ) ;
#133409 = ORIENTED_EDGE ( 'NONE', *, *, #116529, .F. ) ;
#133410 = EDGE_LOOP ( 'NONE', ( #5389, #82668, #56276, #126472 ) ) ;
#133411 = ADVANCED_FACE ( 'NONE', ( #52751 ), #118731, .T. ) ;
#133412 = DIRECTION ( 'NONE',  ( -1.000000000000000000, -1.224606353822377258E-16, -0.000000000000000000 ) ) ;
#133413 = PLANE ( 'NONE',  #118113 ) ;
#133414 = ORIENTED_EDGE ( 'NONE', *, *, #103934, .F. ) ;
#133415 = DIRECTION ( 'NONE',  ( 1.400468248933914810E-15, 0.9647414015272155474, -0.2631995976047525887 ) ) ;
#133416 = CARTESIAN_POINT ( 'NONE',  ( -4.499999999999968914, -12.66682484999667047, -0.6294897503864036459 ) ) ;
#133417 = CARTESIAN_POINT ( 'NONE',  ( 28.96659967656959722, 6.759292476615649470, 12.28218704918528736 ) ) ;
#133418 = CYLINDRICAL_SURFACE ( 'NONE', #51163, 2.500000000000000000 ) ;
#133419 = ORIENTED_EDGE ( 'NONE', *, *, #63952, .F. ) ;
#133420 = FACE_OUTER_BOUND ( 'NONE', #133954, .T. ) ;
#133421 = EDGE_CURVE ( 'NONE', #99639, #26527, #43333, .T. ) ;
#133422 = CARTESIAN_POINT ( 'NONE',  ( 25.39999999999999858, -1.600000000000094458, 34.92499999999998295 ) ) ;
#133423 = LINE ( 'NONE', #12331, #54540 ) ;
#133424 = CARTESIAN_POINT ( 'NONE',  ( 23.70025512860841133, -27.71228299555189523, 4.000000000000000000 ) ) ;
#133425 = DIRECTION ( 'NONE',  ( -1.000000000000000000, -0.000000000000000000, -0.000000000000000000 ) ) ;
#133426 = DIRECTION ( 'NONE',  ( -0.7071067811865486830, -0.7071067811865464625, 0.000000000000000000 ) ) ;
#133427 = EDGE_CURVE ( 'NONE', #129470, #42524, #32459, .T. ) ;
#133428 = DIRECTION ( 'NONE',  ( 1.000000000000000000, 0.000000000000000000, 0.000000000000000000 ) ) ;
#133429 = ORIENTED_EDGE ( 'NONE', *, *, #142582, .T. ) ;
#133430 = EDGE_LOOP ( 'NONE', ( #60186, #1959, #13931, #81043, #54123 ) ) ;
#133431 = CARTESIAN_POINT ( 'NONE',  ( 117.6879301918981184, 6.110000000000002984, -1.637169565754156730 ) ) ;
#133432 = ORIENTED_EDGE ( 'NONE', *, *, #81364, .F. ) ;
#133433 = EDGE_CURVE ( 'NONE', #124008, #24896, #58544, .T. ) ;
#133434 = DIRECTION ( 'NONE',  ( 0.000000000000000000, 0.000000000000000000, -1.000000000000000000 ) ) ;
#133435 = AXIS2_PLACEMENT_3D ( 'NONE', #22130, #66384, #55510 ) ;
#133436 = DIRECTION ( 'NONE',  ( 0.7071067811865487940, 0.7071067811865463515, 0.000000000000000000 ) ) ;
#133437 = DIRECTION ( 'NONE',  ( -0.7071067811865486830, -0.7071067811865464625, -0.000000000000000000 ) ) ;
#133438 = CARTESIAN_POINT ( 'NONE',  ( 3.328169399223508851, -12.74070752338415247, 4.000000000000000000 ) ) ;
#133439 = CARTESIAN_POINT ( 'NONE',  ( 114.8287635252314516, 0.000000000000000000, -6.109999999999998543 ) ) ;
#133440 = ORIENTED_EDGE ( 'NONE', *, *, #9139, .T. ) ;
#133441 = ADVANCED_FACE ( 'NONE', ( #46949 ), #41970, .F. ) ;
#133442 = ORIENTED_EDGE ( 'NONE', *, *, #60958, .F. ) ;
#133443 = AXIS2_PLACEMENT_3D ( 'NONE', #127879, #59764, #93088 ) ;
#133444 = CARTESIAN_POINT ( 'NONE',  ( 25.39999999999999858, -57.15000000000003411, -15.92500000000064730 ) ) ;
#133445 = PLANE ( 'NONE',  #33949 ) ;
#133446 =( BOUNDED_CURVE ( )  B_SPLINE_CURVE ( 3, ( #52270, #141428, #96455, #118951 ),
 .UNSPECIFIED., .F., .T. ) 
 B_SPLINE_CURVE_WITH_KNOTS ( ( 4, 4 ),
 ( 4.874499669516390910, 4.920172610314182293 ),
 .UNSPECIFIED. ) 
 CURVE ( )  GEOMETRIC_REPRESENTATION_ITEM ( )  RATIONAL_B_SPLINE_CURVE ( ( 1.000000000000000000, 0.9998261727610758820, 0.9998261727610758820, 1.000000000000000000 ) ) 
 REPRESENTATION_ITEM ( '' )  );
#133447 = ORIENTED_EDGE ( 'NONE', *, *, #96086, .F. ) ;
#133448 = VERTEX_POINT ( 'NONE', #59928 ) ;
#133449 = CARTESIAN_POINT ( 'NONE',  ( 39.52126352523143282, -4.472830434245839371, -4.472830434245840259 ) ) ;
#133450 = EDGE_CURVE ( 'NONE', #14639, #54134, #138917, .T. ) ;
#133451 = VERTEX_POINT ( 'NONE', #92515 ) ;
#133452 = DIRECTION ( 'NONE',  ( -0.7071067811865477948, 0.000000000000000000, 0.7071067811865473507 ) ) ;
#133453 = CARTESIAN_POINT ( 'NONE',  ( -9.524999999999991473, -4.870000000000014317, -10.00000000000000178 ) ) ;
#133454 = CARTESIAN_POINT ( 'NONE',  ( 15.48921356237309510, -27.52281430457066236, 5.000000000000000000 ) ) ;
#133455 = AXIS2_PLACEMENT_3D ( 'NONE', #1830, #46133, #134566 ) ;
#133456 = CARTESIAN_POINT ( 'NONE',  ( 28.78709685856477307, 3.054999999999997495, 5.291415217122919401 ) ) ;
#133457 = ORIENTED_EDGE ( 'NONE', *, *, #9325, .F. ) ;
#133458 = AXIS2_PLACEMENT_3D ( 'NONE', #72340, #4836, #93327 ) ;
#133459 = VERTEX_POINT ( 'NONE', #128049 ) ;
#133460 = ORIENTED_EDGE ( 'NONE', *, *, #138082, .T. ) ;
#133461 = VERTEX_POINT ( 'NONE', #104095 ) ;
#133462 = CARTESIAN_POINT ( 'NONE',  ( 0.2100385299584282828, 0.4000000000000001332, -2.083955186700111817 ) ) ;
#133463 = FACE_OUTER_BOUND ( 'NONE', #52708, .T. ) ;
#133464 = EDGE_CURVE ( 'NONE', #102488, #17773, #71512, .T. ) ;
#133465 = ORIENTED_EDGE ( 'NONE', *, *, #15132, .T. ) ;
#133466 = LINE ( 'NONE', #56661, #110756 ) ;
#133467 = VECTOR ( 'NONE', #32381, 1000.000000000000000 ) ;
#133468 = DIRECTION ( 'NONE',  ( 1.000000000000000000, 0.000000000000000000, 0.000000000000000000 ) ) ;
#133469 = LINE ( 'NONE', #21121, #85974 ) ;
#133470 = EDGE_CURVE ( 'NONE', #123427, #97084, #49054, .T. ) ;
#133472 = FACE_BOUND ( 'NONE', #130867, .T. ) ;
#133471 = VECTOR ( 'NONE', #25736, 999.9999999999998863 ) ;
#133473 = VERTEX_POINT ( 'NONE', #115674 ) ;
#133474 = PLANE ( 'NONE',  #87408 ) ;
#133475 = FACE_OUTER_BOUND ( 'NONE', #4734, .T. ) ;
#133476 = CARTESIAN_POINT ( 'NONE',  ( 21.48921356237309155, -27.52281430457070499, 5.000000000000000000 ) ) ;
#133478 = ADVANCED_FACE ( 'NONE', ( #128734 ), #17806, .F. ) ;
#133477 = CARTESIAN_POINT ( 'NONE',  ( 18.00548008471250583, 28.92564299267925776, 4.000000000000000000 ) ) ;
#133479 = ORIENTED_EDGE ( 'NONE', *, *, #113073, .T. ) ;
#133480 = PLANE ( 'NONE',  #142984 ) ;
#133481 = VERTEX_POINT ( 'NONE', #28002 ) ;
#133482 = EDGE_LOOP ( 'NONE', ( #36610, #139794, #11115, #40314 ) ) ;
#133483 = VECTOR ( 'NONE', #6609, 1000.000000000000000 ) ;
#133484 = ORIENTED_EDGE ( 'NONE', *, *, #55288, .F. ) ;
#133485 = VECTOR ( 'NONE', #55362, 1000.000000000000000 ) ;
#133486 = VECTOR ( 'NONE', #36271, 1000.000000000000227 ) ;
#133487 = CARTESIAN_POINT ( 'NONE',  ( 50.95376352523145158, -6.109999999999998543, -3.741295971395162543E-16 ) ) ;
#133488 = ORIENTED_EDGE ( 'NONE', *, *, #124996, .T. ) ;
#133489 = FACE_OUTER_BOUND ( 'NONE', #85324, .T. ) ;
#133490 =( NAMED_UNIT ( * ) SI_UNIT ( $, .STERADIAN. ) SOLID_ANGLE_UNIT ( ) );
#133491 = VERTEX_POINT ( 'NONE', #38875 ) ;
#133492 = CARTESIAN_POINT ( 'NONE',  ( -15.00548008471250228, 28.92564299267927552, 4.000000000000000000 ) ) ;
#133493 = AXIS2_PLACEMENT_3D ( 'NONE', #78855, #24446, #36065 ) ;
#133494 = EDGE_CURVE ( 'NONE', #55424, #126070, #127299, .T. ) ;
#133495 = DIRECTION ( 'NONE',  ( -0.7071067811865487940, 0.7071067811865463515, -0.000000000000000000 ) ) ;
#133496 = DIRECTION ( 'NONE',  ( -0.6830127018922181881, 0.6830127018922202975, -0.2588190451025214056 ) ) ;
#133497 = DIRECTION ( 'NONE',  ( -1.000000000000000000, 0.000000000000000000, -0.000000000000000000 ) ) ;
#133498 = CARTESIAN_POINT ( 'NONE',  ( -6.707106781186485733, -12.74070752338415602, 5.000000000000000000 ) ) ;
#133499 = DIRECTION ( 'NONE',  ( 0.7071067811865486830, -0.7071067811865464625, -0.000000000000000000 ) ) ;
#133500 = ORIENTED_EDGE ( 'NONE', *, *, #15131, .T. ) ;
#133501 = ORIENTED_EDGE ( 'NONE', *, *, #116652, .F. ) ;
#133502 = ORIENTED_EDGE ( 'NONE', *, *, #4660, .F. ) ;
#133503 = ORIENTED_EDGE ( 'NONE', *, *, #101625, .T. ) ;
#133504 = LINE ( 'NONE', #134221, #42716 ) ;
#133505 = LINE ( 'NONE', #76271, #51387 ) ;
#133506 = VERTEX_POINT ( 'NONE', #50473 ) ;
#133507 = ORIENTED_EDGE ( 'NONE', *, *, #90558, .F. ) ;
#133508 = CARTESIAN_POINT ( 'NONE',  ( -14.99999999999988454, -10.44781430457071814, 5.000000000000000000 ) ) ;
#133509 = DIRECTION ( 'NONE',  ( -0.7071067811865486830, 0.7071067811865464625, 0.000000000000000000 ) ) ;
#133510 = DIRECTION ( 'NONE',  ( -0.000000000000000000, -0.000000000000000000, 1.000000000000000000 ) ) ;
#133511 = ORIENTED_EDGE ( 'NONE', *, *, #106476, .F. ) ;
#133512 = LINE ( 'NONE', #34200, #48670 ) ;
#133513 = DIRECTION ( 'NONE',  ( -0.000000000000000000, 0.3543493200069153248, 0.9351131265310292928 ) ) ;
#133514 = CARTESIAN_POINT ( 'NONE',  ( 29.23373647476855552, 5.808823158059036373, 5.808823158059032821 ) ) ;
#133515 = EDGE_CURVE ( 'NONE', #123567, #141805, #6196, .T. ) ;
#133516 = VECTOR ( 'NONE', #23099, 1000.000000000000000 ) ;
#133517 = LINE ( 'NONE', #89, #64366 ) ;
#133518 = EDGE_LOOP ( 'NONE', ( #129834, #47354, #110941, #70282 ) ) ;
#133519 = CARTESIAN_POINT ( 'NONE',  ( 113.8079301918981230, -6.109999999999999432, 1.637169565754158507 ) ) ;
#133520 = ADVANCED_FACE ( 'NONE', ( #51192 ), #93959, .F. ) ;
#133521 = DIRECTION ( 'NONE',  ( 1.000000000000000000, 0.000000000000000000, 0.000000000000000000 ) ) ;
#133522 = CARTESIAN_POINT ( 'NONE',  ( -15.18398860626900237, 28.73617430169797871, 5.000000000000000000 ) ) ;
#133523 = DIRECTION ( 'NONE',  ( 0.3543493200069164351, 2.781805975412904658E-17, -0.9351131265310288487 ) ) ;
#133525 = ORIENTED_EDGE ( 'NONE', *, *, #46240, .T. ) ;
#133524 = LINE ( 'NONE', #77722, #75021 ) ;
#133526 = VECTOR ( 'NONE', #47875, 999.9999999999998863 ) ;
#133527 = PLANE ( 'NONE',  #64854 ) ;
#133528 = VERTEX_POINT ( 'NONE', #106235 ) ;
#133529 = DIRECTION ( 'NONE',  ( -0.3543493200069162685, -0.000000000000000000, -0.9351131265310288487 ) ) ;
#133530 = DIRECTION ( 'NONE',  ( 0.3543493200069162685, -0.000000000000000000, -0.9351131265310288487 ) ) ;
#133531 = ADVANCED_FACE ( 'NONE', ( #48319 ), #117824, .F. ) ;
#133532 = EDGE_CURVE ( 'NONE', #32577, #30830, #73649, .T. ) ;
#133533 = DIRECTION ( 'NONE',  ( -1.000000000000000000, -1.224606353822377258E-16, -0.000000000000000000 ) ) ;
#133534 = ORIENTED_EDGE ( 'NONE', *, *, #82592, .F. ) ;
#133535 = CARTESIAN_POINT ( 'NONE',  ( 24.56840764549667355, 0.000000000000000000, 2.500000000000001332 ) ) ;
#133536 = LINE ( 'NONE', #90003, #23312 ) ;
#133537 = CARTESIAN_POINT ( 'NONE',  ( -14.99451991528749595, 28.92564299267948513, 4.000000000000000000 ) ) ;
#133538 = VECTOR ( 'NONE', #45866, 1000.000000000000227 ) ;
#133539 = VERTEX_POINT ( 'NONE', #28731 ) ;
#133540 = CARTESIAN_POINT ( 'NONE',  ( -4.499999999999968914, 0.4497235411627387158, -5.599840258123551351 ) ) ;
#133541 = ORIENTED_EDGE ( 'NONE', *, *, #94394, .F. ) ;
#133542 = ADVANCED_FACE ( 'NONE', ( #72973 ), #95388, .T. ) ;
#133543 = CARTESIAN_POINT ( 'NONE',  ( 34.49999999999975131, 16.18958161055405753, -11.56426086740803427 ) ) ;
#133544 = VECTOR ( 'NONE', #54494, 1000.000000000000227 ) ;
#133546 = EDGE_LOOP ( 'NONE', ( #111275, #95077, #25762, #45471, #77512, #35455 ) ) ;
#133545 = DIRECTION ( 'NONE',  ( 1.000000000000000000, 1.224606353822377258E-16, 0.000000000000000000 ) ) ;
#133547 = ADVANCED_FACE ( 'NONE', ( #106974 ), #26570, .F. ) ;
#133548 = ORIENTED_EDGE ( 'NONE', *, *, #121299, .F. ) ;
#133549 = DIRECTION ( 'NONE',  ( 0.7071067811865487940, 0.7071067811865463515, -0.000000000000000000 ) ) ;
#133550 = CARTESIAN_POINT ( 'NONE',  ( 31.49999999999977973, -13.91253812416061386, 4.000000000000000000 ) ) ;
#133551 = ORIENTED_EDGE ( 'NONE', *, *, #130, .F. ) ;
#133552 = EDGE_CURVE ( 'NONE', #67920, #86102, #125897, .T. ) ;
#133553 = VECTOR ( 'NONE', #121868, 1000.000000000000000 ) ;
#133554 = DIRECTION ( 'NONE',  ( -0.7071067811865487940, 0.7071067811865463515, -0.000000000000000000 ) ) ;
#133555 = LINE ( 'NONE', #25475, #4340 ) ;
#133556 = DIRECTION ( 'NONE',  ( 0.000000000000000000, -1.000000000000000000, 0.000000000000000000 ) ) ;
#133557 = AXIS2_PLACEMENT_3D ( 'NONE', #82301, #17707, #72887 ) ;
#133558 = ORIENTED_EDGE ( 'NONE', *, *, #80871, .F. ) ;
#133559 = DIRECTION ( 'NONE',  ( 0.7071067811865487940, -0.7071067811865463515, 0.000000000000000000 ) ) ;
#133561 = VECTOR ( 'NONE', #32862, 1000.000000000000000 ) ;
#133560 = DIRECTION ( 'NONE',  ( -0.7071067811865486830, -0.7071067811865464625, 0.000000000000000000 ) ) ;
#133562 = CARTESIAN_POINT ( 'NONE',  ( 1.499999999999997780, 7.087461875839172087, 4.000000000000000000 ) ) ;
#133563 = EDGE_CURVE ( 'NONE', #56577, #63324, #38394, .T. ) ;
#133564 = CARTESIAN_POINT ( 'NONE',  ( 126.1802896944664525, -7.122564593600495542, 1.486291407750432114 ) ) ;
#133565 = CARTESIAN_POINT ( 'NONE',  ( 32.28709685856477307, 3.054999999999997939, 5.291415217122920289 ) ) ;
#133566 = DIRECTION ( 'NONE',  ( 0.000000000000000000, -1.000000000000000000, 0.000000000000000000 ) ) ;
#133567 = ORIENTED_EDGE ( 'NONE', *, *, #116128, .F. ) ;
#133568 = ORIENTED_EDGE ( 'NONE', *, *, #122719, .T. ) ;
#133569 = CARTESIAN_POINT ( 'NONE',  ( -38.99451991528749062, 28.92564299267965211, 4.000000000000000000 ) ) ;
#133570 = ORIENTED_EDGE ( 'NONE', *, *, #55162, .F. ) ;
#133571 = VERTEX_POINT ( 'NONE', #97524 ) ;
#133572 = ORIENTED_EDGE ( 'NONE', *, *, #41427, .F. ) ;
#133573 = ADVANCED_FACE ( 'NONE', ( #22100 ), #31576, .T. ) ;
#133574 = PLANE ( 'NONE',  #128970 ) ;
#133575 = DIRECTION ( 'NONE',  ( -0.7071067811865487940, 0.7071067811865463515, -0.000000000000000000 ) ) ;
#133576 = ORIENTED_EDGE ( 'NONE', *, *, #75218, .T. ) ;
#133577 = CARTESIAN_POINT ( 'NONE',  ( -21.29974487139158512, -27.71228299555221142, 4.000000000000000000 ) ) ;
#133578 = CARTESIAN_POINT ( 'NONE',  ( 28.49999999999980105, 8.900465351122175406, -2.516491619111579592 ) ) ;
#133579 = LINE ( 'NONE', #883, #69475 ) ;
#133580 = VECTOR ( 'NONE', #64439, 1000.000000000000227 ) ;
#133581 = CARTESIAN_POINT ( 'NONE',  ( 39.18398860626899705, 28.73617430169814568, 5.000000000000000000 ) ) ;
#133582 = CARTESIAN_POINT ( 'NONE',  ( 121.3337635252314328, 6.110000000000001208, 1.122388791418549305E-15 ) ) ;
#133583 = VERTEX_POINT ( 'NONE', #54766 ) ;
#133584 = EDGE_CURVE ( 'NONE', #56805, #104812, #109839, .T. ) ;
#133585 = CARTESIAN_POINT ( 'NONE',  ( -22.64175702458846828, 15.75929247661555088, 19.34181609438704541 ) ) ;
#133586 = CARTESIAN_POINT ( 'NONE',  ( -57.18398860626899705, 28.73617430169827358, 5.000000000000000000 ) ) ;
#133587 = CARTESIAN_POINT ( 'NONE',  ( -11.27718569542934191, -21.72500000000000853, 5.000000000000000000 ) ) ;
#133588 = CARTESIAN_POINT ( 'NONE',  ( -13.49999999999990763, -1.533600742197719580, 5.000000000000000000 ) ) ;
#133589 = PLANE ( 'NONE',  #31222 ) ;
#133590 = VECTOR ( 'NONE', #118460, 1000.000000000000000 ) ;
#133591 = CARTESIAN_POINT ( 'NONE',  ( -25.39999999999996305, 0.000000000000000000, 2.500000000000000000 ) ) ;
#133592 = DIRECTION ( 'NONE',  ( -1.000000000000000000, -1.224606353822377258E-16, -0.000000000000000000 ) ) ;
#133593 = AXIS2_PLACEMENT_3D ( 'NONE', #18782, #60932, #95637 ) ;
#133594 = CARTESIAN_POINT ( 'NONE',  ( 44.85002705046287730, -5.819803920172572198, -5.819803920172572198 ) ) ;
#133595 = EDGE_CURVE ( 'NONE', #91203, #50701, #64206, .T. ) ;
#133596 = FACE_OUTER_BOUND ( 'NONE', #31068, .T. ) ;
#133597 = VECTOR ( 'NONE', #9645, 1000.000000000000000 ) ;
#133598 = LINE ( 'NONE', #45887, #39215 ) ;
#133599 = EDGE_LOOP ( 'NONE', ( #65176, #54682, #141957, #3612 ) ) ;
#133600 = VERTEX_POINT ( 'NONE', #98262 ) ;
#133601 = CARTESIAN_POINT ( 'NONE',  ( 42.41666666666665719, -6.884901960086287076, -3.975000000000000977 ) ) ;
#133602 = DIRECTION ( 'NONE',  ( -1.000000000000000000, -1.224606353822377258E-16, -0.000000000000000000 ) ) ;
#133603 = VECTOR ( 'NONE', #19475, 1000.000000000000000 ) ;
#133605 = CARTESIAN_POINT ( 'NONE',  ( 45.48921356237309510, -27.52281430457087197, 5.000000000000000000 ) ) ;
#133604 = AXIS2_PLACEMENT_3D ( 'NONE', #87947, #77108, #87240 ) ;
#133606 = ORIENTED_EDGE ( 'NONE', *, *, #39422, .T. ) ;
#133607 = DIRECTION ( 'NONE',  ( 0.6830127018922180770, -0.6830127018922202975, -0.2588190451025213501 ) ) ;
#133608 = LINE ( 'NONE', #37131, #127979 ) ;
#133609 = CARTESIAN_POINT ( 'NONE',  ( 42.00043019189809712, -3.055000000000002380, 5.291415217122920289 ) ) ;
#133610 = ORIENTED_EDGE ( 'NONE', *, *, #126365, .T. ) ;
#133611 = CARTESIAN_POINT ( 'NONE',  ( -34.47516574401890210, -4.509482387884336418, 4.998110765256836174 ) ) ;
#133612 = EDGE_LOOP ( 'NONE', ( #24386, #115324, #17099, #29120 ) ) ;
#133613 = ORIENTED_EDGE ( 'NONE', *, *, #13037, .F. ) ;
#133614 = CARTESIAN_POINT ( 'NONE',  ( -39.18398860626899705, 28.73617430169814568, 5.000000000000000000 ) ) ;
#133615 = LINE ( 'NONE', #34290, #38389 ) ;
#133616 = CARTESIAN_POINT ( 'NONE',  ( -42.29974487139158157, -27.71228299555235708, 4.000000000000000000 ) ) ;
#133617 = ORIENTED_EDGE ( 'NONE', *, *, #99935, .T. ) ;
#133618 = DIRECTION ( 'NONE',  ( -0.000000000000000000, -0.000000000000000000, 1.000000000000000000 ) ) ;
#133619 = ORIENTED_EDGE ( 'NONE', *, *, #56688, .T. ) ;
#133620 = CARTESIAN_POINT ( 'NONE',  ( -42.18398860626899705, 28.73617430169816700, 5.000000000000000000 ) ) ;
#133621 = LINE ( 'NONE', #90847, #18373 ) ;
#133622 = CARTESIAN_POINT ( 'NONE',  ( -39.48921356237310221, -27.52281430457082934, 5.000000000000000000 ) ) ;
#133623 = CARTESIAN_POINT ( 'NONE',  ( 1.629999999999999893, 0.4000000000000001887, -2.303088455023527104 ) ) ;
#133624 = VECTOR ( 'NONE', #1170, 1000.000000000000227 ) ;
#133625 = LINE ( 'NONE', #138434, #25389 ) ;
#133626 =( BOUNDED_CURVE ( )  B_SPLINE_CURVE ( 3, ( #118385, #55303, #53892, #86506 ),
 .UNSPECIFIED., .F., .T. ) 
 B_SPLINE_CURVE_WITH_KNOTS ( ( 4, 4 ),
 ( 5.043186909253423167, 5.074607125596354074 ),
 .UNSPECIFIED. ) 
 CURVE ( )  GEOMETRIC_REPRESENTATION_ITEM ( )  RATIONAL_B_SPLINE_CURVE ( ( 1.000000000000000000, 0.9999177325257868620, 0.9999177325257868620, 1.000000000000000000 ) ) 
 REPRESENTATION_ITEM ( '' )  );
#133627 = ORIENTED_EDGE ( 'NONE', *, *, #20937, .T. ) ;
#133628 = VECTOR ( 'NONE', #88883, 1000.000000000000000 ) ;
#133629 = FACE_OUTER_BOUND ( 'NONE', #116038, .T. ) ;
#133630 = CARTESIAN_POINT ( 'NONE',  ( 62.18293019189812298, -1.637169565754158951, -6.109999999999998543 ) ) ;
#133631 = DIRECTION ( 'NONE',  ( 0.000000000000000000, -1.000000000000000000, 0.000000000000000000 ) ) ;
#133632 = LINE ( 'NONE', #123494, #91757 ) ;
#133633 = CARTESIAN_POINT ( 'NONE',  ( 0.000000000000000000, 0.000000000000000000, 5.000000000000000000 ) ) ;
#133634 = ADVANCED_FACE ( 'NONE', ( #8346 ), #129440, .F. ) ;
#133635 = ORIENTED_EDGE ( 'NONE', *, *, #16007, .T. ) ;
#133636 = CARTESIAN_POINT ( 'NONE',  ( 26.43999999999999773, 2.055000000000001492, 0.000000000000000000 ) ) ;
#133637 =( LENGTH_UNIT ( ) NAMED_UNIT ( * ) SI_UNIT ( .MILLI., .METRE. ) );
#133638 = ORIENTED_EDGE ( 'NONE', *, *, #80303, .F. ) ;
#133639 = CARTESIAN_POINT ( 'NONE',  ( 17.99999999999986855, 7.007997736742456851, -8.085015511992068582 ) ) ;
#133640 = ORIENTED_EDGE ( 'NONE', *, *, #96489, .T. ) ;
#133641 = FACE_OUTER_BOUND ( 'NONE', #22611, .T. ) ;
#133642 = CARTESIAN_POINT ( 'NONE',  ( 21.18398860626899349, 28.73617430169802134, 5.000000000000000000 ) ) ;
#133643 = VECTOR ( 'NONE', #65136, 1000.000000000000227 ) ;
#133644 = DIRECTION ( 'NONE',  ( 1.000000000000000000, 0.000000000000000000, 0.000000000000000000 ) ) ;
#133645 = CARTESIAN_POINT ( 'NONE',  ( 32.99999999999977973, -0.4125381241607516403, 4.000000000000000000 ) ) ;
#133646 = EDGE_CURVE ( 'NONE', #138878, #93773, #19265, .T. ) ;
#133647 = FACE_BOUND ( 'NONE', #5217, .T. ) ;
#133648 = DIRECTION ( 'NONE',  ( -0.6830127018922180770, -0.6830127018922204085, -0.2588190451025213501 ) ) ;
#133649 = CARTESIAN_POINT ( 'NONE',  ( -66.29974487139159578, -27.71228299555252406, 4.000000000000000000 ) ) ;
#133650 = EDGE_CURVE ( 'NONE', #11420, #12388, #86679, .T. ) ;
#133651 = CARTESIAN_POINT ( 'NONE',  ( 11.99999999999992006, -4.068876922607777225, 4.000000000000000000 ) ) ;
#133653 = ORIENTED_EDGE ( 'NONE', *, *, #109605, .F. ) ;
#133652 = FACE_OUTER_BOUND ( 'NONE', #59360, .T. ) ;
#133654 = DIRECTION ( 'NONE',  ( -0.6830127018922180770, -0.6830127018922204085, -0.2588190451025213501 ) ) ;
#133655 = ORIENTED_EDGE ( 'NONE', *, *, #71559, .T. ) ;
#133656 = ORIENTED_EDGE ( 'NONE', *, *, #115636, .F. ) ;
#133657 = CARTESIAN_POINT ( 'NONE',  ( 79.24543019189810877, -5.291415217122918513, -3.055000000000000160 ) ) ;
#133658 = ORIENTED_EDGE ( 'NONE', *, *, #88831, .F. ) ;
#133659 = VECTOR ( 'NONE', #32005, 1000.000000000000000 ) ;
#133660 = ADVANCED_FACE ( 'NONE', ( #140330 ), #109118, .F. ) ;
#133661 = DIRECTION ( 'NONE',  ( 0.7071067811865486830, -0.7071067811865464625, -0.000000000000000000 ) ) ;
#133662 = ORIENTED_EDGE ( 'NONE', *, *, #88842, .F. ) ;
#133663 = CARTESIAN_POINT ( 'NONE',  ( -39.18398860626899705, 28.73617430169814568, 5.000000000000000000 ) ) ;
#133664 = ADVANCED_FACE ( 'NONE', ( #66357 ), #20675, .F. ) ;
#133665 = FACE_OUTER_BOUND ( 'NONE', #22360, .T. ) ;
#133666 = CYLINDRICAL_SURFACE ( 'NONE', #80796, 2.500000000000000444 ) ;
#133667 = LINE ( 'NONE', #134387, #61756 ) ;
#133668 = CARTESIAN_POINT ( 'NONE',  ( 1.516262732464673579, 0.3999999999999995226, 2.467792535850613866 ) ) ;
#133669 = DIRECTION ( 'NONE',  ( -0.7071067811865486830, -0.7071067811865464625, 0.000000000000000000 ) ) ;
#133670 = LINE ( 'NONE', #78575, #60939 ) ;
#133671 = FACE_OUTER_BOUND ( 'NONE', #40930, .T. ) ;
#133672 = ORIENTED_EDGE ( 'NONE', *, *, #72838, .F. ) ;
#133673 = EDGE_CURVE ( 'NONE', #26241, #3326, #77252, .T. ) ;
#133674 = EDGE_CURVE ( 'NONE', #18494, #11065, #51911, .T. ) ;
#133675 = ORIENTED_EDGE ( 'NONE', *, *, #55838, .T. ) ;
#133676 = LINE ( 'NONE', #44562, #118414 ) ;
#133677 = ORIENTED_EDGE ( 'NONE', *, *, #67931, .T. ) ;
#133678 = ORIENTED_EDGE ( 'NONE', *, *, #43942, .T. ) ;
#133680 = ORIENTED_EDGE ( 'NONE', *, *, #111958, .T. ) ;
#133679 = AXIS2_PLACEMENT_3D ( 'NONE', #75873, #99022, #43252 ) ;
#133681 = CARTESIAN_POINT ( 'NONE',  ( 28.14626352523143638, -4.472830434245840259, 4.472830434245838482 ) ) ;
#133682 = ORIENTED_EDGE ( 'NONE', *, *, #45362, .T. ) ;
#133683 = DIRECTION ( 'NONE',  ( -0.6830127018922181881, 0.6830127018922202975, -0.2588190451025214056 ) ) ;
#133684 = CIRCLE ( 'NONE', #103531, 2.055000000000000160 ) ;
#133685 = VECTOR ( 'NONE', #132960, 1000.000000000000227 ) ;
#133686 = FILL_AREA_STYLE ('',( #89452 ) ) ;
#133687 = STYLED_ITEM ( 'NONE', ( #15870 ), #110241 ) ;
#133688 = CARTESIAN_POINT ( 'NONE',  ( -1.828763525231447584, 0.000000000000000000, 7.934999999999990727 ) ) ;
#133689 = CARTESIAN_POINT ( 'NONE',  ( 17.49525436401519229, 4.684374302865251138, -29.47233687491770482 ) ) ;
#133690 = EDGE_LOOP ( 'NONE', ( #20770, #111243, #31734, #104483 ) ) ;
#133691 = CARTESIAN_POINT ( 'NONE',  ( 6.005480084712508493, 28.92564299267933947, 4.000000000000000000 ) ) ;
#133692 = EDGE_CURVE ( 'NONE', #15110, #84993, #143180, .T. ) ;
#133693 = DIRECTION ( 'NONE',  ( -0.7071067811865486830, -0.7071067811865464625, -0.000000000000000000 ) ) ;
#133694 = AXIS2_PLACEMENT_3D ( 'NONE', #31277, #121637, #79646 ) ;
#133695 = CARTESIAN_POINT ( 'NONE',  ( 23.99451991528749062, 28.92564299267954908, 4.000000000000000000 ) ) ;
#133697 = ORIENTED_EDGE ( 'NONE', *, *, #101538, .F. ) ;
#133696 = CARTESIAN_POINT ( 'NONE',  ( -69.29974487139159578, -27.71228299555254537, 4.000000000000000000 ) ) ;
#133698 = EDGE_LOOP ( 'NONE', ( #63555, #26674, #31104, #36473 ) ) ;
#133699 =( LENGTH_UNIT ( ) NAMED_UNIT ( * ) SI_UNIT ( .MILLI., .METRE. ) );
#133700 = CARTESIAN_POINT ( 'NONE',  ( -11.99999999999991651, -8.731860332648849976, -2.120594902707566565 ) ) ;
#133701 = ADVANCED_FACE ( 'NONE', ( #21413 ), #126435, .F. ) ;
#133702 = EDGE_CURVE ( 'NONE', #46893, #42124, #37087, .T. ) ;
#133703 = LINE ( 'NONE', #91616, #5426 ) ;
#133704 = ORIENTED_EDGE ( 'NONE', *, *, #115987, .F. ) ;
#133705 = DIRECTION ( 'NONE',  ( 0.7071067811865486830, -0.7071067811865464625, -0.000000000000000000 ) ) ;
#133706 = PLANE ( 'NONE',  #29389 ) ;
#133707 = ORIENTED_EDGE ( 'NONE', *, *, #7742, .T. ) ;
#133708 = DIRECTION ( 'NONE',  ( 0.000000000000000000, 0.000000000000000000, 1.000000000000000000 ) ) ;
#133709 = FILL_AREA_STYLE ('',( #113349 ) ) ;
#133710 = CARTESIAN_POINT ( 'NONE',  ( 60.18398860626900415, 28.73617430169829490, 5.000000000000000000 ) ) ;
#133711 = DIRECTION ( 'NONE',  ( -0.6830127018922181881, 0.6830127018922202975, -0.2588190451025214056 ) ) ;
#133712 = EDGE_CURVE ( 'NONE', #47325, #22051, #91490, .T. ) ;
#133713 = DIRECTION ( 'NONE',  ( 1.734723475976806848E-16, -1.000000000000000000, 0.000000000000000000 ) ) ;
#133714 = LINE ( 'NONE', #66323, #7464 ) ;
#133715 = LINE ( 'NONE', #3174, #77213 ) ;
#133716 = ADVANCED_FACE ( 'NONE', ( #70491 ), #338, .T. ) ;
#133717 = DIRECTION ( 'NONE',  ( -0.000000000000000000, 0.3543493200069153248, 0.9351131265310292928 ) ) ;
#133718 = ORIENTED_EDGE ( 'NONE', *, *, #91294, .F. ) ;
#133719 = EDGE_CURVE ( 'NONE', #143089, #11916, #26893, .T. ) ;
#133720 = ORIENTED_EDGE ( 'NONE', *, *, #106030, .F. ) ;
#133721 = VECTOR ( 'NONE', #90166, 1000.000000000000000 ) ;
#133722 = CARTESIAN_POINT ( 'NONE',  ( 25.39999999999999858, -1.600000000000094458, 34.92499999999998295 ) ) ;
#133723 = LINE ( 'NONE', #67789, #106123 ) ;
#133724 = CARTESIAN_POINT ( 'NONE',  ( 9.813491353976328213, -15.74070752338412049, 8.904080028138917413 ) ) ;
#133725 = ADVANCED_FACE ( 'NONE', ( #103073 ), #59588, .F. ) ;
#133726 = VERTEX_POINT ( 'NONE', #48692 ) ;
#133727 = DIRECTION ( 'NONE',  ( -0.3543493200069162685, -0.000000000000000000, -0.9351131265310288487 ) ) ;
#133728 = CARTESIAN_POINT ( 'NONE',  ( 23.99999999999983302, -6.033600742197676503, 5.000000000000000000 ) ) ;
#133729 = EDGE_CURVE ( 'NONE', #38905, #99727, #49437, .T. ) ;
#133730 = DIRECTION ( 'NONE',  ( -0.5735764363510503783, -0.8191520442889886899, 0.000000000000000000 ) ) ;
#133731 = VERTEX_POINT ( 'NONE', #135704 ) ;
#133732 =( NAMED_UNIT ( * ) SI_UNIT ( $, .STERADIAN. ) SOLID_ANGLE_UNIT ( ) );
#133733 = LINE ( 'NONE', #136387, #127550 ) ;
#133734 = DIRECTION ( 'NONE',  ( -0.7071067811865487940, 0.7071067811865463515, -0.000000000000000000 ) ) ;
#133735 = ADVANCED_FACE ( 'NONE', ( #47319 ), #77941, .F. ) ;
#133736 = CARTESIAN_POINT ( 'NONE',  ( 9.707013264292969623, -21.74070752338406365, 4.999753212805217117 ) ) ;
#133737 = CARTESIAN_POINT ( 'NONE',  ( 53.87043019189811588, -3.055000000000001936, 5.291415217122918513 ) ) ;
#133738 = LINE ( 'NONE', #45328, #69661 ) ;
#133739 = DIRECTION ( 'NONE',  ( 0.7071067811865487940, 0.7071067811865463515, 0.000000000000000000 ) ) ;
#133740 =( NAMED_UNIT ( * ) PLANE_ANGLE_UNIT ( ) SI_UNIT ( $, .RADIAN. ) );
#133741 = LINE ( 'NONE', #109109, #139030 ) ;
#133742 = ORIENTED_EDGE ( 'NONE', *, *, #4100, .F. ) ;
#133743 = LINE ( 'NONE', #134460, #111306 ) ;
#133744 = EDGE_LOOP ( 'NONE', ( #131331, #106313, #12439, #80715 ) ) ;
#133745 = DIRECTION ( 'NONE',  ( 0.000000000000000000, -1.000000000000000000, 0.000000000000000000 ) ) ;
#133746 = CARTESIAN_POINT ( 'NONE',  ( 0.005480084712502889671, 28.92564299267938210, 4.000000000000000000 ) ) ;
#133747 = DIRECTION ( 'NONE',  ( 0.000000000000000000, 0.000000000000000000, 1.000000000000000000 ) ) ;
#133748 = DIRECTION ( 'NONE',  ( 0.7071067811865487940, -0.7071067811865463515, 0.000000000000000000 ) ) ;
#133749 = DIRECTION ( 'NONE',  ( 1.000000000000000000, -0.000000000000000000, 0.000000000000000000 ) ) ;
#133750 = VERTEX_POINT ( 'NONE', #81341 ) ;
#133751 = VERTEX_POINT ( 'NONE', #93626 ) ;
#133752 = LINE ( 'NONE', #89523, #136675 ) ;
#133753 = PLANE ( 'NONE',  #120910 ) ;
#133754 = DIRECTION ( 'NONE',  ( 0.7071067811865487940, 0.7071067811865463515, 0.000000000000000000 ) ) ;
#133756 = EDGE_CURVE ( 'NONE', #69257, #14507, #69030, .T. ) ;
#133755 = CARTESIAN_POINT ( 'NONE',  ( 16.67080628287043709, -3.047499999999997211, -5.278424836066143655 ) ) ;
#133757 = CARTESIAN_POINT ( 'NONE',  ( 78.39169371712955581, 2.130196079827421762, 7.950000000000001066 ) ) ;
#133759 = EDGE_CURVE ( 'NONE', #88152, #130798, #15306, .T. ) ;
#133758 = CARTESIAN_POINT ( 'NONE',  ( -7.823340898400223509, 5.259292476615665457, 15.86257073897099801 ) ) ;
#133760 = DIRECTION ( 'NONE',  ( -0.7071067811865486830, -0.7071067811865464625, 0.000000000000000000 ) ) ;
#133761 = ORIENTED_EDGE ( 'NONE', *, *, #123265, .T. ) ;
#133762 = VECTOR ( 'NONE', #16297, 1000.000000000000227 ) ;
#133763 = CARTESIAN_POINT ( 'NONE',  ( 78.00000000000000000, 0.000000000000000000, -7.950000000000000178 ) ) ;
#133764 = DIRECTION ( 'NONE',  ( -0.7071067811865486830, 0.7071067811865464625, 0.000000000000000000 ) ) ;
#133765 = LINE ( 'NONE', #113415, #36938 ) ;
#133766 = DIRECTION ( 'NONE',  ( -0.6830127018922181881, 0.6830127018922202975, -0.2588190451025214056 ) ) ;
#133767 = VERTEX_POINT ( 'NONE', #99663 ) ;
#133768 = EDGE_CURVE ( 'NONE', #77873, #32412, #36388, .T. ) ;
#133769 = DIRECTION ( 'NONE',  ( 0.7071067811865486830, -0.7071067811865464625, -0.000000000000000000 ) ) ;
#133770 = CARTESIAN_POINT ( 'NONE',  ( -30.48921356237309510, -27.52281430457076894, 5.000000000000000000 ) ) ;
#133771 = CARTESIAN_POINT ( 'NONE',  ( 63.43793019189811133, -6.110000000000001208, 1.637169565754158951 ) ) ;
#133772 = VERTEX_POINT ( 'NONE', #3706 ) ;
#133773 = EDGE_LOOP ( 'NONE', ( #108045, #4832, #14638, #90666 ) ) ;
#133774 = DIRECTION ( 'NONE',  ( 0.000000000000000000, -1.000000000000000000, 0.000000000000000000 ) ) ;
#133775 = VECTOR ( 'NONE', #1180, 1000.000000000000000 ) ;
#133776 = FACE_OUTER_BOUND ( 'NONE', #17032, .T. ) ;
#133777 = DIRECTION ( 'NONE',  ( -0.7071067811865486830, -0.7071067811865464625, 0.000000000000000000 ) ) ;
#133778 = CIRCLE ( 'NONE', #119866, 0.5000000000000004441 ) ;
#133779 = CARTESIAN_POINT ( 'NONE',  ( 60.18398860626900415, 28.73617430169829490, 5.000000000000000000 ) ) ;
#133780 = CARTESIAN_POINT ( 'NONE',  ( -12.70000000000000107, -60.06289321881342858, 24.72882142070204736 ) ) ;
#133782 = ORIENTED_EDGE ( 'NONE', *, *, #17798, .F. ) ;
#133781 = FACE_OUTER_BOUND ( 'NONE', #37767, .T. ) ;
#133783 =( REPRESENTATION_RELATIONSHIP ('NONE','NONE', #69070, #39429 ) REPRESENTATION_RELATIONSHIP_WITH_TRANSFORMATION ( #52504 )SHAPE_REPRESENTATION_RELATIONSHIP( ) );
#133784 = DIRECTION ( 'NONE',  ( 0.000000000000000000, -1.000000000000000000, 0.000000000000000000 ) ) ;
#133785 = PLANE ( 'NONE',  #68521 ) ;
#133786 = CARTESIAN_POINT ( 'NONE',  ( -23.99999999999982947, -0.1606350220013114671, 4.664761815935120737 ) ) ;
#133787 = AXIS2_PLACEMENT_3D ( 'NONE', #128316, #28990, #59499 ) ;
#133788 = CARTESIAN_POINT ( 'NONE',  ( 17.51078643762690845, -27.52281430457043143, 5.000000000000000000 ) ) ;
#133789 = MECHANICAL_DESIGN_GEOMETRIC_PRESENTATION_REPRESENTATION (  '', ( #103637 ), #82883 ) ;
#133790 = VERTEX_POINT ( 'NONE', #133053 ) ;
#133791 = EDGE_LOOP ( 'NONE', ( #95220, #49716, #24207, #41043 ) ) ;
#133792 = CARTESIAN_POINT ( 'NONE',  ( 56.14626352523143282, -4.472830434245840259, 4.472830434245839371 ) ) ;
#133793 = VERTEX_POINT ( 'NONE', #37834 ) ;
#133794 = CARTESIAN_POINT ( 'NONE',  ( 20.51078643762690490, -27.52281430457041012, 5.000000000000000000 ) ) ;
#133795 = LINE ( 'NONE', #68559, #129052 ) ;
#133796 = DIRECTION ( 'NONE',  ( 0.7071067811865486830, -0.7071067811865464625, -0.000000000000000000 ) ) ;
#133797 = ADVANCED_FACE ( 'NONE', ( #33737 ), #113210, .F. ) ;
#133798 = CARTESIAN_POINT ( 'NONE',  ( 30.48921356237309510, -27.52281430457076894, 5.000000000000000000 ) ) ;
#133799 = CARTESIAN_POINT ( 'NONE',  ( 54.22916666666666430, 7.950000000000001954, -2.130196079827421762 ) ) ;
#133800 = ORIENTED_EDGE ( 'NONE', *, *, #123166, .F. ) ;
#133801 = ORIENTED_EDGE ( 'NONE', *, *, #35308, .F. ) ;
#133802 = CARTESIAN_POINT ( 'NONE',  ( -3.706792507240715295, 20.25929247661552068, 20.83292124670815681 ) ) ;
#133803 = ORIENTED_EDGE ( 'NONE', *, *, #104734, .T. ) ;
#133804 = CARTESIAN_POINT ( 'NONE',  ( -29.29289321881324426, 5.259292476615659240, 5.000000000000000000 ) ) ;
#133805 = DIRECTION ( 'NONE',  ( -0.7071067811865487940, 0.7071067811865463515, 0.000000000000000000 ) ) ;
#133806 = DIRECTION ( 'NONE',  ( 0.7071067811865487940, 0.7071067811865463515, -0.000000000000000000 ) ) ;
#133807 = VERTEX_POINT ( 'NONE', #113939 ) ;
#133808 = EDGE_CURVE ( 'NONE', #124820, #41591, #92896, .T. ) ;
#133809 = EDGE_CURVE ( 'NONE', #135883, #130610, #60302, .T. ) ;
#133810 = FACE_BOUND ( 'NONE', #117737, .T. ) ;
#133811 = LINE ( 'NONE', #112763, #80282 ) ;
#133812 = FACE_OUTER_BOUND ( 'NONE', #19650, .T. ) ;
#133813 = LINE ( 'NONE', #34499, #80701 ) ;
#133814 = VECTOR ( 'NONE', #131168, 999.9999999999998863 ) ;
#133815 = CARTESIAN_POINT ( 'NONE',  ( 18.18398860626898994, 28.73617430169800002, 5.000000000000000000 ) ) ;
#133816 = EDGE_CURVE ( 'NONE', #53919, #41067, #126251, .T. ) ;
#133817 = ADVANCED_FACE ( 'NONE', ( #84205 ), #89405, .T. ) ;
#133818 = CARTESIAN_POINT ( 'NONE',  ( 23.67183060077630330, -21.74070752338406365, 4.000000000000000000 ) ) ;
#133819 = CARTESIAN_POINT ( 'NONE',  ( 147.9560000000000173, 7.919999999999947526, -18.97500000000001918 ) ) ;
#133820 = ORIENTED_EDGE ( 'NONE', *, *, #141389, .F. ) ;
#133821 = VERTEX_POINT ( 'NONE', #139295 ) ;
#133822 = CARTESIAN_POINT ( 'NONE',  ( 106.8079301918981230, -6.109999999999998543, 1.637169565754158507 ) ) ;
#133823 = ORIENTED_EDGE ( 'NONE', *, *, #56373, .F. ) ;
#133824 = ADVANCED_FACE ( 'NONE', ( #42117 ), #98604, .T. ) ;
#133825 =( LENGTH_UNIT ( ) NAMED_UNIT ( * ) SI_UNIT ( .MILLI., .METRE. ) );
#133826 = ORIENTED_EDGE ( 'NONE', *, *, #117336, .F. ) ;
#133827 = CARTESIAN_POINT ( 'NONE',  ( -26.84387692260740366, -22.22500000000000142, 4.000000000000000000 ) ) ;
#133828 = CARTESIAN_POINT ( 'NONE',  ( 4.712472949537106715, 0.000000000000000000, 6.094999999999989981 ) ) ;
#133829 = COLOUR_RGB ( '', 0.08235294, 0.09019608, 0.10196078) ;
#133830 = ADVANCED_FACE ( 'NONE', ( #141402 ), #129809, .F. ) ;
#133831 = CARTESIAN_POINT ( 'NONE',  ( 32.99999999999976552, 11.58746187583913390, 4.000000000000000000 ) ) ;
#133832 = ORIENTED_EDGE ( 'NONE', *, *, #85932, .F. ) ;
#133833 = CARTESIAN_POINT ( 'NONE',  ( 34.47516574401890921, -17.97193265888400049, 4.998110765256835286 ) ) ;
#133834 = DIRECTION ( 'NONE',  ( 2.496005001405472275E-15, 1.000000000000000000, 0.000000000000000000 ) ) ;
#133835 = CARTESIAN_POINT ( 'NONE',  ( 160.0000000000000000, 0.000000000000000000, 0.000000000000000000 ) ) ;
#133836 = CARTESIAN_POINT ( 'NONE',  ( -21.18398860626899349, 28.73617430169802134, 5.000000000000000000 ) ) ;
#133837 = CARTESIAN_POINT ( 'NONE',  ( 2.087472949537105826, -6.094999999999989981, 3.732111120401553285E-16 ) ) ;
#133838 = EDGE_CURVE ( 'NONE', #103756, #43110, #71898, .T. ) ;
#133839 = DIRECTION ( 'NONE',  ( -0.000000000000000000, -0.3543493200069152693, 0.9351131265310292928 ) ) ;
#133840 = VERTEX_POINT ( 'NONE', #18155 ) ;
#133841 = DIRECTION ( 'NONE',  ( 0.7071067811865486830, -0.7071067811865464625, -0.000000000000000000 ) ) ;
#133842 = CARTESIAN_POINT ( 'NONE',  ( 27.18398860626900060, 28.73617430169806042, 5.000000000000000000 ) ) ;
#133843 = ORIENTED_EDGE ( 'NONE', *, *, #76096, .T. ) ;
#133844 = ORIENTED_EDGE ( 'NONE', *, *, #58646, .F. ) ;
#133845 = ORIENTED_EDGE ( 'NONE', *, *, #87128, .T. ) ;
#133846 = CARTESIAN_POINT ( 'NONE',  ( 54.10459685856476852, 1.637169565754164946, -6.109999999999999432 ) ) ;
#133847 = EDGE_CURVE ( 'NONE', #13520, #65516, #106595, .T. ) ;
#133848 = ORIENTED_EDGE ( 'NONE', *, *, #55601, .T. ) ;
#133849 = DIRECTION ( 'NONE',  ( -0.000000000000000000, 0.3543493200069153248, 0.9351131265310292928 ) ) ;
#133850 = CARTESIAN_POINT ( 'NONE',  ( 3.837472949537105826, 6.094999999999989981, -1.119633336120465690E-15 ) ) ;
#133851 = AXIS2_PLACEMENT_3D ( 'NONE', #135123, #122045, #90145 ) ;
#133852 = CARTESIAN_POINT ( 'NONE',  ( 93.91709685856477563, 3.054999999999998828, 5.291415217122922066 ) ) ;
#133853 = DIRECTION ( 'NONE',  ( 0.7071067811865486830, -0.7071067811865464625, -0.000000000000000000 ) ) ;
#133854 = ORIENTED_EDGE ( 'NONE', *, *, #32919, .F. ) ;
#133855 = EDGE_CURVE ( 'NONE', #111950, #98883, #51560, .T. ) ;
#133856 = ORIENTED_EDGE ( 'NONE', *, *, #74157, .T. ) ;
#133857 = CARTESIAN_POINT ( 'NONE',  ( 32.99999999999977973, 14.96639925780211122, 5.000000000000000000 ) ) ;
#133858 = CARTESIAN_POINT ( 'NONE',  ( 28.49999999999981171, 8.319652575858409449, -8.582050562765761725 ) ) ;
#133859 = EDGE_LOOP ( 'NONE', ( #104846, #44259, #114390, #38801, #99779, #99014, #32818, #62570 ) ) ;
#133860 = FACE_OUTER_BOUND ( 'NONE', #12585, .T. ) ;
#133861 = CARTESIAN_POINT ( 'NONE',  ( 8.188407645496676324, -3.851859888774471706E-31, 2.500000000000001332 ) ) ;
#133863 = EDGE_CURVE ( 'NONE', #132022, #116559, #39989, .T. ) ;
#133862 = DIRECTION ( 'NONE',  ( -0.7071067811865486830, 0.7071067811865464625, 0.000000000000000000 ) ) ;
#133864 = ORIENTED_EDGE ( 'NONE', *, *, #1120, .F. ) ;
#133865 = DIRECTION ( 'NONE',  ( -0.000000000000000000, 1.000000000000000000, -0.000000000000000000 ) ) ;
#133866 = PLANE ( 'NONE',  #47545 ) ;
#133867 = ORIENTED_EDGE ( 'NONE', *, *, #64623, .T. ) ;
#133868 = EDGE_CURVE ( 'NONE', #48369, #108055, #29078, .T. ) ;
#133869 = ORIENTED_EDGE ( 'NONE', *, *, #126081, .F. ) ;
#133870 = VERTEX_POINT ( 'NONE', #16767 ) ;
#133871 = DIRECTION ( 'NONE',  ( -0.3543493200069162685, -0.000000000000000000, -0.9351131265310288487 ) ) ;
#133872 = MECHANICAL_DESIGN_GEOMETRIC_PRESENTATION_REPRESENTATION (  '', ( #45931 ), #138534 ) ;
#133873 = ADVANCED_FACE ( 'NONE', ( #138558 ), #28376, .F. ) ;
#133874 = DIRECTION ( 'NONE',  ( 0.000000000000000000, -1.000000000000000000, 0.000000000000000000 ) ) ;
#133875 = AXIS2_PLACEMENT_3D ( 'NONE', #51816, #104745, #59835 ) ;
#133876 = PLANE ( 'NONE',  #53222 ) ;
#133877 = DIRECTION ( 'NONE',  ( -0.7071067811865486830, -0.7071067811865464625, 0.000000000000000000 ) ) ;
#133878 = VERTEX_POINT ( 'NONE', #116791 ) ;
#133879 = VECTOR ( 'NONE', #83201, 1000.000000000000000 ) ;
#133880 = AXIS2_PLACEMENT_3D ( 'NONE', #17225, #116540, #28827 ) ;
#133881 = SURFACE_STYLE_FILL_AREA ( #112829 ) ;
#133882 = CARTESIAN_POINT ( 'NONE',  ( 13.10373647476855297, 5.808823158059036373, 5.808823158059032821 ) ) ;
#133883 = DIRECTION ( 'NONE',  ( 0.000000000000000000, 0.000000000000000000, 1.000000000000000000 ) ) ;
#133884 = CARTESIAN_POINT ( 'NONE',  ( -29.99999999999979039, 2.342191155542419523, -5.001666872980017331 ) ) ;
#133885 = EDGE_CURVE ( 'NONE', #18576, #96758, #17474, .T. ) ;
#133886 = LINE ( 'NONE', #34578, #37401 ) ;
#133887 = ORIENTED_EDGE ( 'NONE', *, *, #79226, .T. ) ;
#133888 = ORIENTED_EDGE ( 'NONE', *, *, #6500, .F. ) ;
#133889 = VERTEX_POINT ( 'NONE', #74015 ) ;
#133890 = CARTESIAN_POINT ( 'NONE',  ( 20.27083333333333570, 6.094999999999991758, 1.633150327867686880 ) ) ;
#133891 = FACE_BOUND ( 'NONE', #48482, .T. ) ;
#133892 = AXIS2_PLACEMENT_3D ( 'NONE', #78457, #22597, #68326 ) ;
#133893 = CARTESIAN_POINT ( 'NONE',  ( -66.18398860626901126, 28.73617430169833753, 5.000000000000000000 ) ) ;
#133894 = ADVANCED_FACE ( 'NONE', ( #6552 ), #18902, .F. ) ;
#133895 = LINE ( 'NONE', #34586, #78413 ) ;
#133896 = CARTESIAN_POINT ( 'NONE',  ( 7.652374387692081115, 8.843121118309934303, -3.475427755405318120 ) ) ;
#133897 = LINE ( 'NONE', #72262, #120099 ) ;
#133898 = CARTESIAN_POINT ( 'NONE',  ( -27.18398860626900060, 28.73617430169806042, 5.000000000000000000 ) ) ;
#133899 = LINE ( 'NONE', #12812, #16253 ) ;
#133900 = CARTESIAN_POINT ( 'NONE',  ( -39.29974487139159578, -27.71228299555233576, 4.000000000000000000 ) ) ;
#133901 = ORIENTED_EDGE ( 'NONE', *, *, #7118, .F. ) ;
#133902 = DIRECTION ( 'NONE',  ( -1.000000000000000000, -0.000000000000000000, -0.000000000000000000 ) ) ;
#133903 = VERTEX_POINT ( 'NONE', #42829 ) ;
#133904 = CARTESIAN_POINT ( 'NONE',  ( 19.86756573869621434, -2.692863782213888335, -33.80212331857929797 ) ) ;
#133905 = VERTEX_POINT ( 'NONE', #142144 ) ;
#133906 = VECTOR ( 'NONE', #2456, 1000.000000000000227 ) ;
#133907 = AXIS2_PLACEMENT_3D ( 'NONE', #107265, #76084, #7942 ) ;
#133908 = CARTESIAN_POINT ( 'NONE',  ( -19.93618820137057668, -3.270000000000008455, -36.99999999997771738 ) ) ;
#133910 = VERTEX_POINT ( 'NONE', #10166 ) ;
#133909 = CARTESIAN_POINT ( 'NONE',  ( 0.000000000000000000, 0.000000000000000000, 5.000000000000000000 ) ) ;
#133911 = CARTESIAN_POINT ( 'NONE',  ( 6.938893903907228378E-15, -3.412538124160723108, 4.000000000000000000 ) ) ;
#133912 = DIRECTION ( 'NONE',  ( 0.7071067811865487940, 0.7071067811865463515, 0.000000000000000000 ) ) ;
#133913 = VERTEX_POINT ( 'NONE', #43520 ) ;
#133914 = SURFACE_SIDE_STYLE ('',( #100581 ) ) ;
#133915 = VERTEX_POINT ( 'NONE', #131977 ) ;
#133916 = DIRECTION ( 'NONE',  ( 0.000000000000000000, -1.000000000000000000, 0.000000000000000000 ) ) ;
#133917 = EDGE_LOOP ( 'NONE', ( #43297, #18447, #108447, #82281 ) ) ;
#133918 = DIRECTION ( 'NONE',  ( 0.7071067811865486830, -0.7071067811865464625, -0.000000000000000000 ) ) ;
#133919 = ADVANCED_FACE ( 'NONE', ( #707 ), #132714, .T. ) ;
#133920 = CARTESIAN_POINT ( 'NONE',  ( 99.82919371712955581, -3.975000000000001865, 6.884901960086284411 ) ) ;
#133921 =( NAMED_UNIT ( * ) SI_UNIT ( $, .STERADIAN. ) SOLID_ANGLE_UNIT ( ) );
#133922 = CARTESIAN_POINT ( 'NONE',  ( 23.32000000000000028, 9.521314400968980422E-16, 0.000000000000000000 ) ) ;
#133923 = ORIENTED_EDGE ( 'NONE', *, *, #81776, .F. ) ;
#133924 = CARTESIAN_POINT ( 'NONE',  ( 12.18398860626900060, 28.73617430169795739, 5.000000000000000000 ) ) ;
#133925 = LINE ( 'NONE', #74205, #88968 ) ;
#133926 = DIRECTION ( 'NONE',  ( 0.7071067811865487940, 0.7071067811865463515, 0.000000000000000000 ) ) ;
#133927 = CARTESIAN_POINT ( 'NONE',  ( 10.79166666666666785, -3.047499999999994547, 5.278424836066145431 ) ) ;
#133928 = CARTESIAN_POINT ( 'NONE',  ( 22.72873647476855652, 5.808823158059031044, -5.808823158059037262 ) ) ;
#133929 = VECTOR ( 'NONE', #18078, 1000.000000000000000 ) ;
#133930 = DIRECTION ( 'NONE',  ( 0.7071067811865486830, -0.7071067811865464625, -0.000000000000000000 ) ) ;
#133931 = CARTESIAN_POINT ( 'NONE',  ( 1.827855086967997700, 4.202752102959690472E-16, 0.000000000000000000 ) ) ;
#133932 = ORIENTED_EDGE ( 'NONE', *, *, #55829, .T. ) ;
#133934 = ORIENTED_EDGE ( 'NONE', *, *, #42137, .F. ) ;
#133933 = AXIS2_PLACEMENT_3D ( 'NONE', #94484, #61218, #38699 ) ;
#133935 = CARTESIAN_POINT ( 'NONE',  ( 2.010880286539464379, -22.02621442084248216, 4.990779571109223767 ) ) ;
#133936 = ORIENTED_EDGE ( 'NONE', *, *, #13743, .F. ) ;
#133937 = CARTESIAN_POINT ( 'NONE',  ( 94.35459685856476142, -1.637169565754161615, 6.110000000000000320 ) ) ;
#133938 = DIRECTION ( 'NONE',  ( 0.6830127018922181881, 0.6830127018922202975, -0.2588190451025214056 ) ) ;
#133939 = DIRECTION ( 'NONE',  ( -0.7071067811865487940, 0.7071067811865463515, -0.000000000000000000 ) ) ;
#133940 = CARTESIAN_POINT ( 'NONE',  ( -34.92500000000001137, -7.199905483972716347, 4.759050581649336920 ) ) ;
#133941 = CARTESIAN_POINT ( 'NONE',  ( -25.39999999999996305, 0.000000000000000000, 0.000000000000000000 ) ) ;
#133942 = ORIENTED_EDGE ( 'NONE', *, *, #92692, .F. ) ;
#133943 = CARTESIAN_POINT ( 'NONE',  ( 28.49999999999980460, -20.53675388469227769, 2.352720554255958607 ) ) ;
#133944 = DIRECTION ( 'NONE',  ( 0.3543493200069163240, -0.000000000000000000, 0.9351131265310288487 ) ) ;
#133945 = LINE ( 'NONE', #113603, #44282 ) ;
#133946 = DIRECTION ( 'NONE',  ( 0.7071067811865487940, 0.7071067811865463515, 0.000000000000000000 ) ) ;
#133948 = EDGE_LOOP ( 'NONE', ( #137435, #122375 ) ) ;
#133947 = PLANE ( 'NONE',  #68397 ) ;
#133949 = CARTESIAN_POINT ( 'NONE',  ( 3.250000000000000000, 0.000000000000000000, 0.000000000000000000 ) ) ;
#133950 = LINE ( 'NONE', #123088, #22204 ) ;
#133951 = CARTESIAN_POINT ( 'NONE',  ( -24.79289321881327979, -8.240707523384198652, 5.000000000000000000 ) ) ;
#133952 = DIRECTION ( 'NONE',  ( -0.6830127018922180770, -0.6830127018922204085, -0.2588190451025213501 ) ) ;
#133953 = CARTESIAN_POINT ( 'NONE',  ( 22.49999999999984723, 15.43112307739202826, 4.000000000000000000 ) ) ;
#133954 = EDGE_LOOP ( 'NONE', ( #133442, #121748, #26297, #120111 ) ) ;
#133955 = ORIENTED_EDGE ( 'NONE', *, *, #128477, .F. ) ;
#133956 = ORIENTED_EDGE ( 'NONE', *, *, #105693, .T. ) ;
#133957 = CARTESIAN_POINT ( 'NONE',  ( 95.81293019189807580, -1.637169565754159617, -6.110000000000001208 ) ) ;
#133958 = EDGE_LOOP ( 'NONE', ( #15993, #7689, #85190, #111152 ) ) ;
#133959 = CARTESIAN_POINT ( 'NONE',  ( 31.49999999999978684, 3.052185695429138423, 5.000000000000000000 ) ) ;
#133960 = DIRECTION ( 'NONE',  ( -0.000000000000000000, -1.000000000000000000, -0.000000000000000000 ) ) ;
#133961 = CARTESIAN_POINT ( 'NONE',  ( 50.99451991528749062, 28.92564299267973738, 4.000000000000000000 ) ) ;
#133962 = CARTESIAN_POINT ( 'NONE',  ( -63.48921356237309510, -27.52281430457099631, 5.000000000000000000 ) ) ;
#133963 = ORIENTED_EDGE ( 'NONE', *, *, #36337, .F. ) ;
#133964 = FACE_OUTER_BOUND ( 'NONE', #94783, .T. ) ;
#133965 = CARTESIAN_POINT ( 'NONE',  ( 1.499999999999994449, 3.073033219394626592, -6.593910359670966947 ) ) ;
#133966 = LINE ( 'NONE', #24487, #125166 ) ;
#133967 = CARTESIAN_POINT ( 'NONE',  ( 88.72459685856478018, -1.637169565754160949, 6.109999999999997655 ) ) ;
#133968 = EDGE_LOOP ( 'NONE', ( #33902, #34257, #54372, #89135 ) ) ;
#133969 = DIRECTION ( 'NONE',  ( 0.6830127018922180770, -0.6830127018922204085, -0.2588190451025213501 ) ) ;
#133970 = ADVANCED_FACE ( 'NONE', ( #45697 ), #143544, .F. ) ;
#133971 = EDGE_CURVE ( 'NONE', #74639, #25093, #56594, .T. ) ;
#133972 = CARTESIAN_POINT ( 'NONE',  ( 24.09999999999999787, 9.521314400968980422E-16, 0.000000000000000000 ) ) ;
#133973 = VECTOR ( 'NONE', #109927, 1000.000000000000227 ) ;
#133974 = AXIS2_PLACEMENT_3D ( 'NONE', #103366, #59217, #79556 ) ;
#133975 = VECTOR ( 'NONE', #95645, 1000.000000000000227 ) ;
#133976 = ORIENTED_EDGE ( 'NONE', *, *, #106933, .T. ) ;
#133977 = ORIENTED_EDGE ( 'NONE', *, *, #127014, .T. ) ;
#133978 = AXIS2_PLACEMENT_3D ( 'NONE', #131680, #122195, #41810 ) ;
#133979 = DIRECTION ( 'NONE',  ( -0.7071067811865486830, -0.7071067811865464625, -0.000000000000000000 ) ) ;
#133980 = EDGE_CURVE ( 'NONE', #16744, #49722, #109491, .T. ) ;
#133981 = ADVANCED_FACE ( 'NONE', ( #20315 ), #23164, .F. ) ;
#133982 =( NAMED_UNIT ( * ) PLANE_ANGLE_UNIT ( ) SI_UNIT ( $, .RADIAN. ) );
#133983 = CARTESIAN_POINT ( 'NONE',  ( 25.00456980810188767, 6.871911579029510442, -3.967499999999998916 ) ) ;
#133984 = CARTESIAN_POINT ( 'NONE',  ( -47.99451991528749062, 28.92564299267971251, 4.000000000000000000 ) ) ;
#133985 = VECTOR ( 'NONE', #18084, 1000.000000000000000 ) ;
#133986 = AXIS2_PLACEMENT_3D ( 'NONE', #96187, #128835, #16487 ) ;
#133987 = DIRECTION ( 'NONE',  ( 0.7071067811865487940, -0.7071067811865463515, 0.000000000000000000 ) ) ;
#133988 = DIRECTION ( 'NONE',  ( -0.7071067811865487940, 0.7071067811865463515, 0.000000000000000000 ) ) ;
#133989 = EDGE_CURVE ( 'NONE', #92202, #70018, #78301, .T. ) ;
#133990 = ADVANCED_FACE ( 'NONE', ( #108738 ), #9419, .F. ) ;
#133991 = PLANE ( 'NONE',  #121470 ) ;
#133992 = VERTEX_POINT ( 'NONE', #131244 ) ;
#133993 =( BOUNDED_CURVE ( )  B_SPLINE_CURVE ( 3, ( #53225, #65593, #43801, #88017 ),
 .UNSPECIFIED., .F., .F. ) 
 B_SPLINE_CURVE_WITH_KNOTS ( ( 4, 4 ),
 ( 5.005968288816738720, 5.074607125596333645 ),
 .UNSPECIFIED. ) 
 CURVE ( )  GEOMETRIC_REPRESENTATION_ITEM ( )  RATIONAL_B_SPLINE_CURVE ( ( 1.000000000000000000, 0.9996074310407766506, 0.9996074310407766506, 1.000000000000000000 ) ) 
 REPRESENTATION_ITEM ( '' )  );
#133994 = ORIENTED_EDGE ( 'NONE', *, *, #64442, .T. ) ;
#133996 = EDGE_CURVE ( 'NONE', #63182, #25281, #65269, .T. ) ;
#133995 = CARTESIAN_POINT ( 'NONE',  ( 3.469446951953614189E-15, 8.587461875839158765, 4.000000000000000000 ) ) ;
#133997 = ORIENTED_EDGE ( 'NONE', *, *, #25090, .T. ) ;
#133998 = ORIENTED_EDGE ( 'NONE', *, *, #52468, .T. ) ;
#133999 = VECTOR ( 'NONE', #118912, 1000.000000000000000 ) ;
#134000 = EDGE_CURVE ( 'NONE', #58156, #57981, #43741, .T. ) ;
#134001 = EDGE_CURVE ( 'NONE', #72640, #80026, #122489, .T. ) ;
#134002 = CIRCLE ( 'NONE', #96905, 0.5000000000000004441 ) ;
#134003 = DIRECTION ( 'NONE',  ( -0.000000000000000000, 0.3543493200069153248, 0.9351131265310292928 ) ) ;
#134004 = VERTEX_POINT ( 'NONE', #12309 ) ;
#134005 = CARTESIAN_POINT ( 'NONE',  ( -15.18398860626900237, 28.73617430169797871, 5.000000000000000000 ) ) ;
#134006 = DIRECTION ( 'NONE',  ( -0.7071067811865487940, 0.7071067811865463515, 0.000000000000000000 ) ) ;
#134007 = DIRECTION ( 'NONE',  ( 1.000000000000000000, 0.000000000000000000, 0.000000000000000000 ) ) ;
#134008 = CARTESIAN_POINT ( 'NONE',  ( 128.5894344200537489, -52.00875322212550600, 39.86617647058822911 ) ) ;
#134009 = AXIS2_PLACEMENT_3D ( 'NONE', #9416, #43518, #108025 ) ;
#134010 = AXIS2_PLACEMENT_3D ( 'NONE', #30550, #29807, #42868 ) ;
#134011 = LINE ( 'NONE', #57192, #37551 ) ;
#134012 = ORIENTED_EDGE ( 'NONE', *, *, #96784, .T. ) ;
#134013 = VECTOR ( 'NONE', #70978, 1000.000000000000000 ) ;
#134014 = EDGE_CURVE ( 'NONE', #59677, #70620, #133404, .T. ) ;
#134015 = DIRECTION ( 'NONE',  ( 0.000000000000000000, -1.000000000000000000, 0.000000000000000000 ) ) ;
#134016 = VECTOR ( 'NONE', #137478, 1000.000000000000227 ) ;
#134017 = ORIENTED_EDGE ( 'NONE', *, *, #55334, .T. ) ;
#134018 = DIRECTION ( 'NONE',  ( -0.000000000000000000, -0.000000000000000000, 1.000000000000000000 ) ) ;
#134019 = ORIENTED_EDGE ( 'NONE', *, *, #113327, .T. ) ;
#134020 = CARTESIAN_POINT ( 'NONE',  ( 5.671830600776431197, -12.74070752338415424, 4.000000000000000000 ) ) ;
#134021 = VERTEX_POINT ( 'NONE', #32660 ) ;
#134022 = LINE ( 'NONE', #34711, #29652 ) ;
#134023 = EDGE_LOOP ( 'NONE', ( #129940, #114905, #38558, #108831 ) ) ;
#134024 = ORIENTED_EDGE ( 'NONE', *, *, #120773, .T. ) ;
#134025 = AXIS2_PLACEMENT_3D ( 'NONE', #112351, #68865, #70316 ) ;
#134026 = EDGE_CURVE ( 'NONE', #36664, #58070, #54653, .T. ) ;
#134027 = ORIENTED_EDGE ( 'NONE', *, *, #39591, .F. ) ;
#134028 = PRESENTATION_LAYER_ASSIGNMENT (  '', '', ( #103870 ) ) ;
#134029 = PLANE ( 'NONE',  #129963 ) ;
#134030 = DIRECTION ( 'NONE',  ( 0.7071067811865486830, -0.7071067811865464625, -0.000000000000000000 ) ) ;
#134031 = CARTESIAN_POINT ( 'NONE',  ( 0.7928932188134545367, 3.759292476615681888, 5.000000000000000000 ) ) ;
#134032 = DIRECTION ( 'NONE',  ( -0.6830127018922180770, -0.6830127018922204085, -0.2588190451025213501 ) ) ;
#134033 = CARTESIAN_POINT ( 'NONE',  ( 115.2087635252314470, -7.482591942790329030E-16, 6.110000000000001208 ) ) ;
#134034 = FACE_OUTER_BOUND ( 'NONE', #123044, .T. ) ;
#134035 = CARTESIAN_POINT ( 'NONE',  ( 8.994519915287490619, 28.92564299267944250, 4.000000000000000000 ) ) ;
#134036 = LINE ( 'NONE', #33331, #136181 ) ;
#134037 = EDGE_CURVE ( 'NONE', #129523, #99824, #121774, .T. ) ;
#134038 = VECTOR ( 'NONE', #93056, 1000.000000000000227 ) ;
#134039 = FACE_OUTER_BOUND ( 'NONE', #54056, .T. ) ;
#134041 = EDGE_CURVE ( 'NONE', #137069, #50477, #11569, .T. ) ;
#134040 = DIRECTION ( 'NONE',  ( -1.000000000000000000, -1.224606353822377258E-16, -0.000000000000000000 ) ) ;
#134042 = ORIENTED_EDGE ( 'NONE', *, *, #31591, .F. ) ;
#134043 = CARTESIAN_POINT ( 'NONE',  ( 1.903119261757429959, -22.22500000000000142, -8.955551095671996364 ) ) ;
#134044 = DIRECTION ( 'NONE',  ( -0.7071067811865487940, 0.7071067811865463515, 0.000000000000000000 ) ) ;
#134045 = CARTESIAN_POINT ( 'NONE',  ( 14.99451991528749595, 28.92564299267948513, 4.000000000000000000 ) ) ;
#134046 = ORIENTED_EDGE ( 'NONE', *, *, #143215, .F. ) ;
#134047 = ADVANCED_FACE ( 'NONE', ( #34093 ), #23924, .T. ) ;
#134048 = ORIENTED_EDGE ( 'NONE', *, *, #88489, .F. ) ;
#134049 = FACE_OUTER_BOUND ( 'NONE', #122080, .T. ) ;
#134050 = ORIENTED_EDGE ( 'NONE', *, *, #90629, .F. ) ;
#134051 = EDGE_CURVE ( 'NONE', #103176, #50701, #26759, .T. ) ;
#134052 = EDGE_CURVE ( 'NONE', #67739, #88536, #13715, .T. ) ;
#134053 = ORIENTED_EDGE ( 'NONE', *, *, #128054, .F. ) ;
#134054 = CARTESIAN_POINT ( 'NONE',  ( -18.00548008471250583, 28.92564299267925776, 4.000000000000000000 ) ) ;
#134055 = CARTESIAN_POINT ( 'NONE',  ( 26.20710678118636494, 15.75929247661556687, 5.000000000000000000 ) ) ;
#134056 = CARTESIAN_POINT ( 'NONE',  ( 0.005480084712502889671, 28.92564299267938210, 4.000000000000000000 ) ) ;
#134057 = DIRECTION ( 'NONE',  ( -0.7071067811865487940, 0.7071067811865463515, 0.000000000000000000 ) ) ;
#134058 = VERTEX_POINT ( 'NONE', #15148 ) ;
#134059 = DIRECTION ( 'NONE',  ( 0.7071067811865486830, -0.7071067811865464625, -0.000000000000000000 ) ) ;
#134060 = ORIENTED_EDGE ( 'NONE', *, *, #45204, .F. ) ;
#134061 = CARTESIAN_POINT ( 'NONE',  ( 42.29974487139158157, -27.71228299555235708, 4.000000000000000000 ) ) ;
#134062 = CARTESIAN_POINT ( 'NONE',  ( 15.08790314143521982, 6.871911579029515771, 3.967499999999989146 ) ) ;
#134063 = EDGE_LOOP ( 'NONE', ( #9181, #111866, #2447, #81806 ) ) ;
#134064 = CARTESIAN_POINT ( 'NONE',  ( 86.68293019189813720, -1.637169565754159173, -6.109999999999999432 ) ) ;
#134065 = LINE ( 'NONE', #124602, #143182 ) ;
#134066 = EDGE_CURVE ( 'NONE', #63600, #134564, #81165, .T. ) ;
#134067 = PLANE ( 'NONE',  #39598 ) ;
#134068 = EDGE_LOOP ( 'NONE', ( #111945, #84120, #17291, #135792 ) ) ;
#134069 = EDGE_LOOP ( 'NONE', ( #85250, #84274, #78339, #133718 ) ) ;
#134070 = EDGE_LOOP ( 'NONE', ( #72106, #24342, #21505, #21168 ) ) ;
#134071 = LINE ( 'NONE', #87699, #54273 ) ;
#134072 = CARTESIAN_POINT ( 'NONE',  ( 6.639999999999984581, -40.42999999999999972, -40.00000000000000000 ) ) ;
#134073 = DIRECTION ( 'NONE',  ( -0.000000000000000000, 0.000000000000000000, 1.000000000000000000 ) ) ;
#134074 = CARTESIAN_POINT ( 'NONE',  ( 29.20710678118634007, -11.24070752338416668, 5.000000000000000000 ) ) ;
#134075 = CARTESIAN_POINT ( 'NONE',  ( -11.20710678118646442, 18.75929247661552779, 5.000000000000000000 ) ) ;
#134076 = ORIENTED_EDGE ( 'NONE', *, *, #133107, .T. ) ;
#134077 = DIRECTION ( 'NONE',  ( 0.7071067811865487940, 0.7071067811865463515, -0.000000000000000000 ) ) ;
#134078 = ADVANCED_FACE ( 'NONE', ( #59430 ), #2856, .F. ) ;
#134079 = LINE ( 'NONE', #134815, #44558 ) ;
#134080 = ORIENTED_EDGE ( 'NONE', *, *, #105988, .T. ) ;
#134081 = DIRECTION ( 'NONE',  ( 0.6830127018922180770, -0.6830127018922204085, -0.2588190451025213501 ) ) ;
#134082 = VECTOR ( 'NONE', #11850, 1000.000000000000000 ) ;
#134083 = VECTOR ( 'NONE', #58087, 1000.000000000000000 ) ;
#134084 = PRESENTATION_LAYER_ASSIGNMENT (  '', '', ( #113259 ) ) ;
#134085 = CYLINDRICAL_SURFACE ( 'NONE', #132744, 6.349999999999999645 ) ;
#134086 = ORIENTED_EDGE ( 'NONE', *, *, #93477, .F. ) ;
#134087 = AXIS2_PLACEMENT_3D ( 'NONE', #1319, #66615, #43427 ) ;
#134090 = ADVANCED_FACE ( 'NONE', ( #37663 ), #4222, .T. ) ;
#134089 = ORIENTED_EDGE ( 'NONE', *, *, #94554, .F. ) ;
#134088 = PLANE ( 'NONE',  #132018 ) ;
#134091 = EDGE_LOOP ( 'NONE', ( #91425, #86336, #4398 ) ) ;
#134092 = CARTESIAN_POINT ( 'NONE',  ( -23.99999999999983302, 15.45873954670183359, -0.03131636524288453072 ) ) ;
#134093 = CARTESIAN_POINT ( 'NONE',  ( 152.4000000000000057, 7.919999999999947526, 16.57230000000002335 ) ) ;
#134094 = ORIENTED_EDGE ( 'NONE', *, *, #127521, .F. ) ;
#134095 = DIRECTION ( 'NONE',  ( 1.000000000000000000, 0.000000000000000000, 0.000000000000000000 ) ) ;
#134096 = STYLED_ITEM ( 'NONE', ( #140663 ), #139343 ) ;
#134097 = EDGE_LOOP ( 'NONE', ( #116356, #39140, #28739, #128735, #22468, #120965 ) ) ;
#134098 = PLANE ( 'NONE',  #126222 ) ;
#134099 = LINE ( 'NONE', #2096, #127285 ) ;
#134100 = EDGE_CURVE ( 'NONE', #22612, #117925, #47848, .T. ) ;
#134101 = CARTESIAN_POINT ( 'NONE',  ( -13.17183060077637968, 12.75929247661559351, 4.000000000000000000 ) ) ;
#134102 = CARTESIAN_POINT ( 'NONE',  ( 47.76669371712955581, -7.949999999999998401, 2.130196079827423983 ) ) ;
#134103 = DIRECTION ( 'NONE',  ( 1.000000000000000000, -0.000000000000000000, 0.000000000000000000 ) ) ;
#134104 = CARTESIAN_POINT ( 'NONE',  ( -14.99999999999989164, 13.55218569542902607, 5.000000000000000000 ) ) ;
#134105 = CARTESIAN_POINT ( 'NONE',  ( -1.033400323430223811, 6.759292476615649470, 12.28218704918521809 ) ) ;
#134106 = CARTESIAN_POINT ( 'NONE',  ( 23.24139925780185223, 21.72500000000000853, 5.000000000000000000 ) ) ;
#134107 = CARTESIAN_POINT ( 'NONE',  ( 25.06206980810188512, -7.934999999999991616, -2.126176841940955242 ) ) ;
#134109 = VECTOR ( 'NONE', #24431, 1000.000000000000227 ) ;
#134108 = CARTESIAN_POINT ( 'NONE',  ( 7.939999999999994174, -32.12917598568331101, -10.00000000000000178 ) ) ;
#134110 = LINE ( 'NONE', #100052, #64459 ) ;
#134111 = CIRCLE ( 'NONE', #69327, 28.00000000000001776 ) ;
#134112 = CARTESIAN_POINT ( 'NONE',  ( 24.29974487139158867, -27.71228299555223273, 4.000000000000000000 ) ) ;
#134113 = CARTESIAN_POINT ( 'NONE',  ( 38.71998032010573354, 0.7592924766157138627, 14.27032725228017895 ) ) ;
#134114 = ORIENTED_EDGE ( 'NONE', *, *, #35906, .T. ) ;
#134115 = ADVANCED_FACE ( 'NONE', ( #112355 ), #36230, .F. ) ;
#134116 = EDGE_LOOP ( 'NONE', ( #119958, #55525, #14166, #90438 ) ) ;
#134117 = CARTESIAN_POINT ( 'NONE',  ( 105.4166666666666572, -6.884901960086287076, -3.975000000000000977 ) ) ;
#134118 = ADVANCED_FACE ( 'NONE', ( #2110 ), #91334, .T. ) ;
#134119 = ORIENTED_EDGE ( 'NONE', *, *, #77906, .T. ) ;
#134120 = VERTEX_POINT ( 'NONE', #92013 ) ;
#134121 = ORIENTED_EDGE ( 'NONE', *, *, #54703, .F. ) ;
#134122 = CARTESIAN_POINT ( 'NONE',  ( -2.999999999999981792, 20.70535890316561023, 1.956823837851923598 ) ) ;
#134123 = PLANE ( 'NONE',  #111192 ) ;
#134124 = CARTESIAN_POINT ( 'NONE',  ( 14.69992816670506208, 9.499966918880492273, -0.1465975642050108829 ) ) ;
#134125 = ORIENTED_EDGE ( 'NONE', *, *, #51855, .T. ) ;
#134126 = VECTOR ( 'NONE', #36593, 999.9999999999998863 ) ;
#134127 = DIRECTION ( 'NONE',  ( -0.000000000000000000, 0.000000000000000000, 1.000000000000000000 ) ) ;
#134128 = CARTESIAN_POINT ( 'NONE',  ( 7.139999999999991687, -35.69931899287964683, -11.97485302731577939 ) ) ;
#134129 = VECTOR ( 'NONE', #133739, 999.9999999999998863 ) ;
#134130 = FACE_OUTER_BOUND ( 'NONE', #20890, .T. ) ;
#134131 = ORIENTED_EDGE ( 'NONE', *, *, #89533, .T. ) ;
#134132 = EDGE_CURVE ( 'NONE', #91102, #140981, #119484, .T. ) ;
#134133 = DIRECTION ( 'NONE',  ( -0.7071067811865486830, -0.7071067811865464625, 0.000000000000000000 ) ) ;
#134134 = CARTESIAN_POINT ( 'NONE',  ( -35.99451991528749772, 28.92564299267963079, 4.000000000000000000 ) ) ;
#134135 = PLANE ( 'NONE',  #100032 ) ;
#134136 = VECTOR ( 'NONE', #75127, 1000.000000000000000 ) ;
#134137 = LINE ( 'NONE', #2881, #40663 ) ;
#134138 = LINE ( 'NONE', #123275, #67856 ) ;
#134139 = DIRECTION ( 'NONE',  ( 0.7071067811865486830, -0.7071067811865464625, -0.000000000000000000 ) ) ;
#134140 = STYLED_ITEM ( 'NONE', ( #135657 ), #57143 ) ;
#134141 = DIRECTION ( 'NONE',  ( 0.6830127018922180770, -0.6830127018922204085, -0.2588190451025213501 ) ) ;
#134142 = FACE_OUTER_BOUND ( 'NONE', #72044, .T. ) ;
#134143 = ORIENTED_EDGE ( 'NONE', *, *, #4876, .T. ) ;
#134144 = ORIENTED_EDGE ( 'NONE', *, *, #118390, .T. ) ;
#134145 = CARTESIAN_POINT ( 'NONE',  ( 122.6462635252314328, -4.472830434245840259, 4.472830434245839371 ) ) ;
#134146 = ORIENTED_EDGE ( 'NONE', *, *, #32757, .T. ) ;
#134147 = CARTESIAN_POINT ( 'NONE',  ( 99.43749999999998579, 5.819803920172574863, -5.819803920172573086 ) ) ;
#134148 = AXIS2_PLACEMENT_3D ( 'NONE', #24064, #90013, #13151 ) ;
#134149 = CARTESIAN_POINT ( 'NONE',  ( -15.70710678118642711, -12.74070752338415069, 5.000000000000000000 ) ) ;
#134150 = CARTESIAN_POINT ( 'NONE',  ( -10.49999999999992184, -10.04351517176479014, -1.623559851933848330 ) ) ;
#134151 = DIRECTION ( 'NONE',  ( 0.000000000000000000, -0.000000000000000000, -1.000000000000000000 ) ) ;
#134152 = CARTESIAN_POINT ( 'NONE',  ( 117.5995968585647944, -6.109999999999997655, -1.637169565754160283 ) ) ;
#134153 = ORIENTED_EDGE ( 'NONE', *, *, #40698, .F. ) ;
#134154 = EDGE_CURVE ( 'NONE', #83338, #28064, #104296, .T. ) ;
#134155 = VERTEX_POINT ( 'NONE', #34801 ) ;
#134156 = LINE ( 'NONE', #13055, #112578 ) ;
#134157 = ORIENTED_EDGE ( 'NONE', *, *, #67563, .F. ) ;
#134158 = ORIENTED_EDGE ( 'NONE', *, *, #75739, .T. ) ;
#134159 = EDGE_LOOP ( 'NONE', ( #80515, #132950, #71178, #122231, #136358 ) ) ;
#134160 = CARTESIAN_POINT ( 'NONE',  ( 42.29974487139158157, -27.71228299555235708, 4.000000000000000000 ) ) ;
#134161 = EDGE_CURVE ( 'NONE', #40586, #69387, #57287, .T. ) ;
#134162 = CARTESIAN_POINT ( 'NONE',  ( 4.004569808101885897, 6.871911579029510442, -3.967499999999998916 ) ) ;
#134163 = ADVANCED_FACE ( 'NONE', ( #135545 ), #80456, .F. ) ;
#134164 = EDGE_CURVE ( 'NONE', #69243, #138595, #113772, .T. ) ;
#134165 = CARTESIAN_POINT ( 'NONE',  ( 32.14126352523144448, 4.472830434245836706, 4.472830434245840259 ) ) ;
#134166 = EDGE_CURVE ( 'NONE', #121813, #116985, #124646, .T. ) ;
#134167 = EDGE_LOOP ( 'NONE', ( #119400, #100390, #67669 ) ) ;
#134169 = ADVANCED_FACE ( 'NONE', ( #25323 ), #69589, .T. ) ;
#134168 = DIRECTION ( 'NONE',  ( 0.7071067811865487940, 0.7071067811865463515, 0.000000000000000000 ) ) ;
#134170 = ORIENTED_EDGE ( 'NONE', *, *, #67133, .F. ) ;
#134171 = EDGE_LOOP ( 'NONE', ( #95114, #128363, #813, #120065 ) ) ;
#134172 = ORIENTED_EDGE ( 'NONE', *, *, #38227, .F. ) ;
#134173 = EDGE_CURVE ( 'NONE', #56006, #52354, #28909, .T. ) ;
#134174 = EDGE_CURVE ( 'NONE', #65622, #137194, #127503, .T. ) ;
#134175 = DIRECTION ( 'NONE',  ( 0.7071067811865487940, -0.7071067811865463515, 0.000000000000000000 ) ) ;
#134176 = DIRECTION ( 'NONE',  ( -0.5735764363510507113, 0.8191520442889885789, 1.003171929053520926E-16 ) ) ;
#134177 = EDGE_LOOP ( 'NONE', ( #15105, #16909, #131480, #109943, #97890, #88502 ) ) ;
#134178 = FACE_OUTER_BOUND ( 'NONE', #47168, .T. ) ;
#134179 = ADVANCED_FACE ( 'NONE', ( #7845 ), #62261, .F. ) ;
#134180 = AXIS2_PLACEMENT_3D ( 'NONE', #110425, #122019, #133644 ) ;
#134181 = DIRECTION ( 'NONE',  ( 0.3543493200069162685, -0.000000000000000000, -0.9351131265310288487 ) ) ;
#134182 = AXIS2_PLACEMENT_3D ( 'NONE', #59904, #94638, #26549 ) ;
#134183 = AXIS2_PLACEMENT_3D ( 'NONE', #58873, #97, #88607 ) ;
#134184 = CARTESIAN_POINT ( 'NONE',  ( 28.49999999999981171, -14.94781430457067550, 5.000000000000000000 ) ) ;
#134185 = VECTOR ( 'NONE', #59170, 1000.000000000000227 ) ;
#134186 = EDGE_CURVE ( 'NONE', #126057, #50446, #27451, .T. ) ;
#134187 = FACE_BOUND ( 'NONE', #685, .T. ) ;
#134188 = ORIENTED_EDGE ( 'NONE', *, *, #80572, .T. ) ;
#134189 = ADVANCED_FACE ( 'NONE', ( #105029 ), #72456, .T. ) ;
#134190 = DIRECTION ( 'NONE',  ( 0.5735764363510453823, -0.8191520442889923537, 1.003171929053525486E-16 ) ) ;
#134191 = PLANE ( 'NONE',  #115500 ) ;
#134192 = CARTESIAN_POINT ( 'NONE',  ( -32.54016161050240186, 18.75929247661552424, 8.305906642995411815 ) ) ;
#134193 = CARTESIAN_POINT ( 'NONE',  ( -34.92500000000001137, 22.22500000000000142, 5.000000000000000000 ) ) ;
#134194 = EDGE_LOOP ( 'NONE', ( #102083, #18464, #106481, #88031 ) ) ;
#134195 = CARTESIAN_POINT ( 'NONE',  ( 25.49999999999982592, -4.796895815300992183, -3.611700055028623790 ) ) ;
#134196 = ORIENTED_EDGE ( 'NONE', *, *, #45840, .F. ) ;
#134197 = ORIENTED_EDGE ( 'NONE', *, *, #111637, .F. ) ;
#134198 = EDGE_CURVE ( 'NONE', #70580, #33680, #117314, .T. ) ;
#134199 = ORIENTED_EDGE ( 'NONE', *, *, #121299, .T. ) ;
#134200 = CARTESIAN_POINT ( 'NONE',  ( 49.05793019189810877, 6.110000000000000320, -1.637169565754156064 ) ) ;
#134201 = ORIENTED_EDGE ( 'NONE', *, *, #133389, .T. ) ;
#134202 = VECTOR ( 'NONE', #141561, 1000.000000000000000 ) ;
#134203 = DIRECTION ( 'NONE',  ( -0.7071067811865486830, -0.7071067811865464625, 0.000000000000000000 ) ) ;
#134204 = LINE ( 'NONE', #70420, #91336 ) ;
#134205 = EDGE_LOOP ( 'NONE', ( #13127, #91198, #37349, #55077 ) ) ;
#134206 = CARTESIAN_POINT ( 'NONE',  ( -51.18398860626899705, 28.73617430169823095, 5.000000000000000000 ) ) ;
#134207 = LINE ( 'NONE', #12402, #99020 ) ;
#134208 = AXIS2_PLACEMENT_3D ( 'NONE', #96246, #117992, #140488 ) ;
#134209 = CIRCLE ( 'NONE', #60225, 0.5000000000000000000 ) ;
#134210 = AXIS2_PLACEMENT_3D ( 'NONE', #142527, #22135, #55516 ) ;
#134211 = PLANE ( 'NONE',  #50251 ) ;
#134212 = LINE ( 'NONE', #79147, #18109 ) ;
#134213 = LINE ( 'NONE', #79148, #25094 ) ;
#134214 = DIRECTION ( 'NONE',  ( -1.000000000000000000, -1.224606353822377258E-16, -0.000000000000000000 ) ) ;
#134215 = VERTEX_POINT ( 'NONE', #94846 ) ;
#134216 = ADVANCED_FACE ( 'NONE', ( #16579 ), #107164, .T. ) ;
#134217 = ORIENTED_EDGE ( 'NONE', *, *, #126834, .T. ) ;
#134218 = ORIENTED_EDGE ( 'NONE', *, *, #50078, .T. ) ;
#134219 = ORIENTED_EDGE ( 'NONE', *, *, #14392, .F. ) ;
#134220 = AXIS2_PLACEMENT_3D ( 'NONE', #82127, #126301, #115380 ) ;
#134221 = CARTESIAN_POINT ( 'NONE',  ( -17.99451991528748351, 28.92564299267950645, 4.000000000000000000 ) ) ;
#134222 = ORIENTED_EDGE ( 'NONE', *, *, #102941, .F. ) ;
#134223 = MECHANICAL_DESIGN_GEOMETRIC_PRESENTATION_REPRESENTATION (  '', ( #25110 ), #64788 ) ;
#134224 = VERTEX_POINT ( 'NONE', #128233 ) ;
#134225 = CIRCLE ( 'NONE', #81045, 2.055000000000000604 ) ;
#134226 = AXIS2_PLACEMENT_3D ( 'NONE', #66061, #10901, #77646 ) ;
#134227 = DIRECTION ( 'NONE',  ( 0.7071067811865487940, 0.7071067811865463515, 0.000000000000000000 ) ) ;
#134228 = ORIENTED_EDGE ( 'NONE', *, *, #49619, .F. ) ;
#134229 = VECTOR ( 'NONE', #86530, 1000.000000000000000 ) ;
#134230 = DIRECTION ( 'NONE',  ( 0.7071067811865487940, 0.7071067811865463515, 0.000000000000000000 ) ) ;
#134231 = EDGE_CURVE ( 'NONE', #53824, #24327, #17306, .T. ) ;
#134232 = CARTESIAN_POINT ( 'NONE',  ( -8.200031220168323642, 8.259292476615634371, 16.85664084051843048 ) ) ;
#134233 = CARTESIAN_POINT ( 'NONE',  ( 25.00456980810188767, 6.871911579029510442, -3.967499999999998916 ) ) ;
#134234 = CARTESIAN_POINT ( 'NONE',  ( 25.17183060077629619, -2.240707523384255939, 4.000000000000000000 ) ) ;
#134235 = VERTEX_POINT ( 'NONE', #7106 ) ;
#134236 = CARTESIAN_POINT ( 'NONE',  ( 106.8079301918981230, -6.109999999999999432, 1.637169565754158507 ) ) ;
#134238 = EDGE_CURVE ( 'NONE', #92174, #126797, #52086, .T. ) ;
#134237 = LINE ( 'NONE', #79173, #67558 ) ;
#134239 = DIRECTION ( 'NONE',  ( -0.000000000000000000, 0.000000000000000000, 1.000000000000000000 ) ) ;
#134240 = DIRECTION ( 'NONE',  ( 0.000000000000000000, -1.000000000000000000, 0.000000000000000000 ) ) ;
#134241 = AXIS2_PLACEMENT_3D ( 'NONE', #12998, #24603, #102188 ) ;
#134243 = ORIENTED_EDGE ( 'NONE', *, *, #33880, .F. ) ;
#134242 = CARTESIAN_POINT ( 'NONE',  ( 54.18398860626899705, 28.73617430169825226, 5.000000000000000000 ) ) ;
#134244 = LINE ( 'NONE', #45125, #20840 ) ;
#134245 = VERTEX_POINT ( 'NONE', #115879 ) ;
#134246 = FACE_OUTER_BOUND ( 'NONE', #52253, .T. ) ;
#134247 = CARTESIAN_POINT ( 'NONE',  ( 34.92499999999998295, 3.759292476615685441, 4.255531930566164078 ) ) ;
#134248 = FACE_OUTER_BOUND ( 'NONE', #129954, .T. ) ;
#134249 = ORIENTED_EDGE ( 'NONE', *, *, #73941, .T. ) ;
#134250 = CARTESIAN_POINT ( 'NONE',  ( 58.42753753994787047, -47.70829528212280479, 34.92499999999998295 ) ) ;
#134251 = EDGE_CURVE ( 'NONE', #71156, #69437, #96262, .T. ) ;
#134252 = CARTESIAN_POINT ( 'NONE',  ( 131.8806778009765708, -49.14999999999999147, 40.92499999999998295 ) ) ;
#134253 = LINE ( 'NONE', #44412, #127841 ) ;
#134254 = VERTEX_POINT ( 'NONE', #95579 ) ;
#134255 = VECTOR ( 'NONE', #55239, 1000.000000000000000 ) ;
#134256 = DIRECTION ( 'NONE',  ( -0.000000000000000000, -0.3543493200069152693, 0.9351131265310292928 ) ) ;
#134257 = VERTEX_POINT ( 'NONE', #30331 ) ;
#134258 = LINE ( 'NONE', #23320, #129465 ) ;
#134261 = EDGE_CURVE ( 'NONE', #82848, #10331, #140508, .T. ) ;
#134260 = ORIENTED_EDGE ( 'NONE', *, *, #123066, .F. ) ;
#134259 = DIRECTION ( 'NONE',  ( 0.7071067811865487940, 0.7071067811865463515, 0.000000000000000000 ) ) ;
#134262 = ORIENTED_EDGE ( 'NONE', *, *, #15182, .T. ) ;
#134263 = CARTESIAN_POINT ( 'NONE',  ( 42.18398860626899705, 28.73617430169816700, 5.000000000000000000 ) ) ;
#134264 = CARTESIAN_POINT ( 'NONE',  ( -9.183988606268997046, 28.73617430169793607, 5.000000000000000000 ) ) ;
#134265 = ORIENTED_EDGE ( 'NONE', *, *, #40518, .T. ) ;
#134266 = CARTESIAN_POINT ( 'NONE',  ( -22.49999999999984723, 15.43112307739202826, 4.000000000000000000 ) ) ;
#134267 = FACE_OUTER_BOUND ( 'NONE', #102208, .T. ) ;
#134268 = LINE ( 'NONE', #98755, #67757 ) ;
#134269 = EDGE_LOOP ( 'NONE', ( #13661, #85178, #22319, #34764 ) ) ;
#134270 = DIRECTION ( 'NONE',  ( 0.7071067811865487940, 0.7071067811865463515, 0.000000000000000000 ) ) ;
#134271 = LINE ( 'NONE', #101623, #7332 ) ;
#134272 = DIRECTION ( 'NONE',  ( -0.7071067811865487940, 0.7071067811865463515, -0.000000000000000000 ) ) ;
#134273 = CARTESIAN_POINT ( 'NONE',  ( -30.48921356237309510, -27.52281430457076894, 5.000000000000000000 ) ) ;
#134274 = CARTESIAN_POINT ( 'NONE',  ( 125.9076131992937775, -6.355826491133410805, 4.106188095953474892 ) ) ;
#134275 = CARTESIAN_POINT ( 'NONE',  ( -48.29974487139158867, -27.71228299555239971, 4.000000000000000000 ) ) ;
#134276 = ORIENTED_EDGE ( 'NONE', *, *, #43091, .F. ) ;
#134277 = EDGE_LOOP ( 'NONE', ( #134527, #48657, #49922, #102358 ) ) ;
#134278 = ORIENTED_EDGE ( 'NONE', *, *, #141542, .T. ) ;
#134279 = LINE ( 'NONE', #112517, #83649 ) ;
#134280 = AXIS2_PLACEMENT_3D ( 'NONE', #70096, #112135, #1187 ) ;
#134281 = EDGE_CURVE ( 'NONE', #11065, #117806, #19451, .T. ) ;
#134282 = EDGE_LOOP ( 'NONE', ( #92604, #118499, #86566, #51937 ) ) ;
#134283 = VERTEX_POINT ( 'NONE', #41195 ) ;
#134284 = ORIENTED_EDGE ( 'NONE', *, *, #130561, .T. ) ;
#134285 = VECTOR ( 'NONE', #1630, 1000.000000000000000 ) ;
#134286 = DIRECTION ( 'NONE',  ( 0.7071067811865487940, 0.7071067811865463515, 0.000000000000000000 ) ) ;
#134287 = DIRECTION ( 'NONE',  ( 0.000000000000000000, -1.000000000000000000, 0.000000000000000000 ) ) ;
#134288 = AXIS2_PLACEMENT_3D ( 'NONE', #49383, #103016, #3652 ) ;
#134289 = VECTOR ( 'NONE', #52227, 1000.000000000000000 ) ;
#134290 = VECTOR ( 'NONE', #52897, 1000.000000000000227 ) ;
#134291 = ORIENTED_EDGE ( 'NONE', *, *, #89116, .F. ) ;
#134292 =( BOUNDED_CURVE ( )  B_SPLINE_CURVE ( 3, ( #62005, #38103, #93883, #6832 ),
 .UNSPECIFIED., .F., .T. ) 
 B_SPLINE_CURVE_WITH_KNOTS ( ( 4, 4 ),
 ( 5.005968288816749379, 5.074607125596352297 ),
 .UNSPECIFIED. ) 
 CURVE ( )  GEOMETRIC_REPRESENTATION_ITEM ( )  RATIONAL_B_SPLINE_CURVE ( ( 1.000000000000000000, 0.9996074310407765395, 0.9996074310407765395, 1.000000000000000000 ) ) 
 REPRESENTATION_ITEM ( '' )  );
#134293 = CARTESIAN_POINT ( 'NONE',  ( 24.29974487139158867, -27.71228299555223273, 4.000000000000000000 ) ) ;
#134294 = CARTESIAN_POINT ( 'NONE',  ( 25.39999999999998792, 7.299101704619667785, 2.356075668539098444 ) ) ;
#134295 = STYLED_ITEM ( 'NONE', ( #139408 ), #114719 ) ;
#134296 = DIRECTION ( 'NONE',  ( 1.000000000000000000, 0.000000000000000000, 0.000000000000000000 ) ) ;
#134297 = LINE ( 'NONE', #154, #106582 ) ;
#134298 = CARTESIAN_POINT ( 'NONE',  ( 119.4379301918981042, -6.110000000000001208, 1.637169565754158951 ) ) ;
#134299 = ORIENTED_EDGE ( 'NONE', *, *, #47265, .T. ) ;
#134300 = EDGE_CURVE ( 'NONE', #127633, #129923, #90213, .T. ) ;
#134301 = PLANE ( 'NONE',  #139076 ) ;
#134302 = CARTESIAN_POINT ( 'NONE',  ( -6.707013264292997157, -21.74070752338405654, 4.999753212805220670 ) ) ;
#134303 = PLANE ( 'NONE',  #123654 ) ;
#134304 = VECTOR ( 'NONE', #65692, 1000.000000000000000 ) ;
#134305 = DIRECTION ( 'NONE',  ( -0.3543493200069162685, -0.000000000000000000, -0.9351131265310288487 ) ) ;
#134306 = CARTESIAN_POINT ( 'NONE',  ( -3.183988606268992161, 28.73617430169789699, 5.000000000000000000 ) ) ;
#134307 = DIRECTION ( 'NONE',  ( 0.000000000000000000, -1.000000000000000000, 0.000000000000000000 ) ) ;
#134308 = CARTESIAN_POINT ( 'NONE',  ( 27.29974487139158512, -27.71228299555225405, 4.000000000000000000 ) ) ;
#134309 = CARTESIAN_POINT ( 'NONE',  ( 45.57919371712955581, 3.975000000000002753, -6.884901960086283523 ) ) ;
#134310 = DIRECTION ( 'NONE',  ( -0.7071067811865487940, 0.7071067811865463515, -0.000000000000000000 ) ) ;
#134311 = PLANE ( 'NONE',  #122493 ) ;
#134312 = ORIENTED_EDGE ( 'NONE', *, *, #56337, .F. ) ;
#134313 = EDGE_LOOP ( 'NONE', ( #107731, #111794, #137502, #88910 ) ) ;
#134314 = CARTESIAN_POINT ( 'NONE',  ( 43.00000000000000000, 0.000000000000000000, -7.950000000000000178 ) ) ;
#134315 = CARTESIAN_POINT ( 'NONE',  ( -24.18398860626899705, 28.73617430169804265, 5.000000000000000000 ) ) ;
#134316 = VECTOR ( 'NONE', #6565, 999.9999999999998863 ) ;
#134317 = VECTOR ( 'NONE', #56428, 999.9999999999998863 ) ;
#134318 = VERTEX_POINT ( 'NONE', #128924 ) ;
#134319 = CARTESIAN_POINT ( 'NONE',  ( 127.0000000000000568, -4.122959376248258145, -4.874446087595273092 ) ) ;
#134320 = ADVANCED_FACE ( 'NONE', ( #93453 ), #83292, .F. ) ;
#134321 = CARTESIAN_POINT ( 'NONE',  ( -25.39999999999996305, 3.061616997868383141E-16, -2.500000000000000000 ) ) ;
#134322 = CIRCLE ( 'NONE', #136666, 2.055000000000000604 ) ;
#134323 = CARTESIAN_POINT ( 'NONE',  ( 41.12543019189809712, 5.291415217122919401, 3.055000000000002824 ) ) ;
#134324 = ORIENTED_EDGE ( 'NONE', *, *, #3261, .T. ) ;
#134325 = VECTOR ( 'NONE', #76534, 1000.000000000000000 ) ;
#134326 = CARTESIAN_POINT ( 'NONE',  ( -8.576721541936407789, 11.25929247661560240, 17.85071094206586650 ) ) ;
#134327 = ORIENTED_EDGE ( 'NONE', *, *, #138389, .T. ) ;
#134328 = LINE ( 'NONE', #125605, #84344 ) ;
#134329 = AXIS2_PLACEMENT_3D ( 'NONE', #38373, #27466, #71729 ) ;
#134330 = DIRECTION ( 'NONE',  ( 0.5735764363510451602, 0.8191520442889924647, 0.000000000000000000 ) ) ;
#134331 = CARTESIAN_POINT ( 'NONE',  ( -32.67183060077624646, 5.259292476615669010, 4.000000000000000000 ) ) ;
#134332 = PLANE ( 'NONE',  #81235 ) ;
#134333 = ORIENTED_EDGE ( 'NONE', *, *, #41060, .T. ) ;
#134334 = LINE ( 'NONE', #124156, #83628 ) ;
#134335 = ORIENTED_EDGE ( 'NONE', *, *, #56610, .F. ) ;
#134336 = VECTOR ( 'NONE', #73635, 1000.000000000000000 ) ;
#134337 = CARTESIAN_POINT ( 'NONE',  ( 39.30836038379622011, 7.949999999999996625, 2.130196079827431088 ) ) ;
#134338 = CARTESIAN_POINT ( 'NONE',  ( -9.489213562373095101, -27.52281430457062328, 5.000000000000000000 ) ) ;
#134339 = PLANE ( 'NONE',  #46948 ) ;
#134340 = AXIS2_PLACEMENT_3D ( 'NONE', #12509, #79256, #24120 ) ;
#134341 = DIRECTION ( 'NONE',  ( -0.3543493200069162685, -0.000000000000000000, -0.9351131265310288487 ) ) ;
#134342 = CARTESIAN_POINT ( 'NONE',  ( 12.51280225271498736, 2.500000000000000444, 3.061616997868383634E-16 ) ) ;
#134343 = EDGE_CURVE ( 'NONE', #68198, #127842, #103341, .T. ) ;
#134344 = ORIENTED_EDGE ( 'NONE', *, *, #37440, .T. ) ;
#134345 = STYLED_ITEM ( 'NONE', ( #17035 ), #41826 ) ;
#134346 = CARTESIAN_POINT ( 'NONE',  ( 87.28752705046288440, 0.000000000000000000, -7.949999999999998401 ) ) ;
#134347 = CARTESIAN_POINT ( 'NONE',  ( 58.97459685856478018, 1.637169565754164058, -6.109999999999996767 ) ) ;
#134348 = EDGE_CURVE ( 'NONE', #113319, #60930, #82576, .T. ) ;
#134349 = FACE_OUTER_BOUND ( 'NONE', #65449, .T. ) ;
#134351 = ADVANCED_FACE ( 'NONE', ( #64387 ), #119451, .F. ) ;
#134350 = FACE_OUTER_BOUND ( 'NONE', #88714, .T. ) ;
#134353 = VERTEX_POINT ( 'NONE', #20865 ) ;
#134352 = LINE ( 'NONE', #35049, #52531 ) ;
#134354 = ORIENTED_EDGE ( 'NONE', *, *, #7143, .T. ) ;
#134355 = VECTOR ( 'NONE', #138573, 1000.000000000000000 ) ;
#134356 = LINE ( 'NONE', #24857, #139636 ) ;
#134357 = ORIENTED_EDGE ( 'NONE', *, *, #90866, .T. ) ;
#134358 = ADVANCED_FACE ( 'NONE', ( #131794 ), #22982, .F. ) ;
#134359 = CARTESIAN_POINT ( 'NONE',  ( 7.499999999999947597, 6.431123077392115306, 4.000000000000000000 ) ) ;
#134360 = EDGE_LOOP ( 'NONE', ( #14100, #87438, #31973, #40935, #110892, #121377 ) ) ;
#134361 = FACE_OUTER_BOUND ( 'NONE', #82334, .T. ) ;
#134362 = LINE ( 'NONE', #45236, #57233 ) ;
#134363 = VECTOR ( 'NONE', #134059, 1000.000000000000000 ) ;
#134364 = CARTESIAN_POINT ( 'NONE',  ( 0.8348608954644654023, 0.3999999999999995226, 2.317232259782045833 ) ) ;
#134365 = ADVANCED_FACE ( 'NONE', ( #65863 ), #9239, .F. ) ;
#134366 = FACE_BOUND ( 'NONE', #71134, .T. ) ;
#134367 = ADVANCED_FACE ( 'NONE', ( #31765 ), #15374, .T. ) ;
#134368 = DIRECTION ( 'NONE',  ( -0.000000000000000000, 0.3543493200069153248, 0.9351131265310292928 ) ) ;
#134369 = PLANE ( 'NONE',  #90714 ) ;
#134370 = PLANE ( 'NONE',  #13198 ) ;
#134372 = ORIENTED_EDGE ( 'NONE', *, *, #121401, .F. ) ;
#134371 = DIRECTION ( 'NONE',  ( 1.000000000000000000, 0.000000000000000000, 0.000000000000000000 ) ) ;
#134373 = CIRCLE ( 'NONE', #25470, 4.000000000000000000 ) ;
#134374 = CARTESIAN_POINT ( 'NONE',  ( 34.92499999999998295, -5.337538124160927211, 4.000000000000000000 ) ) ;
#134375 = EDGE_CURVE ( 'NONE', #38197, #81300, #21602, .T. ) ;
#134376 = ORIENTED_EDGE ( 'NONE', *, *, #4194, .F. ) ;
#134377 = ORIENTED_EDGE ( 'NONE', *, *, #64308, .T. ) ;
#134378 = CARTESIAN_POINT ( 'NONE',  ( 71.37043019189812298, -3.055000000000001492, 5.291415217122917625 ) ) ;
#134379 = ORIENTED_EDGE ( 'NONE', *, *, #7843, .T. ) ;
#134380 = LINE ( 'NONE', #46704, #139072 ) ;
#134381 = VERTEX_POINT ( 'NONE', #32484 ) ;
#134382 = CARTESIAN_POINT ( 'NONE',  ( 33.70710678118631165, -18.74070752338409562, 5.000000000000000000 ) ) ;
#134383 = ADVANCED_FACE ( 'NONE', ( #88296 ), #41937, .F. ) ;
#134384 = AXIS2_PLACEMENT_3D ( 'NONE', #98417, #46211, #9963 ) ;
#134385 = CARTESIAN_POINT ( 'NONE',  ( 14.81601139373099585, 28.73617430169776910, 5.000000000000000000 ) ) ;
#134386 = AXIS2_PLACEMENT_3D ( 'NONE', #87262, #19144, #30008 ) ;
#134387 = CARTESIAN_POINT ( 'NONE',  ( -31.64175702458840789, 15.75929247661556332, 19.34181609438707383 ) ) ;
#134388 = CARTESIAN_POINT ( 'NONE',  ( 7.122370700763592133, -39.92999999999999972, 19.06900128115122328 ) ) ;
#134389 = PLANE ( 'NONE',  #1785 ) ;
#134390 = CARTESIAN_POINT ( 'NONE',  ( -3.693269933095963964, -3.740707523384241728, 12.88036043432868460 ) ) ;
#134391 = CARTESIAN_POINT ( 'NONE',  ( -5.999999999999960032, -15.41253812416059432, 4.000000000000000000 ) ) ;
#134392 = ORIENTED_EDGE ( 'NONE', *, *, #80877, .T. ) ;
#134393 = ADVANCED_FACE ( 'NONE', ( #96968 ), #42665, .F. ) ;
#134394 = VECTOR ( 'NONE', #26003, 1000.000000000000000 ) ;
#134395 = MECHANICAL_DESIGN_GEOMETRIC_PRESENTATION_REPRESENTATION (  '', ( #104343 ), #129823 ) ;
#134396 = VECTOR ( 'NONE', #59387, 1000.000000000000227 ) ;
#134397 = ORIENTED_EDGE ( 'NONE', *, *, #127373, .F. ) ;
#134398 = DIRECTION ( 'NONE',  ( -0.7071067811865487940, 0.7071067811865463515, 0.000000000000000000 ) ) ;
#134399 = CARTESIAN_POINT ( 'NONE',  ( 6.707013264292989163, -21.74070752338407075, 4.999753212805213565 ) ) ;
#134400 = ORIENTED_EDGE ( 'NONE', *, *, #76954, .T. ) ;
#134401 = CIRCLE ( 'NONE', #2406, 2.055000000000001048 ) ;
#134402 = ORIENTED_EDGE ( 'NONE', *, *, #38277, .T. ) ;
#134403 = ORIENTED_EDGE ( 'NONE', *, *, #80475, .F. ) ;
#134404 = CARTESIAN_POINT ( 'NONE',  ( 30.47959685856476852, 6.109999999999999432, 1.637169565754164280 ) ) ;
#134405 = EDGE_LOOP ( 'NONE', ( #35251, #112455, #67258, #75008 ) ) ;
#134406 = AXIS2_PLACEMENT_3D ( 'NONE', #83311, #94864, #37680 ) ;
#134407 = CARTESIAN_POINT ( 'NONE',  ( -27.70710678118633652, -12.74070752338415247, 5.000000000000000000 ) ) ;
#134408 = EDGE_CURVE ( 'NONE', #139225, #98928, #142666, .T. ) ;
#134409 = CARTESIAN_POINT ( 'NONE',  ( -1.537096858564780844, -3.967499999999994476, 6.871911579029513106 ) ) ;
#134410 = CARTESIAN_POINT ( 'NONE',  ( 34.92499999999998295, 2.464645009310418633, -2.487937186831653325 ) ) ;
#134411 = ORIENTED_EDGE ( 'NONE', *, *, #119747, .T. ) ;
#134412 = CARTESIAN_POINT ( 'NONE',  ( -34.92500000000001137, 22.22500000000000142, 4.000000000000000000 ) ) ;
#134413 = CARTESIAN_POINT ( 'NONE',  ( -19.93618820137057668, -0.2700000000508183118, -36.99999999997771738 ) ) ;
#134414 = VECTOR ( 'NONE', #94811, 1000.000000000000000 ) ;
#134415 = CARTESIAN_POINT ( 'NONE',  ( -9.005480084712511157, 28.92564299267931816, 4.000000000000000000 ) ) ;
#134417 = ORIENTED_EDGE ( 'NONE', *, *, #10733, .F. ) ;
#134416 = CARTESIAN_POINT ( 'NONE',  ( 72.48921356237309510, -27.52281430457106026, 5.000000000000000000 ) ) ;
#134418 = ORIENTED_EDGE ( 'NONE', *, *, #2361, .F. ) ;
#134419 = CYLINDRICAL_SURFACE ( 'NONE', #49597, 3.000000000000002665 ) ;
#134420 = CARTESIAN_POINT ( 'NONE',  ( -33.49816348513935793, -17.24070752338410628, 8.407044977365300653 ) ) ;
#134421 = CARTESIAN_POINT ( 'NONE',  ( -45.48921356237309510, -27.52281430457087197, 5.000000000000000000 ) ) ;
#134422 = ORIENTED_EDGE ( 'NONE', *, *, #103479, .T. ) ;
#134423 = VECTOR ( 'NONE', #40042, 1000.000000000000227 ) ;
#134424 = DIRECTION ( 'NONE',  ( -0.6830127018922181881, 0.6830127018922202975, -0.2588190451025214056 ) ) ;
#134425 = FACE_OUTER_BOUND ( 'NONE', #124015, .T. ) ;
#134426 = AXIS2_PLACEMENT_3D ( 'NONE', #142237, #32758, #87120 ) ;
#134427 = EDGE_CURVE ( 'NONE', #109534, #66627, #98700, .T. ) ;
#134429 = DIRECTION ( 'NONE',  ( 0.7071067811865487940, -0.7071067811865463515, 0.000000000000000000 ) ) ;
#134428 = VECTOR ( 'NONE', #66191, 1000.000000000000000 ) ;
#134430 = PLANE ( 'NONE',  #72600 ) ;
#134431 = CYLINDRICAL_SURFACE ( 'NONE', #94834, 1.749999999999999778 ) ;
#134432 = AXIS2_PLACEMENT_3D ( 'NONE', #49609, #50300, #16190 ) ;
#134433 = CARTESIAN_POINT ( 'NONE',  ( -21.81246187583931473, -22.22500000000000142, 4.000000000000000000 ) ) ;
#134434 = PLANE ( 'NONE',  #16689 ) ;
#134435 = DIRECTION ( 'NONE',  ( 0.7071067811865487940, 0.7071067811865463515, 0.000000000000000000 ) ) ;
#134436 = CARTESIAN_POINT ( 'NONE',  ( -16.49999999999989697, -14.70932175296479549, -11.46312253303834261 ) ) ;
#134438 = EDGE_CURVE ( 'NONE', #93683, #26697, #20148, .T. ) ;
#134437 = VERTEX_POINT ( 'NONE', #53520 ) ;
#134439 = VECTOR ( 'NONE', #122845, 1000.000000000000000 ) ;
#134440 = VERTEX_POINT ( 'NONE', #97726 ) ;
#134441 = FILL_AREA_STYLE_COLOUR ( '', #3906 ) ;
#134442 = CARTESIAN_POINT ( 'NONE',  ( 32.99999999999977263, -19.06887692260762179, 4.000000000000000000 ) ) ;
#134443 = LINE ( 'NONE', #124974, #29673 ) ;
#134444 = ORIENTED_EDGE ( 'NONE', *, *, #87535, .F. ) ;
#134445 = VECTOR ( 'NONE', #42471, 1000.000000000000000 ) ;
#134446 = LINE ( 'NONE', #24935, #108570 ) ;
#134447 = DIRECTION ( 'NONE',  ( -0.6830127018922181881, 0.6830127018922202975, -0.2588190451025214056 ) ) ;
#134448 = DIRECTION ( 'NONE',  ( -0.000000000000000000, 0.3543493200069153248, 0.9351131265310292928 ) ) ;
#134449 = ORIENTED_EDGE ( 'NONE', *, *, #60379, .F. ) ;
#134450 = DIRECTION ( 'NONE',  ( -0.000000000000000000, 0.000000000000000000, 1.000000000000000000 ) ) ;
#134451 = VECTOR ( 'NONE', #110899, 1000.000000000000000 ) ;
#134452 = CARTESIAN_POINT ( 'NONE',  ( 35.99451991528749772, 28.92564299267963079, 4.000000000000000000 ) ) ;
#134453 = CARTESIAN_POINT ( 'NONE',  ( 29.99999999999979039, 15.45873954670187445, -0.03131636524301203289 ) ) ;
#134454 = CARTESIAN_POINT ( 'NONE',  ( 53.43293019189810167, 1.637169565754156730, 6.110000000000001208 ) ) ;
#134455 = DIRECTION ( 'NONE',  ( -0.3543493200069162685, -0.000000000000000000, -0.9351131265310288487 ) ) ;
#134456 = CARTESIAN_POINT ( 'NONE',  ( 0.000000000000000000, -4.999999999999999112, -7.627214432543508948 ) ) ;
#134457 = PLANE ( 'NONE',  #27881 ) ;
#134458 = EDGE_CURVE ( 'NONE', #60511, #109568, #534, .T. ) ;
#134459 = ORIENTED_EDGE ( 'NONE', *, *, #1875, .T. ) ;
#134460 = CARTESIAN_POINT ( 'NONE',  ( 22.07159235450331991, -2.500000000000000000, 3.061616997868384127E-16 ) ) ;
#134461 = EDGE_LOOP ( 'NONE', ( #32245, #77166, #134622, #100130 ) ) ;
#134462 = VECTOR ( 'NONE', #61676, 999.9999999999998863 ) ;
#134463 = CARTESIAN_POINT ( 'NONE',  ( -30.48921356237309510, -27.52281430457076894, 5.000000000000000000 ) ) ;
#134464 = LINE ( 'NONE', #135197, #76273 ) ;
#134465 = DIRECTION ( 'NONE',  ( -0.6830127018922180770, -0.6830127018922204085, -0.2588190451025213501 ) ) ;
#134466 = CARTESIAN_POINT ( 'NONE',  ( -3.489213562373097322, -27.52281430457057709, 5.000000000000000000 ) ) ;
#134467 = ADVANCED_FACE ( 'NONE', ( #65129 ), #99123, .F. ) ;
#134468 = CARTESIAN_POINT ( 'NONE',  ( 0.000000000000000000, 0.000000000000000000, 5.000000000000000000 ) ) ;
#134469 = CARTESIAN_POINT ( 'NONE',  ( 48.18398860626899705, 28.73617430169820608, 5.000000000000000000 ) ) ;
#134470 = ORIENTED_EDGE ( 'NONE', *, *, #12421, .T. ) ;
#134471 = ADVANCED_FACE ( 'NONE', ( #89020 ), #33916, .F. ) ;
#134472 = ORIENTED_EDGE ( 'NONE', *, *, #49133, .T. ) ;
#134473 = LINE ( 'NONE', #79420, #57977 ) ;
#134474 = CARTESIAN_POINT ( 'NONE',  ( -24.48921356237309510, -27.52281430457072631, 5.000000000000000000 ) ) ;
#134475 = UNCERTAINTY_MEASURE_WITH_UNIT (LENGTH_MEASURE( 1.000000000000000082E-05 ), #45802, 'distance_accuracy_value', 'NONE');
#134476 = AXIS2_PLACEMENT_3D ( 'NONE', #127706, #116086, #3723 ) ;
#134477 = AXIS2_PLACEMENT_3D ( 'NONE', #23118, #134073, #10824 ) ;
#134478 = CARTESIAN_POINT ( 'NONE',  ( 11.99451991528749417, 28.92564299267946382, 4.000000000000000000 ) ) ;
#134479 = CARTESIAN_POINT ( 'NONE',  ( 116.6458333333333570, 2.130196079827470168, -7.949999999999977973 ) ) ;
#134480 = CARTESIAN_POINT ( 'NONE',  ( 76.78752705046289861, 0.000000000000000000, -7.949999999999998401 ) ) ;
#134481 = FACE_OUTER_BOUND ( 'NONE', #67141, .T. ) ;
#134482 = DIRECTION ( 'NONE',  ( -0.7071067811865486830, 0.7071067811865464625, 0.000000000000000000 ) ) ;
#134483 = VERTEX_POINT ( 'NONE', #132544 ) ;
#134484 = CARTESIAN_POINT ( 'NONE',  ( 70.85416666666667140, -2.130196079827425315, -7.950000000000001066 ) ) ;
#134485 = LINE ( 'NONE', #20699, #141905 ) ;
#134486 = DIRECTION ( 'NONE',  ( -0.7071067811865486830, 0.7071067811865464625, 0.000000000000000000 ) ) ;
#134487 = DIRECTION ( 'NONE',  ( 0.000000000000000000, 0.000000000000000000, 1.000000000000000000 ) ) ;
#134488 = EDGE_LOOP ( 'NONE', ( #118301, #107957, #80581, #128346 ) ) ;
#134489 = VECTOR ( 'NONE', #62073, 1000.000000000000000 ) ;
#134490 = ADVANCED_FACE ( 'NONE', ( #43359 ), #87571, .T. ) ;
#134491 = CARTESIAN_POINT ( 'NONE',  ( 7.014532492589830248, 3.821174125832445049E-16, 0.000000000000000000 ) ) ;
#134492 = AXIS2_PLACEMENT_3D ( 'NONE', #114389, #136139, #36824 ) ;
#134493 = VECTOR ( 'NONE', #80343, 1000.000000000000000 ) ;
#134494 = DIRECTION ( 'NONE',  ( 1.000000000000000000, 1.224606353822377258E-16, 0.000000000000000000 ) ) ;
#134495 = CARTESIAN_POINT ( 'NONE',  ( 65.47959685856477563, 6.109999999999999432, 1.637169565754164280 ) ) ;
#134496 = ORIENTED_EDGE ( 'NONE', *, *, #8699, .T. ) ;
#134498 = ORIENTED_EDGE ( 'NONE', *, *, #9905, .T. ) ;
#134497 = VECTOR ( 'NONE', #120461, 1000.000000000000000 ) ;
#134499 = VECTOR ( 'NONE', #7276, 1000.000000000000000 ) ;
#134500 = VECTOR ( 'NONE', #83517, 999.9999999999998863 ) ;
#134502 = DIRECTION ( 'NONE',  ( 0.000000000000000000, -1.000000000000000000, 0.000000000000000000 ) ) ;
#134501 = AXIS2_PLACEMENT_3D ( 'NONE', #42422, #75747, #54715 ) ;
#134503 = DIRECTION ( 'NONE',  ( 0.7071067811865487940, 0.7071067811865463515, -0.000000000000000000 ) ) ;
#134504 = CARTESIAN_POINT ( 'NONE',  ( 44.45833333333332149, 3.974999999999997424, 6.884901960086288852 ) ) ;
#134505 = CARTESIAN_POINT ( 'NONE',  ( -34.82816939922327748, 12.75929247661559529, 4.000000000000000000 ) ) ;
#134507 = ORIENTED_EDGE ( 'NONE', *, *, #64947, .F. ) ;
#134506 = PLANE ( 'NONE',  #45315 ) ;
#134508 = PLANE ( 'NONE',  #2008 ) ;
#134509 = CARTESIAN_POINT ( 'NONE',  ( 2.241399257802041856, 21.72499999999999432, 5.000000000000000000 ) ) ;
#134510 = FACE_OUTER_BOUND ( 'NONE', #49114, .T. ) ;
#134511 = VECTOR ( 'NONE', #38915, 1000.000000000000000 ) ;
#134512 = DIRECTION ( 'NONE',  ( 0.6830127018922181881, 0.6830127018922202975, -0.2588190451025214056 ) ) ;
#134513 = ORIENTED_EDGE ( 'NONE', *, *, #134014, .T. ) ;
#134515 = EDGE_CURVE ( 'NONE', #36084, #106881, #91840, .T. ) ;
#134514 = VERTEX_POINT ( 'NONE', #125195 ) ;
#134516 = CARTESIAN_POINT ( 'NONE',  ( 55.70876352523143282, -7.482591942790329030E-16, 6.110000000000001208 ) ) ;
#134517 = EDGE_CURVE ( 'NONE', #98656, #128903, #80288, .T. ) ;
#134518 = ORIENTED_EDGE ( 'NONE', *, *, #132574, .F. ) ;
#134519 = AXIS2_PLACEMENT_3D ( 'NONE', #39879, #49332, #93516 ) ;
#134520 = CARTESIAN_POINT ( 'NONE',  ( 24.48921356237309510, -27.52281430457072631, 5.000000000000000000 ) ) ;
#134521 = ADVANCED_FACE ( 'NONE', ( #136065 ), #70151, .F. ) ;
#134522 = DIRECTION ( 'NONE',  ( 0.7071067811865487940, 0.7071067811865463515, -0.000000000000000000 ) ) ;
#134523 = DIRECTION ( 'NONE',  ( -1.000000000000000000, 0.000000000000000000, 0.000000000000000000 ) ) ;
#134524 = VECTOR ( 'NONE', #54070, 999.9999999999998863 ) ;
#134525 = CARTESIAN_POINT ( 'NONE',  ( 125.5000000000000568, -3.922572014496796822, -6.914906274931464480 ) ) ;
#134526 = CARTESIAN_POINT ( 'NONE',  ( 55.24999999999999289, -9.735942053221458872E-16, 7.950000000000000178 ) ) ;
#134527 = ORIENTED_EDGE ( 'NONE', *, *, #22113, .F. ) ;
#134528 = VERTEX_POINT ( 'NONE', #1243 ) ;
#134529 = DIRECTION ( 'NONE',  ( -0.6830127018922180770, -0.6830127018922204085, -0.2588190451025213501 ) ) ;
#134530 = CARTESIAN_POINT ( 'NONE',  ( -17.29187175597492399, -1.888566033147011769, -32.52167028562607243 ) ) ;
#134531 = ADVANCED_FACE ( 'NONE', ( #102015 ), #121866, .T. ) ;
#134532 = EDGE_CURVE ( 'NONE', #53505, #24661, #80988, .T. ) ;
#134533 = ORIENTED_EDGE ( 'NONE', *, *, #110546, .F. ) ;
#134534 = VECTOR ( 'NONE', #46655, 1000.000000000000227 ) ;
#134535 = FILL_AREA_STYLE ('',( #25744 ) ) ;
#134536 = AXIS2_PLACEMENT_3D ( 'NONE', #130301, #118682, #83212 ) ;
#134537 = CARTESIAN_POINT ( 'NONE',  ( -34.75611968250420603, -6.187065745292570362, 4.955485411084898040 ) ) ;
#134538 = CARTESIAN_POINT ( 'NONE',  ( 0.000000000000000000, 0.000000000000000000, 5.000000000000000000 ) ) ;
#134539 = VECTOR ( 'NONE', #123247, 1000.000000000000000 ) ;
#134540 = ORIENTED_EDGE ( 'NONE', *, *, #107714, .T. ) ;
#134541 = ADVANCED_FACE ( 'NONE', ( #113588 ), #14988, .F. ) ;
#134542 = FACE_BOUND ( 'NONE', #29699, .T. ) ;
#134543 = TOROIDAL_SURFACE ( 'NONE', #81251, 3.000000000000000000, 3.000000000000000000 ) ;
#134544 = EDGE_CURVE ( 'NONE', #5991, #126851, #59262, .T. ) ;
#134545 = CARTESIAN_POINT ( 'NONE',  ( 7.251592354503322291, 2.500000000000001776, 0.000000000000000000 ) ) ;
#134546 = CARTESIAN_POINT ( 'NONE',  ( -34.92500000000001137, 22.22500000000000142, 4.000000000000000000 ) ) ;
#134547 = CARTESIAN_POINT ( 'NONE',  ( 36.97502705046289151, -5.819803920172573086, 5.819803920172573086 ) ) ;
#134548 = CARTESIAN_POINT ( 'NONE',  ( 32.99999999999975842, -13.39766691384881092, -10.96608748226473828 ) ) ;
#134549 = CARTESIAN_POINT ( 'NONE',  ( 94.86850992298124652, -32.76500000000005031, -11.46000000000045205 ) ) ;
#134550 = ORIENTED_EDGE ( 'NONE', *, *, #142496, .F. ) ;
#134551 = STYLED_ITEM ( 'NONE', ( #66177 ), #41202 ) ;
#134552 = ORIENTED_EDGE ( 'NONE', *, *, #39841, .T. ) ;
#134553 = CARTESIAN_POINT ( 'NONE',  ( 102.2870968585647802, 3.054999999999997495, 5.291415217122919401 ) ) ;
#134554 = ORIENTED_EDGE ( 'NONE', *, *, #88654, .T. ) ;
#134555 = EDGE_CURVE ( 'NONE', #80319, #51865, #134712, .T. ) ;
#134556 = PLANE ( 'NONE',  #102122 ) ;
#134557 = VERTEX_POINT ( 'NONE', #12134 ) ;
#134558 = VECTOR ( 'NONE', #49097, 999.9999999999998863 ) ;
#134559 = CYLINDRICAL_SURFACE ( 'NONE', #26190, 7.950000000000000178 ) ;
#134560 = EDGE_CURVE ( 'NONE', #22767, #51759, #46979, .T. ) ;
#134561 = VECTOR ( 'NONE', #105360, 1000.000000000000227 ) ;
#134562 = DIRECTION ( 'NONE',  ( -1.000000000000000000, -1.224606353822377258E-16, -0.000000000000000000 ) ) ;
#134563 = DIRECTION ( 'NONE',  ( 0.3543493200069162685, -0.000000000000000000, -0.9351131265310288487 ) ) ;
#134564 = VERTEX_POINT ( 'NONE', #89705 ) ;
#134565 = CARTESIAN_POINT ( 'NONE',  ( -28.49999999999979750, -6.839392718269155402, -8.480912228396016772 ) ) ;
#134566 = DIRECTION ( 'NONE',  ( -0.7071067811865486830, -0.7071067811865464625, 0.000000000000000000 ) ) ;
#134567 = DIRECTION ( 'NONE',  ( 0.000000000000000000, 1.000000000000000000, 0.000000000000000000 ) ) ;
#134568 = AXIS2_PLACEMENT_3D ( 'NONE', #108485, #64318, #119379 ) ;
#134569 = PLANE ( 'NONE',  #41179 ) ;
#134570 = CARTESIAN_POINT ( 'NONE',  ( 27.20419371712955225, -6.884901960086285300, -3.975000000000000089 ) ) ;
#134571 = ADVANCED_FACE ( 'NONE', ( #3386 ), #47845, .T. ) ;
#134572 = VECTOR ( 'NONE', #4722, 1000.000000000000000 ) ;
#134573 = CARTESIAN_POINT ( 'NONE',  ( 131.5423521607622774, -49.05583548141699168, -39.86617647058817226 ) ) ;
#134574 = ORIENTED_EDGE ( 'NONE', *, *, #21206, .F. ) ;
#134575 = LINE ( 'NONE', #78048, #135238 ) ;
#134576 = CARTESIAN_POINT ( 'NONE',  ( -25.01459476339044130, 2.945717840782780428, 4.000000000000000000 ) ) ;
#134577 = ORIENTED_EDGE ( 'NONE', *, *, #4457, .T. ) ;
#134578 = VERTEX_POINT ( 'NONE', #23741 ) ;
#134579 = ORIENTED_EDGE ( 'NONE', *, *, #68273, .F. ) ;
#134580 = EDGE_CURVE ( 'NONE', #106170, #135404, #68009, .T. ) ;
#134581 = CARTESIAN_POINT ( 'NONE',  ( 56.72959685856476142, -6.110000000000000320, -1.637169565754161393 ) ) ;
#134582 = EDGE_CURVE ( 'NONE', #130556, #17773, #47679, .T. ) ;
#134583 = AXIS2_PLACEMENT_3D ( 'NONE', #104498, #137148, #137872 ) ;
#134584 = ORIENTED_EDGE ( 'NONE', *, *, #99160, .F. ) ;
#134585 = PLANE ( 'NONE',  #136999 ) ;
#134586 = EDGE_CURVE ( 'NONE', #140292, #94283, #90421, .T. ) ;
#134587 = CARTESIAN_POINT ( 'NONE',  ( 6.899972949537105826, 4.461849672132297329, -4.461849672132302658 ) ) ;
#134588 = CARTESIAN_POINT ( 'NONE',  ( 92.60459685856477563, 1.637169565754164946, -6.109999999999999432 ) ) ;
#134589 = LINE ( 'NONE', #12763, #54094 ) ;
#134590 = ORIENTED_EDGE ( 'NONE', *, *, #60958, .T. ) ;
#134591 = CARTESIAN_POINT ( 'NONE',  ( 33.18398860626899705, 28.73617430169810305, 5.000000000000000000 ) ) ;
#134592 = ORIENTED_EDGE ( 'NONE', *, *, #116602, .F. ) ;
#134593 = DIRECTION ( 'NONE',  ( 0.7071067811865487940, -0.7071067811865463515, 0.000000000000000000 ) ) ;
#134594 = CARTESIAN_POINT ( 'NONE',  ( 30.79289321881324781, 6.759292476615653023, 5.000000000000000000 ) ) ;
#134595 = ORIENTED_EDGE ( 'NONE', *, *, #18487, .T. ) ;
#134596 = CARTESIAN_POINT ( 'NONE',  ( -5.510786437626906675, -27.52281430457051314, 5.000000000000000000 ) ) ;
#134597 = CARTESIAN_POINT ( 'NONE',  ( 127.2245968585647660, -1.637169565754161171, 6.109999999999998543 ) ) ;
#134599 = ORIENTED_EDGE ( 'NONE', *, *, #74114, .F. ) ;
#134598 = CIRCLE ( 'NONE', #88339, 5.968999999999998529 ) ;
#134600 = DIRECTION ( 'NONE',  ( -0.6830127018922181881, 0.6830127018922202975, -0.2588190451025214056 ) ) ;
#134601 = ORIENTED_EDGE ( 'NONE', *, *, #89612, .F. ) ;
#134602 = EDGE_LOOP ( 'NONE', ( #85829, #47974, #28690, #137891 ) ) ;
#134603 = ORIENTED_EDGE ( 'NONE', *, *, #45738, .F. ) ;
#134604 = VECTOR ( 'NONE', #104450, 1000.000000000000000 ) ;
#134605 = VECTOR ( 'NONE', #58378, 1000.000000000000227 ) ;
#134606 = VECTOR ( 'NONE', #28895, 1000.000000000000000 ) ;
#134607 = VECTOR ( 'NONE', #112395, 1000.000000000000000 ) ;
#134608 = CIRCLE ( 'NONE', #129932, 2.500000000000000888 ) ;
#134609 = DIRECTION ( 'NONE',  ( 0.7071067811865486830, -0.7071067811865464625, -0.000000000000000000 ) ) ;
#134610 = PLANE ( 'NONE',  #75153 ) ;
#134611 = DIRECTION ( 'NONE',  ( 0.7071067811865487940, 0.7071067811865463515, 0.000000000000000000 ) ) ;
#134612 = DIRECTION ( 'NONE',  ( -0.3543493200069162685, -0.000000000000000000, -0.9351131265310288487 ) ) ;
#134614 = VERTEX_POINT ( 'NONE', #106092 ) ;
#134613 = VECTOR ( 'NONE', #85094, 1000.000000000000000 ) ;
#134615 = FACE_OUTER_BOUND ( 'NONE', #13395, .T. ) ;
#134616 = CARTESIAN_POINT ( 'NONE',  ( 21.85373647476855297, -5.808823158059035485, -5.808823158059033709 ) ) ;
#134617 = DIRECTION ( 'NONE',  ( -0.000000000000000000, 0.3543493200069153248, 0.9351131265310292928 ) ) ;
#134618 = CARTESIAN_POINT ( 'NONE',  ( 22.49999999999984368, -17.91344420646040447, 1.358650452708515921 ) ) ;
#134619 = AXIS2_PLACEMENT_3D ( 'NONE', #115583, #96697, #16285 ) ;
#134620 = CARTESIAN_POINT ( 'NONE',  ( -32.75085989791905661, 22.27000000000000313, -14.49214836789566263 ) ) ;
#134621 = VERTEX_POINT ( 'NONE', #18369 ) ;
#134622 = ORIENTED_EDGE ( 'NONE', *, *, #9053, .F. ) ;
#134623 = EDGE_CURVE ( 'NONE', #21154, #3387, #52443, .T. ) ;
#134624 = ORIENTED_EDGE ( 'NONE', *, *, #106568, .T. ) ;
#134625 =( NAMED_UNIT ( * ) PLANE_ANGLE_UNIT ( ) SI_UNIT ( $, .RADIAN. ) );
#134626 = CARTESIAN_POINT ( 'NONE',  ( -29.99999999999979039, -6.033600742197676503, 5.000000000000000000 ) ) ;
#134627 = UNCERTAINTY_MEASURE_WITH_UNIT (LENGTH_MEASURE( 1.000000000000000082E-05 ), #53307, 'distance_accuracy_value', 'NONE');
#134628 = PLANE ( 'NONE',  #979 ) ;
#134629 = FILL_AREA_STYLE ('',( #26561 ) ) ;
#134630 = CARTESIAN_POINT ( 'NONE',  ( 8.122631387037495543, 8.712540773999728927, 3.790917003805983843 ) ) ;
#134631 = VECTOR ( 'NONE', #110089, 1000.000000000000000 ) ;
#134632 = VECTOR ( 'NONE', #142015, 1000.000000000000000 ) ;
#134633 = CARTESIAN_POINT ( 'NONE',  ( -2.292893218813429890, 11.25929247661560417, 5.000000000000000000 ) ) ;
#134634 = DIRECTION ( 'NONE',  ( 0.7071067811865487940, 0.7071067811865463515, 0.000000000000000000 ) ) ;
#134635 = FACE_OUTER_BOUND ( 'NONE', #80664, .T. ) ;
#134636 = DIRECTION ( 'NONE',  ( -0.000000000000000000, 0.3543493200069153248, 0.9351131265310292928 ) ) ;
#134637 = VECTOR ( 'NONE', #94434, 1000.000000000000000 ) ;
#134638 = DIRECTION ( 'NONE',  ( 1.000000000000000000, 0.000000000000000000, 0.000000000000000000 ) ) ;
#134639 = ORIENTED_EDGE ( 'NONE', *, *, #8258, .F. ) ;
#134640 = VECTOR ( 'NONE', #56416, 1000.000000000000227 ) ;
#134641 = VERTEX_POINT ( 'NONE', #40199 ) ;
#134642 = FACE_OUTER_BOUND ( 'NONE', #59156, .T. ) ;
#134643 = ORIENTED_EDGE ( 'NONE', *, *, #74648, .T. ) ;
#134644 = EDGE_CURVE ( 'NONE', #6354, #55705, #108228, .T. ) ;
#134645 = AXIS2_PLACEMENT_3D ( 'NONE', #87897, #129983, #132141 ) ;
#134646 = CARTESIAN_POINT ( 'NONE',  ( 0.000000000000000000, 0.000000000000000000, 0.000000000000000000 ) ) ;
#134647 = CARTESIAN_POINT ( 'NONE',  ( -0.2997448713915885632, -27.71228299555206220, 4.000000000000000000 ) ) ;
#134648 = ORIENTED_EDGE ( 'NONE', *, *, #66746, .T. ) ;
#134649 = ADVANCED_FACE ( 'NONE', ( #95959 ), #130769, .T. ) ;
#134650 = SURFACE_STYLE_USAGE ( .BOTH. , #133914 ) ;
#134651 = ORIENTED_EDGE ( 'NONE', *, *, #65583, .T. ) ;
#134652 = CARTESIAN_POINT ( 'NONE',  ( -12.48921356237309155, -27.52281430457064104, 5.000000000000000000 ) ) ;
#134653 = ORIENTED_EDGE ( 'NONE', *, *, #119431, .T. ) ;
#134654 = EDGE_CURVE ( 'NONE', #113899, #82267, #6766, .T. ) ;
#134655 = CARTESIAN_POINT ( 'NONE',  ( 39.48921356237310221, -27.52281430457082934, 5.000000000000000000 ) ) ;
#134656 = CARTESIAN_POINT ( 'NONE',  ( 106.8291937171295700, -3.975000000000001865, 6.884901960086284411 ) ) ;
#134657 = DIRECTION ( 'NONE',  ( 0.000000000000000000, -1.000000000000000000, 0.000000000000000000 ) ) ;
#134658 = CARTESIAN_POINT ( 'NONE',  ( 32.99999999999976552, 20.58746187583904330, 4.000000000000000000 ) ) ;
#134659 = ORIENTED_EDGE ( 'NONE', *, *, #120413, .T. ) ;
#134660 = EDGE_CURVE ( 'NONE', #142281, #61677, #30736, .T. ) ;
#134661 = PLANE ( 'NONE',  #12094 ) ;
#134662 = CARTESIAN_POINT ( 'NONE',  ( -20.20666063542138957, 21.75929247661549226, 4.998822639870715179 ) ) ;
#134663 = CARTESIAN_POINT ( 'NONE',  ( 0.000000000000000000, 0.000000000000000000, 0.000000000000000000 ) ) ;
#134665 = VECTOR ( 'NONE', #133437, 1000.000000000000000 ) ;
#134664 = CARTESIAN_POINT ( 'NONE',  ( 12.54166666666666785, 3.047499999999993214, -5.278424836066146320 ) ) ;
#134666 = CARTESIAN_POINT ( 'NONE',  ( -69.29974487139159578, -27.71228299555254537, 4.000000000000000000 ) ) ;
#134668 = VECTOR ( 'NONE', #52932, 1000.000000000000000 ) ;
#134667 = FACE_OUTER_BOUND ( 'NONE', #125534, .T. ) ;
#134669 = CARTESIAN_POINT ( 'NONE',  ( -29.28242261357413057, -21.73023691814492864, 5.000000000000000888 ) ) ;
#134670 = VERTEX_POINT ( 'NONE', #19120 ) ;
#134671 = EDGE_CURVE ( 'NONE', #114653, #122222, #96501, .T. ) ;
#134672 = PLANE ( 'NONE',  #83704 ) ;
#134673 = ORIENTED_EDGE ( 'NONE', *, *, #102397, .F. ) ;
#134675 = VECTOR ( 'NONE', #35465, 1000.000000000000000 ) ;
#134674 = CARTESIAN_POINT ( 'NONE',  ( 96.97959685856478984, 6.109999999999999432, 1.637169565754164280 ) ) ;
#134676 = LINE ( 'NONE', #35372, #124103 ) ;
#134677 = FILL_AREA_STYLE ('',( #46245 ) ) ;
#134679 = AXIS2_PLACEMENT_3D ( 'NONE', #49752, #73621, #29381 ) ;
#134678 = CARTESIAN_POINT ( 'NONE',  ( 1.629999999999999893, -0.4000000000000004108, 2.303088455023526215 ) ) ;
#134680 = DIRECTION ( 'NONE',  ( -0.3543493200069163240, -0.000000000000000000, 0.9351131265310288487 ) ) ;
#134681 = ORIENTED_EDGE ( 'NONE', *, *, #48661, .T. ) ;
#134682 = EDGE_CURVE ( 'NONE', #124216, #72242, #56826, .T. ) ;
#134683 = DIRECTION ( 'NONE',  ( -0.000000000000000000, 0.000000000000000000, 1.000000000000000000 ) ) ;
#134684 = FACE_OUTER_BOUND ( 'NONE', #82690, .T. ) ;
#134685 = DIRECTION ( 'NONE',  ( -0.6830127018922180770, -0.6830127018922204085, -0.2588190451025213501 ) ) ;
#134686 = ORIENTED_EDGE ( 'NONE', *, *, #69438, .T. ) ;
#134687 = DIRECTION ( 'NONE',  ( 0.7071067811865486830, -0.7071067811865464625, -0.000000000000000000 ) ) ;
#134689 = VERTEX_POINT ( 'NONE', #127909 ) ;
#134688 = FACE_OUTER_BOUND ( 'NONE', #103189, .T. ) ;
#134690 = DIRECTION ( 'NONE',  ( 0.7071067811865487940, 0.7071067811865463515, 0.000000000000000000 ) ) ;
#134691 = ADVANCED_FACE ( 'NONE', ( #28589 ), #118418, .F. ) ;
#134692 = FACE_OUTER_BOUND ( 'NONE', #1766, .T. ) ;
#134693 = AXIS2_PLACEMENT_3D ( 'NONE', #126935, #50832, #139292 ) ;
#134694 = CARTESIAN_POINT ( 'NONE',  ( 2.510786437626908008, -27.52281430457053446, 5.000000000000000000 ) ) ;
#134695 = PLANE ( 'NONE',  #8521 ) ;
#134696 = DIRECTION ( 'NONE',  ( -0.7071067811865486830, 0.7071067811865464625, 0.000000000000000000 ) ) ;
#134697 = ORIENTED_EDGE ( 'NONE', *, *, #48328, .F. ) ;
#134698 = ORIENTED_EDGE ( 'NONE', *, *, #125199, .T. ) ;
#134699 = EDGE_LOOP ( 'NONE', ( #86383, #32668, #80161, #20717 ) ) ;
#134700 = CARTESIAN_POINT ( 'NONE',  ( 84.87543019189810423, -5.291415217122920289, -3.055000000000001492 ) ) ;
#134701 = ORIENTED_EDGE ( 'NONE', *, *, #72994, .F. ) ;
#134702 = CARTESIAN_POINT ( 'NONE',  ( -34.42500000000001137, -21.72500000000000142, 4.500000000000000888 ) ) ;
#134703 = EDGE_CURVE ( 'NONE', #43125, #32348, #116291, .T. ) ;
#134704 = DIRECTION ( 'NONE',  ( 0.3543493200069162685, -0.000000000000000000, -0.9351131265310288487 ) ) ;
#134705 = PLANE ( 'NONE',  #78134 ) ;
#134706 = DIRECTION ( 'NONE',  ( -0.7071067811865486830, 0.7071067811865464625, 0.000000000000000000 ) ) ;
#134707 = ORIENTED_EDGE ( 'NONE', *, *, #9409, .F. ) ;
#134708 = CIRCLE ( 'NONE', #72216, 2.500000000000000444 ) ;
#134709 = VECTOR ( 'NONE', #106550, 1000.000000000000000 ) ;
#134710 = LINE ( 'NONE', #15702, #28264 ) ;
#134712 =( BOUNDED_CURVE ( )  B_SPLINE_CURVE ( 3, ( #2680, #35363, #134669, #1934 ),
 .UNSPECIFIED., .F., .F. ) 
 B_SPLINE_CURVE_WITH_KNOTS ( ( 4, 4 ),
 ( 1.901594255663634492, 1.933014472006554740 ),
 .UNSPECIFIED. ) 
 CURVE ( )  GEOMETRIC_REPRESENTATION_ITEM ( )  RATIONAL_B_SPLINE_CURVE ( ( 1.000000000000000000, 0.9999177325257868620, 0.9999177325257868620, 1.000000000000000000 ) ) 
 REPRESENTATION_ITEM ( '' )  );
#134711 = FACE_OUTER_BOUND ( 'NONE', #77698, .T. ) ;
#134713 = EDGE_CURVE ( 'NONE', #107902, #45966, #105403, .T. ) ;
#134714 = ADVANCED_FACE ( 'NONE', ( #129292 ), #59517, .T. ) ;
#134716 = VECTOR ( 'NONE', #90123, 1000.000000000000000 ) ;
#134715 = CARTESIAN_POINT ( 'NONE',  ( -12.69999999999998153, 0.000000000000000000, 0.000000000000000000 ) ) ;
#134717 = CARTESIAN_POINT ( 'NONE',  ( 82.89126352523142316, -4.472830434245839371, -4.472830434245839371 ) ) ;
#134718 = ORIENTED_EDGE ( 'NONE', *, *, #11788, .T. ) ;
#134719 = CARTESIAN_POINT ( 'NONE',  ( 15.63964197871511885, 8.074661077379714058, 4.334728602384618767 ) ) ;
#134720 = AXIS2_PLACEMENT_3D ( 'NONE', #120123, #65094, #122278 ) ;
#134721 = VECTOR ( 'NONE', #120903, 999.9999999999998863 ) ;
#134722 = CARTESIAN_POINT ( 'NONE',  ( -12.69999999999998153, 0.000000000000000000, 0.000000000000000000 ) ) ;
#134723 = VECTOR ( 'NONE', #115684, 1000.000000000000000 ) ;
#134724 = VECTOR ( 'NONE', #112229, 1000.000000000000000 ) ;
#134725 = EDGE_CURVE ( 'NONE', #76657, #136607, #29984, .T. ) ;
#134726 = VECTOR ( 'NONE', #94225, 999.9999999999998863 ) ;
#134727 = ORIENTED_EDGE ( 'NONE', *, *, #55483, .F. ) ;
#134728 = ORIENTED_EDGE ( 'NONE', *, *, #60211, .T. ) ;
#134729 = DIRECTION ( 'NONE',  ( 0.3543493200069162685, -0.000000000000000000, -0.9351131265310288487 ) ) ;
#134730 = EDGE_CURVE ( 'NONE', #18576, #32728, #72847, .T. ) ;
#134731 = CARTESIAN_POINT ( 'NONE',  ( -7.786780966966368567, 12.75929247661558996, 10.29404684609033538 ) ) ;
#134732 = PLANE ( 'NONE',  #129917 ) ;
#134733 = PLANE ( 'NONE',  #122057 ) ;
#134734 = CARTESIAN_POINT ( 'NONE',  ( -23.67183060077630685, 17.25929247661554200, 4.000000000000000000 ) ) ;
#134735 = DIRECTION ( 'NONE',  ( -1.000000000000000000, -0.000000000000000000, -0.000000000000000000 ) ) ;
#134736 = ORIENTED_EDGE ( 'NONE', *, *, #143484, .T. ) ;
#134737 = EDGE_LOOP ( 'NONE', ( #71904, #82131, #104178, #65283 ) ) ;
#134738 = EDGE_CURVE ( 'NONE', #82163, #126053, #51048, .T. ) ;
#134739 = FACE_OUTER_BOUND ( 'NONE', #44353, .T. ) ;
#134740 = ORIENTED_EDGE ( 'NONE', *, *, #94940, .F. ) ;
#134741 = ORIENTED_EDGE ( 'NONE', *, *, #131495, .F. ) ;
#134742 = EDGE_CURVE ( 'NONE', #37853, #28081, #139515, .T. ) ;
#134743 = AXIS2_PLACEMENT_3D ( 'NONE', #48249, #59171, #122221 ) ;
#134744 = VECTOR ( 'NONE', #8930, 1000.000000000000000 ) ;
#134745 = DIRECTION ( 'NONE',  ( -0.000000000000000000, -1.000000000000000000, -0.000000000000000000 ) ) ;
#134746 = ORIENTED_EDGE ( 'NONE', *, *, #3836, .T. ) ;
#134747 = CARTESIAN_POINT ( 'NONE',  ( -5.816011393731002066, 28.73617430169783304, 5.000000000000000000 ) ) ;
#134748 = FACE_OUTER_BOUND ( 'NONE', #10206, .T. ) ;
#134749 = VECTOR ( 'NONE', #129570, 1000.000000000000000 ) ;
#134750 = LINE ( 'NONE', #81066, #119734 ) ;
#134751 = LINE ( 'NONE', #35444, #57730 ) ;
#134752 = VECTOR ( 'NONE', #113239, 999.9999999999998863 ) ;
#134753 = DIRECTION ( 'NONE',  ( -0.7071067811865486830, 0.7071067811865464625, 0.000000000000000000 ) ) ;
#134754 = ORIENTED_EDGE ( 'NONE', *, *, #53359, .F. ) ;
#134755 = CARTESIAN_POINT ( 'NONE',  ( -34.76445279868696758, 22.22500000000000142, 5.060837336147055332 ) ) ;
#134756 = ORIENTED_EDGE ( 'NONE', *, *, #16138, .F. ) ;
#134757 = LINE ( 'NONE', #78215, #78223 ) ;
#134758 = ORIENTED_EDGE ( 'NONE', *, *, #125024, .T. ) ;
#134759 = CARTESIAN_POINT ( 'NONE',  ( -63.18398860626900415, 28.73617430169831621, 5.000000000000000000 ) ) ;
#134760 = ORIENTED_EDGE ( 'NONE', *, *, #37958, .F. ) ;
#134761 = PLANE ( 'NONE',  #115307 ) ;
#134762 = ORIENTED_EDGE ( 'NONE', *, *, #68214, .F. ) ;
#134763 = EDGE_LOOP ( 'NONE', ( #64908, #53614, #132224, #14671 ) ) ;
#134764 = AXIS2_PLACEMENT_3D ( 'NONE', #27740, #93722, #71999 ) ;
#134765 = ORIENTED_EDGE ( 'NONE', *, *, #108715, .F. ) ;
#134766 = ADVANCED_FACE ( 'NONE', ( #128602 ), #29276, .F. ) ;
#134767 = CARTESIAN_POINT ( 'NONE',  ( 23.96628934044694148, -0.2106608083017111055, 4.443784815937100063 ) ) ;
#134768 = DIRECTION ( 'NONE',  ( -1.000000000000000000, -1.224606353822377258E-16, -0.000000000000000000 ) ) ;
#134769 = DIRECTION ( 'NONE',  ( -0.000000000000000000, 1.000000000000000000, 0.000000000000000000 ) ) ;
#134770 = CARTESIAN_POINT ( 'NONE',  ( 120.6045968585647756, 1.637169565754164946, -6.109999999999999432 ) ) ;
#134771 = CARTESIAN_POINT ( 'NONE',  ( -28.49999999999979750, -9.462702396501040170, -9.474982329943451020 ) ) ;
#134772 = LINE ( 'NONE', #36842, #18080 ) ;
#134775 = DIRECTION ( 'NONE',  ( -1.000000000000000000, -1.224606353822377258E-16, -0.000000000000000000 ) ) ;
#134774 = PLANE ( 'NONE',  #18067 ) ;
#134773 = AXIS2_PLACEMENT_3D ( 'NONE', #83333, #6412, #117347 ) ;
#134776 = VECTOR ( 'NONE', #55661, 999.9999999999998863 ) ;
#134777 = DIRECTION ( 'NONE',  ( -0.6830127018922181881, 0.6830127018922202975, -0.2588190451025214056 ) ) ;
#134778 = SURFACE_STYLE_FILL_AREA ( #131896 ) ;
#134779 = ORIENTED_EDGE ( 'NONE', *, *, #28726, .F. ) ;
#134780 = FILL_AREA_STYLE ('',( #46350 ) ) ;
#134781 = CARTESIAN_POINT ( 'NONE',  ( 34.42499999999998295, 1.541399257802028577, 5.000000000000000000 ) ) ;
#134782 = LINE ( 'NONE', #134045, #26331 ) ;
#134783 = ORIENTED_EDGE ( 'NONE', *, *, #103664, .T. ) ;
#134784 = EDGE_LOOP ( 'NONE', ( #71091, #8536, #75228, #18562 ) ) ;
#134785 = VECTOR ( 'NONE', #28347, 1000.000000000000000 ) ;
#134786 = DIRECTION ( 'NONE',  ( 0.7071067811865486830, -0.7071067811865464625, -0.000000000000000000 ) ) ;
#134787 = VERTEX_POINT ( 'NONE', #41577 ) ;
#134788 = CARTESIAN_POINT ( 'NONE',  ( -12.69999999999998153, 0.000000000000000000, 0.000000000000000000 ) ) ;
#134789 = CARTESIAN_POINT ( 'NONE',  ( -26.29289321881327268, -0.7407075233842718154, 5.000000000000000000 ) ) ;
#134790 = LINE ( 'NONE', #136178, #39394 ) ;
#134791 = PLANE ( 'NONE',  #62575 ) ;
#134792 = ORIENTED_EDGE ( 'NONE', *, *, #41483, .T. ) ;
#134793 = CARTESIAN_POINT ( 'NONE',  ( -21.29974487139158512, -27.71228299555221142, 4.000000000000000000 ) ) ;
#134794 = VECTOR ( 'NONE', #105556, 1000.000000000000000 ) ;
#134795 = ORIENTED_EDGE ( 'NONE', *, *, #57818, .F. ) ;
#134796 = DIRECTION ( 'NONE',  ( 0.7071067811865486830, -0.7071067811865464625, -0.000000000000000000 ) ) ;
#134797 = CARTESIAN_POINT ( 'NONE',  ( 30.83790314143522338, -6.871911579029513106, -3.967499999999993587 ) ) ;
#134798 = ORIENTED_EDGE ( 'NONE', *, *, #23055, .T. ) ;
#134799 = CARTESIAN_POINT ( 'NONE',  ( 84.64126352523145158, 4.472830434245837594, 4.472830434245841147 ) ) ;
#134800 = CARTESIAN_POINT ( 'NONE',  ( 8.902796541008825670, -8.547859821797413105, 4.147131456889309398 ) ) ;
#134801 = ORIENTED_EDGE ( 'NONE', *, *, #75860, .T. ) ;
#134802 = ORIENTED_EDGE ( 'NONE', *, *, #102956, .T. ) ;
#134803 = ORIENTED_EDGE ( 'NONE', *, *, #29114, .F. ) ;
#134804 = LINE ( 'NONE', #71666, #68155 ) ;
#134805 = CARTESIAN_POINT ( 'NONE',  ( 66.18398860626901126, 28.73617430169833753, 5.000000000000000000 ) ) ;
#134806 = VECTOR ( 'NONE', #19776, 1000.000000000000000 ) ;
#134808 = CARTESIAN_POINT ( 'NONE',  ( -11.51078643762690490, -27.52281430457047406, 5.000000000000000000 ) ) ;
#134807 = VECTOR ( 'NONE', #19230, 1000.000000000000000 ) ;
#134809 = VECTOR ( 'NONE', #18773, 999.9999999999998863 ) ;
#134810 = PLANE ( 'NONE',  #119067 ) ;
#134811 = ORIENTED_EDGE ( 'NONE', *, *, #138983, .F. ) ;
#134812 = CARTESIAN_POINT ( 'NONE',  ( -7.171830600776418763, -5.240707523384232402, 4.000000000000000000 ) ) ;
#134813 = PRESENTATION_LAYER_ASSIGNMENT (  '', '', ( #113985 ) ) ;
#134814 = DIRECTION ( 'NONE',  ( -1.000000000000000000, 1.451651444332056451E-15, 0.000000000000000000 ) ) ;
#134815 = CARTESIAN_POINT ( 'NONE',  ( 8.700255128608413102, -27.71228299555199825, 4.000000000000000000 ) ) ;
#134816 = ORIENTED_EDGE ( 'NONE', *, *, #69180, .T. ) ;
#134817 = VECTOR ( 'NONE', #129469, 999.9999999999998863 ) ;
#134818 = AXIS2_PLACEMENT_3D ( 'NONE', #28566, #31413, #29252 ) ;
#134819 = STYLED_ITEM ( 'NONE', ( #96315 ), #11968 ) ;
#134820 = FACE_OUTER_BOUND ( 'NONE', #41135, .T. ) ;
#134821 = ORIENTED_EDGE ( 'NONE', *, *, #4762, .F. ) ;
#134822 = EDGE_CURVE ( 'NONE', #20530, #131775, #130030, .T. ) ;
#134824 = ORIENTED_EDGE ( 'NONE', *, *, #44231, .T. ) ;
#134823 = CARTESIAN_POINT ( 'NONE',  ( 58.77385498567181799, -47.18881911353551573, -35.55177538329067488 ) ) ;
#134825 = VERTEX_POINT ( 'NONE', #131464 ) ;
#134826 = EDGE_CURVE ( 'NONE', #3994, #73071, #5926, .T. ) ;
#134827 = EDGE_CURVE ( 'NONE', #142647, #4395, #107657, .T. ) ;
#134828 = CARTESIAN_POINT ( 'NONE',  ( 8.031592354503320763, 9.902892378096218942E-16, 0.000000000000000000 ) ) ;
#134829 = CARTESIAN_POINT ( 'NONE',  ( 34.47516574401890921, -20.97193265888397207, 4.998110765256833510 ) ) ;
#134830 = ORIENTED_EDGE ( 'NONE', *, *, #56951, .F. ) ;
#134831 = UNCERTAINTY_MEASURE_WITH_UNIT (LENGTH_MEASURE( 1.000000000000000082E-05 ), #21217, 'distance_accuracy_value', 'NONE');
#134832 = VERTEX_POINT ( 'NONE', #45898 ) ;
#134833 = EDGE_CURVE ( 'NONE', #17542, #74043, #23392, .T. ) ;
#134834 = EDGE_CURVE ( 'NONE', #20599, #70176, #80917, .T. ) ;
#134835 = DIRECTION ( 'NONE',  ( 1.000000000000000000, 0.000000000000000000, 0.000000000000000000 ) ) ;
#134836 = DIRECTION ( 'NONE',  ( 0.7071067811865487940, -0.7071067811865463515, 0.000000000000000000 ) ) ;
#134837 = DIRECTION ( 'NONE',  ( -0.6830127018922181881, 0.6830127018922202975, -0.2588190451025214056 ) ) ;
#134838 = CARTESIAN_POINT ( 'NONE',  ( -34.92500000000001137, 11.57121408575941324, 9.037117742336748805 ) ) ;
#134839 = DIRECTION ( 'NONE',  ( 0.7071067811865487940, 0.7071067811865463515, 0.000000000000000000 ) ) ;
#134840 = EDGE_CURVE ( 'NONE', #103327, #68975, #33599, .T. ) ;
#134841 = DIRECTION ( 'NONE',  ( 1.000000000000000000, 1.224606353822377258E-16, 0.000000000000000000 ) ) ;
#134842 = DIRECTION ( 'NONE',  ( 0.6830127018922181881, 0.6830127018922202975, -0.2588190451025214056 ) ) ;
#134843 = LINE ( 'NONE', #114465, #64583 ) ;
#134844 = CARTESIAN_POINT ( 'NONE',  ( 16.89540314143521726, 2.126176841940962348, 7.934999999999989839 ) ) ;
#134845 = FACE_OUTER_BOUND ( 'NONE', #137692, .T. ) ;
#134846 = DIRECTION ( 'NONE',  ( 0.000000000000000000, 0.000000000000000000, 1.000000000000000000 ) ) ;
#134847 = LINE ( 'NONE', #79773, #28136 ) ;
#134848 = DIRECTION ( 'NONE',  ( 0.7071067811865486830, -0.7071067811865464625, -0.000000000000000000 ) ) ;
#134849 = ORIENTED_EDGE ( 'NONE', *, *, #137173, .F. ) ;
#134850 = VECTOR ( 'NONE', #29338, 1000.000000000000000 ) ;
#134851 = ORIENTED_EDGE ( 'NONE', *, *, #134154, .F. ) ;
#134853 = EDGE_CURVE ( 'NONE', #118081, #48278, #142349, .T. ) ;
#134852 = CARTESIAN_POINT ( 'NONE',  ( 93.75000000000000000, -9.735942053221458872E-16, 7.950000000000000178 ) ) ;
#134854 = ORIENTED_EDGE ( 'NONE', *, *, #107947, .T. ) ;
#134855 = ORIENTED_EDGE ( 'NONE', *, *, #52456, .T. ) ;
#134856 = CIRCLE ( 'NONE', #95476, 2.500000000000000444 ) ;
#134857 = ORIENTED_EDGE ( 'NONE', *, *, #101637, .F. ) ;
#134858 = LINE ( 'NONE', #101468, #55002 ) ;
#134859 = LINE ( 'NONE', #89875, #74180 ) ;
#134860 = CONICAL_SURFACE ( 'NONE', #19124, 2.055000000000001048, 0.9599310885968758145 ) ;
#134861 = CARTESIAN_POINT ( 'NONE',  ( 13.21932050955820692, 8.913545539526866790, -3.292927883844741110 ) ) ;
#134862 = VERTEX_POINT ( 'NONE', #66918 ) ;
#134863 = CARTESIAN_POINT ( 'NONE',  ( -36.18398860626899705, 28.73617430169812437, 5.000000000000000000 ) ) ;
#134864 = CARTESIAN_POINT ( 'NONE',  ( -6.793339364578430128, 21.75929247661548871, 4.998822639870703632 ) ) ;
#134865 = DIRECTION ( 'NONE',  ( -0.7071067811865486830, -0.7071067811865464625, -0.000000000000000000 ) ) ;
#134866 = DIRECTION ( 'NONE',  ( 0.6830127018922180770, -0.6830127018922204085, -0.2588190451025213501 ) ) ;
#134867 = CARTESIAN_POINT ( 'NONE',  ( 28.19018167574430933, -18.74070752338409207, 7.910009926591441420 ) ) ;
#134868 = CARTESIAN_POINT ( 'NONE',  ( 7.499999999999954703, 1.466399257802248446, 5.000000000000000000 ) ) ;
#134869 = DIRECTION ( 'NONE',  ( -0.7071067811865486830, -0.7071067811865464625, -0.000000000000000000 ) ) ;
#134870 = EDGE_CURVE ( 'NONE', #138219, #5611, #916, .T. ) ;
#134872 = AXIS2_PLACEMENT_3D ( 'NONE', #18255, #117572, #75543 ) ;
#134871 = CARTESIAN_POINT ( 'NONE',  ( 38.99451991528749062, 28.92564299267965211, 4.000000000000000000 ) ) ;
#134873 = CARTESIAN_POINT ( 'NONE',  ( 31.49999999999977973, -2.173586137069110968, -4.605770156576038055 ) ) ;
#134874 = LINE ( 'NONE', #12333, #84745 ) ;
#134875 = CARTESIAN_POINT ( 'NONE',  ( 152.4000000000000057, 26.55578643762684266, 34.51078643762689069 ) ) ;
#134876 = DIRECTION ( 'NONE',  ( 0.7071067811865487940, 0.7071067811865463515, -0.000000000000000000 ) ) ;
#134877 = ORIENTED_EDGE ( 'NONE', *, *, #40129, .F. ) ;
#134878 = ORIENTED_EDGE ( 'NONE', *, *, #5281, .F. ) ;
#134879 = CARTESIAN_POINT ( 'NONE',  ( 113.6045968585647614, 1.637169565754164946, -6.109999999999999432 ) ) ;
#134880 =( BOUNDED_CURVE ( )  B_SPLINE_CURVE ( 3, ( #142580, #44735, #65766, #43272 ),
 .UNSPECIFIED., .F., .T. ) 
 B_SPLINE_CURVE_WITH_KNOTS ( ( 4, 4 ),
 ( 5.772031613926481342, 5.830584196225661486 ),
 .UNSPECIFIED. ) 
 CURVE ( )  GEOMETRIC_REPRESENTATION_ITEM ( )  RATIONAL_B_SPLINE_CURVE ( ( 1.000000000000000000, 0.9997143199977724937, 0.9997143199977724937, 1.000000000000000000 ) ) 
 REPRESENTATION_ITEM ( '' )  );
#134881 = ORIENTED_EDGE ( 'NONE', *, *, #89796, .T. ) ;
#134882 = VECTOR ( 'NONE', #20556, 1000.000000000000000 ) ;
#134883 = ADVANCED_FACE ( 'NONE', ( #111098 ), #98808, .T. ) ;
#134884 = CARTESIAN_POINT ( 'NONE',  ( 99.29166666666667140, 3.975000000000003642, -6.884901960086285300 ) ) ;
#134885 = CIRCLE ( 'NONE', #33066, 2.500000000000000888 ) ;
#134886 = FACE_OUTER_BOUND ( 'NONE', #11492, .T. ) ;
#134887 = DIRECTION ( 'NONE',  ( 8.673617379884034239E-17, -1.000000000000000000, 0.000000000000000000 ) ) ;
#134888 = ADVANCED_FACE ( 'NONE', ( #11790 ), #11064, .T. ) ;
#134889 = CARTESIAN_POINT ( 'NONE',  ( 109.4329301918981088, 1.637169565754156508, 6.110000000000000320 ) ) ;
#134890 = ORIENTED_EDGE ( 'NONE', *, *, #62605, .F. ) ;
#134891 = ADVANCED_FACE ( 'NONE', ( #66215 ), #55335, .F. ) ;
#134892 = ORIENTED_EDGE ( 'NONE', *, *, #863, .T. ) ;
#134893 = DIRECTION ( 'NONE',  ( 1.000000000000000000, 0.000000000000000000, 0.000000000000000000 ) ) ;
#134894 = CIRCLE ( 'NONE', #86227, 9.119999999999999218 ) ;
#134895 = CARTESIAN_POINT ( 'NONE',  ( 97.39583333333332860, -2.130196079827427091, 7.949999999999998401 ) ) ;
#134896 = EDGE_CURVE ( 'NONE', #5082, #138480, #102427, .T. ) ;
#134897 = ORIENTED_EDGE ( 'NONE', *, *, #76555, .T. ) ;
#134898 = ORIENTED_EDGE ( 'NONE', *, *, #7395, .F. ) ;
#134899 = ORIENTED_EDGE ( 'NONE', *, *, #78045, .F. ) ;
#134900 = LINE ( 'NONE', #34860, #139473 ) ;
#134901 = AXIS2_PLACEMENT_3D ( 'NONE', #8033, #129840, #30542 ) ;
#134903 = EDGE_CURVE ( 'NONE', #7972, #29609, #60349, .T. ) ;
#134902 =( BOUNDED_CURVE ( )  B_SPLINE_CURVE ( 3, ( #60493, #104670, #114806, #39445 ),
 .UNSPECIFIED., .F., .F. ) 
 B_SPLINE_CURVE_WITH_KNOTS ( ( 4, 4 ),
 ( 5.920967161967927161, 7.341195215986655143 ),
 .UNSPECIFIED. ) 
 CURVE ( )  GEOMETRIC_REPRESENTATION_ITEM ( )  RATIONAL_B_SPLINE_CURVE ( ( 1.000000000000000000, 0.8388583629366577199, 0.8388583629366577199, 1.000000000000000000 ) ) 
 REPRESENTATION_ITEM ( '' )  );
#134904 = CARTESIAN_POINT ( 'NONE',  ( 29.66209685856477307, -5.291415217122919401, 3.054999999999997939 ) ) ;
#134905 = VERTEX_POINT ( 'NONE', #124860 ) ;
#134906 = ORIENTED_EDGE ( 'NONE', *, *, #98621, .T. ) ;
#134907 = ADVANCED_FACE ( 'NONE', ( #26276 ), #4433, .F. ) ;
#134908 = CARTESIAN_POINT ( 'NONE',  ( 0.000000000000000000, 0.000000000000000000, 5.000000000000000000 ) ) ;
#134909 = ORIENTED_EDGE ( 'NONE', *, *, #61510, .T. ) ;
#134910 = VERTEX_POINT ( 'NONE', #58960 ) ;
#134911 = VECTOR ( 'NONE', #139979, 1000.000000000000114 ) ;
#134912 = VERTEX_POINT ( 'NONE', #5195 ) ;
#134913 = AXIS2_PLACEMENT_3D ( 'NONE', #88722, #130806, #65563 ) ;
#134914 = AXIS2_PLACEMENT_3D ( 'NONE', #130863, #29363, #73606 ) ;
#134915 = CARTESIAN_POINT ( 'NONE',  ( 12.32816939922344623, -15.74070752338411694, 4.000000000000000000 ) ) ;
#134916 = VECTOR ( 'NONE', #130460, 1000.000000000000000 ) ;
#134917 = PLANE ( 'NONE',  #72995 ) ;
#134918 = DIRECTION ( 'NONE',  ( -1.000000000000000000, -1.224606353822377258E-16, -0.000000000000000000 ) ) ;
#134919 = EDGE_CURVE ( 'NONE', #97217, #104460, #15953, .T. ) ;
#134920 = ORIENTED_EDGE ( 'NONE', *, *, #118263, .F. ) ;
#134921 = DIRECTION ( 'NONE',  ( 0.7071067811865486830, -0.7071067811865464625, -0.000000000000000000 ) ) ;
#134922 = AXIS2_PLACEMENT_3D ( 'NONE', #109696, #11060, #9646 ) ;
#134923 = CONICAL_SURFACE ( 'NONE', #107139, 2.055000000000000604, 0.9599310885968764806 ) ;
#134924 = DIRECTION ( 'NONE',  ( 1.000000000000000000, 0.000000000000000000, 0.000000000000000000 ) ) ;
#134925 = CARTESIAN_POINT ( 'NONE',  ( 0.000000000000000000, 0.000000000000000000, 4.999999999999998224 ) ) ;
#134926 = FACE_BOUND ( 'NONE', #54069, .T. ) ;
#134927 = ORIENTED_EDGE ( 'NONE', *, *, #106994, .F. ) ;
#134928 = CARTESIAN_POINT ( 'NONE',  ( -1.499999999999994449, 16.18958161055402911, -11.56426086740811776 ) ) ;
#134929 = LINE ( 'NONE', #2189, #83166 ) ;
#134930 = PLANE ( 'NONE',  #95448 ) ;
#134931 = EDGE_CURVE ( 'NONE', #8819, #5949, #70538, .T. ) ;
#134932 = VERTEX_POINT ( 'NONE', #93675 ) ;
#134933 = CARTESIAN_POINT ( 'NONE',  ( 27.18398860626900060, 28.73617430169806042, 5.000000000000000000 ) ) ;
#134934 = ORIENTED_EDGE ( 'NONE', *, *, #40098, .F. ) ;
#134935 = ORIENTED_EDGE ( 'NONE', *, *, #80351, .T. ) ;
#134936 = EDGE_LOOP ( 'NONE', ( #45017, #33917, #135816, #118775 ) ) ;
#134937 = EDGE_CURVE ( 'NONE', #109252, #133102, #123472, .T. ) ;
#134938 = CARTESIAN_POINT ( 'NONE',  ( 34.47459685856478728, 1.637169565754164280, -6.109999999999996767 ) ) ;
#134939 = VERTEX_POINT ( 'NONE', #35757 ) ;
#134940 = VECTOR ( 'NONE', #31563, 1000.000000000000000 ) ;
#134941 = DIRECTION ( 'NONE',  ( 0.7071067811865487940, 0.7071067811865463515, -0.000000000000000000 ) ) ;
#134942 = EDGE_CURVE ( 'NONE', #71967, #12285, #136440, .T. ) ;
#134943 = DIRECTION ( 'NONE',  ( 1.000000000000000000, 0.000000000000000000, 0.000000000000000000 ) ) ;
#134944 = ORIENTED_EDGE ( 'NONE', *, *, #5213, .F. ) ;
#134945 = CARTESIAN_POINT ( 'NONE',  ( 16.78501580275800720, -3.740707523384238176, 15.76143240460127792 ) ) ;
#134946 = VECTOR ( 'NONE', #61659, 1000.000000000000000 ) ;
#134947 = ADVANCED_FACE ( 'NONE', ( #112559 ), #25539, .F. ) ;
#134948 = CARTESIAN_POINT ( 'NONE',  ( -21.48921356237309155, -27.52281430457070499, 5.000000000000000000 ) ) ;
#134949 = SURFACE_SIDE_STYLE ('',( #13110 ) ) ;
#134950 = VECTOR ( 'NONE', #139452, 1000.000000000000000 ) ;
#134951 = DIRECTION ( 'NONE',  ( 1.000000000000000000, -0.000000000000000000, 0.000000000000000000 ) ) ;
#134952 = VERTEX_POINT ( 'NONE', #57491 ) ;
#134953 = EDGE_LOOP ( 'NONE', ( #109647, #6197, #74826, #4570 ) ) ;
#134954 = ORIENTED_EDGE ( 'NONE', *, *, #14273, .T. ) ;
#134955 = CIRCLE ( 'NONE', #70090, 2.055000000000001048 ) ;
#134956 = ORIENTED_EDGE ( 'NONE', *, *, #53889, .F. ) ;
#134957 = CARTESIAN_POINT ( 'NONE',  ( 8.111591955682463606, -2.055000000000000160, 0.000000000000000000 ) ) ;
#134958 = ORIENTED_EDGE ( 'NONE', *, *, #138484, .F. ) ;
#134959 = ORIENTED_EDGE ( 'NONE', *, *, #67462, .F. ) ;
#134960 = LINE ( 'NONE', #35651, #76797 ) ;
#134961 = ADVANCED_FACE ( 'NONE', ( #35027 ), #69812, .F. ) ;
#134962 = CARTESIAN_POINT ( 'NONE',  ( -34.49999999999975131, -16.91253812416058366, 4.000000000000000000 ) ) ;
#134963 = ORIENTED_EDGE ( 'NONE', *, *, #132200, .T. ) ;
#134964 = CARTESIAN_POINT ( 'NONE',  ( 8.292893218813404133, -18.74070752338409562, 5.000000000000000000 ) ) ;
#134965 = DIRECTION ( 'NONE',  ( 0.000000000000000000, -1.000000000000000000, 0.000000000000000000 ) ) ;
#134966 = CARTESIAN_POINT ( 'NONE',  ( 27.19206980810188767, -7.934999999999991616, -2.126176841940955242 ) ) ;
#134967 = CARTESIAN_POINT ( 'NONE',  ( 2.816011393730999401, 28.73617430169785436, 5.000000000000000000 ) ) ;
#134968 = VERTEX_POINT ( 'NONE', #81394 ) ;
#134970 = CARTESIAN_POINT ( 'NONE',  ( -9.792893218813384593, -14.24070752338413470, 5.000000000000000000 ) ) ;
#134969 = CARTESIAN_POINT ( 'NONE',  ( 110.5995968585647802, -6.109999999999998543, -1.637169565754160727 ) ) ;
#134971 = CARTESIAN_POINT ( 'NONE',  ( 34.49999999999975842, 16.08746187583908949, 4.000000000000000000 ) ) ;
#134972 = CARTESIAN_POINT ( 'NONE',  ( -34.47516574401892342, -7.509482387884301779, 4.998110765256835286 ) ) ;
#134973 = CIRCLE ( 'NONE', #23810, 5.968999999999998529 ) ;
#134974 = ORIENTED_EDGE ( 'NONE', *, *, #16201, .T. ) ;
#134975 = LINE ( 'NONE', #11697, #56536 ) ;
#134977 = ORIENTED_EDGE ( 'NONE', *, *, #92794, .F. ) ;
#134976 = CARTESIAN_POINT ( 'NONE',  ( 20.97999999999999687, 2.055000000000001492, 0.000000000000000000 ) ) ;
#134979 = VECTOR ( 'NONE', #112714, 1000.000000000000000 ) ;
#134978 = LINE ( 'NONE', #33523, #57837 ) ;
#134980 = ORIENTED_EDGE ( 'NONE', *, *, #30240, .T. ) ;
#134981 =( NAMED_UNIT ( * ) SI_UNIT ( $, .STERADIAN. ) SOLID_ANGLE_UNIT ( ) );
#134982 = CARTESIAN_POINT ( 'NONE',  ( 11.99999999999992362, 17.58746187583906107, 4.000000000000000000 ) ) ;
#134983 = CARTESIAN_POINT ( 'NONE',  ( 6.850051285410198254, -8.240707523384193323, 17.25253755692240532 ) ) ;
#134984 = CYLINDRICAL_SURFACE ( 'NONE', #135158, 2.500000000000000444 ) ;
#134985 = VERTEX_POINT ( 'NONE', #103794 ) ;
#134986 = DIRECTION ( 'NONE',  ( -0.000000000000000000, 0.000000000000000000, 1.000000000000000000 ) ) ;
#134987 = DIRECTION ( 'NONE',  ( -0.7071067811865486830, 0.7071067811865464625, 0.000000000000000000 ) ) ;
#134988 = DIRECTION ( 'NONE',  ( -1.000000000000000000, 0.000000000000000000, 0.000000000000000000 ) ) ;
#134989 = ORIENTED_EDGE ( 'NONE', *, *, #99707, .F. ) ;
#134990 = VECTOR ( 'NONE', #78009, 1000.000000000000000 ) ;
#134991 = CARTESIAN_POINT ( 'NONE',  ( 22.49999999999984368, -1.695981523266237634, 4.571483868317931964 ) ) ;
#134992 = ORIENTED_EDGE ( 'NONE', *, *, #47976, .T. ) ;
#134993 = CARTESIAN_POINT ( 'NONE',  ( -39.18398860626899705, 28.73617430169814568, 5.000000000000000000 ) ) ;
#134995 = EDGE_LOOP ( 'NONE', ( #10239, #27322, #51341, #10634 ) ) ;
#134994 = FACE_OUTER_BOUND ( 'NONE', #48096, .T. ) ;
#134996 = EDGE_CURVE ( 'NONE', #14052, #98566, #135065, .T. ) ;
#134997 = ORIENTED_EDGE ( 'NONE', *, *, #2826, .T. ) ;
#134998 = VECTOR ( 'NONE', #1267, 1000.000000000000000 ) ;
#134999 = DIRECTION ( 'NONE',  ( -0.7071067811865486830, -0.7071067811865464625, 0.000000000000000000 ) ) ;
#135000 = CARTESIAN_POINT ( 'NONE',  ( -7.499999999999951150, -12.66682484999667224, -0.6294897503864105293 ) ) ;
#135001 = VERTEX_POINT ( 'NONE', #113990 ) ;
#135002 = EDGE_CURVE ( 'NONE', #24379, #54976, #124147, .T. ) ;
#135003 = EDGE_CURVE ( 'NONE', #18734, #23623, #125601, .T. ) ;
#135004 = DIRECTION ( 'NONE',  ( -1.000000000000000000, -1.224606353822377258E-16, -0.000000000000000000 ) ) ;
#135005 = EDGE_CURVE ( 'NONE', #102417, #35044, #47366, .T. ) ;
#135006 = EDGE_LOOP ( 'NONE', ( #68352, #58946, #55095, #94876 ) ) ;
#135007 = LINE ( 'NONE', #24775, #72063 ) ;
#135008 = EDGE_CURVE ( 'NONE', #36381, #66501, #46647, .T. ) ;
#135009 = LINE ( 'NONE', #122657, #76824 ) ;
#135010 = DIRECTION ( 'NONE',  ( 0.7071067811865487940, 0.7071067811865463515, 0.000000000000000000 ) ) ;
#135011 = VECTOR ( 'NONE', #37634, 1000.000000000000000 ) ;
#135012 = LINE ( 'NONE', #91487, #58648 ) ;
#135013 = DIRECTION ( 'NONE',  ( -0.000000000000000000, 0.000000000000000000, 1.000000000000000000 ) ) ;
#135014 = EDGE_CURVE ( 'NONE', #80414, #136986, #113253, .T. ) ;
#135015 = DIRECTION ( 'NONE',  ( 0.000000000000000000, 0.000000000000000000, 1.000000000000000000 ) ) ;
#135017 = ORIENTED_EDGE ( 'NONE', *, *, #72818, .F. ) ;
#135016 = VECTOR ( 'NONE', #19046, 1000.000000000000000 ) ;
#135018 = AXIS2_PLACEMENT_3D ( 'NONE', #125656, #94422, #137957 ) ;
#135019 = ORIENTED_EDGE ( 'NONE', *, *, #74489, .F. ) ;
#135020 = ORIENTED_EDGE ( 'NONE', *, *, #82655, .F. ) ;
#135022 = EDGE_CURVE ( 'NONE', #2765, #114790, #80665, .T. ) ;
#135021 = CARTESIAN_POINT ( 'NONE',  ( 115.6250000000000000, -7.950000000000000178, -4.867971026610729436E-16 ) ) ;
#135023 = ORIENTED_EDGE ( 'NONE', *, *, #105365, .F. ) ;
#135024 = ORIENTED_EDGE ( 'NONE', *, *, #4528, .T. ) ;
#135025 = ORIENTED_EDGE ( 'NONE', *, *, #69185, .F. ) ;
#135026 = VECTOR ( 'NONE', #50252, 1000.000000000000000 ) ;
#135027 = VECTOR ( 'NONE', #117855, 1000.000000000000000 ) ;
#135028 = CARTESIAN_POINT ( 'NONE',  ( 1.195149646228581108, -4.118442677489636772, -5.569367250693685101 ) ) ;
#135029 = AXIS2_PLACEMENT_3D ( 'NONE', #133819, #35958, #24334 ) ;
#135030 = CARTESIAN_POINT ( 'NONE',  ( 17.39159235450332019, 9.902892378096218942E-16, 0.000000000000000000 ) ) ;
#135031 = VERTEX_POINT ( 'NONE', #41414 ) ;
#135032 = DIRECTION ( 'NONE',  ( 0.7071067811865486830, -0.7071067811865464625, -0.000000000000000000 ) ) ;
#135033 = CARTESIAN_POINT ( 'NONE',  ( 25.39999999999998082, 6.833818690505176541, 2.948798542676217327 ) ) ;
#135034 = EDGE_CURVE ( 'NONE', #28318, #8822, #85620, .T. ) ;
#135035 = CARTESIAN_POINT ( 'NONE',  ( -19.49999999999986500, 12.05218569542904383, 5.000000000000000000 ) ) ;
#135036 = DIRECTION ( 'NONE',  ( -0.7071067811865487940, 0.7071067811865463515, 0.000000000000000000 ) ) ;
#135037 = CARTESIAN_POINT ( 'NONE',  ( 123.9587635252314470, 0.000000000000000000, -6.110000000000001208 ) ) ;
#135038 = ORIENTED_EDGE ( 'NONE', *, *, #39142, .T. ) ;
#135039 = FACE_OUTER_BOUND ( 'NONE', #20583, .T. ) ;
#135040 = CARTESIAN_POINT ( 'NONE',  ( -30.79333936457826226, 21.75929247661549581, 4.998822639870701856 ) ) ;
#135041 = LINE ( 'NONE', #90054, #49560 ) ;
#135042 = DIRECTION ( 'NONE',  ( -0.3543493200069162685, -0.000000000000000000, -0.9351131265310288487 ) ) ;
#135043 = LINE ( 'NONE', #104507, #75315 ) ;
#135044 = EDGE_CURVE ( 'NONE', #121175, #74390, #30561, .T. ) ;
#135045 = FACE_OUTER_BOUND ( 'NONE', #70982, .T. ) ;
#135046 = LINE ( 'NONE', #92924, #20320 ) ;
#135047 = CARTESIAN_POINT ( 'NONE',  ( 50.68336038379622011, -2.130196079827426203, 7.949999999999997513 ) ) ;
#135048 = PLANE ( 'NONE',  #53717 ) ;
#135050 = LINE ( 'NONE', #122693, #117817 ) ;
#135049 = AXIS2_PLACEMENT_3D ( 'NONE', #122658, #21215, #865 ) ;
#135051 = ORIENTED_EDGE ( 'NONE', *, *, #21934, .F. ) ;
#135052 = VERTEX_POINT ( 'NONE', #106653 ) ;
#135053 = CARTESIAN_POINT ( 'NONE',  ( 45.77083333333332149, -7.949999999999999289, -2.130196079827426203 ) ) ;
#135054 = VERTEX_POINT ( 'NONE', #50878 ) ;
#135055 = LINE ( 'NONE', #102415, #23045 ) ;
#135056 = LINE ( 'NONE', #14670, #67049 ) ;
#135057 = ORIENTED_EDGE ( 'NONE', *, *, #117257, .T. ) ;
#135058 = CARTESIAN_POINT ( 'NONE',  ( -19.93618820135885272, -3.270000000000008455, -36.39086428169088094 ) ) ;
#135059 = VECTOR ( 'NONE', #123720, 999.9999999999998863 ) ;
#135060 = CARTESIAN_POINT ( 'NONE',  ( 32.99999999999977973, 7.552185695429098899, 5.000000000000000000 ) ) ;
#135061 = CARTESIAN_POINT ( 'NONE',  ( 39.52126352523143282, -4.472830434245839371, -4.472830434245840259 ) ) ;
#135062 = AXIS2_PLACEMENT_3D ( 'NONE', #6696, #127086, #72775 ) ;
#135063 = ORIENTED_EDGE ( 'NONE', *, *, #143232, .T. ) ;
#135064 = EDGE_CURVE ( 'NONE', #13774, #62936, #7342, .T. ) ;
#135065 = LINE ( 'NONE', #48746, #121975 ) ;
#135066 = ORIENTED_EDGE ( 'NONE', *, *, #72475, .T. ) ;
#135067 = CARTESIAN_POINT ( 'NONE',  ( 12.19999999999999574, -27.55040120718573604, 16.07347811296899209 ) ) ;
#135068 = DIRECTION ( 'NONE',  ( 0.7071067811865487940, 0.7071067811865463515, 0.000000000000000000 ) ) ;
#135070 = EDGE_CURVE ( 'NONE', #40303, #16626, #29817, .T. ) ;
#135069 = DIRECTION ( 'NONE',  ( -0.7071067811865486830, -0.7071067811865464625, 0.000000000000000000 ) ) ;
#135071 = AXIS2_PLACEMENT_3D ( 'NONE', #138163, #131569, #55442 ) ;
#135072 = DIRECTION ( 'NONE',  ( -0.6830127018922180770, 0.6830127018922202975, -0.2588190451025213501 ) ) ;
#135073 = ORIENTED_EDGE ( 'NONE', *, *, #77838, .F. ) ;
#135074 = CARTESIAN_POINT ( 'NONE',  ( -8.292893218813391698, 20.25929247661551003, 5.000000000000000000 ) ) ;
#135075 = ORIENTED_EDGE ( 'NONE', *, *, #119317, .F. ) ;
#135076 = CARTESIAN_POINT ( 'NONE',  ( 38.87086038379622721, 6.884901960086289741, -3.974999999999993427 ) ) ;
#135077 = DIRECTION ( 'NONE',  ( -0.3543493200069162685, -0.000000000000000000, -0.9351131265310288487 ) ) ;
#135078 = LINE ( 'NONE', #35770, #91756 ) ;
#135079 = DIRECTION ( 'NONE',  ( -0.7071067811865486830, -0.7071067811865464625, 0.000000000000000000 ) ) ;
#135080 = LINE ( 'NONE', #34303, #115598 ) ;
#135081 = EDGE_CURVE ( 'NONE', #35471, #50028, #84927, .T. ) ;
#135082 = AXIS2_PLACEMENT_3D ( 'NONE', #114885, #126497, #48240 ) ;
#135083 = VECTOR ( 'NONE', #44610, 1000.000000000000000 ) ;
#135084 = LINE ( 'NONE', #55358, #29139 ) ;
#135085 = CARTESIAN_POINT ( 'NONE',  ( 55.32876352523144448, 0.000000000000000000, -6.109999999999998543 ) ) ;
#135086 = DIRECTION ( 'NONE',  ( 0.000000000000000000, 1.000000000000000000, 0.000000000000000000 ) ) ;
#135087 = EDGE_CURVE ( 'NONE', #2401, #106633, #87334, .T. ) ;
#135088 = DIRECTION ( 'NONE',  ( 1.000000000000000000, 0.000000000000000000, 0.000000000000000000 ) ) ;
#135090 = ORIENTED_EDGE ( 'NONE', *, *, #47798, .F. ) ;
#135089 = LINE ( 'NONE', #90104, #6232 ) ;
#135091 = ORIENTED_EDGE ( 'NONE', *, *, #133433, .T. ) ;
#135092 = AXIS2_PLACEMENT_3D ( 'NONE', #1019, #124951, #110489 ) ;
#135093 = CARTESIAN_POINT ( 'NONE',  ( 4.171830600776440079, 12.75929247661559351, 4.000000000000000000 ) ) ;
#135094 = ORIENTED_EDGE ( 'NONE', *, *, #97993, .F. ) ;
#135095 = CARTESIAN_POINT ( 'NONE',  ( 0.2569208697893813897, 0.3999999999999995781, 2.015694669338588429 ) ) ;
#135096 = ORIENTED_EDGE ( 'NONE', *, *, #77304, .T. ) ;
#135097 = CARTESIAN_POINT ( 'NONE',  ( -25.39999999999996305, 3.061616997868383141E-16, -2.500000000000000000 ) ) ;
#135098 = CARTESIAN_POINT ( 'NONE',  ( -31.92499999999997584, -6.270000000000012896, -40.00000000000000000 ) ) ;
#135099 = AXIS2_PLACEMENT_3D ( 'NONE', #100912, #90031, #15301 ) ;
#135100 = CARTESIAN_POINT ( 'NONE',  ( 28.00000000000002487, -52.14999999999999147, 59.92500000000006111 ) ) ;
#135101 = ADVANCED_FACE ( 'NONE', ( #107387 ), #51605, .F. ) ;
#135102 = FACE_BOUND ( 'NONE', #87512, .T. ) ;
#135103 = CARTESIAN_POINT ( 'NONE',  ( -14.09068777029287567, 6.496774105546209377, 4.000000000000000000 ) ) ;
#135104 = EDGE_CURVE ( 'NONE', #139894, #79492, #82808, .T. ) ;
#135105 = DIRECTION ( 'NONE',  ( -1.000000000000000000, -1.224606353822377258E-16, -0.000000000000000000 ) ) ;
#135106 = VECTOR ( 'NONE', #36595, 1000.000000000000000 ) ;
#135107 = CARTESIAN_POINT ( 'NONE',  ( 22.21247294953710494, 0.000000000000000000, 6.094999999999989981 ) ) ;
#135109 = ORIENTED_EDGE ( 'NONE', *, *, #12421, .F. ) ;
#135108 = CARTESIAN_POINT ( 'NONE',  ( -19.49999999999987210, -2.777013188829482893, 4.549262955118030582 ) ) ;
#135110 = VERTEX_POINT ( 'NONE', #19665 ) ;
#135111 = CARTESIAN_POINT ( 'NONE',  ( -6.771599798802371950, -34.64999999999999147, 17.99210858042621908 ) ) ;
#135112 = ORIENTED_EDGE ( 'NONE', *, *, #136647, .T. ) ;
#135113 = ORIENTED_EDGE ( 'NONE', *, *, #127966, .T. ) ;
#135114 = CARTESIAN_POINT ( 'NONE',  ( 75.45376352523145158, -6.109999999999998543, -3.741295971395162543E-16 ) ) ;
#135115 = ORIENTED_EDGE ( 'NONE', *, *, #96828, .T. ) ;
#135116 = DIRECTION ( 'NONE',  ( 0.7071067811865487940, 0.7071067811865463515, 0.000000000000000000 ) ) ;
#135117 = ORIENTED_EDGE ( 'NONE', *, *, #25225, .T. ) ;
#135118 = LINE ( 'NONE', #112615, #65331 ) ;
#135119 = VECTOR ( 'NONE', #142248, 1000.000000000000000 ) ;
#135120 = CARTESIAN_POINT ( 'NONE',  ( 122.1875000000000000, -5.819803920172573974, 5.819803920172573086 ) ) ;
#135121 = EDGE_CURVE ( 'NONE', #54378, #127190, #118244, .T. ) ;
#135122 = PLANE ( 'NONE',  #119644 ) ;
#135123 = CARTESIAN_POINT ( 'NONE',  ( 0.000000000000000000, 0.000000000000000000, 5.000000000000000000 ) ) ;
#135124 = DIRECTION ( 'NONE',  ( 0.6830127018922180770, -0.6830127018922204085, -0.2588190451025213501 ) ) ;
#135125 = CARTESIAN_POINT ( 'NONE',  ( 14.99999999999989697, -9.412538124160656494, 4.000000000000000000 ) ) ;
#135126 = CARTESIAN_POINT ( 'NONE',  ( 0.000000000000000000, 0.000000000000000000, 5.000000000000000000 ) ) ;
#135127 = ORIENTED_EDGE ( 'NONE', *, *, #37672, .T. ) ;
#135128 = VECTOR ( 'NONE', #15200, 1000.000000000000000 ) ;
#135129 = ORIENTED_EDGE ( 'NONE', *, *, #77584, .F. ) ;
#135130 = CARTESIAN_POINT ( 'NONE',  ( 24.99581563014004715, 3.703558271726553830, 4.317415941188023076 ) ) ;
#135131 = CARTESIAN_POINT ( 'NONE',  ( 19.41972383043609440, 2.500000000000000888, 0.000000000000000000 ) ) ;
#135132 = EDGE_LOOP ( 'NONE', ( #88796, #45107, #2985, #107665 ) ) ;
#135133 = ORIENTED_EDGE ( 'NONE', *, *, #139445, .F. ) ;
#135134 = ORIENTED_EDGE ( 'NONE', *, *, #58039, .T. ) ;
#135135 = ADVANCED_FACE ( 'NONE', ( #50174 ), #89596, .T. ) ;
#135136 = CARTESIAN_POINT ( 'NONE',  ( 26.39626352523142927, 4.472830434245840259, -4.472830434245838482 ) ) ;
#135137 = ORIENTED_EDGE ( 'NONE', *, *, #109008, .T. ) ;
#135138 = CARTESIAN_POINT ( 'NONE',  ( 44.89583333333332149, -2.130196079827427091, 7.949999999999998401 ) ) ;
#135139 = AXIS2_PLACEMENT_3D ( 'NONE', #9516, #44350, #125274 ) ;
#135140 = CARTESIAN_POINT ( 'NONE',  ( -8.292893218813397027, -18.74070752338409562, 5.000000000000000000 ) ) ;
#135141 = VECTOR ( 'NONE', #139101, 1000.000000000000227 ) ;
#135142 = CARTESIAN_POINT ( 'NONE',  ( 1.671236474768553082, 0.000000000000000000, 7.934999999999990727 ) ) ;
#135143 = CARTESIAN_POINT ( 'NONE',  ( 16.42522110613515451, 1.155309361455200357, -30.62612907365273429 ) ) ;
#135144 = ORIENTED_EDGE ( 'NONE', *, *, #129818, .T. ) ;
#135145 = DIRECTION ( 'NONE',  ( -0.6830127018922181881, 0.6830127018922202975, -0.2588190451025214056 ) ) ;
#135146 = DIRECTION ( 'NONE',  ( -0.6830127018922181881, 0.6830127018922202975, -0.2588190451025214056 ) ) ;
#135147 = CARTESIAN_POINT ( 'NONE',  ( -39.33010218547241266, 17.25929247661553845, 19.83885114516080606 ) ) ;
#135149 = EDGE_LOOP ( 'NONE', ( #90321, #120492, #30588, #34561 ) ) ;
#135148 = LINE ( 'NONE', #45287, #77314 ) ;
#135150 = ORIENTED_EDGE ( 'NONE', *, *, #52449, .T. ) ;
#135151 = CARTESIAN_POINT ( 'NONE',  ( 34.49999999999975842, -16.53574439159934073, 4.994342998332164107 ) ) ;
#135152 = LINE ( 'NONE', #134420, #21365 ) ;
#135153 = AXIS2_PLACEMENT_3D ( 'NONE', #9564, #53837, #131381 ) ;
#135154 = PLANE ( 'NONE',  #137407 ) ;
#135155 = ORIENTED_EDGE ( 'NONE', *, *, #142204, .F. ) ;
#135156 = DIRECTION ( 'NONE',  ( -1.000000000000000000, -1.224606353822377258E-16, -0.000000000000000000 ) ) ;
#135157 = DIRECTION ( 'NONE',  ( -0.7071067811865486830, -0.7071067811865464625, 0.000000000000000000 ) ) ;
#135158 = AXIS2_PLACEMENT_3D ( 'NONE', #24756, #113177, #13853 ) ;
#135159 = CARTESIAN_POINT ( 'NONE',  ( -25.49999999999981526, 1.087461875839237591, 4.000000000000000000 ) ) ;
#135160 = DIRECTION ( 'NONE',  ( 0.000000000000000000, 0.000000000000000000, 1.000000000000000000 ) ) ;
#135161 = DIRECTION ( 'NONE',  ( -0.7071067811865486830, -0.7071067811865464625, 0.000000000000000000 ) ) ;
#135162 = CARTESIAN_POINT ( 'NONE',  ( -12.70710678118645198, -6.740707523384211086, 5.000000000000000000 ) ) ;
#135163 = PLANE ( 'NONE',  #2958 ) ;
#135164 =( BOUNDED_CURVE ( )  B_SPLINE_CURVE ( 3, ( #64163, #131557, #8994, #20627 ),
 .UNSPECIFIED., .F., .T. ) 
 B_SPLINE_CURVE_WITH_KNOTS ( ( 4, 4 ),
 ( 2.001653308786175867, 3.503810798801451742 ),
 .UNSPECIFIED. ) 
 CURVE ( )  GEOMETRIC_REPRESENTATION_ITEM ( )  RATIONAL_B_SPLINE_CURVE ( ( 1.000000000000000000, 0.8206354192515253887, 0.8206354192515253887, 1.000000000000000000 ) ) 
 REPRESENTATION_ITEM ( '' )  );
#135165 = CARTESIAN_POINT ( 'NONE',  ( 21.77497294953710494, 4.461849672132300881, 4.461849672132299105 ) ) ;
#135166 = CARTESIAN_POINT ( 'NONE',  ( -5.999999999999963585, -13.39766691384884290, -10.96608748226464414 ) ) ;
#135167 = CARTESIAN_POINT ( 'NONE',  ( 114.7500000000000000, -9.735942053221458872E-16, 7.950000000000000178 ) ) ;
#135168 = VERTEX_POINT ( 'NONE', #27677 ) ;
#135169 = ORIENTED_EDGE ( 'NONE', *, *, #28115, .F. ) ;
#135170 =( NAMED_UNIT ( * ) SI_UNIT ( $, .STERADIAN. ) SOLID_ANGLE_UNIT ( ) );
#135171 = CARTESIAN_POINT ( 'NONE',  ( -19.17183060077633883, 18.75929247661552068, 4.000000000000000000 ) ) ;
#135172 = CIRCLE ( 'NONE', #121358, 2.500000000000000888 ) ;
#135173 = DIRECTION ( 'NONE',  ( 0.000000000000000000, 0.000000000000000000, -1.000000000000000000 ) ) ;
#135174 = CARTESIAN_POINT ( 'NONE',  ( 0.000000000000000000, -21.72500000000000142, 4.500000000000000888 ) ) ;
#135175 = ADVANCED_FACE ( 'NONE', ( #63904 ), #71947, .F. ) ;
#135176 = VECTOR ( 'NONE', #4896, 1000.000000000000000 ) ;
#135177 = DIRECTION ( 'NONE',  ( -1.000000000000000000, -0.000000000000000000, -0.000000000000000000 ) ) ;
#135178 = PLANE ( 'NONE',  #22800 ) ;
#135179 = ADVANCED_FACE ( 'NONE', ( #96476 ), #52992, .F. ) ;
#135180 = EDGE_CURVE ( 'NONE', #3063, #23219, #74055, .T. ) ;
#135181 = ORIENTED_EDGE ( 'NONE', *, *, #61257, .F. ) ;
#135182 = CARTESIAN_POINT ( 'NONE',  ( 122.6835989386367345, -1.600000000000094458, 34.92499999999998295 ) ) ;
#135183 = EDGE_CURVE ( 'NONE', #100764, #110693, #105250, .T. ) ;
#135184 = DIRECTION ( 'NONE',  ( 0.000000000000000000, -1.000000000000000000, 0.000000000000000000 ) ) ;
#135185 = AXIS2_PLACEMENT_3D ( 'NONE', #17129, #60682, #104102 ) ;
#135186 = DIRECTION ( 'NONE',  ( 0.7071067811865487940, 0.7071067811865463515, -0.000000000000000000 ) ) ;
#135187 = EDGE_CURVE ( 'NONE', #40291, #133314, #140720, .T. ) ;
#135188 = CARTESIAN_POINT ( 'NONE',  ( 58.68293019189811588, -1.637169565754159173, -6.109999999999999432 ) ) ;
#135189 = LINE ( 'NONE', #24256, #139081 ) ;
#135190 = CARTESIAN_POINT ( 'NONE',  ( 22.17183060077632462, 18.75929247661553134, 4.000000000000000000 ) ) ;
#135191 = CARTESIAN_POINT ( 'NONE',  ( 5.999999999999963585, 2.342191155542457714, -5.001666872980099043 ) ) ;
#135192 = ORIENTED_EDGE ( 'NONE', *, *, #11271, .F. ) ;
#135193 = EDGE_CURVE ( 'NONE', #13287, #10331, #39297, .T. ) ;
#135194 = VERTEX_POINT ( 'NONE', #83524 ) ;
#135195 = VECTOR ( 'NONE', #100367, 999.9999999999998863 ) ;
#135196 = DIRECTION ( 'NONE',  ( 0.000000000000000000, 0.000000000000000000, 1.000000000000000000 ) ) ;
#135197 = CARTESIAN_POINT ( 'NONE',  ( 24.09999999999999787, 2.055000000000001492, 2.516649172247811554E-16 ) ) ;
#135198 = CARTESIAN_POINT ( 'NONE',  ( -9.330102185472595622, 17.25929247661553845, 19.83885114516073500 ) ) ;
#135199 = EDGE_CURVE ( 'NONE', #107544, #123094, #8054, .T. ) ;
#135200 = CARTESIAN_POINT ( 'NONE',  ( -66.48921356237309510, -27.52281430457101763, 5.000000000000000000 ) ) ;
#135201 = EDGE_CURVE ( 'NONE', #110885, #53800, #135419, .T. ) ;
#135202 = PLANE ( 'NONE',  #76537 ) ;
#135203 = CARTESIAN_POINT ( 'NONE',  ( 2.292893218813441880, 8.259292476615639700, 5.000000000000000000 ) ) ;
#135204 = ORIENTED_EDGE ( 'NONE', *, *, #81642, .F. ) ;
#135205 = ORIENTED_EDGE ( 'NONE', *, *, #64932, .F. ) ;
#135206 = CARTESIAN_POINT ( 'NONE',  ( 1.828169399223521507, 18.75929247661552779, 4.000000000000000000 ) ) ;
#135207 = CARTESIAN_POINT ( 'NONE',  ( -33.48921356237309510, -27.52281430457078670, 5.000000000000000000 ) ) ;
#135208 = CARTESIAN_POINT ( 'NONE',  ( -22.49999999999984013, -19.91253812416055879, 4.000000000000000000 ) ) ;
#135209 = EDGE_CURVE ( 'NONE', #15478, #135598, #12171, .T. ) ;
#135210 = PLANE ( 'NONE',  #101260 ) ;
#135211 = CARTESIAN_POINT ( 'NONE',  ( 71.39169371712955581, 2.130196079827421762, 7.950000000000001066 ) ) ;
#135212 = CARTESIAN_POINT ( 'NONE',  ( 0.000000000000000000, 2.375000000000000000, 4.319999999999998508 ) ) ;
#135213 = AXIS2_PLACEMENT_3D ( 'NONE', #135825, #48113, #37220 ) ;
#135214 = DIRECTION ( 'NONE',  ( 0.2400000000000085398, -0.000000000000000000, 0.9707728879609256456 ) ) ;
#135215 = ORIENTED_EDGE ( 'NONE', *, *, #21229, .T. ) ;
#135216 = CARTESIAN_POINT ( 'NONE',  ( 74.50000000000000000, 0.000000000000000000, -7.950000000000000178 ) ) ;
#135217 = CARTESIAN_POINT ( 'NONE',  ( 36.48921356237310221, -27.52281430457080802, 5.000000000000000000 ) ) ;
#135218 = DIRECTION ( 'NONE',  ( 0.6830127018922181881, 0.6830127018922202975, -0.2588190451025214056 ) ) ;
#135219 = CARTESIAN_POINT ( 'NONE',  ( -11.99999999999991118, 7.552185695429091794, 5.000000000000000000 ) ) ;
#135220 = ORIENTED_EDGE ( 'NONE', *, *, #73162, .F. ) ;
#135221 = AXIS2_PLACEMENT_3D ( 'NONE', #106532, #107954, #41297 ) ;
#135222 = LINE ( 'NONE', #92370, #21268 ) ;
#135223 = CARTESIAN_POINT ( 'NONE',  ( -8.999999999999936051, -6.033600742197680056, 5.000000000000000000 ) ) ;
#135224 = CARTESIAN_POINT ( 'NONE',  ( 66.50043019189810423, -3.055000000000002380, 5.291415217122920289 ) ) ;
#135225 = EDGE_CURVE ( 'NONE', #25103, #1859, #112882, .T. ) ;
#135226 = CARTESIAN_POINT ( 'NONE',  ( -29.99999999999977618, 20.58746187583903264, 4.000000000000000000 ) ) ;
#135227 = EDGE_LOOP ( 'NONE', ( #45587, #69543, #49964, #9023 ) ) ;
#135228 = EDGE_LOOP ( 'NONE', ( #130269, #49901, #39383, #101897 ) ) ;
#135229 = DIRECTION ( 'NONE',  ( -0.000000000000000000, -0.3543493200069152693, 0.9351131265310292928 ) ) ;
#135230 = FILL_AREA_STYLE ('',( #110561 ) ) ;
#135231 = CARTESIAN_POINT ( 'NONE',  ( -13.09320915088844650, 2.775078171252264081, 4.657771095945246742 ) ) ;
#135232 = DIRECTION ( 'NONE',  ( -0.7071067811865487940, 0.7071067811865463515, 0.000000000000000000 ) ) ;
#135234 = EDGE_LOOP ( 'NONE', ( #4715, #19113, #5843 ) ) ;
#135233 = DIRECTION ( 'NONE',  ( -1.000000000000000000, -0.000000000000000000, 0.000000000000000000 ) ) ;
#135235 = DIRECTION ( 'NONE',  ( 0.000000000000000000, -1.000000000000000000, 0.000000000000000000 ) ) ;
#135236 = LINE ( 'NONE', #99712, #128710 ) ;
#135237 = DIRECTION ( 'NONE',  ( 1.000000000000000000, 1.224606353822377258E-16, 0.000000000000000000 ) ) ;
#135238 = VECTOR ( 'NONE', #121516, 1000.000000000000000 ) ;
#135239 = CARTESIAN_POINT ( 'NONE',  ( 60.48921356237309510, -27.52281430457097500, 5.000000000000000000 ) ) ;
#135240 = ORIENTED_EDGE ( 'NONE', *, *, #70023, .F. ) ;
#135241 = ORIENTED_EDGE ( 'NONE', *, *, #50413, .F. ) ;
#135242 = CARTESIAN_POINT ( 'NONE',  ( 51.62543019189811133, 5.291415217122919401, 3.055000000000002824 ) ) ;
#135243 = AXIS2_PLACEMENT_3D ( 'NONE', #10679, #31061, #120146 ) ;
#135244 = ORIENTED_EDGE ( 'NONE', *, *, #18314, .F. ) ;
#135245 = CARTESIAN_POINT ( 'NONE',  ( -10.49999999999991296, -6.839392718269134974, -8.480912228396059405 ) ) ;
#135246 = DIRECTION ( 'NONE',  ( -0.7071067811865486830, -0.7071067811865464625, 0.000000000000000000 ) ) ;
#135247 = ADVANCED_FACE ( 'NONE', ( #112920 ), #45565, .F. ) ;
#135248 = DIRECTION ( 'NONE',  ( -0.000000000000000000, 0.000000000000000000, 1.000000000000000000 ) ) ;
#135249 = CARTESIAN_POINT ( 'NONE',  ( 53.79166666666667140, 3.975000000000003642, -6.884901960086285300 ) ) ;
#135250 = ORIENTED_EDGE ( 'NONE', *, *, #98117, .T. ) ;
#135251 = ORIENTED_EDGE ( 'NONE', *, *, #61199, .T. ) ;
#135252 = CARTESIAN_POINT ( 'NONE',  ( -10.49999999999992895, 11.52377502935401843, -1.522421517564061411 ) ) ;
#135253 = CARTESIAN_POINT ( 'NONE',  ( -17.00227007675744417, -0.8971235601602828291, -35.72539454602287634 ) ) ;
#135254 = EDGE_LOOP ( 'NONE', ( #98120, #96346, #72493, #86598 ) ) ;
#135255 = MECHANICAL_DESIGN_GEOMETRIC_PRESENTATION_REPRESENTATION (  '', ( #91271 ), #19519 ) ;
#135256 = EDGE_CURVE ( 'NONE', #88862, #38475, #113625, .T. ) ;
#135258 = VECTOR ( 'NONE', #45203, 1000.000000000000000 ) ;
#135257 = DIRECTION ( 'NONE',  ( 0.6830127018922181881, 0.6830127018922202975, -0.2588190451025214056 ) ) ;
#135259 = ORIENTED_EDGE ( 'NONE', *, *, #13442, .F. ) ;
#135260 = CARTESIAN_POINT ( 'NONE',  ( 17.99451991528748351, 28.92564299267950645, 4.000000000000000000 ) ) ;
#135261 = CARTESIAN_POINT ( 'NONE',  ( 60.18398860626900415, 28.73617430169829490, 5.000000000000000000 ) ) ;
#135262 = ORIENTED_EDGE ( 'NONE', *, *, #92794, .T. ) ;
#135263 = VECTOR ( 'NONE', #124093, 1000.000000000000227 ) ;
#135264 = VECTOR ( 'NONE', #18289, 1000.000000000000000 ) ;
#135265 = ADVANCED_FACE ( 'NONE', ( #102050 ), #134705, .F. ) ;
#135266 = FACE_BOUND ( 'NONE', #143305, .T. ) ;
#135267 = DIRECTION ( 'NONE',  ( 0.7071067811865486830, -0.7071067811865464625, -0.000000000000000000 ) ) ;
#135268 = DIRECTION ( 'NONE',  ( 0.7071067811865487940, 0.7071067811865463515, 0.000000000000000000 ) ) ;
#135269 = FACE_OUTER_BOUND ( 'NONE', #44560, .T. ) ;
#135270 = CARTESIAN_POINT ( 'NONE',  ( -18.70710678118640402, -6.740707523384209310, 5.000000000000000000 ) ) ;
#135271 = AXIS2_PLACEMENT_3D ( 'NONE', #88395, #98530, #121691 ) ;
#135272 = CARTESIAN_POINT ( 'NONE',  ( -0.2997448713915885632, -27.71228299555206220, 4.000000000000000000 ) ) ;
#135273 = DIRECTION ( 'NONE',  ( -0.9999999999999998890, -1.027676218325029051E-30, 1.224646799147357645E-16 ) ) ;
#135274 = ORIENTED_EDGE ( 'NONE', *, *, #68377, .F. ) ;
#135275 = VECTOR ( 'NONE', #93040, 1000.000000000000000 ) ;
#135276 = ORIENTED_EDGE ( 'NONE', *, *, #36590, .F. ) ;
#135277 = CARTESIAN_POINT ( 'NONE',  ( 102.4329301918980946, 1.637169565754156508, 6.110000000000000320 ) ) ;
#135278 = VERTEX_POINT ( 'NONE', #124515 ) ;
#135279 = LINE ( 'NONE', #36636, #139179 ) ;
#135280 = ORIENTED_EDGE ( 'NONE', *, *, #63338, .T. ) ;
#135281 = DIRECTION ( 'NONE',  ( -1.000000000000000000, -0.000000000000000000, -0.000000000000000000 ) ) ;
#135282 = LINE ( 'NONE', #35966, #126501 ) ;
#135283 = LINE ( 'NONE', #80887, #40183 ) ;
#135284 = ORIENTED_EDGE ( 'NONE', *, *, #28267, .T. ) ;
#135285 = CARTESIAN_POINT ( 'NONE',  ( 18.18398860626898994, 28.73617430169800002, 5.000000000000000000 ) ) ;
#135286 = EDGE_CURVE ( 'NONE', #139679, #37520, #80326, .T. ) ;
#135287 = LINE ( 'NONE', #35970, #3735 ) ;
#135288 = CARTESIAN_POINT ( 'NONE',  ( 21.77612515620402078, 4.584330080086930965E-16, 0.000000000000000000 ) ) ;
#135289 = LINE ( 'NONE', #103317, #89725 ) ;
#135290 = CARTESIAN_POINT ( 'NONE',  ( -18.64318742751726887, -20.24070752338407075, 21.22881796311208191 ) ) ;
#135291 = AXIS2_PLACEMENT_3D ( 'NONE', #41159, #129585, #52051 ) ;
#135292 = CARTESIAN_POINT ( 'NONE',  ( -12.69999999999998153, 3.061616997868383634E-16, -2.500000000000000444 ) ) ;
#135293 = ORIENTED_EDGE ( 'NONE', *, *, #85819, .F. ) ;
#135294 = CARTESIAN_POINT ( 'NONE',  ( 17.06332250466817158, 4.584330080086930965E-16, 0.000000000000000000 ) ) ;
#135295 = CARTESIAN_POINT ( 'NONE',  ( -30.70701326429283640, -21.74070752338405654, 4.999753212805224223 ) ) ;
#135296 = VERTEX_POINT ( 'NONE', #122345 ) ;
#135297 = EDGE_CURVE ( 'NONE', #25651, #71266, #23022, .T. ) ;
#135298 = ORIENTED_EDGE ( 'NONE', *, *, #110101, .T. ) ;
#135299 = EDGE_CURVE ( 'NONE', #137211, #78146, #31860, .T. ) ;
#135300 = ORIENTED_EDGE ( 'NONE', *, *, #64308, .F. ) ;
#135301 = B_SPLINE_CURVE_WITH_KNOTS ( 'NONE', 3,
 ( #90731, #32785, #34194, #123362, #80, #68287, #78412, #87852, #79161, #79879, #77011, #21874, #44383, #122609, #13119, #23281 ),
 .UNSPECIFIED., .F., .F.,
 ( 4, 2, 2, 2, 2, 2, 2, 4 ),
 ( 0.000000000000000000, 0.0005244841081218725408, 0.001048968216243745082, 0.002097936432487507077, 0.003146904648731268638, 0.004195872864975030633, 0.006293809297462554624, 0.008391745729950078614 ),
 .UNSPECIFIED. ) ;
#135302 = CARTESIAN_POINT ( 'NONE',  ( 53.22959685856476852, -6.110000000000000320, -1.637169565754161393 ) ) ;
#135303 = ORIENTED_EDGE ( 'NONE', *, *, #138071, .F. ) ;
#135304 = CARTESIAN_POINT ( 'NONE',  ( 8.649972949537106715, -4.461849672132299105, 4.461849672132299993 ) ) ;
#135305 = CARTESIAN_POINT ( 'NONE',  ( 93.04209685856476142, 5.291415217122923842, -3.054999999999996163 ) ) ;
#135306 = DIRECTION ( 'NONE',  ( -0.3543493200069162685, -0.000000000000000000, -0.9351131265310288487 ) ) ;
#135307 = ORIENTED_EDGE ( 'NONE', *, *, #86002, .T. ) ;
#135308 = DIRECTION ( 'NONE',  ( 0.000000000000000000, -0.3543493200069153248, -0.9351131265310291818 ) ) ;
#135309 = EDGE_LOOP ( 'NONE', ( #16303, #77824, #62593, #39616 ) ) ;
#135310 =( LENGTH_UNIT ( ) NAMED_UNIT ( * ) SI_UNIT ( .MILLI., .METRE. ) );
#135311 = DIRECTION ( 'NONE',  ( -0.000000000000000000, 0.000000000000000000, 1.000000000000000000 ) ) ;
#135312 = ORIENTED_EDGE ( 'NONE', *, *, #59279, .T. ) ;
#135313 = ADVANCED_FACE ( 'NONE', ( #90463 ), #101330, .F. ) ;
#135314 = VECTOR ( 'NONE', #58102, 1000.000000000000227 ) ;
#135315 = LINE ( 'NONE', #101219, #58367 ) ;
#135316 = DIRECTION ( 'NONE',  ( -0.7071067811865486830, -0.7071067811865464625, 0.000000000000000000 ) ) ;
#135317 = CARTESIAN_POINT ( 'NONE',  ( 125.4745968585647944, 1.637169565754164280, -6.109999999999997655 ) ) ;
#135318 = EDGE_LOOP ( 'NONE', ( #16043, #123652, #48562, #134898 ) ) ;
#135319 = DIRECTION ( 'NONE',  ( -0.7071067811865486830, -0.7071067811865464625, 0.000000000000000000 ) ) ;
#135320 = VERTEX_POINT ( 'NONE', #133273 ) ;
#135321 = VERTEX_POINT ( 'NONE', #35403 ) ;
#135322 = VERTEX_POINT ( 'NONE', #13580 ) ;
#135323 = CARTESIAN_POINT ( 'NONE',  ( 16.49999999999989342, -14.94781430457067550, 5.000000000000000000 ) ) ;
#135324 = FACE_OUTER_BOUND ( 'NONE', #22256, .T. ) ;
#135325 = DIRECTION ( 'NONE',  ( -0.3543493200069162685, -0.000000000000000000, -0.9351131265310288487 ) ) ;
#135326 = DIRECTION ( 'NONE',  ( -0.7071067811865486830, 0.7071067811865464625, 0.000000000000000000 ) ) ;
#135327 = DIRECTION ( 'NONE',  ( -0.7071067811865487940, 0.7071067811865463515, 0.000000000000000000 ) ) ;
#135328 = VERTEX_POINT ( 'NONE', #66578 ) ;
#135329 = AXIS2_PLACEMENT_3D ( 'NONE', #110997, #78406, #132087 ) ;
#135330 = EDGE_CURVE ( 'NONE', #139613, #40545, #89739, .T. ) ;
#135331 = CIRCLE ( 'NONE', #40439, 2.000000000000001776 ) ;
#135332 = CARTESIAN_POINT ( 'NONE',  ( 25.49956980810189222, -3.967499999999998028, -6.871911579029511330 ) ) ;
#135333 = DIRECTION ( 'NONE',  ( 0.000000000000000000, -1.000000000000000000, 0.000000000000000000 ) ) ;
#135334 = ADVANCED_FACE ( 'NONE', ( #86373 ), #112224, .F. ) ;
#135335 = DIRECTION ( 'NONE',  ( 0.7071067811865487940, 0.7071067811865463515, 0.000000000000000000 ) ) ;
#135336 = LINE ( 'NONE', #113537, #86036 ) ;
#135337 = ORIENTED_EDGE ( 'NONE', *, *, #80719, .F. ) ;
#135338 = EDGE_CURVE ( 'NONE', #44187, #141351, #123102, .T. ) ;
#135339 = VECTOR ( 'NONE', #133067, 999.9999999999998863 ) ;
#135340 = EDGE_LOOP ( 'NONE', ( #58051, #57783, #141933, #47158 ) ) ;
#135341 = ORIENTED_EDGE ( 'NONE', *, *, #108355, .T. ) ;
#135342 = CARTESIAN_POINT ( 'NONE',  ( 2.994519915287485734, 28.92564299267940342, 4.000000000000000000 ) ) ;
#135343 = CYLINDRICAL_SURFACE ( 'NONE', #9315, 0.5000000000000004441 ) ;
#135344 = CARTESIAN_POINT ( 'NONE',  ( 17.99999999999987566, -9.412538124160654718, 4.000000000000000000 ) ) ;
#135345 = PLANE ( 'NONE',  #11203 ) ;
#135346 = ADVANCED_FACE ( 'NONE', ( #11430 ), #12876, .T. ) ;
#135348 = EDGE_CURVE ( 'NONE', #27038, #81522, #24481, .T. ) ;
#135347 = CARTESIAN_POINT ( 'NONE',  ( 16.30000000000000071, 2.055000000000001492, 2.516649172247811554E-16 ) ) ;
#135349 = CARTESIAN_POINT ( 'NONE',  ( 19.17183060077633883, -8.240707523384196875, 4.000000000000000000 ) ) ;
#135350 = AXIS2_PLACEMENT_3D ( 'NONE', #59229, #92504, #91126 ) ;
#135351 = LINE ( 'NONE', #123027, #91194 ) ;
#135352 = DIRECTION ( 'NONE',  ( -0.000000000000000000, 0.3543493200069153248, 0.9351131265310292928 ) ) ;
#135353 = VECTOR ( 'NONE', #37142, 1000.000000000000114 ) ;
#135354 = DIRECTION ( 'NONE',  ( 0.6830127018922181881, 0.6830127018922202975, -0.2588190451025214056 ) ) ;
#135355 = CARTESIAN_POINT ( 'NONE',  ( -11.99999999999991118, 18.08204922493371924, 0.9627537363045149954 ) ) ;
#135356 = VERTEX_POINT ( 'NONE', #99903 ) ;
#135357 = FILL_AREA_STYLE_COLOUR ( '', #87027 ) ;
#135358 = ORIENTED_EDGE ( 'NONE', *, *, #30466, .T. ) ;
#135359 = CARTESIAN_POINT ( 'NONE',  ( -13.17183060077637791, 15.75929247661555443, 4.000000000000000000 ) ) ;
#135361 = EDGE_LOOP ( 'NONE', ( #113778, #117567, #8657, #106131 ) ) ;
#135360 = CARTESIAN_POINT ( 'NONE',  ( 2.206660635421510808, 21.75929247661549937, 4.998822639870701856 ) ) ;
#135362 = EDGE_CURVE ( 'NONE', #63259, #137446, #4818, .T. ) ;
#135363 = EDGE_CURVE ( 'NONE', #136197, #816, #5566, .T. ) ;
#135364 = CARTESIAN_POINT ( 'NONE',  ( 0.000000000000000000, -60.00000000000000000, 0.000000000000000000 ) ) ;
#135365 = CARTESIAN_POINT ( 'NONE',  ( 26.20666063542134339, 21.75929247661549581, 4.998822639870700968 ) ) ;
#135366 = ORIENTED_EDGE ( 'NONE', *, *, #106503, .F. ) ;
#135367 = CARTESIAN_POINT ( 'NONE',  ( 11.70025512860841133, -27.71228299555198049, 4.000000000000000000 ) ) ;
#135368 = ORIENTED_EDGE ( 'NONE', *, *, #67953, .F. ) ;
#135369 = LINE ( 'NONE', #114970, #141631 ) ;
#135370 = EDGE_LOOP ( 'NONE', ( #11482, #100361, #52949, #117456 ) ) ;
#135371 = STYLED_ITEM ( 'NONE', ( #86068 ), #8773 ) ;
#135372 = PLANE ( 'NONE',  #22094 ) ;
#135373 = EDGE_CURVE ( 'NONE', #24682, #100698, #60728, .T. ) ;
#135374 = CARTESIAN_POINT ( 'NONE',  ( 106.5375270504628844, -9.735942053221456900E-16, 7.949999999999998401 ) ) ;
#135375 = PLANE ( 'NONE',  #115720 ) ;
#135376 = AXIS2_PLACEMENT_3D ( 'NONE', #120287, #86988, #100018 ) ;
#135377 = CARTESIAN_POINT ( 'NONE',  ( -5.994519915287488843, 28.92564299267942118, 4.000000000000000000 ) ) ;
#135378 = ORIENTED_EDGE ( 'NONE', *, *, #136210, .F. ) ;
#135379 = VECTOR ( 'NONE', #61471, 1000.000000000000000 ) ;
#135380 = DIRECTION ( 'NONE',  ( -1.000000000000000000, -1.224606353822377258E-16, -0.000000000000000000 ) ) ;
#135381 = PLANE ( 'NONE',  #51927 ) ;
#135382 = DIRECTION ( 'NONE',  ( -1.000000000000000000, -1.224606353822377258E-16, -0.000000000000000000 ) ) ;
#135383 = CARTESIAN_POINT ( 'NONE',  ( 12.83333333333333393, 5.278424836066143655, -3.047499999999997655 ) ) ;
#135384 = CARTESIAN_POINT ( 'NONE',  ( 0.000000000000000000, 0.000000000000000000, 5.000000000000000000 ) ) ;
#135385 = EDGE_CURVE ( 'NONE', #97144, #111999, #34150, .T. ) ;
#135386 = DIRECTION ( 'NONE',  ( -0.3543493200069162685, -0.000000000000000000, -0.9351131265310288487 ) ) ;
#135387 = EDGE_LOOP ( 'NONE', ( #104394, #24038, #131438, #106825 ) ) ;
#135388 = CIRCLE ( 'NONE', #63583, 5.999999999999998224 ) ;
#135389 = DIRECTION ( 'NONE',  ( -0.000000000000000000, -0.000000000000000000, 1.000000000000000000 ) ) ;
#135390 = ORIENTED_EDGE ( 'NONE', *, *, #43017, .T. ) ;
#135391 = CARTESIAN_POINT ( 'NONE',  ( 90.27126352523143282, 4.472830434245839371, 4.472830434245842035 ) ) ;
#135392 = CARTESIAN_POINT ( 'NONE',  ( 39.48921356237310221, -27.52281430457082934, 5.000000000000000000 ) ) ;
#135393 = CARTESIAN_POINT ( 'NONE',  ( -19.49999999999986500, -6.839392718269142080, -8.480912228396038088 ) ) ;
#135394 = EDGE_CURVE ( 'NONE', #125758, #102340, #81028, .T. ) ;
#135395 = CARTESIAN_POINT ( 'NONE',  ( 152.4000000000000057, -17.48000000000005016, 12.69999999999954454 ) ) ;
#135396 = CARTESIAN_POINT ( 'NONE',  ( -34.17183060077623225, -8.240707523384200428, 4.000000000000000000 ) ) ;
#135397 = VERTEX_POINT ( 'NONE', #94708 ) ;
#135398 = LINE ( 'NONE', #91851, #30327 ) ;
#135399 = CARTESIAN_POINT ( 'NONE',  ( 23.99999999999984013, -3.412538124160721331, 4.000000000000000000 ) ) ;
#135400 = VERTEX_POINT ( 'NONE', #3420 ) ;
#135401 = CARTESIAN_POINT ( 'NONE',  ( -6.005480084712508493, 28.92564299267933947, 4.000000000000000000 ) ) ;
#135402 = CARTESIAN_POINT ( 'NONE',  ( -1.179999999999998161, -6.391994993740214959, 10.00000000000000000 ) ) ;
#135405 = ADVANCED_FACE ( 'NONE', ( #138249 ), #47713, .F. ) ;
#135404 = VERTEX_POINT ( 'NONE', #59983 ) ;
#135403 = CARTESIAN_POINT ( 'NONE',  ( -17.29289321881333308, -6.740707523384211086, 5.000000000000000000 ) ) ;
#135406 = EDGE_CURVE ( 'NONE', #66395, #56761, #103453, .T. ) ;
#135407 = DIRECTION ( 'NONE',  ( -0.3543493200069162685, -0.000000000000000000, -0.9351131265310288487 ) ) ;
#135408 = DIRECTION ( 'NONE',  ( 0.6830127018922181881, 0.6830127018922202975, -0.2588190451025214056 ) ) ;
#135409 = DIRECTION ( 'NONE',  ( -0.000000000000000000, 0.000000000000000000, 1.000000000000000000 ) ) ;
#135410 = CYLINDRICAL_SURFACE ( 'NONE', #53929, 2.247899999999996901 ) ;
#135411 = ORIENTED_EDGE ( 'NONE', *, *, #95833, .F. ) ;
#135412 = EDGE_CURVE ( 'NONE', #19799, #121985, #49837, .T. ) ;
#135413 = ORIENTED_EDGE ( 'NONE', *, *, #67377, .F. ) ;
#135414 = ORIENTED_EDGE ( 'NONE', *, *, #35186, .F. ) ;
#135415 = CARTESIAN_POINT ( 'NONE',  ( 78.60459685856477563, 1.637169565754164946, -6.109999999999999432 ) ) ;
#135416 = ORIENTED_EDGE ( 'NONE', *, *, #44867, .T. ) ;
#135417 = DIRECTION ( 'NONE',  ( 0.3543493200069162685, -0.000000000000000000, -0.9351131265310288487 ) ) ;
#135418 = DIRECTION ( 'NONE',  ( -0.000000000000000000, -0.3543493200069152693, 0.9351131265310292928 ) ) ;
#135419 = LINE ( 'NONE', #23781, #119786 ) ;
#135420 = LINE ( 'NONE', #35404, #80507 ) ;
#135421 = ORIENTED_EDGE ( 'NONE', *, *, #18051, .F. ) ;
#135422 = CARTESIAN_POINT ( 'NONE',  ( 104.1041666666666572, 2.130196079827460398, 7.949999999999981526 ) ) ;
#135424 = AXIS2_PLACEMENT_3D ( 'NONE', #89108, #45621, #124574 ) ;
#135423 = CARTESIAN_POINT ( 'NONE',  ( 24.39999999999999858, -1.600000000000013634, 20.40202195861969159 ) ) ;
#135425 = FACE_OUTER_BOUND ( 'NONE', #11049, .T. ) ;
#135426 = CARTESIAN_POINT ( 'NONE',  ( 78.95376352523145158, -6.109999999999998543, -3.741295971395162543E-16 ) ) ;
#135427 = ORIENTED_EDGE ( 'NONE', *, *, #3268, .T. ) ;
#135428 = PLANE ( 'NONE',  #132374 ) ;
#135429 = DIRECTION ( 'NONE',  ( 0.000000000000000000, 0.000000000000000000, 1.000000000000000000 ) ) ;
#135430 = VERTEX_POINT ( 'NONE', #93311 ) ;
#135431 = ORIENTED_EDGE ( 'NONE', *, *, #91557, .T. ) ;
#135432 = CARTESIAN_POINT ( 'NONE',  ( -29.99999999999979039, -9.033600742197645417, 5.000000000000000000 ) ) ;
#135433 = DIRECTION ( 'NONE',  ( -1.000000000000000000, -1.224606353822377258E-16, -0.000000000000000000 ) ) ;
#135434 = CARTESIAN_POINT ( 'NONE',  ( 21.35873647476855552, 5.808823158059031044, -5.808823158059037262 ) ) ;
#135435 = FACE_OUTER_BOUND ( 'NONE', #115941, .T. ) ;
#135436 = SURFACE_STYLE_USAGE ( .BOTH. , #13604 ) ;
#135437 = DIRECTION ( 'NONE',  ( -0.000000000000000000, 0.000000000000000000, 1.000000000000000000 ) ) ;
#135438 = DIRECTION ( 'NONE',  ( -1.000000000000000000, -0.000000000000000000, -0.000000000000000000 ) ) ;
#135439 = AXIS2_PLACEMENT_3D ( 'NONE', #96823, #28046, #30914 ) ;
#135440 = ORIENTED_EDGE ( 'NONE', *, *, #113757, .F. ) ;
#135441 = EDGE_LOOP ( 'NONE', ( #75559, #122362, #54726, #57912, #40620 ) ) ;
#135442 =( GEOMETRIC_REPRESENTATION_CONTEXT ( 3 ) GLOBAL_UNCERTAINTY_ASSIGNED_CONTEXT ( ( #47503 ) ) GLOBAL_UNIT_ASSIGNED_CONTEXT ( ( #116815, #21614, #45540 ) ) REPRESENTATION_CONTEXT ( 'NONE', 'WORKASPACE' ) );
#135443 = CARTESIAN_POINT ( 'NONE',  ( 8.895833333333333925, 1.633150327867687324, -6.094999999999991758 ) ) ;
#135444 = ORIENTED_EDGE ( 'NONE', *, *, #14051, .F. ) ;
#135445 = EDGE_LOOP ( 'NONE', ( #62348, #26512, #25507, #55963 ) ) ;
#135446 = CARTESIAN_POINT ( 'NONE',  ( -9.475126127850408864, 14.25929247661557220, 9.797011795316615590 ) ) ;
#135447 = ORIENTED_EDGE ( 'NONE', *, *, #77954, .F. ) ;
#135448 = COLOUR_RGB ( '', 0.40784314, 0.44705882, 0.49803922) ;
#135449 = DIRECTION ( 'NONE',  ( 0.000000000000000000, -1.000000000000000000, 0.000000000000000000 ) ) ;
#135450 = DIRECTION ( 'NONE',  ( 0.7071067811865487940, 0.7071067811865463515, 0.000000000000000000 ) ) ;
#135451 = DIRECTION ( 'NONE',  ( 1.000000000000000000, 0.000000000000000000, 0.000000000000000000 ) ) ;
#135452 = PLANE ( 'NONE',  #67697 ) ;
#135453 = ORIENTED_EDGE ( 'NONE', *, *, #76437, .F. ) ;
#135454 = DIRECTION ( 'NONE',  ( 0.000000000000000000, -1.000000000000000000, 0.000000000000000000 ) ) ;
#135455 = VERTEX_POINT ( 'NONE', #61444 ) ;
#135456 = ADVANCED_FACE ( 'NONE', ( #116491 ), #128102, .F. ) ;
#135457 = DIRECTION ( 'NONE',  ( -0.7071067811865486830, -0.7071067811865464625, -0.000000000000000000 ) ) ;
#135458 = VERTEX_POINT ( 'NONE', #71571 ) ;
#135459 = ORIENTED_EDGE ( 'NONE', *, *, #89753, .T. ) ;
#135461 = EDGE_CURVE ( 'NONE', #114304, #96071, #4093, .T. ) ;
#135460 = LINE ( 'NONE', #60036, #106010 ) ;
#135462 = ORIENTED_EDGE ( 'NONE', *, *, #127643, .T. ) ;
#135463 = VERTEX_POINT ( 'NONE', #25915 ) ;
#135464 = LINE ( 'NONE', #43608, #4739 ) ;
#135465 = ORIENTED_EDGE ( 'NONE', *, *, #67875, .F. ) ;
#135466 = VECTOR ( 'NONE', #16219, 999.9999999999998863 ) ;
#135467 = DIRECTION ( 'NONE',  ( -0.7071067811865487940, 0.7071067811865463515, 0.000000000000000000 ) ) ;
#135468 = VECTOR ( 'NONE', #72036, 1000.000000000000000 ) ;
#135469 = VECTOR ( 'NONE', #8461, 1000.000000000000000 ) ;
#135470 = DIRECTION ( 'NONE',  ( -0.7071067811865486830, 0.7071067811865464625, 0.000000000000000000 ) ) ;
#135471 = CARTESIAN_POINT ( 'NONE',  ( 115.6462635252314328, -4.472830434245840259, 4.472830434245838482 ) ) ;
#135472 = DIRECTION ( 'NONE',  ( 0.6830127018922180770, -0.6830127018922204085, -0.2588190451025213501 ) ) ;
#135474 = EDGE_CURVE ( 'NONE', #53161, #100056, #91875, .T. ) ;
#135473 = VECTOR ( 'NONE', #72379, 1000.000000000000227 ) ;
#135475 = CARTESIAN_POINT ( 'NONE',  ( -1.499999999999987566, -4.796895815301023269, -3.611700055028684631 ) ) ;
#135476 = DIRECTION ( 'NONE',  ( -0.3543493200069162685, -0.000000000000000000, -0.9351131265310288487 ) ) ;
#135477 = DIRECTION ( 'NONE',  ( -0.6830127018922180770, -0.6830127018922204085, -0.2588190451025213501 ) ) ;
#135478 = EDGE_CURVE ( 'NONE', #118358, #89658, #115731, .T. ) ;
#135479 = DIRECTION ( 'NONE',  ( -0.3543493200069162685, -0.000000000000000000, -0.9351131265310288487 ) ) ;
#135480 = EDGE_LOOP ( 'NONE', ( #13431, #73770, #101669, #119318, #98356 ) ) ;
#135481 = DIRECTION ( 'NONE',  ( 1.000000000000000000, 0.000000000000000000, -0.000000000000000000 ) ) ;
#135482 = FACE_OUTER_BOUND ( 'NONE', #140300, .T. ) ;
#135483 = ORIENTED_EDGE ( 'NONE', *, *, #95825, .T. ) ;
#135484 = ORIENTED_EDGE ( 'NONE', *, *, #132915, .F. ) ;
#135485 = CARTESIAN_POINT ( 'NONE',  ( 24.18398860626899705, 28.73617430169804265, 5.000000000000000000 ) ) ;
#135486 = EDGE_CURVE ( 'NONE', #48518, #91920, #28059, .T. ) ;
#135487 = ORIENTED_EDGE ( 'NONE', *, *, #64393, .T. ) ;
#135488 = FACE_OUTER_BOUND ( 'NONE', #57253, .T. ) ;
#135489 = CARTESIAN_POINT ( 'NONE',  ( -41.99451991528749062, 28.92564299267967343, 4.000000000000000000 ) ) ;
#135490 = CARTESIAN_POINT ( 'NONE',  ( 38.99451991528749062, 28.92564299267965211, 4.000000000000000000 ) ) ;
#135491 = CARTESIAN_POINT ( 'NONE',  ( 10.49999999999993250, 0.4497235411627560353, -5.599840258123518488 ) ) ;
#135492 = ORIENTED_EDGE ( 'NONE', *, *, #128203, .T. ) ;
#135493 = CYLINDRICAL_SURFACE ( 'NONE', #7115, 2.552699999999959779 ) ;
#135494 = VERTEX_POINT ( 'NONE', #28785 ) ;
#135495 = CARTESIAN_POINT ( 'NONE',  ( -25.49999999999982236, -16.53360074219757081, 5.000000000000000000 ) ) ;
#135496 = CARTESIAN_POINT ( 'NONE',  ( 25.73373647476855552, 5.808823158059036373, 5.808823158059032821 ) ) ;
#135497 = ORIENTED_EDGE ( 'NONE', *, *, #135610, .T. ) ;
#135498 = CARTESIAN_POINT ( 'NONE',  ( 10.32500000000000107, -8.432637487761466488, 4.375000000000001776 ) ) ;
#135499 = CARTESIAN_POINT ( 'NONE',  ( 26.48334561358936412, 22.22500000000000142, 4.500000000000000888 ) ) ;
#135500 = ORIENTED_EDGE ( 'NONE', *, *, #116154, .F. ) ;
#135501 = EDGE_CURVE ( 'NONE', #3029, #133340, #39671, .T. ) ;
#135502 = VERTEX_POINT ( 'NONE', #117178 ) ;
#135503 = ORIENTED_EDGE ( 'NONE', *, *, #43411, .T. ) ;
#135504 = DIRECTION ( 'NONE',  ( -0.6830127018922181881, 0.6830127018922202975, -0.2588190451025214056 ) ) ;
#135505 = LINE ( 'NONE', #122451, #136646 ) ;
#135506 = FACE_OUTER_BOUND ( 'NONE', #21782, .T. ) ;
#135507 = FACE_OUTER_BOUND ( 'NONE', #113025, .T. ) ;
#135508 = ORIENTED_EDGE ( 'NONE', *, *, #140915, .F. ) ;
#135509 = CARTESIAN_POINT ( 'NONE',  ( 17.68342038867199051, -6.740707523384219968, 11.88629033278119884 ) ) ;
#135510 = EDGE_CURVE ( 'NONE', #36671, #4396, #99003, .T. ) ;
#135511 = EDGE_CURVE ( 'NONE', #54370, #94334, #114349, .T. ) ;
#135512 = CARTESIAN_POINT ( 'NONE',  ( -13.11151487241215108, 3.778085383357084659, 4.109577000315249862 ) ) ;
#135513 = LINE ( 'NONE', #69556, #92981 ) ;
#135514 = DIRECTION ( 'NONE',  ( 0.6830127018922180770, -0.6830127018922204085, -0.2588190451025213501 ) ) ;
#135515 = VERTEX_POINT ( 'NONE', #81760 ) ;
#135517 = EDGE_CURVE ( 'NONE', #117707, #18279, #26628, .T. ) ;
#135516 = FACE_OUTER_BOUND ( 'NONE', #15603, .T. ) ;
#135518 = VERTEX_POINT ( 'NONE', #86004 ) ;
#135520 = ORIENTED_EDGE ( 'NONE', *, *, #92626, .F. ) ;
#135519 = CARTESIAN_POINT ( 'NONE',  ( 61.46640106136302961, -43.14999999999999147, -34.92499999999998295 ) ) ;
#135522 = ORIENTED_EDGE ( 'NONE', *, *, #122336, .T. ) ;
#135521 = ADVANCED_FACE ( 'NONE', ( #75855 ), #141832, .T. ) ;
#135523 = EDGE_CURVE ( 'NONE', #117707, #288, #30929, .T. ) ;
#135524 = LINE ( 'NONE', #124627, #77127 ) ;
#135525 = PLANE ( 'NONE',  #103950 ) ;
#135526 = ORIENTED_EDGE ( 'NONE', *, *, #22975, .F. ) ;
#135527 = CARTESIAN_POINT ( 'NONE',  ( 3.707106781186523481, 17.25929247661554200, 5.000000000000000000 ) ) ;
#135528 = ORIENTED_EDGE ( 'NONE', *, *, #113226, .T. ) ;
#135529 = DIRECTION ( 'NONE',  ( 1.000000000000000000, 0.000000000000000000, 0.000000000000000000 ) ) ;
#135530 = FACE_OUTER_BOUND ( 'NONE', #11986, .T. ) ;
#135531 = VECTOR ( 'NONE', #14840, 1000.000000000000227 ) ;
#135532 = LINE ( 'NONE', #36218, #55447 ) ;
#135533 = EDGE_CURVE ( 'NONE', #73204, #122401, #12311, .T. ) ;
#135534 = CARTESIAN_POINT ( 'NONE',  ( -11.29289321881337571, -3.740707523384243505, 5.000000000000000000 ) ) ;
#135536 = PLANE ( 'NONE',  #136895 ) ;
#135535 = VECTOR ( 'NONE', #33786, 1000.000000000000000 ) ;
#135537 = CARTESIAN_POINT ( 'NONE',  ( -11.51078643762690490, -27.52281430457047406, 5.000000000000000000 ) ) ;
#135538 = DIRECTION ( 'NONE',  ( 1.000000000000000000, 0.000000000000000000, 0.000000000000000000 ) ) ;
#135539 = CARTESIAN_POINT ( 'NONE',  ( -34.92500000000001137, 22.22500000000000142, 4.500000000000000888 ) ) ;
#135540 = CARTESIAN_POINT ( 'NONE',  ( 24.77040314143521726, -7.934999999999989839, 2.126176841940957907 ) ) ;
#135541 = CARTESIAN_POINT ( 'NONE',  ( 2.020403141435219485, 7.934999999999988951, -2.126176841940961904 ) ) ;
#135542 = CARTESIAN_POINT ( 'NONE',  ( 23.16170612452605226, -6.740707523384209310, 16.75550250614872638 ) ) ;
#135543 = ADVANCED_FACE ( 'NONE', ( #128787 ), #89703, .T. ) ;
#135544 = DIRECTION ( 'NONE',  ( 0.7071067811865487940, 0.7071067811865463515, -0.000000000000000000 ) ) ;
#135545 = FACE_OUTER_BOUND ( 'NONE', #139410, .T. ) ;
#135546 = ORIENTED_EDGE ( 'NONE', *, *, #119335, .T. ) ;
#135547 =( BOUNDED_CURVE ( )  B_SPLINE_CURVE ( 3, ( #113161, #23288, #67567, #12426 ),
 .UNSPECIFIED., .F., .F. ) 
 B_SPLINE_CURVE_WITH_KNOTS ( ( 4, 4 ),
 ( 2.972453342939735066, 3.211474374380906660 ),
 .UNSPECIFIED. ) 
 CURVE ( )  GEOMETRIC_REPRESENTATION_ITEM ( )  RATIONAL_B_SPLINE_CURVE ( ( 1.000000000000000000, 0.9952447427727517670, 0.9952447427727517670, 1.000000000000000000 ) ) 
 REPRESENTATION_ITEM ( '' )  );
#135548 = ORIENTED_EDGE ( 'NONE', *, *, #53151, .F. ) ;
#135549 = CARTESIAN_POINT ( 'NONE',  ( 88.64583333333334281, 2.130196079827431976, -7.949999999999999289 ) ) ;
#135550 = VERTEX_POINT ( 'NONE', #118619 ) ;
#135551 = VECTOR ( 'NONE', #81888, 1000.000000000000227 ) ;
#135552 = ORIENTED_EDGE ( 'NONE', *, *, #107002, .T. ) ;
#135553 = ORIENTED_EDGE ( 'NONE', *, *, #69080, .T. ) ;
#135554 = DIRECTION ( 'NONE',  ( 0.000000000000000000, -1.000000000000000000, 0.000000000000000000 ) ) ;
#135555 = CARTESIAN_POINT ( 'NONE',  ( -8.700255128608413102, -27.71228299555199825, 4.000000000000000000 ) ) ;
#135556 = CARTESIAN_POINT ( 'NONE',  ( 10.61825861377528035, 8.432637487761462936, 4.375000000000001776 ) ) ;
#135557 = ORIENTED_EDGE ( 'NONE', *, *, #86931, .T. ) ;
#135558 = CARTESIAN_POINT ( 'NONE',  ( 16.60343192894632480, -14.24070752338413293, 19.24067776001729513 ) ) ;
#135559 = DIRECTION ( 'NONE',  ( -0.7071067811865487940, 0.7071067811865463515, -0.000000000000000000 ) ) ;
#135560 = FACE_OUTER_BOUND ( 'NONE', #68448, .T. ) ;
#135561 = CARTESIAN_POINT ( 'NONE',  ( 126.4161154897344943, 7.034615505666292457, -0.2322217439817755857 ) ) ;
#135562 = LINE ( 'NONE', #100777, #74299 ) ;
#135563 = FACE_OUTER_BOUND ( 'NONE', #29323, .T. ) ;
#135564 = CARTESIAN_POINT ( 'NONE',  ( -27.64318742751720848, -20.24070752338407786, 21.22881796311206770 ) ) ;
#135565 = CARTESIAN_POINT ( 'NONE',  ( 34.75611968250419181, 14.81293425470724046, 4.955485411084880276 ) ) ;
#135566 = CARTESIAN_POINT ( 'NONE',  ( 27.00000000000000711, 5.307397310025502080, 4.669168585031851393 ) ) ;
#135567 = DIRECTION ( 'NONE',  ( 0.000000000000000000, 1.000000000000000000, -0.000000000000000000 ) ) ;
#135568 = CARTESIAN_POINT ( 'NONE',  ( 33.48921356237309510, -27.52281430457078670, 5.000000000000000000 ) ) ;
#135569 = DIRECTION ( 'NONE',  ( 0.7071067811865486830, -0.7071067811865464625, -0.000000000000000000 ) ) ;
#135570 = CIRCLE ( 'NONE', #110068, 1.749999999999999778 ) ;
#135571 = DIRECTION ( 'NONE',  ( -0.7071067811865486830, 0.7071067811865464625, 0.000000000000000000 ) ) ;
#135572 = EDGE_CURVE ( 'NONE', #51152, #48040, #75163, .T. ) ;
#135573 = EDGE_CURVE ( 'NONE', #44042, #114197, #130959, .T. ) ;
#135574 = VERTEX_POINT ( 'NONE', #9859 ) ;
#135575 = ORIENTED_EDGE ( 'NONE', *, *, #138109, .T. ) ;
#135576 = AXIS2_PLACEMENT_3D ( 'NONE', #29799, #30544, #74776 ) ;
#135577 = CARTESIAN_POINT ( 'NONE',  ( 114.4795968585647614, 6.109999999999999432, 1.637169565754164280 ) ) ;
#135578 = ORIENTED_EDGE ( 'NONE', *, *, #118971, .T. ) ;
#135579 = CIRCLE ( 'NONE', #8229, 2.500000000000000444 ) ;
#135580 = DIRECTION ( 'NONE',  ( 0.7071067811865486830, -0.7071067811865463515, 0.000000000000000000 ) ) ;
#135581 = MECHANICAL_DESIGN_GEOMETRIC_PRESENTATION_REPRESENTATION (  '', ( #128632 ), #29076 ) ;
#135582 = CARTESIAN_POINT ( 'NONE',  ( -29.51783344222318206, 22.22500000000000142, 7.048977539241911394 ) ) ;
#135583 = ADVANCED_FACE ( 'NONE', ( #53369 ), #31632, .F. ) ;
#135584 = CARTESIAN_POINT ( 'NONE',  ( 25.39999999999999858, -2.600000000000060929, 28.92500000000001492 ) ) ;
#135585 = LINE ( 'NONE', #14498, #4860 ) ;
#135586 = CARTESIAN_POINT ( 'NONE',  ( 109.1412635252314374, 4.472830434245836706, 4.472830434245840259 ) ) ;
#135587 = ORIENTED_EDGE ( 'NONE', *, *, #111250, .T. ) ;
#135588 = ORIENTED_EDGE ( 'NONE', *, *, #97333, .T. ) ;
#135589 = DIRECTION ( 'NONE',  ( -0.6830127018922180770, -0.6830127018922204085, -0.2588190451025213501 ) ) ;
#135590 = CARTESIAN_POINT ( 'NONE',  ( -34.00193056682073944, -22.22500000000000142, 4.500000000000000888 ) ) ;
#135591 = EDGE_LOOP ( 'NONE', ( #127224, #121705, #18220, #63502 ) ) ;
#135592 = ORIENTED_EDGE ( 'NONE', *, *, #108429, .T. ) ;
#135593 = ORIENTED_EDGE ( 'NONE', *, *, #5900, .T. ) ;
#135594 = CARTESIAN_POINT ( 'NONE',  ( 2.999999999999988898, 8.966399257802175171, 5.000000000000000000 ) ) ;
#135595 = DIRECTION ( 'NONE',  ( 0.6830127018922180770, -0.6830127018922204085, -0.2588190451025213501 ) ) ;
#135596 = CARTESIAN_POINT ( 'NONE',  ( 29.22459685856478018, -1.637169565754160949, 6.109999999999997655 ) ) ;
#135597 = ORIENTED_EDGE ( 'NONE', *, *, #22242, .F. ) ;
#135598 = VERTEX_POINT ( 'NONE', #140380 ) ;
#135599 = CARTESIAN_POINT ( 'NONE',  ( -34.92500000000001137, 22.22500000000000142, 4.000000000000000000 ) ) ;
#135600 = EDGE_LOOP ( 'NONE', ( #54764, #37026, #14620, #65023 ) ) ;
#135601 = EDGE_LOOP ( 'NONE', ( #86663, #18102, #100262, #60844 ) ) ;
#135602 = PLANE ( 'NONE',  #772 ) ;
#135603 = DIRECTION ( 'NONE',  ( 0.7071067811865487940, -0.7071067811865463515, -0.000000000000000000 ) ) ;
#135604 = CARTESIAN_POINT ( 'NONE',  ( 78.82919371712957002, -3.975000000000001865, 6.884901960086284411 ) ) ;
#135605 = ORIENTED_EDGE ( 'NONE', *, *, #27646, .F. ) ;
#135606 = DIRECTION ( 'NONE',  ( 0.7071067811865486830, -0.7071067811865464625, -0.000000000000000000 ) ) ;
#135607 = CARTESIAN_POINT ( 'NONE',  ( 51.18398860626899705, 28.73617430169823095, 5.000000000000000000 ) ) ;
#135608 = FACE_OUTER_BOUND ( 'NONE', #22899, .T. ) ;
#135609 = DIRECTION ( 'NONE',  ( -0.6830127018922181881, 0.6830127018922202975, -0.2588190451025214056 ) ) ;
#135610 = EDGE_CURVE ( 'NONE', #82851, #3366, #20732, .T. ) ;
#135611 = FACE_BOUND ( 'NONE', #95836, .T. ) ;
#135612 = VERTEX_POINT ( 'NONE', #41070 ) ;
#135613 = DIRECTION ( 'NONE',  ( 0.7071067811865487940, 0.7071067811865463515, 0.000000000000000000 ) ) ;
#135614 = EDGE_CURVE ( 'NONE', #30612, #27690, #131661, .T. ) ;
#135615 = CARTESIAN_POINT ( 'NONE',  ( 24.18500016416798459, 22.22500000000000142, -17.39898871004312042 ) ) ;
#135616 = LINE ( 'NONE', #105115, #63094 ) ;
#135617 = ORIENTED_EDGE ( 'NONE', *, *, #102397, .T. ) ;
#135618 = CARTESIAN_POINT ( 'NONE',  ( 16.49999999999988987, 18.43112307739199451, 4.000000000000000000 ) ) ;
#135619 = VERTEX_POINT ( 'NONE', #42531 ) ;
#135620 = ORIENTED_EDGE ( 'NONE', *, *, #24812, .T. ) ;
#135621 = ORIENTED_EDGE ( 'NONE', *, *, #131313, .T. ) ;
#135622 = EDGE_CURVE ( 'NONE', #134021, #48818, #29467, .T. ) ;
#135623 = EDGE_CURVE ( 'NONE', #67893, #135518, #32345, .T. ) ;
#135624 = CIRCLE ( 'NONE', #29134, 5.968999999999998529 ) ;
#135625 = CARTESIAN_POINT ( 'NONE',  ( 39.72459685856477307, -1.637169565754160949, 6.109999999999997655 ) ) ;
#135626 = ORIENTED_EDGE ( 'NONE', *, *, #25026, .F. ) ;
#135627 = LINE ( 'NONE', #45787, #23233 ) ;
#135628 = AXIS2_PLACEMENT_3D ( 'NONE', #9678, #140219, #86560 ) ;
#135629 = LINE ( 'NONE', #79137, #91418 ) ;
#135630 = EDGE_CURVE ( 'NONE', #72508, #42487, #71601, .T. ) ;
#135631 = VERTEX_POINT ( 'NONE', #107736 ) ;
#135632 = DIRECTION ( 'NONE',  ( -0.7071067811865487940, 0.7071067811865463515, -0.000000000000000000 ) ) ;
#135633 = CARTESIAN_POINT ( 'NONE',  ( 0.000000000000000000, 1.465179874765178344E-16, 1.142820323027524232 ) ) ;
#135634 = EDGE_CURVE ( 'NONE', #73177, #32784, #62125, .T. ) ;
#135635 = CARTESIAN_POINT ( 'NONE',  ( -4.828169399223495084, -11.24070752338417201, 4.000000000000000000 ) ) ;
#135636 = LINE ( 'NONE', #124746, #143523 ) ;
#135637 = LINE ( 'NONE', #15937, #18139 ) ;
#135638 = CARTESIAN_POINT ( 'NONE',  ( 42.29974487139158157, -27.71228299555235708, 4.000000000000000000 ) ) ;
#135639 = ORIENTED_EDGE ( 'NONE', *, *, #58465, .F. ) ;
#135640 = ORIENTED_EDGE ( 'NONE', *, *, #84683, .T. ) ;
#135641 = VERTEX_POINT ( 'NONE', #19319 ) ;
#135642 = ORIENTED_EDGE ( 'NONE', *, *, #143322, .F. ) ;
#135643 = CARTESIAN_POINT ( 'NONE',  ( 26.99999999999980815, 19.93112307739197675, 4.000000000000000000 ) ) ;
#135644 = EDGE_CURVE ( 'NONE', #84525, #79859, #139704, .T. ) ;
#135645 = ORIENTED_EDGE ( 'NONE', *, *, #57872, .F. ) ;
#135646 = VERTEX_POINT ( 'NONE', #97580 ) ;
#135647 = CARTESIAN_POINT ( 'NONE',  ( 22.85159235450332105, 9.902892378096218942E-16, 0.000000000000000000 ) ) ;
#135648 = LINE ( 'NONE', #60988, #97190 ) ;
#135649 = ORIENTED_EDGE ( 'NONE', *, *, #105617, .T. ) ;
#135650 = DIRECTION ( 'NONE',  ( 1.000000000000000000, 1.224606353822377258E-16, 0.000000000000000000 ) ) ;
#135651 = ADVANCED_FACE ( 'NONE', ( #40386 ), #8397, .T. ) ;
#135652 = VERTEX_POINT ( 'NONE', #88158 ) ;
#135653 = CIRCLE ( 'NONE', #26875, 2.500000000000000888 ) ;
#135654 = CARTESIAN_POINT ( 'NONE',  ( 66.18398860626901126, 28.73617430169833753, 5.000000000000000000 ) ) ;
#135655 = CARTESIAN_POINT ( 'NONE',  ( 25.87956980810188767, 3.967499999999998916, 6.871911579029510442 ) ) ;
#135656 = STYLED_ITEM ( 'NONE', ( #71951 ), #108794 ) ;
#135657 = PRESENTATION_STYLE_ASSIGNMENT (( #83423 ) ) ;
#135658 = ORIENTED_EDGE ( 'NONE', *, *, #23566, .T. ) ;
#135660 = DIRECTION ( 'NONE',  ( 0.7071067811865486830, -0.7071067811865464625, -0.000000000000000000 ) ) ;
#135659 = CARTESIAN_POINT ( 'NONE',  ( 111.9120968585647944, 5.291415217122922066, -3.054999999999995275 ) ) ;
#135661 = VECTOR ( 'NONE', #121903, 1000.000000000000000 ) ;
#135662 = VECTOR ( 'NONE', #93653, 1000.000000000000000 ) ;
#135663 = LINE ( 'NONE', #26187, #122771 ) ;
#135664 = PLANE ( 'NONE',  #55735 ) ;
#135665 = ADVANCED_FACE ( 'NONE', ( #35222 ), #55532, .F. ) ;
#135666 = ORIENTED_EDGE ( 'NONE', *, *, #11243, .T. ) ;
#135667 = DIRECTION ( 'NONE',  ( -0.7071067811865486830, 0.7071067811865464625, 0.000000000000000000 ) ) ;
#135668 = VERTEX_POINT ( 'NONE', #2532 ) ;
#135669 = DIRECTION ( 'NONE',  ( -1.000000000000000000, -1.224606353822377258E-16, -0.000000000000000000 ) ) ;
#135670 = CARTESIAN_POINT ( 'NONE',  ( -39.18398860626899705, 28.73617430169814568, 5.000000000000000000 ) ) ;
#135671 = AXIS2_PLACEMENT_3D ( 'NONE', #66019, #10856, #55123 ) ;
#135672 = PRESENTATION_STYLE_ASSIGNMENT (( #61009 ) ) ;
#135673 = CARTESIAN_POINT ( 'NONE',  ( 0.000000000000000000, 21.72500000000000142, 4.500000000000000888 ) ) ;
#135674 = CARTESIAN_POINT ( 'NONE',  ( -34.92500000000001137, 22.22500000000000142, 4.000000000000000000 ) ) ;
#135675 = ORIENTED_EDGE ( 'NONE', *, *, #29172, .T. ) ;
#135676 = EDGE_CURVE ( 'NONE', #91343, #139204, #1111, .T. ) ;
#135677 = ADVANCED_FACE ( 'NONE', ( #35937 ), #132407, .T. ) ;
#135678 = DIRECTION ( 'NONE',  ( -0.000000000000000000, -0.000000000000000000, 1.000000000000000000 ) ) ;
#135679 = CARTESIAN_POINT ( 'NONE',  ( 12.08840764549667668, 9.139736423841732040E-16, 0.000000000000000000 ) ) ;
#135680 = VERTEX_POINT ( 'NONE', #67116 ) ;
#135681 = DIRECTION ( 'NONE',  ( -0.000000000000000000, 0.3543493200069153248, 0.9351131265310292928 ) ) ;
#135683 = ADVANCED_FACE ( 'NONE', ( #101152 ), #44691, .T. ) ;
#135682 = CARTESIAN_POINT ( 'NONE',  ( -39.48921356237310221, -27.52281430457082934, 5.000000000000000000 ) ) ;
#135684 = ORIENTED_EDGE ( 'NONE', *, *, #100811, .F. ) ;
#135686 = ORIENTED_EDGE ( 'NONE', *, *, #29011, .F. ) ;
#135685 = PLANE ( 'NONE',  #16264 ) ;
#135687 = ORIENTED_EDGE ( 'NONE', *, *, #116842, .F. ) ;
#135688 = PLANE ( 'NONE',  #79716 ) ;
#135689 = DIRECTION ( 'NONE',  ( -0.7071067811865486830, -0.7071067811865464625, 0.000000000000000000 ) ) ;
#135690 = ORIENTED_EDGE ( 'NONE', *, *, #11070, .F. ) ;
#135691 = DIRECTION ( 'NONE',  ( 0.7071067811865486830, -0.7071067811865464625, -0.000000000000000000 ) ) ;
#135692 = LINE ( 'NONE', #124097, #9016 ) ;
#135693 =( BOUNDED_CURVE ( )  B_SPLINE_CURVE ( 2, ( #8836, #74903, #53093, #107490, #119768, #20466, #108170, #63320, #42265, #8154, #141565, #86476, #130706 ),
 .UNSPECIFIED., .F., .T. ) 
 B_SPLINE_CURVE_WITH_KNOTS ( ( 3, 2, 2, 2, 2, 2, 3 ),
 ( 0.1000000000000000333, 0.1083333333333333648, 0.1166666666666666963, 0.1250000000000000278, 0.1333333333333333592, 0.1416666666666666907, 0.1500000000000000222 ),
 .UNSPECIFIED. ) 
 CURVE ( )  GEOMETRIC_REPRESENTATION_ITEM ( )  RATIONAL_B_SPLINE_CURVE ( ( 0.9999999999999998890, 0.9659258262890684232, 1.000000000000000000, 0.9659258262890683122, 1.000000000000000000, 0.9659258262890683122, 1.000000000000000000, 0.9659258262890683122, 1.000000000000000000, 0.9659258262890683122, 1.000000000000000000, 0.9659258262890682012, 1.000000000000000222 ) ) 
 REPRESENTATION_ITEM ( '' )  );
#135694 = ORIENTED_EDGE ( 'NONE', *, *, #19445, .F. ) ;
#135695 = EDGE_CURVE ( 'NONE', #104041, #23176, #86430, .T. ) ;
#135696 = CARTESIAN_POINT ( 'NONE',  ( -3.299744871391591339, -27.71228299555208352, 4.000000000000000000 ) ) ;
#135697 = CARTESIAN_POINT ( 'NONE',  ( 3.707106781186514599, -9.740707523384186217, 5.000000000000000000 ) ) ;
#135698 = LINE ( 'NONE', #124812, #33222 ) ;
#135700 = VECTOR ( 'NONE', #10535, 1000.000000000000000 ) ;
#135699 = CARTESIAN_POINT ( 'NONE',  ( 0.000000000000000000, 0.000000000000000000, 5.000000000000000000 ) ) ;
#135701 = CARTESIAN_POINT ( 'NONE',  ( -39.18398860626899705, 28.73617430169814568, 5.000000000000000000 ) ) ;
#135702 = ADVANCED_FACE ( 'NONE', ( #56977 ), #77308, .F. ) ;
#135703 = DIRECTION ( 'NONE',  ( 0.7071067811865487940, 0.7071067811865463515, 0.000000000000000000 ) ) ;
#135704 = CARTESIAN_POINT ( 'NONE',  ( -9.328169399223465774, 17.25929247661554555, 4.000000000000000000 ) ) ;
#135705 = VERTEX_POINT ( 'NONE', #396 ) ;
#135706 = ORIENTED_EDGE ( 'NONE', *, *, #53385, .F. ) ;
#135707 = ORIENTED_EDGE ( 'NONE', *, *, #1244, .F. ) ;
#135708 = CARTESIAN_POINT ( 'NONE',  ( 118.8333333333333286, -6.884901960086287964, 3.974999999999998312 ) ) ;
#135709 = ORIENTED_EDGE ( 'NONE', *, *, #19337, .T. ) ;
#135710 = ORIENTED_EDGE ( 'NONE', *, *, #38464, .F. ) ;
#135711 = ORIENTED_EDGE ( 'NONE', *, *, #130264, .T. ) ;
#135712 = CARTESIAN_POINT ( 'NONE',  ( 0.5689546957196583987, -7.499959106704563006, -0.6961060096647321283 ) ) ;
#135713 = DIRECTION ( 'NONE',  ( -1.000000000000000000, -1.224606353822377258E-16, -0.000000000000000000 ) ) ;
#135714 = ORIENTED_EDGE ( 'NONE', *, *, #19423, .F. ) ;
#135715 = FACE_OUTER_BOUND ( 'NONE', #73821, .T. ) ;
#135716 = CARTESIAN_POINT ( 'NONE',  ( 17.81601139373099940, 28.73617430169775133, 5.000000000000000000 ) ) ;
#135717 = DIRECTION ( 'NONE',  ( -0.7071067811865486830, 0.7071067811865464625, 0.000000000000000000 ) ) ;
#135718 = CARTESIAN_POINT ( 'NONE',  ( -19.49999999999986500, -10.91253812416064406, 4.000000000000000000 ) ) ;
#135719 = CARTESIAN_POINT ( 'NONE',  ( 114.4795968585647614, 6.109999999999999432, 1.637169565754164280 ) ) ;
#135720 = EDGE_LOOP ( 'NONE', ( #46725, #104127, #39005, #44346 ) ) ;
#135721 = DIRECTION ( 'NONE',  ( 0.7071067811865487940, 0.7071067811865463515, 0.000000000000000000 ) ) ;
#135722 = CARTESIAN_POINT ( 'NONE',  ( 36.29974487139159578, -27.71228299555231445, 4.000000000000000000 ) ) ;
#135723 = CARTESIAN_POINT ( 'NONE',  ( 15.18398860626900237, 28.73617430169797871, 5.000000000000000000 ) ) ;
#135724 = CARTESIAN_POINT ( 'NONE',  ( 0.8668240023198436894, 6.544601550655485767, 3.096248083358116965 ) ) ;
#135725 = DIRECTION ( 'NONE',  ( -0.6830127018922180770, -0.6830127018922204085, -0.2588190451025213501 ) ) ;
#135726 =( BOUNDED_CURVE ( )  B_SPLINE_CURVE ( 2, ( #18047, #75348, #52836, #62337, #84779, #107233, #130443, #119510, #41258, #64452, #25763, #113475, #125078 ),
 .UNSPECIFIED., .F., .T. ) 
 B_SPLINE_CURVE_WITH_KNOTS ( ( 3, 2, 2, 2, 2, 2, 3 ),
 ( 0.5000000000000000000, 0.5083333333333333037, 0.5166666666666667185, 0.5250000000000001332, 0.5333333333333334370, 0.5416666666666667407, 0.5500000000000001554 ),
 .UNSPECIFIED. ) 
 CURVE ( )  GEOMETRIC_REPRESENTATION_ITEM ( )  RATIONAL_B_SPLINE_CURVE ( ( 1.000000000000000000, 0.9659258262890683122, 1.000000000000000000, 0.9659258262890683122, 1.000000000000000000, 0.9659258262890683122, 1.000000000000000000, 0.9659258262890683122, 1.000000000000000000, 0.9659258262890683122, 1.000000000000000000, 0.9659258262890678681, 1.000000000000000444 ) ) 
 REPRESENTATION_ITEM ( '' )  );
#135727 = CARTESIAN_POINT ( 'NONE',  ( -7.499999999999947597, 18.43112307739200162, 4.000000000000000000 ) ) ;
#135728 = LINE ( 'NONE', #14657, #82861 ) ;
#135729 = CARTESIAN_POINT ( 'NONE',  ( 48.05836038379621300, -7.949999999999997513, -2.130196079827425759 ) ) ;
#135730 = AXIS2_PLACEMENT_3D ( 'NONE', #38102, #5425, #49705 ) ;
#135731 = DIRECTION ( 'NONE',  ( 0.7071067811865487940, 0.7071067811865463515, 0.000000000000000000 ) ) ;
#135732 = ADVANCED_FACE ( 'NONE', ( #23598 ), #11993, .T. ) ;
#135733 = DIRECTION ( 'NONE',  ( 0.7071067811865487940, 0.7071067811865463515, -0.000000000000000000 ) ) ;
#135734 = VERTEX_POINT ( 'NONE', #121477 ) ;
#135735 = EDGE_LOOP ( 'NONE', ( #107843, #123425, #105700, #86969 ) ) ;
#135736 = CARTESIAN_POINT ( 'NONE',  ( 34.83333333333332860, -6.884901960086287964, 3.974999999999998312 ) ) ;
#135737 = ORIENTED_EDGE ( 'NONE', *, *, #88840, .F. ) ;
#135738 = AXIS2_PLACEMENT_3D ( 'NONE', #70890, #38244, #73714 ) ;
#135739 = ORIENTED_EDGE ( 'NONE', *, *, #26944, .T. ) ;
#135740 = CARTESIAN_POINT ( 'NONE',  ( 9.707106781186482181, 8.259292476615627265, 5.000000000000000000 ) ) ;
#135741 = DIRECTION ( 'NONE',  ( 0.7071067811865486830, -0.7071067811865464625, -0.000000000000000000 ) ) ;
#135742 = VERTEX_POINT ( 'NONE', #65730 ) ;
#135743 = DIRECTION ( 'NONE',  ( 0.6830127018922181881, 0.6830127018922202975, -0.2588190451025214056 ) ) ;
#135744 = CARTESIAN_POINT ( 'NONE',  ( 1.042387978378689350, 0.4000000000000001332, -2.015694669338588429 ) ) ;
#135745 = EDGE_CURVE ( 'NONE', #7189, #21579, #88884, .T. ) ;
#135746 = CARTESIAN_POINT ( 'NONE',  ( 39.95876352523143282, 0.000000000000000000, -6.110000000000001208 ) ) ;
#135748 = ORIENTED_EDGE ( 'NONE', *, *, #134052, .F. ) ;
#135747 = VECTOR ( 'NONE', #133749, 1000.000000000000000 ) ;
#135749 = DIRECTION ( 'NONE',  ( -0.7071067811865486830, -0.7071067811865464625, 0.000000000000000000 ) ) ;
#135750 = EDGE_LOOP ( 'NONE', ( #51201, #61174, #44380, #78887 ) ) ;
#135751 = DIRECTION ( 'NONE',  ( -1.000000000000000000, -1.224606353822377258E-16, -0.000000000000000000 ) ) ;
#135752 = DIRECTION ( 'NONE',  ( -0.7071067811865486830, -0.7071067811865464625, -0.000000000000000000 ) ) ;
#135753 = DIRECTION ( 'NONE',  ( -0.6830127018922180770, -0.6830127018922204085, -0.2588190451025213501 ) ) ;
#135754 = DIRECTION ( 'NONE',  ( 0.000000000000000000, 0.000000000000000000, 1.000000000000000000 ) ) ;
#135755 = ORIENTED_EDGE ( 'NONE', *, *, #65647, .T. ) ;
#135756 = VECTOR ( 'NONE', #85271, 1000.000000000000227 ) ;
#135757 = ADVANCED_FACE ( 'NONE', ( #133111 ), #68562, .T. ) ;
#135758 = ORIENTED_EDGE ( 'NONE', *, *, #11063, .F. ) ;
#135759 = CARTESIAN_POINT ( 'NONE',  ( 39.74586038379622721, 3.974999999999996980, 6.884901960086287964 ) ) ;
#135760 = LINE ( 'NONE', #47377, #127261 ) ;
#135761 = LINE ( 'NONE', #39314, #121961 ) ;
#135762 = CARTESIAN_POINT ( 'NONE',  ( -27.18398860626900060, 28.73617430169806042, 5.000000000000000000 ) ) ;
#135763 = PRESENTATION_LAYER_ASSIGNMENT (  '', '', ( #100976 ) ) ;
#135764 = AXIS2_PLACEMENT_3D ( 'NONE', #105425, #3933, #127183 ) ;
#135765 = AXIS2_PLACEMENT_3D ( 'NONE', #116667, #81949, #61613 ) ;
#135766 = CARTESIAN_POINT ( 'NONE',  ( 59.12043019189810877, 3.055000000000001936, -5.291415217122916737 ) ) ;
#135767 = PLANE ( 'NONE',  #53440 ) ;
#135768 = LINE ( 'NONE', #114007, #3767 ) ;
#135769 = VERTEX_POINT ( 'NONE', #33789 ) ;
#135770 = ORIENTED_EDGE ( 'NONE', *, *, #136620, .T. ) ;
#135771 = CARTESIAN_POINT ( 'NONE',  ( -34.42500000000001137, 0.000000000000000000, 4.500000000000000888 ) ) ;
#135772 = ORIENTED_EDGE ( 'NONE', *, *, #61525, .T. ) ;
#135773 = CARTESIAN_POINT ( 'NONE',  ( 34.49999999999975131, -1.912538124160733766, 4.000000000000000000 ) ) ;
#135774 = PRODUCT_DEFINITION_CONTEXT ( 'detailed design', #57807, 'design' ) ;
#135775 = ORIENTED_EDGE ( 'NONE', *, *, #15479, .F. ) ;
#135776 = CARTESIAN_POINT ( 'NONE',  ( 26.67183060077628554, -18.74070752338408852, 4.000000000000000000 ) ) ;
#135777 = EDGE_CURVE ( 'NONE', #74246, #27583, #112749, .T. ) ;
#135778 = DIRECTION ( 'NONE',  ( 0.7071067811865486830, -0.7071067811865464625, -0.000000000000000000 ) ) ;
#135779 = CARTESIAN_POINT ( 'NONE',  ( 30.29974487139158867, -27.71228299555227537, 4.000000000000000000 ) ) ;
#135780 = FACE_BOUND ( 'NONE', #130797, .T. ) ;
#135781 = LINE ( 'NONE', #48783, #115078 ) ;
#135782 = EDGE_CURVE ( 'NONE', #54290, #75139, #76258, .T. ) ;
#135783 = ADVANCED_FACE ( 'NONE', ( #103282 ), #27157, .F. ) ;
#135784 = CARTESIAN_POINT ( 'NONE',  ( 1.734723475976807094E-15, 7.552185695429095347, 5.000000000000000000 ) ) ;
#135785 = CARTESIAN_POINT ( 'NONE',  ( -15.48921356237309510, -27.52281430457066236, 5.000000000000000000 ) ) ;
#135787 = ORIENTED_EDGE ( 'NONE', *, *, #85932, .T. ) ;
#135786 = CYLINDRICAL_SURFACE ( 'NONE', #75925, 2.500000000000000000 ) ;
#135788 = LINE ( 'NONE', #13979, #42520 ) ;
#135789 = ORIENTED_EDGE ( 'NONE', *, *, #142426, .T. ) ;
#135790 = ADVANCED_FACE ( 'NONE', ( #94545 ), #126462, .F. ) ;
#135791 = ADVANCED_FACE ( 'NONE', ( #48939 ), #138805, .T. ) ;
#135792 = ORIENTED_EDGE ( 'NONE', *, *, #15546, .F. ) ;
#135793 = CARTESIAN_POINT ( 'NONE',  ( 63.05793019189810877, 6.110000000000000320, -1.637169565754156064 ) ) ;
#135794 = EDGE_LOOP ( 'NONE', ( #139564, #107738, #48290, #130860 ) ) ;
#135795 = EDGE_CURVE ( 'NONE', #59855, #19525, #70006, .T. ) ;
#135796 = LINE ( 'NONE', #3797, #118118 ) ;
#135797 = EDGE_CURVE ( 'NONE', #23925, #25963, #71399, .T. ) ;
#135798 = ORIENTED_EDGE ( 'NONE', *, *, #74247, .T. ) ;
#135799 = MECHANICAL_DESIGN_GEOMETRIC_PRESENTATION_REPRESENTATION (  '', ( #17696 ), #38732 ) ;
#135800 = ADVANCED_FACE ( 'NONE', ( #49670 ), #82287, .F. ) ;
#135801 = CARTESIAN_POINT ( 'NONE',  ( -24.48921356237309510, -27.52281430457072631, 5.000000000000000000 ) ) ;
#135802 = EDGE_CURVE ( 'NONE', #72918, #59821, #115558, .T. ) ;
#135803 = DIRECTION ( 'NONE',  ( -0.7071067811865486830, 0.7071067811865464625, 0.000000000000000000 ) ) ;
#135804 = LINE ( 'NONE', #55402, #143158 ) ;
#135806 = SURFACE_STYLE_FILL_AREA ( #57553 ) ;
#135805 = DIRECTION ( 'NONE',  ( -0.000000000000000000, -0.3543493200069152693, 0.9351131265310292928 ) ) ;
#135807 = CARTESIAN_POINT ( 'NONE',  ( 36.48921356237310221, -27.52281430457080802, 5.000000000000000000 ) ) ;
#135808 = CARTESIAN_POINT ( 'NONE',  ( 0.000000000000000000, 0.000000000000000000, 10.00000000000000000 ) ) ;
#135809 = VERTEX_POINT ( 'NONE', #47550 ) ;
#135810 = AXIS2_PLACEMENT_3D ( 'NONE', #20674, #31575, #10506 ) ;
#135811 = ORIENTED_EDGE ( 'NONE', *, *, #22966, .F. ) ;
#135812 = DIRECTION ( 'NONE',  ( 0.000000000000000000, -0.3543493200069152138, 0.9351131265310292928 ) ) ;
#135813 = FACE_OUTER_BOUND ( 'NONE', #141812, .T. ) ;
#135814 = ORIENTED_EDGE ( 'NONE', *, *, #130827, .F. ) ;
#135815 = ADVANCED_FACE ( 'NONE', ( #136630 ), #92403, .F. ) ;
#135816 = ORIENTED_EDGE ( 'NONE', *, *, #59479, .F. ) ;
#135817 = VERTEX_POINT ( 'NONE', #16248 ) ;
#135818 = DIRECTION ( 'NONE',  ( 0.7071067811865487940, 0.7071067811865463515, 0.000000000000000000 ) ) ;
#135819 = ORIENTED_EDGE ( 'NONE', *, *, #23716, .T. ) ;
#135820 = PLANE ( 'NONE',  #106468 ) ;
#135821 = EDGE_CURVE ( 'NONE', #49011, #92088, #101218, .T. ) ;
#135822 = AXIS2_PLACEMENT_3D ( 'NONE', #96535, #41466, #7399 ) ;
#135823 = CARTESIAN_POINT ( 'NONE',  ( -7.265066702820462297, 12.75929247661558996, 18.34774599283958096 ) ) ;
#135824 = CARTESIAN_POINT ( 'NONE',  ( -1.391263525231447584, -5.808823158059033709, 5.808823158059035485 ) ) ;
#135825 = CARTESIAN_POINT ( 'NONE',  ( 48.18398860626899705, 28.73617430169820608, 5.000000000000000000 ) ) ;
#135826 = VERTEX_POINT ( 'NONE', #25735 ) ;
#135827 = VECTOR ( 'NONE', #122936, 1000.000000000000000 ) ;
#135828 = CARTESIAN_POINT ( 'NONE',  ( -45.48921356237309510, -27.52281430457087197, 5.000000000000000000 ) ) ;
#135829 = DIRECTION ( 'NONE',  ( 0.7071067811865487940, 0.7071067811865463515, 0.000000000000000000 ) ) ;
#135831 = ORIENTED_EDGE ( 'NONE', *, *, #90256, .F. ) ;
#135830 = DIRECTION ( 'NONE',  ( 0.6830127018922181881, 0.6830127018922202975, -0.2588190451025214056 ) ) ;
#135832 = VERTEX_POINT ( 'NONE', #14136 ) ;
#135833 = CARTESIAN_POINT ( 'NONE',  ( -60.48921356237309510, -27.52281430457097500, 5.000000000000000000 ) ) ;
#135834 = CARTESIAN_POINT ( 'NONE',  ( 22.07159235450331991, -2.500000000000000444, 3.061616997868384620E-16 ) ) ;
#135835 = LINE ( 'NONE', #36521, #102647 ) ;
#135836 = EDGE_LOOP ( 'NONE', ( #12204, #9726, #31456, #138561 ) ) ;
#135837 = DIRECTION ( 'NONE',  ( -1.000000000000000000, -0.000000000000000000, -0.000000000000000000 ) ) ;
#135838 = EDGE_CURVE ( 'NONE', #46474, #77939, #58428, .T. ) ;
#135839 = CARTESIAN_POINT ( 'NONE',  ( 16.61159235450331906, -7.703719777548943412E-31, 2.500000000000001332 ) ) ;
#135840 = VECTOR ( 'NONE', #7737, 1000.000000000000000 ) ;
#135841 = EDGE_CURVE ( 'NONE', #26904, #117439, #59814, .T. ) ;
#135842 = DIRECTION ( 'NONE',  ( -0.6830127018922180770, -0.6830127018922204085, -0.2588190451025213501 ) ) ;
#135843 = CARTESIAN_POINT ( 'NONE',  ( -19.49999999999985789, -19.91253812416055524, 4.000000000000000000 ) ) ;
#135844 = CARTESIAN_POINT ( 'NONE',  ( 1.980122250714512422, -17.24070752338410273, 20.23474786156469918 ) ) ;
#135845 = EDGE_LOOP ( 'NONE', ( #10412, #80136, #57496, #61840 ) ) ;
#135846 = CARTESIAN_POINT ( 'NONE',  ( 11.99999999999992362, -3.033600742197707145, 5.000000000000000000 ) ) ;
#135847 = FACE_OUTER_BOUND ( 'NONE', #59600, .T. ) ;
#135848 = EDGE_CURVE ( 'NONE', #74997, #68687, #64046, .T. ) ;
#135849 = CARTESIAN_POINT ( 'NONE',  ( -54.18398860626899705, 28.73617430169825226, 5.000000000000000000 ) ) ;
#135850 = DIRECTION ( 'NONE',  ( -0.7071067811865487940, 0.7071067811865463515, -0.000000000000000000 ) ) ;
#135851 = AXIS2_PLACEMENT_3D ( 'NONE', #60549, #48210, #115559 ) ;
#135852 = DIRECTION ( 'NONE',  ( 0.3543493200069162685, -0.000000000000000000, -0.9351131265310288487 ) ) ;
#135853 = ORIENTED_EDGE ( 'NONE', *, *, #25652, .F. ) ;
#135854 = VERTEX_POINT ( 'NONE', #63407 ) ;
#135855 = CARTESIAN_POINT ( 'NONE',  ( -26.99999999999981526, -1.068876922607802538, 4.000000000000000000 ) ) ;
#135856 = CARTESIAN_POINT ( 'NONE',  ( 6.707106781186496391, -18.74070752338408852, 5.000000000000000000 ) ) ;
#135857 = CIRCLE ( 'NONE', #96491, 5.968999999999998529 ) ;
#135858 = AXIS2_PLACEMENT_3D ( 'NONE', #102265, #58069, #58802 ) ;
#135859 = CARTESIAN_POINT ( 'NONE',  ( 7.270403141435219041, -7.934999999999989839, 2.126176841940957907 ) ) ;
#135860 = DIRECTION ( 'NONE',  ( 0.7071067811865487940, 0.7071067811865463515, 0.000000000000000000 ) ) ;
#135861 = VECTOR ( 'NONE', #134680, 1000.000000000000227 ) ;
#135862 = DIRECTION ( 'NONE',  ( 0.6830127018922181881, 0.6830127018922202975, -0.2588190451025214056 ) ) ;
#135863 = LINE ( 'NONE', #90204, #39095 ) ;
#135864 = FACE_OUTER_BOUND ( 'NONE', #57149, .T. ) ;
#135865 = ORIENTED_EDGE ( 'NONE', *, *, #76566, .T. ) ;
#135866 = EDGE_CURVE ( 'NONE', #103352, #104775, #101068, .T. ) ;
#135867 = CARTESIAN_POINT ( 'NONE',  ( 68.99451991528748351, 28.92564299267986172, 4.000000000000000000 ) ) ;
#135868 = VECTOR ( 'NONE', #95076, 1000.000000000000000 ) ;
#135869 = DIRECTION ( 'NONE',  ( -0.6830127018922180770, -0.6830127018922204085, -0.2588190451025213501 ) ) ;
#135870 = CARTESIAN_POINT ( 'NONE',  ( 51.68293019189811588, -1.637169565754159173, -6.109999999999999432 ) ) ;
#135871 = CARTESIAN_POINT ( 'NONE',  ( -2.671830600776445852, 11.25929247661560240, 4.000000000000000000 ) ) ;
#135872 = CARTESIAN_POINT ( 'NONE',  ( 0.000000000000000000, 0.000000000000000000, 5.000000000000000000 ) ) ;
#135873 = EDGE_LOOP ( 'NONE', ( #26536, #129993, #131374, #55974 ) ) ;
#135874 = CARTESIAN_POINT ( 'NONE',  ( 23.96247294953710849, -7.464222240803106570E-16, -6.094999999999989981 ) ) ;
#135875 = ORIENTED_EDGE ( 'NONE', *, *, #135486, .F. ) ;
#135876 = DIRECTION ( 'NONE',  ( -0.7071067811865487940, 0.7071067811865463515, 0.000000000000000000 ) ) ;
#135877 = DIRECTION ( 'NONE',  ( -0.7071067811865487940, 0.7071067811865463515, 0.000000000000000000 ) ) ;
#135878 = PLANE ( 'NONE',  #28000 ) ;
#135879 = CARTESIAN_POINT ( 'NONE',  ( -57.29974487139158157, -27.71228299555246011, 4.000000000000000000 ) ) ;
#135880 = EDGE_CURVE ( 'NONE', #126258, #71524, #130897, .T. ) ;
#135881 = DIRECTION ( 'NONE',  ( -1.000000000000000000, 0.000000000000000000, 0.000000000000000000 ) ) ;
#135882 = CARTESIAN_POINT ( 'NONE',  ( 128.5894344200537489, -52.00875322212550600, 39.86617647058822911 ) ) ;
#135883 = VERTEX_POINT ( 'NONE', #7535 ) ;
#135884 = EDGE_CURVE ( 'NONE', #94958, #82809, #97390, .T. ) ;
#135885 = ORIENTED_EDGE ( 'NONE', *, *, #140199, .T. ) ;
#135886 = CARTESIAN_POINT ( 'NONE',  ( 34.92499999999998295, 0.7592924766157138627, 4.255531930566151644 ) ) ;
#135887 = CARTESIAN_POINT ( 'NONE',  ( -14.75830541574804222, 0.7592924766157138627, 14.37146558664986351 ) ) ;
#135888 = VECTOR ( 'NONE', #137434, 1000.000000000000000 ) ;
#135889 = DIRECTION ( 'NONE',  ( 1.000000000000000000, 0.000000000000000000, 0.000000000000000000 ) ) ;
#135890 = DIRECTION ( 'NONE',  ( -0.3543493200069162685, -0.000000000000000000, -0.9351131265310288487 ) ) ;
#135891 = CARTESIAN_POINT ( 'NONE',  ( 75.62086038379622721, -6.884901960086286188, 3.974999999999997424 ) ) ;
#135892 = EDGE_CURVE ( 'NONE', #53838, #72096, #86564, .T. ) ;
#135893 = VECTOR ( 'NONE', #72869, 1000.000000000000000 ) ;
#135894 = CARTESIAN_POINT ( 'NONE',  ( 26.99999999999981526, -0.4125381241607464222, 4.000000000000000000 ) ) ;
#135895 = ORIENTED_EDGE ( 'NONE', *, *, #118722, .F. ) ;
#135896 = CARTESIAN_POINT ( 'NONE',  ( 64.00000000000000000, 0.000000000000000000, -7.950000000000000178 ) ) ;
#135897 = LINE ( 'NONE', #58393, #134979 ) ;
#135898 = LINE ( 'NONE', #79432, #48542 ) ;
#135899 = LINE ( 'NONE', #113416, #84553 ) ;
#135900 = AXIS2_PLACEMENT_3D ( 'NONE', #14053, #47467, #33708 ) ;
#135901 = ORIENTED_EDGE ( 'NONE', *, *, #72676, .T. ) ;
#135902 = EDGE_CURVE ( 'NONE', #70329, #110682, #129320, .T. ) ;
#135903 = DIRECTION ( 'NONE',  ( 0.6830127018922180770, -0.6830127018922204085, -0.2588190451025213501 ) ) ;
#135904 = EDGE_CURVE ( 'NONE', #67554, #28495, #108984, .T. ) ;
#135905 = LINE ( 'NONE', #89540, #139361 ) ;
#135906 = CARTESIAN_POINT ( 'NONE',  ( 65.91709685856477563, 3.054999999999998828, 5.291415217122922066 ) ) ;
#135907 = CONICAL_SURFACE ( 'NONE', #103386, 2.055000000000000604, 0.9599310885968764806 ) ;
#135908 = FACE_OUTER_BOUND ( 'NONE', #45556, .T. ) ;
#135909 = ORIENTED_EDGE ( 'NONE', *, *, #12967, .F. ) ;
#135910 = ORIENTED_EDGE ( 'NONE', *, *, #10969, .F. ) ;
#135911 = DIRECTION ( 'NONE',  ( -0.6830127018922181881, 0.6830127018922202975, -0.2588190451025214056 ) ) ;
#135912 = LINE ( 'NONE', #91688, #81435 ) ;
#135913 = AXIS2_PLACEMENT_3D ( 'NONE', #110952, #100124, #67517 ) ;
#135914 = DIRECTION ( 'NONE',  ( -1.000000000000000000, -1.224606353822377258E-16, -0.000000000000000000 ) ) ;
#135915 = EDGE_CURVE ( 'NONE', #38500, #61103, #18396, .T. ) ;
#135916 = LINE ( 'NONE', #101134, #88166 ) ;
#135918 = EDGE_LOOP ( 'NONE', ( #84121, #7586, #41708 ) ) ;
#135917 = DIRECTION ( 'NONE',  ( 0.7071067811865487940, 0.7071067811865463515, 0.000000000000000000 ) ) ;
#135919 = DIRECTION ( 'NONE',  ( 0.6830127018922181881, 0.6830127018922202975, -0.2588190451025214056 ) ) ;
#135920 = FACE_OUTER_BOUND ( 'NONE', #16216, .T. ) ;
#135921 = CARTESIAN_POINT ( 'NONE',  ( 17.54840764549667398, 9.139736423841732040E-16, 0.000000000000000000 ) ) ;
#135922 = EDGE_LOOP ( 'NONE', ( #135341, #42121, #6051, #33889 ) ) ;
#135923 = VERTEX_POINT ( 'NONE', #28618 ) ;
#135924 = VECTOR ( 'NONE', #134368, 1000.000000000000000 ) ;
#135925 = DIRECTION ( 'NONE',  ( 1.000000000000000000, 0.000000000000000000, 0.000000000000000000 ) ) ;
#135926 = DIRECTION ( 'NONE',  ( -0.000000000000000000, -1.000000000000000000, 0.000000000000000000 ) ) ;
#135927 = CARTESIAN_POINT ( 'NONE',  ( 42.29974487139158157, -27.71228299555235708, 4.000000000000000000 ) ) ;
#135928 = B_SPLINE_CURVE_WITH_KNOTS ( 'NONE', 3,
 ( #139853, #28216, #54796, #84727 ),
 .UNSPECIFIED., .F., .F.,
 ( 4, 4 ),
 ( 0.000000000000000000, 0.001824211539880441196 ),
 .UNSPECIFIED. ) ;
#135929 = DIRECTION ( 'NONE',  ( -1.000000000000000000, -0.000000000000000000, -0.000000000000000000 ) ) ;
#135930 = FACE_OUTER_BOUND ( 'NONE', #122944, .T. ) ;
#135931 = ORIENTED_EDGE ( 'NONE', *, *, #140388, .F. ) ;
#135932 = ORIENTED_EDGE ( 'NONE', *, *, #71435, .T. ) ;
#135933 = FACE_OUTER_BOUND ( 'NONE', #76446, .T. ) ;
#135934 = ORIENTED_EDGE ( 'NONE', *, *, #107749, .T. ) ;
#135935 = DIRECTION ( 'NONE',  ( -0.3543493200069162685, -0.000000000000000000, -0.9351131265310288487 ) ) ;
#135936 = ORIENTED_EDGE ( 'NONE', *, *, #94098, .F. ) ;
#135937 = FACE_OUTER_BOUND ( 'NONE', #116647, .T. ) ;
#135938 = LINE ( 'NONE', #101162, #102589 ) ;
#135939 = EDGE_LOOP ( 'NONE', ( #45978, #6274, #73108, #61914 ) ) ;
#135940 = VECTOR ( 'NONE', #52826, 1000.000000000000227 ) ;
#135941 = FACE_BOUND ( 'NONE', #52331, .T. ) ;
#135942 = DIRECTION ( 'NONE',  ( -0.000000000000000000, -0.3543493200069152693, 0.9351131265310292928 ) ) ;
#135943 = EDGE_CURVE ( 'NONE', #126702, #6455, #62666, .T. ) ;
#135944 = DIRECTION ( 'NONE',  ( 0.7071067811865486830, -0.7071067811865464625, -0.000000000000000000 ) ) ;
#135945 = LINE ( 'NONE', #45407, #85313 ) ;
#135946 = CARTESIAN_POINT ( 'NONE',  ( 15.18398860626900237, 28.73617430169797871, 5.000000000000000000 ) ) ;
#135947 = VECTOR ( 'NONE', #4646, 999.9999999999998863 ) ;
#135948 = AXIS2_PLACEMENT_3D ( 'NONE', #62330, #106483, #19512 ) ;
#135949 = DIRECTION ( 'NONE',  ( -0.7071067811865486830, -0.7071067811865464625, 0.000000000000000000 ) ) ;
#135950 = CARTESIAN_POINT ( 'NONE',  ( 107.8685099229812465, 7.919999999999951079, -19.04500000000195925 ) ) ;
#135951 = ORIENTED_EDGE ( 'NONE', *, *, #58289, .T. ) ;
#135953 = EDGE_CURVE ( 'NONE', #38622, #85582, #130796, .T. ) ;
#135952 = COLOUR_RGB ( '', 0.31764706, 0.68627451, 0.89019608) ;
#135954 = ORIENTED_EDGE ( 'NONE', *, *, #24514, .F. ) ;
#135955 = CARTESIAN_POINT ( 'NONE',  ( 96.16209685856478018, -5.291415217122919401, 3.054999999999997939 ) ) ;
#135956 = ORIENTED_EDGE ( 'NONE', *, *, #24166, .T. ) ;
#135957 = EDGE_CURVE ( 'NONE', #22428, #70976, #96663, .T. ) ;
#135958 = CARTESIAN_POINT ( 'NONE',  ( 28.17183060077627133, 0.7592924766157069794, 4.000000000000000000 ) ) ;
#135959 = ADVANCED_FACE ( 'NONE', ( #19847 ), #53950, .F. ) ;
#135960 = VECTOR ( 'NONE', #59297, 1000.000000000000000 ) ;
#135961 = LINE ( 'NONE', #93170, #699 ) ;
#135962 = ADVANCED_FACE ( 'NONE', ( #40221 ), #17651, .T. ) ;
#135963 = DIRECTION ( 'NONE',  ( 0.000000000000000000, -1.000000000000000000, 0.000000000000000000 ) ) ;
#135964 = DIRECTION ( 'NONE',  ( -0.7071067811865487940, 0.7071067811865463515, -0.000000000000000000 ) ) ;
#135965 = ORIENTED_EDGE ( 'NONE', *, *, #135201, .T. ) ;
#135966 = DIRECTION ( 'NONE',  ( 0.000000000000000000, -1.000000000000000000, 0.000000000000000000 ) ) ;
#135967 = SURFACE_SIDE_STYLE ('',( #58472 ) ) ;
#135968 = EDGE_CURVE ( 'NONE', #36236, #89986, #2112, .T. ) ;
#135969 = CARTESIAN_POINT ( 'NONE',  ( 26.99451991528749417, 28.92564299267956685, 4.000000000000000000 ) ) ;
#135970 = CARTESIAN_POINT ( 'NONE',  ( 68.81250000000000000, 5.819803920172571310, 5.819803920172576639 ) ) ;
#135971 = CARTESIAN_POINT ( 'NONE',  ( -3.489213562373097322, -27.52281430457057709, 5.000000000000000000 ) ) ;
#135972 = CARTESIAN_POINT ( 'NONE',  ( -8.292893218813391698, 5.259292476615661016, 5.000000000000000000 ) ) ;
#135973 = VERTEX_POINT ( 'NONE', #41607 ) ;
#135974 = DIRECTION ( 'NONE',  ( -1.000000000000000000, -1.224606353822377258E-16, -0.000000000000000000 ) ) ;
#135975 =( BOUNDED_CURVE ( )  B_SPLINE_CURVE ( 3, ( #52636, #11250, #64247, #20720 ),
 .UNSPECIFIED., .F., .F. ) 
 B_SPLINE_CURVE_WITH_KNOTS ( ( 4, 4 ),
 ( 1.502886732431669481, 1.547827028402603888 ),
 .UNSPECIFIED. ) 
 CURVE ( )  GEOMETRIC_REPRESENTATION_ITEM ( )  RATIONAL_B_SPLINE_CURVE ( ( 1.000000000000000000, 0.9998317045644854462, 0.9998317045644854462, 1.000000000000000000 ) ) 
 REPRESENTATION_ITEM ( '' )  );
#135976 = DIRECTION ( 'NONE',  ( 0.3543493200069162685, -0.000000000000000000, -0.9351131265310288487 ) ) ;
#135977 = EDGE_CURVE ( 'NONE', #70558, #89696, #106855, .T. ) ;
#135978 = ORIENTED_EDGE ( 'NONE', *, *, #34402, .T. ) ;
#135979 = VERTEX_POINT ( 'NONE', #106119 ) ;
#135980 = EDGE_CURVE ( 'NONE', #86031, #37037, #64083, .T. ) ;
#135981 = ORIENTED_EDGE ( 'NONE', *, *, #32566, .F. ) ;
#135982 = CARTESIAN_POINT ( 'NONE',  ( 52.93793019189809712, -6.110000000000001208, 1.637169565754158951 ) ) ;
#135983 = VECTOR ( 'NONE', #67753, 1000.000000000000000 ) ;
#135984 = VERTEX_POINT ( 'NONE', #53190 ) ;
#135985 = ADVANCED_FACE ( 'NONE', ( #108252 ), #40906, .F. ) ;
#135986 = CARTESIAN_POINT ( 'NONE',  ( 8.941639616203772789, -6.094999999999989093, 1.633150327867691765 ) ) ;
#135987 = CARTESIAN_POINT ( 'NONE',  ( -23.18650864602347283, -15.74070752338412049, 8.904080028138995573 ) ) ;
#135988 = ORIENTED_EDGE ( 'NONE', *, *, #6623, .F. ) ;
#135989 = DIRECTION ( 'NONE',  ( 0.000000000000000000, -1.000000000000000000, 0.000000000000000000 ) ) ;
#135990 = ORIENTED_EDGE ( 'NONE', *, *, #1250, .F. ) ;
#135991 = DIRECTION ( 'NONE',  ( -0.6830127018922180770, -0.6830127018922204085, -0.2588190451025213501 ) ) ;
#135992 = VECTOR ( 'NONE', #80153, 1000.000000000000000 ) ;
#135994 = ORIENTED_EDGE ( 'NONE', *, *, #126388, .T. ) ;
#135993 = CARTESIAN_POINT ( 'NONE',  ( -3.792893218813425893, -11.24070752338417201, 5.000000000000000000 ) ) ;
#135995 = ORIENTED_EDGE ( 'NONE', *, *, #59661, .F. ) ;
#135996 = DIRECTION ( 'NONE',  ( -0.6830127018922180770, -0.6830127018922204085, -0.2588190451025213501 ) ) ;
#135997 = CARTESIAN_POINT ( 'NONE',  ( 10.82816939922344979, 6.759292476615649470, 4.000000000000000000 ) ) ;
#135998 = CARTESIAN_POINT ( 'NONE',  ( 125.0370968585647944, -3.054999999999999272, -5.291415217122919401 ) ) ;
#135999 = ORIENTED_EDGE ( 'NONE', *, *, #138941, .T. ) ;
#136000 = PLANE ( 'NONE',  #66718 ) ;
#136001 = ORIENTED_EDGE ( 'NONE', *, *, #101235, .F. ) ;
#136002 = ORIENTED_EDGE ( 'NONE', *, *, #16856, .F. ) ;
#136003 = VERTEX_POINT ( 'NONE', #8919 ) ;
#136004 = EDGE_CURVE ( 'NONE', #23245, #98043, #34309, .T. ) ;
#136005 = AXIS2_PLACEMENT_3D ( 'NONE', #74576, #129636, #31770 ) ;
#136006 = LINE ( 'NONE', #114928, #120941 ) ;
#136007 = CARTESIAN_POINT ( 'NONE',  ( -30.29974487139158867, -27.71228299555227537, 4.000000000000000000 ) ) ;
#136008 = LINE ( 'NONE', #12784, #41642 ) ;
#136009 = CARTESIAN_POINT ( 'NONE',  ( -15.18398860626900237, 28.73617430169797871, 5.000000000000000000 ) ) ;
#136010 = EDGE_LOOP ( 'NONE', ( #132617, #130068, #12069, #112930 ) ) ;
#136011 = LINE ( 'NONE', #12081, #121157 ) ;
#136012 = ADVANCED_FACE ( 'NONE', ( #56098 ), #111878, .F. ) ;
#136013 = CARTESIAN_POINT ( 'NONE',  ( 19.52040314143522437, 7.934999999999989839, -2.126176841940961904 ) ) ;
#136014 = CARTESIAN_POINT ( 'NONE',  ( -3.712309939660258795, -21.73547319004781286, 4.999917730833664642 ) ) ;
#136015 = CARTESIAN_POINT ( 'NONE',  ( -42.29974487139158157, -27.71228299555235708, 4.000000000000000000 ) ) ;
#136016 = AXIS2_PLACEMENT_3D ( 'NONE', #136309, #83376, #38441 ) ;
#136017 = ORIENTED_EDGE ( 'NONE', *, *, #90893, .F. ) ;
#136018 = ORIENTED_EDGE ( 'NONE', *, *, #53785, .F. ) ;
#136019 = EDGE_CURVE ( 'NONE', #47990, #123098, #133632, .T. ) ;
#136020 = VERTEX_POINT ( 'NONE', #111124 ) ;
#136021 = CARTESIAN_POINT ( 'NONE',  ( -56.99451991528749062, 28.92564299267978001, 4.000000000000000000 ) ) ;
#136022 = DIRECTION ( 'NONE',  ( -0.7071067811865486830, 0.7071067811865464625, 0.000000000000000000 ) ) ;
#136023 = DIRECTION ( 'NONE',  ( -0.000000000000000000, -1.000000000000000000, -0.000000000000000000 ) ) ;
#136024 = PLANE ( 'NONE',  #135350 ) ;
#136025 = CARTESIAN_POINT ( 'NONE',  ( 34.49999999999975842, -11.94567065516892512, 4.994342998332160555 ) ) ;
#136026 = LINE ( 'NONE', #48308, #70997 ) ;
#136027 = CARTESIAN_POINT ( 'NONE',  ( 80.77083333333331439, -7.949999999999998401, -2.130196079827426203 ) ) ;
#136029 = AXIS2_PLACEMENT_3D ( 'NONE', #80815, #102569, #70669 ) ;
#136028 = CARTESIAN_POINT ( 'NONE',  ( -4.499999999999960920, 1.087461875839230707, 4.000000000000000000 ) ) ;
#136030 = LINE ( 'NONE', #92511, #30213 ) ;
#136031 = EDGE_CURVE ( 'NONE', #67930, #62339, #87264, .T. ) ;
#136032 = DIRECTION ( 'NONE',  ( -0.7071067811865486830, -0.7071067811865464625, -0.000000000000000000 ) ) ;
#136033 = CARTESIAN_POINT ( 'NONE',  ( -10.49999999999992362, -15.29013452822855079, 0.3645803511610097303 ) ) ;
#136034 = CARTESIAN_POINT ( 'NONE',  ( 34.92499999999998295, -13.29806943317888468, 4.500000000000000888 ) ) ;
#136035 = VERTEX_POINT ( 'NONE', #87973 ) ;
#136036 = CARTESIAN_POINT ( 'NONE',  ( 16.84501342860041717, -0.1639118413482353043, -31.04646532293632788 ) ) ;
#136037 = ORIENTED_EDGE ( 'NONE', *, *, #98796, .T. ) ;
#136038 = AXIS2_PLACEMENT_3D ( 'NONE', #139772, #137616, #104961 ) ;
#136039 = CARTESIAN_POINT ( 'NONE',  ( 8.816011393731004731, 28.73617430169781173, 5.000000000000000000 ) ) ;
#136041 = ORIENTED_EDGE ( 'NONE', *, *, #12988, .F. ) ;
#136040 = CARTESIAN_POINT ( 'NONE',  ( 6.299744871391586898, -27.71228299555210484, 4.000000000000000000 ) ) ;
#136042 = VECTOR ( 'NONE', #41089, 1000.000000000000000 ) ;
#136043 = EDGE_CURVE ( 'NONE', #59073, #112772, #43064, .T. ) ;
#136044 = LINE ( 'NONE', #34600, #30140 ) ;
#136045 = DIRECTION ( 'NONE',  ( -0.000000000000000000, 0.000000000000000000, 1.000000000000000000 ) ) ;
#136046 = EDGE_LOOP ( 'NONE', ( #10503, #74893, #54384, #31617 ) ) ;
#136047 = LINE ( 'NONE', #126583, #83185 ) ;
#136048 = ORIENTED_EDGE ( 'NONE', *, *, #96662, .T. ) ;
#136049 = DIRECTION ( 'NONE',  ( 0.7071067811865487940, 0.7071067811865463515, 0.000000000000000000 ) ) ;
#136050 = EDGE_LOOP ( 'NONE', ( #110932, #33282, #23552, #132091 ) ) ;
#136051 = VECTOR ( 'NONE', #65929, 1000.000000000000227 ) ;
#136052 = VECTOR ( 'NONE', #123514, 1000.000000000000000 ) ;
#136053 = LINE ( 'NONE', #27277, #1288 ) ;
#136054 = CARTESIAN_POINT ( 'NONE',  ( 104.3500270504628844, -5.819803920172572198, -5.819803920172572198 ) ) ;
#136055 = DIRECTION ( 'NONE',  ( 0.3543493200069162685, -0.000000000000000000, -0.9351131265310288487 ) ) ;
#136056 = CARTESIAN_POINT ( 'NONE',  ( 12.08840764549667668, 2.500000000000003553, 3.061616997868386099E-16 ) ) ;
#136057 = ORIENTED_EDGE ( 'NONE', *, *, #99734, .T. ) ;
#136058 = FACE_OUTER_BOUND ( 'NONE', #73470, .T. ) ;
#136059 = CARTESIAN_POINT ( 'NONE',  ( -30.28001967989385435, 0.7592924766157104211, 14.27032725228001908 ) ) ;
#136060 = DIRECTION ( 'NONE',  ( 1.000000000000000000, 0.000000000000000000, 0.000000000000000000 ) ) ;
#136061 = CARTESIAN_POINT ( 'NONE',  ( 23.62500000000000355, 6.094999999999989981, -1.119633336120465690E-15 ) ) ;
#136062 = LINE ( 'NONE', #91838, #141708 ) ;
#136063 = VECTOR ( 'NONE', #38762, 1000.000000000000000 ) ;
#136064 = DIRECTION ( 'NONE',  ( -0.6830127018922181881, 0.6830127018922202975, -0.2588190451025214056 ) ) ;
#136065 = FACE_OUTER_BOUND ( 'NONE', #30316, .T. ) ;
#136066 = ORIENTED_EDGE ( 'NONE', *, *, #141858, .F. ) ;
#136067 = FACE_OUTER_BOUND ( 'NONE', #139784, .T. ) ;
#136068 = ORIENTED_EDGE ( 'NONE', *, *, #23128, .T. ) ;
#136069 = EDGE_CURVE ( 'NONE', #69099, #72014, #131485, .T. ) ;
#136070 = CARTESIAN_POINT ( 'NONE',  ( 91.58376352523144703, -6.110000000000001208, -3.741295971395164515E-16 ) ) ;
#136071 = DIRECTION ( 'NONE',  ( -0.6830127018922180770, -0.6830127018922204085, -0.2588190451025213501 ) ) ;
#136072 = FACE_OUTER_BOUND ( 'NONE', #51297, .T. ) ;
#136073 = CARTESIAN_POINT ( 'NONE',  ( 34.49999999999975842, 19.46425560840029689, 4.994342998332160555 ) ) ;
#136074 = DIRECTION ( 'NONE',  ( -0.000000000000000000, 0.000000000000000000, 1.000000000000000000 ) ) ;
#136075 = EDGE_LOOP ( 'NONE', ( #102007, #66503, #79969, #116776 ) ) ;
#136076 = CARTESIAN_POINT ( 'NONE',  ( -0.4892135623730947680, -27.52281430457055578, 5.000000000000000000 ) ) ;
#136077 = CARTESIAN_POINT ( 'NONE',  ( 19.05000000000000071, 3.174999999999997158, 4.000000000000000000 ) ) ;
#136078 = EDGE_CURVE ( 'NONE', #81070, #140110, #32913, .T. ) ;
#136079 = VERTEX_POINT ( 'NONE', #77134 ) ;
#136080 = DIRECTION ( 'NONE',  ( -1.000000000000000000, -0.000000000000000000, -0.000000000000000000 ) ) ;
#136081 = ADVANCED_FACE ( 'NONE', ( #121307 ), #940, .F. ) ;
#136082 =( NAMED_UNIT ( * ) SI_UNIT ( $, .STERADIAN. ) SOLID_ANGLE_UNIT ( ) );
#136084 = VERTEX_POINT ( 'NONE', #57512 ) ;
#136083 = CARTESIAN_POINT ( 'NONE',  ( -54.29974487139159578, -27.71228299555243879, 4.000000000000000000 ) ) ;
#136086 = AXIS2_PLACEMENT_3D ( 'NONE', #71104, #38457, #126861 ) ;
#136085 = DIRECTION ( 'NONE',  ( 0.6830127018922180770, -0.6830127018922204085, -0.2588190451025213501 ) ) ;
#136087 = DIRECTION ( 'NONE',  ( 0.7071067811865487940, -0.7071067811865463515, 0.000000000000000000 ) ) ;
#136088 = LINE ( 'NONE', #100620, #56271 ) ;
#136089 = VERTEX_POINT ( 'NONE', #142372 ) ;
#136090 = ORIENTED_EDGE ( 'NONE', *, *, #102895, .F. ) ;
#136091 = VERTEX_POINT ( 'NONE', #21989 ) ;
#136092 = CARTESIAN_POINT ( 'NONE',  ( 85.02126352523144703, -4.472830434245839371, -4.472830434245840259 ) ) ;
#136093 =( BOUNDED_CURVE ( )  B_SPLINE_CURVE ( 3, ( #36880, #26028, #137655, #70972 ),
 .UNSPECIFIED., .F., .T. ) 
 B_SPLINE_CURVE_WITH_KNOTS ( ( 4, 4 ),
 ( 5.920967161967926273, 7.341195215986589417 ),
 .UNSPECIFIED. ) 
 CURVE ( )  GEOMETRIC_REPRESENTATION_ITEM ( )  RATIONAL_B_SPLINE_CURVE ( ( 1.000000000000000000, 0.8388583629366715977, 0.8388583629366715977, 1.000000000000000000 ) ) 
 REPRESENTATION_ITEM ( '' )  );
#136094 = ORIENTED_EDGE ( 'NONE', *, *, #115738, .F. ) ;
#136095 = CARTESIAN_POINT ( 'NONE',  ( -30.48921356237309510, -27.52281430457076894, 5.000000000000000000 ) ) ;
#136096 = LINE ( 'NONE', #125228, #96532 ) ;
#136097 = DIRECTION ( 'NONE',  ( -1.000000000000000000, -1.224606353822377258E-16, -0.000000000000000000 ) ) ;
#136098 = LINE ( 'NONE', #24482, #105599 ) ;
#136099 = ORIENTED_EDGE ( 'NONE', *, *, #6127, .T. ) ;
#136100 = EDGE_CURVE ( 'NONE', #47525, #91556, #110413, .T. ) ;
#136101 = DIRECTION ( 'NONE',  ( 0.7071067811865487940, 0.7071067811865463515, -0.000000000000000000 ) ) ;
#136102 = CARTESIAN_POINT ( 'NONE',  ( 24.79289321881329045, -14.24070752338413293, 5.000000000000000000 ) ) ;
#136103 = DIRECTION ( 'NONE',  ( -0.7071067811865487940, 0.7071067811865463515, 0.000000000000000000 ) ) ;
#136104 = CARTESIAN_POINT ( 'NONE',  ( 77.34959685856478018, 6.109999999999996767, 1.637169565754163836 ) ) ;
#136105 = ORIENTED_EDGE ( 'NONE', *, *, #101538, .T. ) ;
#136106 = CARTESIAN_POINT ( 'NONE',  ( 48.18398860626899705, 28.73617430169820608, 5.000000000000000000 ) ) ;
#136107 = DIRECTION ( 'NONE',  ( 0.7071067811865487940, 0.7071067811865463515, -0.000000000000000000 ) ) ;
#136108 = DIRECTION ( 'NONE',  ( -0.000000000000000000, 0.3543493200069153248, 0.9351131265310292928 ) ) ;
#136109 = VERTEX_POINT ( 'NONE', #89402 ) ;
#136110 = VERTEX_POINT ( 'NONE', #11088 ) ;
#136111 = DIRECTION ( 'NONE',  ( 0.7071067811865487940, -0.7071067811865463515, 0.000000000000000000 ) ) ;
#136112 = CARTESIAN_POINT ( 'NONE',  ( -14.56319896779161027, -12.74070752338414891, 9.898150129686410281 ) ) ;
#136113 = CARTESIAN_POINT ( 'NONE',  ( 23.10873647476855552, -5.808823158059033709, 5.808823158059035485 ) ) ;
#136114 = DIRECTION ( 'NONE',  ( 0.7071067811865487940, 0.7071067811865463515, 0.000000000000000000 ) ) ;
#136115 = CARTESIAN_POINT ( 'NONE',  ( -74.99451991528749772, 28.92564299267990435, 4.000000000000000000 ) ) ;
#136116 = FACE_OUTER_BOUND ( 'NONE', #8, .T. ) ;
#136117 = DIRECTION ( 'NONE',  ( 1.000000000000000000, 0.000000000000000000, 0.000000000000000000 ) ) ;
#136118 =( NAMED_UNIT ( * ) PLANE_ANGLE_UNIT ( ) SI_UNIT ( $, .RADIAN. ) );
#136119 = EDGE_CURVE ( 'NONE', #43341, #88152, #35048, .T. ) ;
#136120 = ORIENTED_EDGE ( 'NONE', *, *, #46362, .T. ) ;
#136121 =( GEOMETRIC_REPRESENTATION_CONTEXT ( 3 ) GLOBAL_UNCERTAINTY_ASSIGNED_CONTEXT ( ( #76536 ) ) GLOBAL_UNIT_ASSIGNED_CONTEXT ( ( #56860, #113313, #111921 ) ) REPRESENTATION_CONTEXT ( 'NONE', 'WORKASPACE' ) );
#136122 = ORIENTED_EDGE ( 'NONE', *, *, #83237, .T. ) ;
#136123 = EDGE_CURVE ( 'NONE', #109497, #142960, #99537, .T. ) ;
#136124 = LINE ( 'NONE', #34690, #119776 ) ;
#136125 = ORIENTED_EDGE ( 'NONE', *, *, #123353, .F. ) ;
#136126 = ADVANCED_FACE ( 'NONE', ( #78534 ), #122738, .F. ) ;
#136127 = ADVANCED_FACE ( 'NONE', ( #23416 ), #100983, .F. ) ;
#136128 = AXIS2_PLACEMENT_3D ( 'NONE', #45183, #133592, #32123 ) ;
#136129 = DIRECTION ( 'NONE',  ( 0.7071067811865487940, 0.7071067811865463515, 0.000000000000000000 ) ) ;
#136130 = ORIENTED_EDGE ( 'NONE', *, *, #85700, .T. ) ;
#136131 = LINE ( 'NONE', #100668, #15843 ) ;
#136132 = CARTESIAN_POINT ( 'NONE',  ( -39.48921356237310221, -27.52281430457082934, 5.000000000000000000 ) ) ;
#136133 = CARTESIAN_POINT ( 'NONE',  ( -5.395137668124758257, 21.75929247661549937, 21.32995629748187838 ) ) ;
#136134 = CARTESIAN_POINT ( 'NONE',  ( 16.82816939922340893, -17.24070752338411339, 4.000000000000000000 ) ) ;
#136135 = VECTOR ( 'NONE', #62038, 1000.000000000000000 ) ;
#136136 = PLANE ( 'NONE',  #465 ) ;
#136137 = ORIENTED_EDGE ( 'NONE', *, *, #28998, .T. ) ;
#136138 = LINE ( 'NONE', #98686, #72658 ) ;
#136139 = DIRECTION ( 'NONE',  ( -0.6830127018922181881, 0.6830127018922202975, -0.2588190451025214056 ) ) ;
#136140 = AXIS2_PLACEMENT_3D ( 'NONE', #142393, #121325, #118469 ) ;
#136141 = EDGE_CURVE ( 'NONE', #119333, #91761, #1638, .T. ) ;
#136142 = ORIENTED_EDGE ( 'NONE', *, *, #74970, .T. ) ;
#136143 = DIRECTION ( 'NONE',  ( -1.000000000000000000, -1.224606353822377258E-16, -0.000000000000000000 ) ) ;
#136144 = ORIENTED_EDGE ( 'NONE', *, *, #131777, .T. ) ;
#136145 = EDGE_CURVE ( 'NONE', #48159, #3321, #45920, .T. ) ;
#136146 = EDGE_LOOP ( 'NONE', ( #84603, #103547, #70695, #52100 ) ) ;
#136147 = CARTESIAN_POINT ( 'NONE',  ( -9.524001385854420576, 22.03583458319438648, 4.979811245910087614 ) ) ;
#136148 = ORIENTED_EDGE ( 'NONE', *, *, #96849, .F. ) ;
#136149 = ORIENTED_EDGE ( 'NONE', *, *, #84128, .F. ) ;
#136150 = CARTESIAN_POINT ( 'NONE',  ( 15.49238828748955576, -2.500000000000000444, 3.061616997868384127E-16 ) ) ;
#136151 = ORIENTED_EDGE ( 'NONE', *, *, #56657, .T. ) ;
#136153 = AXIS2_PLACEMENT_3D ( 'NONE', #27655, #39275, #70515 ) ;
#136152 = VECTOR ( 'NONE', #62353, 1000.000000000000000 ) ;
#136154 = ADVANCED_FACE ( 'NONE', ( #134350 ), #79291, .T. ) ;
#136155 = CARTESIAN_POINT ( 'NONE',  ( 23.89661266223020419, -0.3091507863911187037, 4.000000000000000000 ) ) ;
#136156 = DIRECTION ( 'NONE',  ( 0.7071067811865487940, 0.7071067811865463515, -0.000000000000000000 ) ) ;
#136157 = CARTESIAN_POINT ( 'NONE',  ( 119.5837635252314470, -6.110000000000001208, -3.741295971395164515E-16 ) ) ;
#136158 = PLANE ( 'NONE',  #33294 ) ;
#136159 = CARTESIAN_POINT ( 'NONE',  ( 24.69524342170288023, 1.235879655689124501, 4.000000000000000000 ) ) ;
#136160 = CARTESIAN_POINT ( 'NONE',  ( -34.92500000000001137, 21.73644205237997795, 4.195230610814792094 ) ) ;
#136161 = DIRECTION ( 'NONE',  ( 1.000000000000000000, 0.000000000000000000, 0.000000000000000000 ) ) ;
#136162 = ADVANCED_FACE ( 'NONE', ( #4458 ), #15371, .F. ) ;
#136163 = CARTESIAN_POINT ( 'NONE',  ( 0.000000000000000000, 0.000000000000000000, 0.000000000000000000 ) ) ;
#136164 = PLANE ( 'NONE',  #16582 ) ;
#136165 = CYLINDRICAL_SURFACE ( 'NONE', #10417, 2.500000000000000444 ) ;
#136166 = ORIENTED_EDGE ( 'NONE', *, *, #80033, .F. ) ;
#136167 = CARTESIAN_POINT ( 'NONE',  ( 9.748407645496676821, 9.139736423841732040E-16, 0.000000000000000000 ) ) ;
#136168 = LINE ( 'NONE', #81099, #38392 ) ;
#136169 = ORIENTED_EDGE ( 'NONE', *, *, #92507, .F. ) ;
#136170 = VERTEX_POINT ( 'NONE', #113279 ) ;
#136171 = EDGE_CURVE ( 'NONE', #72085, #134621, #48766, .T. ) ;
#136172 = DIRECTION ( 'NONE',  ( -0.000000000000000000, 0.3543493200069153248, 0.9351131265310292928 ) ) ;
#136173 = ORIENTED_EDGE ( 'NONE', *, *, #131134, .F. ) ;
#136174 = AXIS2_PLACEMENT_3D ( 'NONE', #77050, #43679, #110332 ) ;
#136175 = LINE ( 'NONE', #26704, #130178 ) ;
#136176 = LINE ( 'NONE', #69524, #17688 ) ;
#136177 = LINE ( 'NONE', #12250, #8546 ) ;
#136178 = CARTESIAN_POINT ( 'NONE',  ( -62.99451991528749772, 28.92564299267982264, 4.000000000000000000 ) ) ;
#136179 = CARTESIAN_POINT ( 'NONE',  ( -20.99451991528748707, 28.92564299267952777, 4.000000000000000000 ) ) ;
#136180 = ORIENTED_EDGE ( 'NONE', *, *, #41124, .F. ) ;
#136181 = VECTOR ( 'NONE', #109411, 1000.000000000000000 ) ;
#136182 = CARTESIAN_POINT ( 'NONE',  ( -8.510786437626906675, -27.52281430457049183, 5.000000000000000000 ) ) ;
#136183 = ORIENTED_EDGE ( 'NONE', *, *, #22966, .T. ) ;
#136184 = CARTESIAN_POINT ( 'NONE',  ( 39.48921356237310221, -27.52281430457082934, 5.000000000000000000 ) ) ;
#136185 = EDGE_CURVE ( 'NONE', #71407, #64361, #48055, .T. ) ;
#136186 = CARTESIAN_POINT ( 'NONE',  ( 28.65040314143521982, 7.934999999999989839, -2.126176841940961904 ) ) ;
#136187 = CARTESIAN_POINT ( 'NONE',  ( 8.897059064271770623, 4.202752102959690472E-16, 0.000000000000000000 ) ) ;
#136188 = CARTESIAN_POINT ( 'NONE',  ( 98.22502705046288440, 5.819803920172573974, -5.819803920172573086 ) ) ;
#136189 = ORIENTED_EDGE ( 'NONE', *, *, #6927, .F. ) ;
#136190 = VERTEX_POINT ( 'NONE', #5219 ) ;
#136191 = EDGE_LOOP ( 'NONE', ( #62529, #92362, #97471, #103431 ) ) ;
#136192 = LINE ( 'NONE', #35503, #132922 ) ;
#136193 = DIRECTION ( 'NONE',  ( -0.7071067811865487940, 0.7071067811865463515, 0.000000000000000000 ) ) ;
#136195 = VECTOR ( 'NONE', #101389, 1000.000000000000000 ) ;
#136194 = CARTESIAN_POINT ( 'NONE',  ( -2.994519915287485734, 28.92564299267940342, 4.000000000000000000 ) ) ;
#136196 = DIRECTION ( 'NONE',  ( 1.000000000000000000, 0.000000000000000000, 0.000000000000000000 ) ) ;
#136197 = VERTEX_POINT ( 'NONE', #82830 ) ;
#136198 = DIRECTION ( 'NONE',  ( -0.6830127018922180770, -0.6830127018922204085, -0.2588190451025213501 ) ) ;
#136199 = VECTOR ( 'NONE', #135186, 1000.000000000000000 ) ;
#136200 = DIRECTION ( 'NONE',  ( -0.7071067811865486830, 0.7071067811865464625, 0.000000000000000000 ) ) ;
#136201 = EDGE_CURVE ( 'NONE', #116001, #52530, #27703, .T. ) ;
#136202 = CARTESIAN_POINT ( 'NONE',  ( 8.292893218813400580, -9.740707523384184441, 5.000000000000000000 ) ) ;
#136203 = LINE ( 'NONE', #94113, #102387 ) ;
#136204 = VERTEX_POINT ( 'NONE', #58255 ) ;
#136205 = CARTESIAN_POINT ( 'NONE',  ( 8.000000000000007105, 0.000000000000000000, 0.000000000000000000 ) ) ;
#136206 = ORIENTED_EDGE ( 'NONE', *, *, #25554, .F. ) ;
#136208 = ORIENTED_EDGE ( 'NONE', *, *, #9795, .F. ) ;
#136207 = FACE_OUTER_BOUND ( 'NONE', #23346, .T. ) ;
#136209 = EDGE_LOOP ( 'NONE', ( #14727, #21671, #86622, #56094 ) ) ;
#136210 = EDGE_CURVE ( 'NONE', #70446, #18049, #103132, .T. ) ;
#136211 = LINE ( 'NONE', #4940, #37779 ) ;
#136212 = CARTESIAN_POINT ( 'NONE',  ( 106.0000000000000000, 0.000000000000000000, -7.950000000000000178 ) ) ;
#136213 = ORIENTED_EDGE ( 'NONE', *, *, #77225, .F. ) ;
#136214 = CARTESIAN_POINT ( 'NONE',  ( -63.48921356237309510, -27.52281430457099631, 5.000000000000000000 ) ) ;
#136215 = ORIENTED_EDGE ( 'NONE', *, *, #63185, .T. ) ;
#136216 = LINE ( 'NONE', #36901, #96084 ) ;
#136217 = LINE ( 'NONE', #47832, #46313 ) ;
#136218 = CARTESIAN_POINT ( 'NONE',  ( 127.2458603837962272, 3.974999999999996980, 6.884901960086287964 ) ) ;
#136219 = PLANE ( 'NONE',  #48500 ) ;
#136220 = CARTESIAN_POINT ( 'NONE',  ( -22.22850677138650610, 20.25929247661551003, 7.808871592221717783 ) ) ;
#136221 = DIRECTION ( 'NONE',  ( 0.000000000000000000, 1.000000000000000000, 0.000000000000000000 ) ) ;
#136222 = LINE ( 'NONE', #60861, #123286 ) ;
#136223 = DIRECTION ( 'NONE',  ( 0.6830127018922180770, -0.6830127018922204085, -0.2588190451025213501 ) ) ;
#136224 =( NAMED_UNIT ( * ) SI_UNIT ( $, .STERADIAN. ) SOLID_ANGLE_UNIT ( ) );
#136225 = CARTESIAN_POINT ( 'NONE',  ( 31.04123647476855297, 0.000000000000000000, 7.934999999999990727 ) ) ;
#136226 = CARTESIAN_POINT ( 'NONE',  ( 0.5620698081018861147, -7.934999999999990727, -2.126176841940955242 ) ) ;
#136227 = CARTESIAN_POINT ( 'NONE',  ( 32.99999999999977263, 4.384688058510604058, -7.090945410444609465 ) ) ;
#136228 = DIRECTION ( 'NONE',  ( -0.7071067811865486830, -0.7071067811865464625, 0.000000000000000000 ) ) ;
#136229 = DIRECTION ( 'NONE',  ( -0.000000000000000000, 0.000000000000000000, 1.000000000000000000 ) ) ;
#136230 = ORIENTED_EDGE ( 'NONE', *, *, #49602, .T. ) ;
#136231 = ORIENTED_EDGE ( 'NONE', *, *, #45906, .T. ) ;
#136232 = CARTESIAN_POINT ( 'NONE',  ( 92.43749999999998579, 5.819803920172573974, -5.819803920172572198 ) ) ;
#136233 = VERTEX_POINT ( 'NONE', #80685 ) ;
#136234 = VERTEX_POINT ( 'NONE', #124884 ) ;
#136235 = EDGE_CURVE ( 'NONE', #100840, #62352, #69828, .T. ) ;
#136236 = CARTESIAN_POINT ( 'NONE',  ( 25.49999999999982947, -1.533600742197721134, 5.000000000000000000 ) ) ;
#136237 = DIRECTION ( 'NONE',  ( 0.7071067811865487940, 0.7071067811865463515, -0.000000000000000000 ) ) ;
#136238 = CARTESIAN_POINT ( 'NONE',  ( 0.000000000000000000, 0.000000000000000000, 0.000000000000000000 ) ) ;
#136239 = EDGE_LOOP ( 'NONE', ( #7654, #53554, #64347, #70539, #76396 ) ) ;
#136240 = PRESENTATION_LAYER_ASSIGNMENT (  '', '', ( #34422 ) ) ;
#136241 = CONICAL_SURFACE ( 'NONE', #15730, 2.552699999999994418, 1.029744258676651869 ) ;
#136243 = CARTESIAN_POINT ( 'NONE',  ( 6.639999999999992575, -35.15000000000000568, 18.14679158439240325 ) ) ;
#136242 = CIRCLE ( 'NONE', #62275, 2.500000000000000444 ) ;
#136244 = AXIS2_PLACEMENT_3D ( 'NONE', #71259, #60391, #104579 ) ;
#136245 = LINE ( 'NONE', #133417, #99592 ) ;
#136246 = CARTESIAN_POINT ( 'NONE',  ( 126.9643883377496962, 2.362378534332376212, 6.061514835086926567 ) ) ;
#136247 = ADVANCED_FACE ( 'NONE', ( #37901 ), #102445, .T. ) ;
#136248 = AXIS2_PLACEMENT_3D ( 'NONE', #98414, #120858, #65825 ) ;
#136249 = EDGE_CURVE ( 'NONE', #66060, #12755, #135768, .T. ) ;
#136250 = CYLINDRICAL_SURFACE ( 'NONE', #5359, 2.500000000000000000 ) ;
#136251 = DIRECTION ( 'NONE',  ( -0.000000000000000000, -0.000000000000000000, -1.000000000000000000 ) ) ;
#136253 = LINE ( 'NONE', #112378, #121657 ) ;
#136252 = AXIS2_PLACEMENT_3D ( 'NONE', #53051, #133497, #34184 ) ;
#136254 = CARTESIAN_POINT ( 'NONE',  ( 63.29974487139158867, -27.71228299555250274, 4.000000000000000000 ) ) ;
#136255 = DIRECTION ( 'NONE',  ( 0.7071067811865486830, -0.7071067811865464625, -0.000000000000000000 ) ) ;
#136256 = VECTOR ( 'NONE', #79388, 1000.000000000000000 ) ;
#136257 = CARTESIAN_POINT ( 'NONE',  ( 30.18398860626900060, 28.73617430169808173, 5.000000000000000000 ) ) ;
#136258 = SURFACE_SIDE_STYLE ('',( #92034 ) ) ;
#136259 = ORIENTED_EDGE ( 'NONE', *, *, #13047, .F. ) ;
#136260 = EDGE_LOOP ( 'NONE', ( #19003, #36370, #89944, #568 ) ) ;
#136261 = CARTESIAN_POINT ( 'NONE',  ( 115.0629301918981042, 1.637169565754157174, 6.110000000000002984 ) ) ;
#136262 = ORIENTED_EDGE ( 'NONE', *, *, #37968, .F. ) ;
#136263 = ADVANCED_FACE ( 'NONE', ( #2354 ), #25561, .F. ) ;
#136264 = CARTESIAN_POINT ( 'NONE',  ( 20.70025512860841133, -27.71228299555191654, 4.000000000000000000 ) ) ;
#136265 = VECTOR ( 'NONE', #74909, 1000.000000000000000 ) ;
#136266 = PLANE ( 'NONE',  #22502 ) ;
#136267 = EDGE_LOOP ( 'NONE', ( #101154, #67962 ) ) ;
#136268 = EDGE_CURVE ( 'NONE', #118158, #118217, #37161, .T. ) ;
#136269 = CARTESIAN_POINT ( 'NONE',  ( 66.18398860626901126, 28.73617430169833753, 5.000000000000000000 ) ) ;
#136270 = DIRECTION ( 'NONE',  ( -0.6830127018922181881, 0.6830127018922202975, -0.2588190451025214056 ) ) ;
#136271 = VECTOR ( 'NONE', #4055, 999.9999999999998863 ) ;
#136272 = CARTESIAN_POINT ( 'NONE',  ( 102.7245968585647802, -1.637169565754160949, 6.109999999999997655 ) ) ;
#136273 = ORIENTED_EDGE ( 'NONE', *, *, #116300, .T. ) ;
#136274 = ORIENTED_EDGE ( 'NONE', *, *, #51679, .T. ) ;
#136275 = CARTESIAN_POINT ( 'NONE',  ( 8.206660635421465955, 21.75929247661549226, 4.998822639870702744 ) ) ;
#136276 = CARTESIAN_POINT ( 'NONE',  ( 34.17183060077623225, 0.7592924766157086447, 4.000000000000000000 ) ) ;
#136277 = VECTOR ( 'NONE', #64367, 1000.000000000000000 ) ;
#136278 = ORIENTED_EDGE ( 'NONE', *, *, #11832, .F. ) ;
#136279 = ORIENTED_EDGE ( 'NONE', *, *, #45530, .T. ) ;
#136280 = ORIENTED_EDGE ( 'NONE', *, *, #74455, .F. ) ;
#136281 = CARTESIAN_POINT ( 'NONE',  ( 10.49999999999992539, 11.52377502935403619, -1.522421517564110038 ) ) ;
#136282 = CARTESIAN_POINT ( 'NONE',  ( 0.1600000000000011136, 3.289720434613005118, -7.220939306079887210 ) ) ;
#136283 = CONICAL_SURFACE ( 'NONE', #73787, 2.055000000000000604, 0.9599310885968764806 ) ;
#136284 = EDGE_CURVE ( 'NONE', #12574, #70009, #131104, .T. ) ;
#136285 = FILL_AREA_STYLE ('',( #3602 ) ) ;
#136286 = EDGE_CURVE ( 'NONE', #75407, #100683, #26990, .T. ) ;
#136287 = CARTESIAN_POINT ( 'NONE',  ( -21.29974487139158512, -27.71228299555221142, 4.000000000000000000 ) ) ;
#136288 = VERTEX_POINT ( 'NONE', #16841 ) ;
#136289 = ORIENTED_EDGE ( 'NONE', *, *, #110385, .T. ) ;
#136290 = EDGE_CURVE ( 'NONE', #109867, #67375, #40864, .T. ) ;
#136291 = DIRECTION ( 'NONE',  ( 0.7071067811865487940, 0.7071067811865463515, 0.000000000000000000 ) ) ;
#136292 = VERTEX_POINT ( 'NONE', #115386 ) ;
#136293 = VERTEX_POINT ( 'NONE', #114700 ) ;
#136294 = VECTOR ( 'NONE', #13325, 1000.000000000000227 ) ;
#136295 = EDGE_CURVE ( 'NONE', #45590, #102711, #60373, .T. ) ;
#136296 = EDGE_CURVE ( 'NONE', #26486, #92120, #79996, .T. ) ;
#136297 = DIRECTION ( 'NONE',  ( 0.6830127018922181881, 0.6830127018922202975, -0.2588190451025214056 ) ) ;
#136298 = DIRECTION ( 'NONE',  ( 0.6830127018922181881, 0.6830127018922202975, -0.2588190451025214056 ) ) ;
#136299 = ORIENTED_EDGE ( 'NONE', *, *, #134517, .F. ) ;
#136300 = CARTESIAN_POINT ( 'NONE',  ( -21.48921356237309155, -27.52281430457070499, 5.000000000000000000 ) ) ;
#136301 = PLANE ( 'NONE',  #10870 ) ;
#136302 = CARTESIAN_POINT ( 'NONE',  ( 0.000000000000000000, 0.000000000000000000, 5.000000000000000000 ) ) ;
#136303 = EDGE_CURVE ( 'NONE', #26845, #131176, #24854, .T. ) ;
#136304 = CARTESIAN_POINT ( 'NONE',  ( -11.99999999999991296, -18.03360074219755660, 5.000000000000000000 ) ) ;
#136305 = FACE_OUTER_BOUND ( 'NONE', #98411, .T. ) ;
#136306 = FACE_BOUND ( 'NONE', #54182, .T. ) ;
#136307 = ADVANCED_FACE ( 'NONE', ( #140738 ), #5921, .F. ) ;
#136308 = EDGE_LOOP ( 'NONE', ( #48727, #82124, #49372, #64511 ) ) ;
#136309 = CARTESIAN_POINT ( 'NONE',  ( -51.18398860626899705, 28.73617430169823095, 5.000000000000000000 ) ) ;
#136310 = CARTESIAN_POINT ( 'NONE',  ( 21.66240673564756491, 0.000000000000000000, 0.000000000000000000 ) ) ;
#136311 = SURFACE_SIDE_STYLE ('',( #92082 ) ) ;
#136312 = EDGE_CURVE ( 'NONE', #118985, #69799, #13096, .T. ) ;
#136313 = ORIENTED_EDGE ( 'NONE', *, *, #94026, .T. ) ;
#136314 = ORIENTED_EDGE ( 'NONE', *, *, #76083, .T. ) ;
#136315 = ORIENTED_EDGE ( 'NONE', *, *, #22191, .F. ) ;
#136316 = ORIENTED_EDGE ( 'NONE', *, *, #16288, .F. ) ;
#136317 = CARTESIAN_POINT ( 'NONE',  ( 42.05793019189811588, 6.110000000000000320, -1.637169565754156064 ) ) ;
#136318 = EDGE_CURVE ( 'NONE', #38121, #130029, #95097, .T. ) ;
#136319 = ORIENTED_EDGE ( 'NONE', *, *, #28016, .F. ) ;
#136320 = EDGE_CURVE ( 'NONE', #95983, #88854, #139367, .T. ) ;
#136321 = CARTESIAN_POINT ( 'NONE',  ( -30.29974487139158867, -27.71228299555227537, 4.000000000000000000 ) ) ;
#136322 = FACE_OUTER_BOUND ( 'NONE', #26651, .T. ) ;
#136323 = CARTESIAN_POINT ( 'NONE',  ( -75.48921356237309510, -27.52281430457107803, 5.000000000000000000 ) ) ;
#136324 = VERTEX_POINT ( 'NONE', #40054 ) ;
#136325 = LINE ( 'NONE', #48616, #7418 ) ;
#136326 = ADVANCED_FACE ( 'NONE', ( #6617 ), #116860, .T. ) ;
#136327 = FACE_OUTER_BOUND ( 'NONE', #43416, .T. ) ;
#136328 = FACE_OUTER_BOUND ( 'NONE', #17507, .T. ) ;
#136329 = CARTESIAN_POINT ( 'NONE',  ( -34.42500000000001137, -6.022814304570508703, 5.000000000000000000 ) ) ;
#136330 = CARTESIAN_POINT ( 'NONE',  ( 12.00548008471251293, 28.92564299267929684, 4.000000000000000000 ) ) ;
#136331 = DIRECTION ( 'NONE',  ( 1.000000000000000000, 0.000000000000000000, 0.000000000000000000 ) ) ;
#136332 = ORIENTED_EDGE ( 'NONE', *, *, #43922, .F. ) ;
#136333 = ORIENTED_EDGE ( 'NONE', *, *, #59981, .F. ) ;
#136335 = VERTEX_POINT ( 'NONE', #130621 ) ;
#136334 = EDGE_CURVE ( 'NONE', #110155, #39265, #118997, .T. ) ;
#136336 = ORIENTED_EDGE ( 'NONE', *, *, #133563, .F. ) ;
#136337 = CARTESIAN_POINT ( 'NONE',  ( 5.999999999999958256, -13.97847968911259819, -0.1324546996126661491 ) ) ;
#136338 = AXIS2_PLACEMENT_3D ( 'NONE', #24349, #22882, #91064 ) ;
#136339 = AXIS2_PLACEMENT_3D ( 'NONE', #63498, #75084, #98241 ) ;
#136340 = ORIENTED_EDGE ( 'NONE', *, *, #126478, .T. ) ;
#136341 = VECTOR ( 'NONE', #82142, 1000.000000000000000 ) ;
#136343 = EDGE_LOOP ( 'NONE', ( #118099, #96540, #25973, #39198 ) ) ;
#136342 = VECTOR ( 'NONE', #98513, 1000.000000000000000 ) ;
#136344 = DIRECTION ( 'NONE',  ( 0.6830127018922180770, -0.6830127018922204085, -0.2588190451025213501 ) ) ;
#136345 = CARTESIAN_POINT ( 'NONE',  ( 9.208651418775088970, 4.584330080086930965E-16, 0.000000000000000000 ) ) ;
#136346 = EDGE_LOOP ( 'NONE', ( #10228, #73151, #101621, #19140 ) ) ;
#136347 = EDGE_CURVE ( 'NONE', #49090, #55653, #28443, .T. ) ;
#136348 = DIRECTION ( 'NONE',  ( 0.7071067811865487940, 0.7071067811865463515, -0.000000000000000000 ) ) ;
#136350 = ORIENTED_EDGE ( 'NONE', *, *, #126773, .T. ) ;
#136349 =( GEOMETRIC_REPRESENTATION_CONTEXT ( 3 ) GLOBAL_UNCERTAINTY_ASSIGNED_CONTEXT ( ( #89664 ) ) GLOBAL_UNIT_ASSIGNED_CONTEXT ( ( #57436, #35703, #859 ) ) REPRESENTATION_CONTEXT ( 'NONE', 'WORKASPACE' ) );
#136351 = CARTESIAN_POINT ( 'NONE',  ( 0.4644479527036028399, 0.4000000000000001887, -2.317232259782045833 ) ) ;
#136352 = EDGE_CURVE ( 'NONE', #62344, #112545, #120682, .T. ) ;
#136353 = CARTESIAN_POINT ( 'NONE',  ( 4.499999999999976019, 7.466399257802187606, 5.000000000000000000 ) ) ;
#136354 = VERTEX_POINT ( 'NONE', #50903 ) ;
#136355 = CARTESIAN_POINT ( 'NONE',  ( 98.64126352523145158, 4.472830434245837594, 4.472830434245841147 ) ) ;
#136356 = DIRECTION ( 'NONE',  ( -0.7071067811865486830, 0.7071067811865464625, 0.000000000000000000 ) ) ;
#136357 = DIRECTION ( 'NONE',  ( -0.7071067811865487940, 0.7071067811865463515, -0.000000000000000000 ) ) ;
#136358 = ORIENTED_EDGE ( 'NONE', *, *, #53665, .F. ) ;
#136359 = ORIENTED_EDGE ( 'NONE', *, *, #104908, .F. ) ;
#136360 = CARTESIAN_POINT ( 'NONE',  ( 0.8183591370940799248, -52.14999999999999147, -41.64500000000001023 ) ) ;
#136361 = ORIENTED_EDGE ( 'NONE', *, *, #43324, .F. ) ;
#136362 = AXIS2_PLACEMENT_3D ( 'NONE', #79757, #24595, #55833 ) ;
#136363 =( NAMED_UNIT ( * ) PLANE_ANGLE_UNIT ( ) SI_UNIT ( $, .RADIAN. ) );
#136364 = DIRECTION ( 'NONE',  ( -0.7071067811865486830, -0.7071067811865464625, 0.000000000000000000 ) ) ;
#136365 = ADVANCED_FACE ( 'NONE', ( #128466 ), #74077, .F. ) ;
#136366 = DIRECTION ( 'NONE',  ( -0.5735764363510507113, 0.8191520442889885789, 1.003171929053520926E-16 ) ) ;
#136367 =( NAMED_UNIT ( * ) SI_UNIT ( $, .STERADIAN. ) SOLID_ANGLE_UNIT ( ) );
#136369 = EDGE_LOOP ( 'NONE', ( #56908, #44260, #101155, #106394 ) ) ;
#136368 =( BOUNDED_CURVE ( )  B_SPLINE_CURVE ( 3, ( #71938, #140038, #19659, #116110 ),
 .UNSPECIFIED., .F., .F. ) 
 B_SPLINE_CURVE_WITH_KNOTS ( ( 4, 4 ),
 ( 2.779374508378132713, 4.199602562396797190 ),
 .UNSPECIFIED. ) 
 CURVE ( )  GEOMETRIC_REPRESENTATION_ITEM ( )  RATIONAL_B_SPLINE_CURVE ( ( 1.000000000000000000, 0.8388583629366712646, 0.8388583629366712646, 1.000000000000000000 ) ) 
 REPRESENTATION_ITEM ( '' )  );
#136370 = AXIS2_PLACEMENT_3D ( 'NONE', #51757, #54610, #84394 ) ;
#136371 = CARTESIAN_POINT ( 'NONE',  ( -16.49999999999988631, 22.01701374228154151, 2.453858888625669366 ) ) ;
#136372 = VERTEX_POINT ( 'NONE', #138630 ) ;
#136373 = CARTESIAN_POINT ( 'NONE',  ( -66.29974487139159578, -27.71228299555252406, 4.000000000000000000 ) ) ;
#136374 = VECTOR ( 'NONE', #70696, 1000.000000000000000 ) ;
#136375 =( BOUNDED_CURVE ( )  B_SPLINE_CURVE ( 3, ( #5011, #138432, #27500, #50008 ),
 .UNSPECIFIED., .F., .F. ) 
 B_SPLINE_CURVE_WITH_KNOTS ( ( 4, 4 ),
 ( 5.143245962375972091, 6.645403452391247079 ),
 .UNSPECIFIED. ) 
 CURVE ( )  GEOMETRIC_REPRESENTATION_ITEM ( )  RATIONAL_B_SPLINE_CURVE ( ( 1.000000000000000000, 0.8206354192515254997, 0.8206354192515254997, 1.000000000000000000 ) ) 
 REPRESENTATION_ITEM ( '' )  );
#136377 = VECTOR ( 'NONE', #80103, 1000.000000000000000 ) ;
#136376 = CARTESIAN_POINT ( 'NONE',  ( -75.18398860626899705, 28.73617430169839793, 5.000000000000000000 ) ) ;
#136378 = ORIENTED_EDGE ( 'NONE', *, *, #116851, .F. ) ;
#136379 = AXIS2_PLACEMENT_3D ( 'NONE', #141184, #43325, #7809 ) ;
#136381 = ORIENTED_EDGE ( 'NONE', *, *, #4822, .F. ) ;
#136380 = CARTESIAN_POINT ( 'NONE',  ( 33.48921356237309510, -27.52281430457078670, 5.000000000000000000 ) ) ;
#136382 = ORIENTED_EDGE ( 'NONE', *, *, #116768, .F. ) ;
#136383 = CARTESIAN_POINT ( 'NONE',  ( -19.28515664589289003, 1.196650378695325090, -30.59010235425025215 ) ) ;
#136384 = VECTOR ( 'NONE', #99118, 1000.000000000000000 ) ;
#136385 =( LENGTH_UNIT ( ) NAMED_UNIT ( * ) SI_UNIT ( .MILLI., .METRE. ) );
#136386 = ORIENTED_EDGE ( 'NONE', *, *, #42125, .F. ) ;
#136387 = CARTESIAN_POINT ( 'NONE',  ( 41.99451991528749062, 28.92564299267967343, 4.000000000000000000 ) ) ;
#136388 = PLANE ( 'NONE',  #102949 ) ;
#136389 = CARTESIAN_POINT ( 'NONE',  ( -12.48921356237309155, -27.52281430457064104, 5.000000000000000000 ) ) ;
#136390 = ORIENTED_EDGE ( 'NONE', *, *, #50851, .F. ) ;
#136391 = FACE_OUTER_BOUND ( 'NONE', #31766, .T. ) ;
#136392 = EDGE_CURVE ( 'NONE', #79017, #35337, #61795, .T. ) ;
#136393 = CARTESIAN_POINT ( 'NONE',  ( 9.792893218813393474, -17.24070752338410628, 5.000000000000000000 ) ) ;
#136394 = SURFACE_SIDE_STYLE ('',( #91485 ) ) ;
#136395 = LINE ( 'NONE', #123421, #40202 ) ;
#136396 = CARTESIAN_POINT ( 'NONE',  ( 126.4628116846214851, -6.884920636358014434, -1.229062542668005742 ) ) ;
#136397 = DIRECTION ( 'NONE',  ( -0.7071067811865486830, -0.7071067811865464625, 0.000000000000000000 ) ) ;
#136398 = DIRECTION ( 'NONE',  ( -0.7071067811865486830, -0.7071067811865464625, 0.000000000000000000 ) ) ;
#136399 = VERTEX_POINT ( 'NONE', #52311 ) ;
#136400 = ORIENTED_EDGE ( 'NONE', *, *, #105654, .F. ) ;
#136401 = ORIENTED_EDGE ( 'NONE', *, *, #46140, .T. ) ;
#136402 = CARTESIAN_POINT ( 'NONE',  ( 118.5416666666666714, -3.975000000000002753, 6.884901960086286188 ) ) ;
#136403 = ORIENTED_EDGE ( 'NONE', *, *, #53279, .F. ) ;
#136404 = EDGE_LOOP ( 'NONE', ( #58910, #94389, #72024, #90488 ) ) ;
#136405 = ORIENTED_EDGE ( 'NONE', *, *, #79733, .T. ) ;
#136406 = CARTESIAN_POINT ( 'NONE',  ( -11.81601139373100651, 28.73617430169779041, 5.000000000000000000 ) ) ;
#136407 = LINE ( 'NONE', #37098, #64769 ) ;
#136408 = ORIENTED_EDGE ( 'NONE', *, *, #49823, .F. ) ;
#136409 = CARTESIAN_POINT ( 'NONE',  ( -27.29974487139158512, -27.71228299555225405, 4.000000000000000000 ) ) ;
#136410 = DIRECTION ( 'NONE',  ( -0.7071067811865486830, 0.7071067811865464625, 0.000000000000000000 ) ) ;
#136411 = DIRECTION ( 'NONE',  ( 0.3543493200069162685, -0.000000000000000000, -0.9351131265310288487 ) ) ;
#136412 = CARTESIAN_POINT ( 'NONE',  ( 113.1670968585647756, -3.055000000000000160, -5.291415217122921177 ) ) ;
#136413 = EDGE_CURVE ( 'NONE', #24882, #43020, #83546, .T. ) ;
#136414 = ORIENTED_EDGE ( 'NONE', *, *, #40589, .F. ) ;
#136415 = CARTESIAN_POINT ( 'NONE',  ( -17.99999999999986855, -19.22509904557638549, 1.855685503482138010 ) ) ;
#136416 = FACE_OUTER_BOUND ( 'NONE', #96280, .T. ) ;
#136417 = EDGE_CURVE ( 'NONE', #82894, #56980, #72704, .T. ) ;
#136418 = CARTESIAN_POINT ( 'NONE',  ( -2.292893218813441880, -12.74070752338415602, 5.000000000000000000 ) ) ;
#136419 = CARTESIAN_POINT ( 'NONE',  ( 0.4557000896773421572, 6.785346537228469366, -3.515855491508740105 ) ) ;
#136420 = FACE_OUTER_BOUND ( 'NONE', #50365, .T. ) ;
#136421 = DIRECTION ( 'NONE',  ( -0.7071067811865487940, 0.7071067811865463515, -0.000000000000000000 ) ) ;
#136422 = CARTESIAN_POINT ( 'NONE',  ( -27.70710678118635428, 14.25929247661557397, 5.000000000000000000 ) ) ;
#136423 = ADVANCED_FACE ( 'NONE', ( #117545 ), #18222, .F. ) ;
#136424 = CARTESIAN_POINT ( 'NONE',  ( 35.51669371712954870, 7.950000000000001066, -2.130196079827421318 ) ) ;
#136425 = DIRECTION ( 'NONE',  ( 0.7071067811865486830, -0.7071067811865464625, -0.000000000000000000 ) ) ;
#136426 = EDGE_LOOP ( 'NONE', ( #91071, #86461, #23813, #42996 ) ) ;
#136427 = EDGE_LOOP ( 'NONE', ( #65319, #71778, #133440, #107136 ) ) ;
#136428 = CARTESIAN_POINT ( 'NONE',  ( 40.22916666666666430, 7.950000000000001954, -2.130196079827421762 ) ) ;
#136429 = EDGE_LOOP ( 'NONE', ( #78444, #124111, #102786, #12288 ) ) ;
#136430 = VERTEX_POINT ( 'NONE', #51624 ) ;
#136431 = EDGE_CURVE ( 'NONE', #137039, #140166, #95817, .T. ) ;
#136432 = DIRECTION ( 'NONE',  ( 0.000000000000000000, 0.000000000000000000, 1.000000000000000000 ) ) ;
#136433 = VERTEX_POINT ( 'NONE', #129880 ) ;
#136434 = PLANE ( 'NONE',  #124264 ) ;
#136435 = CARTESIAN_POINT ( 'NONE',  ( -31.49999999999977973, 16.77039438581775954, 0.4657186855308451667 ) ) ;
#136436 = EDGE_CURVE ( 'NONE', #86454, #2079, #84949, .T. ) ;
#136437 = LINE ( 'NONE', #122894, #67400 ) ;
#136438 = CARTESIAN_POINT ( 'NONE',  ( 31.35459685856476497, -1.637169565754161615, 6.110000000000000320 ) ) ;
#136439 = VERTEX_POINT ( 'NONE', #74818 ) ;
#136440 = LINE ( 'NONE', #82116, #128922 ) ;
#136441 = EDGE_LOOP ( 'NONE', ( #60962, #20992, #114136, #46258, #73132, #518, #124845, #98035, #135522, #108824, #75795, #84319, #130940, #81862, #33382, #90477 ) ) ;
#136442 = DIRECTION ( 'NONE',  ( 0.7071067811865487940, -0.7071067811865463515, 0.000000000000000000 ) ) ;
#136444 = EDGE_CURVE ( 'NONE', #138815, #57169, #103442, .T. ) ;
#136443 = AXIS2_PLACEMENT_3D ( 'NONE', #128329, #139213, #117403 ) ;
#136445 = VECTOR ( 'NONE', #122842, 1000.000000000000000 ) ;
#136446 = VECTOR ( 'NONE', #50350, 1000.000000000000227 ) ;
#136447 = CARTESIAN_POINT ( 'NONE',  ( -28.49999999999981171, -4.216083040037277740, -7.486842126848595846 ) ) ;
#136448 = DIRECTION ( 'NONE',  ( 1.000000000000000000, 0.000000000000000000, 0.000000000000000000 ) ) ;
#136449 = VECTOR ( 'NONE', #58647, 1000.000000000000114 ) ;
#136450 = CARTESIAN_POINT ( 'NONE',  ( 11.29289321881337926, 14.25929247661557753, 5.000000000000000000 ) ) ;
#136451 = ORIENTED_EDGE ( 'NONE', *, *, #73143, .F. ) ;
#136452 = VERTEX_POINT ( 'NONE', #55909 ) ;
#136453 = PLANE ( 'NONE',  #130450 ) ;
#136454 = DIRECTION ( 'NONE',  ( -0.6830127018922181881, 0.6830127018922202975, -0.2588190451025214056 ) ) ;
#136455 = FACE_OUTER_BOUND ( 'NONE', #75859, .T. ) ;
#136456 = EDGE_CURVE ( 'NONE', #87783, #123521, #100111, .T. ) ;
#136457 = VECTOR ( 'NONE', #49951, 1000.000000000000000 ) ;
#136458 = CARTESIAN_POINT ( 'NONE',  ( 44.97459685856478018, 1.637169565754164058, -6.109999999999996767 ) ) ;
#136459 = DIRECTION ( 'NONE',  ( 0.000000000000000000, 0.000000000000000000, -1.000000000000000000 ) ) ;
#136460 = EDGE_CURVE ( 'NONE', #87171, #93941, #762, .T. ) ;
#136461 = DIRECTION ( 'NONE',  ( 0.6830127018922181881, 0.6830127018922202975, -0.2588190451025214056 ) ) ;
#136462 = ORIENTED_EDGE ( 'NONE', *, *, #111462, .F. ) ;
#136463 = ORIENTED_EDGE ( 'NONE', *, *, #111940, .T. ) ;
#136464 = MECHANICAL_DESIGN_GEOMETRIC_PRESENTATION_REPRESENTATION (  '', ( #13711 ), #67048 ) ;
#136465 = VECTOR ( 'NONE', #88059, 1000.000000000000227 ) ;
#136466 = CARTESIAN_POINT ( 'NONE',  ( -12.29974487139158512, -27.71228299555214747, 4.000000000000000000 ) ) ;
#136467 = EDGE_LOOP ( 'NONE', ( #95960, #64640, #40616, #36874 ) ) ;
#136468 = EDGE_CURVE ( 'NONE', #25060, #127256, #132036, .T. ) ;
#136469 = EDGE_CURVE ( 'NONE', #16022, #11025, #45756, .T. ) ;
#136470 = VECTOR ( 'NONE', #40018, 1000.000000000000000 ) ;
#136471 = DIRECTION ( 'NONE',  ( 0.6830127018922180770, -0.6830127018922204085, -0.2588190451025213501 ) ) ;
#136472 = ORIENTED_EDGE ( 'NONE', *, *, #41852, .T. ) ;
#136473 = CARTESIAN_POINT ( 'NONE',  ( 3.328169399223493308, -18.74070752338410273, 4.000000000000000000 ) ) ;
#136474 = AXIS2_PLACEMENT_3D ( 'NONE', #15361, #93685, #116131 ) ;
#136476 = EDGE_CURVE ( 'NONE', #111687, #13822, #111695, .T. ) ;
#136475 = VECTOR ( 'NONE', #139312, 1000.000000000000227 ) ;
#136478 = AXIS2_PLACEMENT_3D ( 'NONE', #30119, #74369, #8338 ) ;
#136477 = LINE ( 'NONE', #58273, #55891 ) ;
#136479 = FACE_BOUND ( 'NONE', #89275, .T. ) ;
#136480 = EDGE_CURVE ( 'NONE', #80319, #89805, #6761, .T. ) ;
#136481 = DIRECTION ( 'NONE',  ( -0.7071067811865486830, 0.7071067811865464625, 0.000000000000000000 ) ) ;
#136482 = DIRECTION ( 'NONE',  ( 1.318980745116185161E-16, -1.000000000000000000, 0.000000000000000000 ) ) ;
#136483 = CARTESIAN_POINT ( 'NONE',  ( 34.49999999999975842, 10.46425560840038571, 4.994342998332157890 ) ) ;
#136484 = FILL_AREA_STYLE_COLOUR ( '', #6331 ) ;
#136486 = ORIENTED_EDGE ( 'NONE', *, *, #20189, .T. ) ;
#136485 = CARTESIAN_POINT ( 'NONE',  ( -11.51078643762690490, -27.52281430457047406, 5.000000000000000000 ) ) ;
#136487 = AXIS2_PLACEMENT_3D ( 'NONE', #1764, #100427, #34445 ) ;
#136488 = PLANE ( 'NONE',  #41709 ) ;
#136489 = VERTEX_POINT ( 'NONE', #34866 ) ;
#136490 = VERTEX_POINT ( 'NONE', #56652 ) ;
#136491 = CARTESIAN_POINT ( 'NONE',  ( 61.59959685856478018, -6.109999999999997655, -1.637169565754160283 ) ) ;
#136492 = ORIENTED_EDGE ( 'NONE', *, *, #132412, .T. ) ;
#136493 = ADVANCED_FACE ( 'NONE', ( #54484 ), #12368, .F. ) ;
#136494 = CARTESIAN_POINT ( 'NONE',  ( 29.99451991528749417, 28.92564299267958816, 4.000000000000000000 ) ) ;
#136495 = CARTESIAN_POINT ( 'NONE',  ( 18.48921356237309510, -27.52281430457068367, 5.000000000000000000 ) ) ;
#136496 = ORIENTED_EDGE ( 'NONE', *, *, #143015, .F. ) ;
#136497 = AXIS2_PLACEMENT_3D ( 'NONE', #109124, #60115, #31582 ) ;
#136498 = ADVANCED_FACE ( 'NONE', ( #1469 ), #108802, .F. ) ;
#136499 = CARTESIAN_POINT ( 'NONE',  ( 34.24999999999998579, -9.735942053221458872E-16, 7.950000000000000178 ) ) ;
#136500 = PLANE ( 'NONE',  #106080 ) ;
#136501 = CARTESIAN_POINT ( 'NONE',  ( -12.69999999999998153, 2.143131898507868051E-16, -1.749999999999999778 ) ) ;
#136502 = FACE_OUTER_BOUND ( 'NONE', #130878, .T. ) ;
#136503 = DIRECTION ( 'NONE',  ( 0.7071067811865486830, -0.7071067811865464625, -0.000000000000000000 ) ) ;
#136504 = ORIENTED_EDGE ( 'NONE', *, *, #97915, .F. ) ;
#136505 = ORIENTED_EDGE ( 'NONE', *, *, #50286, .F. ) ;
#136506 = CARTESIAN_POINT ( 'NONE',  ( 14.39158342593605155, -0.5643469832421100785, 4.274152510792124104 ) ) ;
#136507 = DIRECTION ( 'NONE',  ( -0.000000000000000000, 0.000000000000000000, 1.000000000000000000 ) ) ;
#136508 = ORIENTED_EDGE ( 'NONE', *, *, #44245, .F. ) ;
#136509 = EDGE_LOOP ( 'NONE', ( #128858, #61143, #135192, #52641 ) ) ;
#136510 = ORIENTED_EDGE ( 'NONE', *, *, #101966, .T. ) ;
#136511 = DIRECTION ( 'NONE',  ( -0.7071067811865486830, -0.7071067811865464625, 0.000000000000000000 ) ) ;
#136512 = CARTESIAN_POINT ( 'NONE',  ( 33.18398860626899705, 28.73617430169810305, 5.000000000000000000 ) ) ;
#136513 = ORIENTED_EDGE ( 'NONE', *, *, #65488, .F. ) ;
#136514 = CARTESIAN_POINT ( 'NONE',  ( -33.79289321881321939, -20.24070752338407431, 5.000000000000000000 ) ) ;
#136515 = EDGE_CURVE ( 'NONE', #56258, #63020, #142896, .T. ) ;
#136516 = LINE ( 'NONE', #126359, #111818 ) ;
#136517 = CARTESIAN_POINT ( 'NONE',  ( 9.692069808101887674, -7.934999999999991616, -2.126176841940955242 ) ) ;
#136518 = LINE ( 'NONE', #92294, #7873 ) ;
#136519 = ORIENTED_EDGE ( 'NONE', *, *, #16107, .F. ) ;
#136520 = DIRECTION ( 'NONE',  ( -0.6830127018922181881, 0.6830127018922202975, -0.2588190451025214056 ) ) ;
#136521 = CARTESIAN_POINT ( 'NONE',  ( -17.20829011259837671, -2.505970753447624766, 4.303104124266146080 ) ) ;
#136522 = CARTESIAN_POINT ( 'NONE',  ( 24.29974487139158867, -27.71228299555223273, 4.000000000000000000 ) ) ;
#136524 = VERTEX_POINT ( 'NONE', #43578 ) ;
#136523 = DIRECTION ( 'NONE',  ( 0.000000000000000000, 1.000000000000000000, 0.000000000000000000 ) ) ;
#136525 = ORIENTED_EDGE ( 'NONE', *, *, #70857, .T. ) ;
#136526 = DIRECTION ( 'NONE',  ( 1.000000000000000000, -0.000000000000000000, 0.000000000000000000 ) ) ;
#136527 = DIRECTION ( 'NONE',  ( -0.000000000000000000, 0.000000000000000000, 1.000000000000000000 ) ) ;
#136528 = DIRECTION ( 'NONE',  ( 0.7071067811865486830, -0.7071067811865464625, -0.000000000000000000 ) ) ;
#136529 = ORIENTED_EDGE ( 'NONE', *, *, #82115, .T. ) ;
#136530 = CARTESIAN_POINT ( 'NONE',  ( 33.18398860626899705, 28.73617430169810305, 5.000000000000000000 ) ) ;
#136531 = CARTESIAN_POINT ( 'NONE',  ( -21.48921356237309155, -27.52281430457070499, 5.000000000000000000 ) ) ;
#136532 = CARTESIAN_POINT ( 'NONE',  ( 29.99999999999979039, -21.03360074219752462, 5.000000000000000000 ) ) ;
#136533 = FACE_OUTER_BOUND ( 'NONE', #34330, .T. ) ;
#136534 = CARTESIAN_POINT ( 'NONE',  ( 69.48921356237309510, -27.52281430457103895, 5.000000000000000000 ) ) ;
#136535 = VECTOR ( 'NONE', #12554, 1000.000000000000000 ) ;
#136536 = EDGE_LOOP ( 'NONE', ( #39299, #83992, #3687, #77206 ) ) ;
#136537 = AXIS2_PLACEMENT_3D ( 'NONE', #82, #56702, #24030 ) ;
#136538 = VECTOR ( 'NONE', #101243, 1000.000000000000000 ) ;
#136539 = AXIS2_PLACEMENT_3D ( 'NONE', #80584, #1537, #89995 ) ;
#136540 = CARTESIAN_POINT ( 'NONE',  ( -4.410090645198292414, 9.759292476615618384, 11.28811694763777851 ) ) ;
#136541 = DIRECTION ( 'NONE',  ( -0.000000000000000000, 1.000000000000000000, -0.000000000000000000 ) ) ;
#136542 = CARTESIAN_POINT ( 'NONE',  ( 8.999999999999944933, -3.412538124160723108, 4.000000000000000000 ) ) ;
#136543 = CIRCLE ( 'NONE', #94817, 6.499999999999999112 ) ;
#136544 = LINE ( 'NONE', #23508, #47436 ) ;
#136545 = LINE ( 'NONE', #38680, #101626 ) ;
#136546 = ORIENTED_EDGE ( 'NONE', *, *, #72059, .F. ) ;
#136547 = VERTEX_POINT ( 'NONE', #53767 ) ;
#136548 = CARTESIAN_POINT ( 'NONE',  ( 9.183988606268997046, 28.73617430169793607, 5.000000000000000000 ) ) ;
#136549 = AXIS2_PLACEMENT_3D ( 'NONE', #58560, #36738, #80978 ) ;
#136550 = CARTESIAN_POINT ( 'NONE',  ( 8.874569808101886892, 6.871911579029510442, -3.967499999999998916 ) ) ;
#136551 = LINE ( 'NONE', #47470, #20463 ) ;
#136552 = VECTOR ( 'NONE', #4923, 1000.000000000000114 ) ;
#136553 = CARTESIAN_POINT ( 'NONE',  ( -7.140000000000001457, -35.14999999999999147, 17.49210858042621908 ) ) ;
#136554 = DIRECTION ( 'NONE',  ( -0.7071067811865487940, 0.7071067811865463515, 0.000000000000000000 ) ) ;
#136555 = CARTESIAN_POINT ( 'NONE',  ( 14.81601139373099585, 28.73617430169776910, 5.000000000000000000 ) ) ;
#136556 = ORIENTED_EDGE ( 'NONE', *, *, #39137, .T. ) ;
#136557 = LINE ( 'NONE', #135182, #25650 ) ;
#136558 = EDGE_CURVE ( 'NONE', #118125, #100624, #87795, .T. ) ;
#136559 = DIRECTION ( 'NONE',  ( -0.7071067811865486830, -0.7071067811865464625, 0.000000000000000000 ) ) ;
#136560 = VECTOR ( 'NONE', #56765, 1000.000000000000000 ) ;
#136561 = CYLINDRICAL_SURFACE ( 'NONE', #96733, 3.000000000000000000 ) ;
#136562 = CARTESIAN_POINT ( 'NONE',  ( 46.43293019189811588, 1.637169565754156730, 6.110000000000001208 ) ) ;
#136563 = CARTESIAN_POINT ( 'NONE',  ( 183.9346320274809443, -51.67626207039722175, -38.40320453011149482 ) ) ;
#136564 = VECTOR ( 'NONE', #75837, 1000.000000000000227 ) ;
#136565 = ORIENTED_EDGE ( 'NONE', *, *, #23573, .F. ) ;
#136566 = FACE_OUTER_BOUND ( 'NONE', #835, .T. ) ;
#136567 = VERTEX_POINT ( 'NONE', #142206 ) ;
#136568 = CARTESIAN_POINT ( 'NONE',  ( 19.49999999999986144, -20.53675388469228835, 2.352720554255939511 ) ) ;
#136569 = ADVANCED_FACE ( 'NONE', ( #42895 ), #89234, .F. ) ;
#136570 = ORIENTED_EDGE ( 'NONE', *, *, #90195, .F. ) ;
#136571 = CARTESIAN_POINT ( 'NONE',  ( 14.99999999999989875, -4.068876922607767455, 4.000000000000000000 ) ) ;
#136572 = VECTOR ( 'NONE', #91348, 1000.000000000000000 ) ;
#136573 = CARTESIAN_POINT ( 'NONE',  ( 23.99451991528749062, 28.92564299267954908, 4.000000000000000000 ) ) ;
#136574 = CARTESIAN_POINT ( 'NONE',  ( -5.207106781186511490, 18.75929247661552779, 5.000000000000000000 ) ) ;
#136575 = EDGE_CURVE ( 'NONE', #97535, #89442, #21830, .T. ) ;
#136576 = CARTESIAN_POINT ( 'NONE',  ( -14.51078643762690490, -27.52281430457045275, 5.000000000000000000 ) ) ;
#136577 = DIRECTION ( 'NONE',  ( -0.7071067811865486830, -0.7071067811865464625, 0.000000000000000000 ) ) ;
#136578 =( NAMED_UNIT ( * ) PLANE_ANGLE_UNIT ( ) SI_UNIT ( $, .RADIAN. ) );
#136579 = EDGE_CURVE ( 'NONE', #73550, #30286, #65368, .T. ) ;
#136580 = EDGE_CURVE ( 'NONE', #56496, #113570, #10918, .T. ) ;
#136581 = AXIS2_PLACEMENT_3D ( 'NONE', #57377, #67544, #55219 ) ;
#136582 = ORIENTED_EDGE ( 'NONE', *, *, #93868, .F. ) ;
#136583 = CARTESIAN_POINT ( 'NONE',  ( 26.81601139373100651, 28.73617430169768738, 5.000000000000000000 ) ) ;
#136584 = DIRECTION ( 'NONE',  ( -1.000000000000000000, -1.224606353822377258E-16, -0.000000000000000000 ) ) ;
#136585 = VECTOR ( 'NONE', #14304, 1000.000000000000000 ) ;
#136586 = FACE_OUTER_BOUND ( 'NONE', #113305, .T. ) ;
#136587 = CARTESIAN_POINT ( 'NONE',  ( -48.29974487139158867, -27.71228299555239971, 4.000000000000000000 ) ) ;
#136588 = EDGE_CURVE ( 'NONE', #95640, #111746, #25, .T. ) ;
#136590 = ADVANCED_FACE ( 'NONE', ( #33460 ), #22507, .T. ) ;
#136589 = CARTESIAN_POINT ( 'NONE',  ( 79.26669371712955581, -7.949999999999999289, 2.130196079827424427 ) ) ;
#136591 = DIRECTION ( 'NONE',  ( -0.7071067811865486830, -0.7071067811865464625, -0.000000000000000000 ) ) ;
#136592 = VECTOR ( 'NONE', #98855, 1000.000000000000000 ) ;
#136593 = ORIENTED_EDGE ( 'NONE', *, *, #2735, .T. ) ;
#136594 = ORIENTED_EDGE ( 'NONE', *, *, #20794, .F. ) ;
#136595 = CARTESIAN_POINT ( 'NONE',  ( 60.79166666666665719, 3.975000000000003642, -6.884901960086285300 ) ) ;
#136596 = CARTESIAN_POINT ( 'NONE',  ( 0.000000000000000000, 0.000000000000000000, 5.000000000000000000 ) ) ;
#136597 = ADVANCED_FACE ( 'NONE', ( #36284 ), #93511, .F. ) ;
#136598 = CARTESIAN_POINT ( 'NONE',  ( -34.92500000000001137, 22.22500000000000142, 4.000000000000000000 ) ) ;
#136599 = DIRECTION ( 'NONE',  ( 0.000000000000000000, 0.000000000000000000, 1.000000000000000000 ) ) ;
#136600 = VECTOR ( 'NONE', #106066, 1000.000000000000227 ) ;
#136601 = EDGE_LOOP ( 'NONE', ( #58662, #52276, #134792, #89730 ) ) ;
#136602 = CARTESIAN_POINT ( 'NONE',  ( -13.00193056682089043, -22.22500000000000142, 4.500000000000000888 ) ) ;
#136603 = EDGE_CURVE ( 'NONE', #49880, #111254, #113105, .T. ) ;
#136604 = LINE ( 'NONE', #126439, #44349 ) ;
#136605 = CARTESIAN_POINT ( 'NONE',  ( 54.83376352523143282, 6.110000000000001208, 1.122388791418549305E-15 ) ) ;
#136606 = FACE_OUTER_BOUND ( 'NONE', #63062, .T. ) ;
#136607 = VERTEX_POINT ( 'NONE', #92066 ) ;
#136608 = ORIENTED_EDGE ( 'NONE', *, *, #53589, .F. ) ;
#136609 = VECTOR ( 'NONE', #54538, 1000.000000000000000 ) ;
#136610 = PRESENTATION_STYLE_ASSIGNMENT (( #23766 ) ) ;
#136611 = DIRECTION ( 'NONE',  ( 0.000000000000000000, 2.242629915582283412E-16, -1.000000000000000000 ) ) ;
#136612 = CARTESIAN_POINT ( 'NONE',  ( 0.000000000000000000, 0.000000000000000000, 5.000000000000000000 ) ) ;
#136613 = DIRECTION ( 'NONE',  ( 0.000000000000000000, 1.687538997430237626E-14, 1.000000000000000000 ) ) ;
#136614 = PLANE ( 'NONE',  #141450 ) ;
#136616 = ORIENTED_EDGE ( 'NONE', *, *, #91906, .T. ) ;
#136615 = DIRECTION ( 'NONE',  ( -0.7071067811865486830, -0.7071067811865464625, 0.000000000000000000 ) ) ;
#136617 = LINE ( 'NONE', #72135, #73886 ) ;
#136618 = CARTESIAN_POINT ( 'NONE',  ( 16.49999999999988276, -16.91253812416058722, 4.000000000000000000 ) ) ;
#136619 = DIRECTION ( 'NONE',  ( 0.7071067811865486830, -0.7071067811865464625, -0.000000000000000000 ) ) ;
#136620 = EDGE_CURVE ( 'NONE', #84665, #11791, #102969, .T. ) ;
#136621 = VECTOR ( 'NONE', #71522, 1000.000000000000000 ) ;
#136622 = CARTESIAN_POINT ( 'NONE',  ( -22.49999999999983302, -5.947814304570768762, 5.000000000000000000 ) ) ;
#136623 = VECTOR ( 'NONE', #102342, 1000.000000000000227 ) ;
#136624 = ORIENTED_EDGE ( 'NONE', *, *, #9920, .F. ) ;
#136625 = ORIENTED_EDGE ( 'NONE', *, *, #8312, .F. ) ;
#136626 = SURFACE_SIDE_STYLE ('',( #72866 ) ) ;
#136627 = DIRECTION ( 'NONE',  ( 0.3543493200069162685, -0.000000000000000000, -0.9351131265310288487 ) ) ;
#136628 = CARTESIAN_POINT ( 'NONE',  ( -34.49999999999976552, -4.796895815301057908, -3.611700055028757461 ) ) ;
#136629 = ADVANCED_FACE ( 'NONE', ( #15898 ), #40960, .T. ) ;
#136630 = FACE_OUTER_BOUND ( 'NONE', #13402, .T. ) ;
#136631 = CARTESIAN_POINT ( 'NONE',  ( 71.68336038379621300, -2.130196079827426203, 7.949999999999996625 ) ) ;
#136632 = ORIENTED_EDGE ( 'NONE', *, *, #137614, .F. ) ;
#136633 = ORIENTED_EDGE ( 'NONE', *, *, #52022, .F. ) ;
#136634 = DIRECTION ( 'NONE',  ( -0.000000000000000000, 0.000000000000000000, 1.000000000000000000 ) ) ;
#136635 = PLANE ( 'NONE',  #9769 ) ;
#136636 = ADVANCED_FACE ( 'NONE', ( #123308 ), #124007, .F. ) ;
#136638 = ORIENTED_EDGE ( 'NONE', *, *, #140873, .T. ) ;
#136637 = VECTOR ( 'NONE', #70946, 999.9999999999998863 ) ;
#136639 = DIRECTION ( 'NONE',  ( -1.000000000000000000, 0.000000000000000000, 0.000000000000000000 ) ) ;
#136641 = EDGE_CURVE ( 'NONE', #3062, #66852, #21643, .T. ) ;
#136640 = ORIENTED_EDGE ( 'NONE', *, *, #91099, .T. ) ;
#136642 = DIRECTION ( 'NONE',  ( 1.000000000000000000, 1.224606353822377258E-16, 0.000000000000000000 ) ) ;
#136643 = DIRECTION ( 'NONE',  ( 0.7071067811865487940, 0.7071067811865463515, 0.000000000000000000 ) ) ;
#136644 = VECTOR ( 'NONE', #102857, 1000.000000000000114 ) ;
#136645 = VECTOR ( 'NONE', #90768, 1000.000000000000000 ) ;
#136646 = VECTOR ( 'NONE', #35504, 999.9999999999998863 ) ;
#136647 = EDGE_CURVE ( 'NONE', #9288, #10232, #81961, .T. ) ;
#136648 = AXIS2_PLACEMENT_3D ( 'NONE', #17912, #95500, #96899 ) ;
#136649 = FACE_BOUND ( 'NONE', #75684, .T. ) ;
#136650 = PLANE ( 'NONE',  #22369 ) ;
#136651 = CARTESIAN_POINT ( 'NONE',  ( 3.717577386425651387, -21.73023691814492153, 5.000000000000000000 ) ) ;
#136652 = LINE ( 'NONE', #74829, #20430 ) ;
#136653 = VECTOR ( 'NONE', #4238, 1000.000000000000227 ) ;
#136654 = CARTESIAN_POINT ( 'NONE',  ( -45.48921356237309510, -27.52281430457087197, 5.000000000000000000 ) ) ;
#136655 = EDGE_CURVE ( 'NONE', #52944, #92199, #54843, .T. ) ;
#136656 = DIRECTION ( 'NONE',  ( 0.7071067811865487940, 0.7071067811865463515, -0.000000000000000000 ) ) ;
#136657 = PRODUCT_CONTEXT ( 'NONE', #35596, 'mechanical' ) ;
#136658 = ORIENTED_EDGE ( 'NONE', *, *, #19049, .T. ) ;
#136659 = ORIENTED_EDGE ( 'NONE', *, *, #86915, .T. ) ;
#136660 = CARTESIAN_POINT ( 'NONE',  ( 93.39126352523143737, -4.472830434245838482, -4.472830434245838482 ) ) ;
#136661 = ORIENTED_EDGE ( 'NONE', *, *, #69180, .F. ) ;
#136662 = EDGE_CURVE ( 'NONE', #137138, #77634, #48579, .T. ) ;
#136663 = CARTESIAN_POINT ( 'NONE',  ( 184.1499999999998067, -43.14999999999999147, 34.92499999999998295 ) ) ;
#136664 = VECTOR ( 'NONE', #31733, 1000.000000000000000 ) ;
#136665 = PLANE ( 'NONE',  #9921 ) ;
#136666 = AXIS2_PLACEMENT_3D ( 'NONE', #60529, #62648, #51056 ) ;
#136667 = CARTESIAN_POINT ( 'NONE',  ( 15.18398860626900237, 28.73617430169797871, 5.000000000000000000 ) ) ;
#136668 = ORIENTED_EDGE ( 'NONE', *, *, #16040, .T. ) ;
#136669 = DIRECTION ( 'NONE',  ( -1.000000000000000000, -1.224606353822377258E-16, -0.000000000000000000 ) ) ;
#136670 = AXIS2_PLACEMENT_3D ( 'NONE', #43606, #77686, #109577 ) ;
#136671 = DIRECTION ( 'NONE',  ( 1.000000000000000000, 0.000000000000000000, 0.000000000000000000 ) ) ;
#136672 = DIRECTION ( 'NONE',  ( -0.000000000000000000, 0.3543493200069153248, 0.9351131265310292928 ) ) ;
#136674 = DIRECTION ( 'NONE',  ( 0.7071067811865487940, 0.7071067811865463515, 0.000000000000000000 ) ) ;
#136673 = CARTESIAN_POINT ( 'NONE',  ( -3.005480084712505828, 28.92564299267936079, 4.000000000000000000 ) ) ;
#136675 = VECTOR ( 'NONE', #120710, 1000.000000000000000 ) ;
#136676 = CARTESIAN_POINT ( 'NONE',  ( -34.49999999999976552, 3.653845994658358354, -4.504631822206292213 ) ) ;
#136677 = DIRECTION ( 'NONE',  ( -1.000000000000000000, 0.000000000000000000, 0.000000000000000000 ) ) ;
#136678 = ORIENTED_EDGE ( 'NONE', *, *, #121287, .T. ) ;
#136679 = CIRCLE ( 'NONE', #74194, 5.968999999999998529 ) ;
#136680 = FACE_OUTER_BOUND ( 'NONE', #123123, .T. ) ;
#136681 = DIRECTION ( 'NONE',  ( -0.7071067811865487940, 0.7071067811865463515, 0.000000000000000000 ) ) ;
#136682 = ORIENTED_EDGE ( 'NONE', *, *, #67435, .T. ) ;
#136683 = EDGE_CURVE ( 'NONE', #12215, #114108, #13069, .T. ) ;
#136684 = ORIENTED_EDGE ( 'NONE', *, *, #4728, .T. ) ;
#136685 =( GEOMETRIC_REPRESENTATION_CONTEXT ( 3 ) GLOBAL_UNCERTAINTY_ASSIGNED_CONTEXT ( ( #92356 ) ) GLOBAL_UNIT_ASSIGNED_CONTEXT ( ( #54916, #121569, #10649 ) ) REPRESENTATION_CONTEXT ( 'NONE', 'WORKASPACE' ) );
#136686 = ORIENTED_EDGE ( 'NONE', *, *, #3276, .T. ) ;
#136687 = CARTESIAN_POINT ( 'NONE',  ( 42.43793019189809712, -6.110000000000001208, 1.637169565754158951 ) ) ;
#136688 = ORIENTED_EDGE ( 'NONE', *, *, #599, .T. ) ;
#136689 = VECTOR ( 'NONE', #124279, 1000.000000000000000 ) ;
#136690 = CARTESIAN_POINT ( 'NONE',  ( 9.670806282870438864, -3.047499999999997211, -5.278424836066143655 ) ) ;
#136691 = CARTESIAN_POINT ( 'NONE',  ( -12.82211510476379956, 6.989083614815657874, -30.85058313491061099 ) ) ;
#136692 = ORIENTED_EDGE ( 'NONE', *, *, #74796, .T. ) ;
#136693 = DIRECTION ( 'NONE',  ( -0.7071067811865486830, -0.7071067811865464625, 0.000000000000000000 ) ) ;
#136694 = VERTEX_POINT ( 'NONE', #47898 ) ;
#136695 = CARTESIAN_POINT ( 'NONE',  ( 24.09999999999999787, -2.055000000000000160, 0.000000000000000000 ) ) ;
#136696 = DIRECTION ( 'NONE',  ( -0.6830127018922181881, 0.6830127018922202975, -0.2588190451025214056 ) ) ;
#136698 = VERTEX_POINT ( 'NONE', #101518 ) ;
#136697 = CARTESIAN_POINT ( 'NONE',  ( 44.99451991528749772, 28.92564299267969474, 4.000000000000000000 ) ) ;
#136699 = ORIENTED_EDGE ( 'NONE', *, *, #138991, .F. ) ;
#136700 = EDGE_CURVE ( 'NONE', #137194, #871, #24673, .T. ) ;
#136701 = CARTESIAN_POINT ( 'NONE',  ( 24.41159235450331977, 9.902892378096218942E-16, 0.000000000000000000 ) ) ;
#136702 = LINE ( 'NONE', #37406, #20579 ) ;
#136703 = EDGE_LOOP ( 'NONE', ( #65555, #107113, #140558, #10945 ) ) ;
#136704 = EDGE_CURVE ( 'NONE', #80143, #139533, #4282, .T. ) ;
#136705 = DIRECTION ( 'NONE',  ( -0.7071067811865486830, 0.7071067811865464625, 0.000000000000000000 ) ) ;
#136706 = ORIENTED_EDGE ( 'NONE', *, *, #96818, .F. ) ;
#136707 = ORIENTED_EDGE ( 'NONE', *, *, #13906, .F. ) ;
#136708 = EDGE_LOOP ( 'NONE', ( #90491, #93989, #4196, #99776, #22652, #104803 ) ) ;
#136709 = VERTEX_POINT ( 'NONE', #68932 ) ;
#136710 = DIRECTION ( 'NONE',  ( 0.3543493200069162685, -0.000000000000000000, -0.9351131265310288487 ) ) ;
#136711 = VECTOR ( 'NONE', #58857, 1000.000000000000000 ) ;
#136712 = FACE_BOUND ( 'NONE', #8644, .T. ) ;
#136713 = CARTESIAN_POINT ( 'NONE',  ( -7.033400323430184287, 6.759292476615645917, 12.28218704918520565 ) ) ;
#136714 = DIRECTION ( 'NONE',  ( -0.7071067811865486830, -0.7071067811865464625, 0.000000000000000000 ) ) ;
#136715 = ADVANCED_FACE ( 'NONE', ( #60185 ), #3606, .F. ) ;
#136716 = LINE ( 'NONE', #101237, #120540 ) ;
#136717 = ORIENTED_EDGE ( 'NONE', *, *, #98226, .T. ) ;
#136718 = AXIS2_PLACEMENT_3D ( 'NONE', #138027, #61912, #135881 ) ;
#136719 = CARTESIAN_POINT ( 'NONE',  ( 0.000000000000000000, 0.000000000000000000, 5.000000000000000000 ) ) ;
#136720 = CARTESIAN_POINT ( 'NONE',  ( 19.22873647476855652, 5.808823158059031044, -5.808823158059038150 ) ) ;
#136721 = DIRECTION ( 'NONE',  ( 0.7071067811865486830, -0.7071067811865464625, -0.000000000000000000 ) ) ;
#136722 = DIRECTION ( 'NONE',  ( -1.000000000000000000, -1.224606353822377258E-16, -0.000000000000000000 ) ) ;
#136723 = LINE ( 'NONE', #105515, #116145 ) ;
#136724 = EDGE_LOOP ( 'NONE', ( #30332, #107912, #127646, #68241 ) ) ;
#136725 = ORIENTED_EDGE ( 'NONE', *, *, #77518, .F. ) ;
#136726 = ORIENTED_EDGE ( 'NONE', *, *, #112682, .F. ) ;
#136727 = FILL_AREA_STYLE_COLOUR ( '', #30204 ) ;
#136728 = DIRECTION ( 'NONE',  ( -0.7071067811865486830, -0.7071067811865464625, -0.000000000000000000 ) ) ;
#136729 = FACE_OUTER_BOUND ( 'NONE', #110085, .T. ) ;
#136730 = DIRECTION ( 'NONE',  ( 0.000000000000000000, 0.000000000000000000, 1.000000000000000000 ) ) ;
#136731 = AXIS2_PLACEMENT_3D ( 'NONE', #125502, #101582, #67575 ) ;
#136732 = CARTESIAN_POINT ( 'NONE',  ( -6.183988606268994381, 28.73617430169791476, 5.000000000000000000 ) ) ;
#136733 = CARTESIAN_POINT ( 'NONE',  ( 7.430803446455462868, 8.913522578092118565, 3.292921844800691389 ) ) ;
#136734 = LINE ( 'NONE', #37451, #39542 ) ;
#136735 = AXIS2_PLACEMENT_3D ( 'NONE', #53948, #62665, #18395 ) ;
#136736 = CARTESIAN_POINT ( 'NONE',  ( 29.67183060077626422, -12.74070752338415247, 4.000000000000000000 ) ) ;
#136737 = CARTESIAN_POINT ( 'NONE',  ( 32.99999999999977973, 2.966399257802230682, 5.000000000000000000 ) ) ;
#136738 = CARTESIAN_POINT ( 'NONE',  ( 12.78162688292485782, 21.74787736706806385, 4.999607392498048419 ) ) ;
#136739 = DIRECTION ( 'NONE',  ( 0.000000000000000000, 1.000000000000000000, 0.000000000000000000 ) ) ;
#136740 = VERTEX_POINT ( 'NONE', #91393 ) ;
#136741 = VECTOR ( 'NONE', #100196, 1000.000000000000000 ) ;
#136742 = VECTOR ( 'NONE', #74534, 1000.000000000000227 ) ;
#136744 = DIRECTION ( 'NONE',  ( 0.6830127018922181881, 0.6830127018922202975, -0.2588190451025214056 ) ) ;
#136743 = AXIS2_PLACEMENT_3D ( 'NONE', #109820, #106384, #51352 ) ;
#136745 = ORIENTED_EDGE ( 'NONE', *, *, #110942, .F. ) ;
#136746 = VECTOR ( 'NONE', #109055, 1000.000000000000227 ) ;
#136747 = LINE ( 'NONE', #125899, #85346 ) ;
#136749 = VERTEX_POINT ( 'NONE', #36974 ) ;
#136748 = DIRECTION ( 'NONE',  ( -0.3543493200069162685, -0.000000000000000000, -0.9351131265310288487 ) ) ;
#136750 = CARTESIAN_POINT ( 'NONE',  ( 34.17183060077623225, 9.759292476615620160, 4.000000000000000000 ) ) ;
#136751 = FACE_OUTER_BOUND ( 'NONE', #34281, .T. ) ;
#136752 = EDGE_CURVE ( 'NONE', #138807, #14297, #137016, .T. ) ;
#136753 = EDGE_LOOP ( 'NONE', ( #52256, #88430, #45561 ) ) ;
#136754 = LINE ( 'NONE', #36050, #134109 ) ;
#136755 = ORIENTED_EDGE ( 'NONE', *, *, #119227, .T. ) ;
#136756 = VECTOR ( 'NONE', #137522, 1000.000000000000227 ) ;
#136757 = ORIENTED_EDGE ( 'NONE', *, *, #106663, .F. ) ;
#136758 = CARTESIAN_POINT ( 'NONE',  ( -62.99451991528749772, 28.92564299267982264, 4.000000000000000000 ) ) ;
#136759 = EDGE_CURVE ( 'NONE', #81264, #7112, #37721, .T. ) ;
#136760 = EDGE_CURVE ( 'NONE', #60766, #127270, #71069, .T. ) ;
#136762 = EDGE_CURVE ( 'NONE', #70580, #55207, #71777, .T. ) ;
#136761 = CARTESIAN_POINT ( 'NONE',  ( 100.9958603837962272, -3.974999999999998312, -6.884901960086286188 ) ) ;
#136763 = DIRECTION ( 'NONE',  ( 1.000000000000000000, 0.000000000000000000, 0.000000000000000000 ) ) ;
#136764 = CARTESIAN_POINT ( 'NONE',  ( 10.06000000000000050, 2.055000000000001492, 2.516649172247811554E-16 ) ) ;
#136766 = EDGE_CURVE ( 'NONE', #20476, #83916, #78365, .T. ) ;
#136765 = ORIENTED_EDGE ( 'NONE', *, *, #92476, .T. ) ;
#136767 = VECTOR ( 'NONE', #88544, 1000.000000000000000 ) ;
#136768 = LINE ( 'NONE', #103411, #123386 ) ;
#136769 = DIRECTION ( 'NONE',  ( 0.3543493200069162685, -0.000000000000000000, -0.9351131265310288487 ) ) ;
#136770 = EDGE_CURVE ( 'NONE', #104374, #16647, #7171, .T. ) ;
#136771 = DIRECTION ( 'NONE',  ( 0.3543493200069162685, -0.000000000000000000, -0.9351131265310288487 ) ) ;
#136772 = CARTESIAN_POINT ( 'NONE',  ( 22.02083333333333925, -6.094999999999989981, -1.633150327867689100 ) ) ;
#136774 = AXIS2_PLACEMENT_3D ( 'NONE', #80100, #46034, #123604 ) ;
#136773 = CARTESIAN_POINT ( 'NONE',  ( -15.21590231913187452, -1.409216073889146381, 4.328383627671533063 ) ) ;
#136775 = LINE ( 'NONE', #70838, #90663 ) ;
#136776 = ADVANCED_FACE ( 'NONE', ( #73901 ), #107915, .F. ) ;
#136777 = VERTEX_POINT ( 'NONE', #28972 ) ;
#136778 = AXIS2_PLACEMENT_3D ( 'NONE', #20570, #62686, #38248 ) ;
#136779 = DIRECTION ( 'NONE',  ( -0.6830127018922181881, 0.6830127018922202975, -0.2588190451025214056 ) ) ;
#136781 = EDGE_LOOP ( 'NONE', ( #24222, #84482, #139254, #101969 ) ) ;
#136780 = ADVANCED_FACE ( 'NONE', ( #83355 ), #84943, .T. ) ;
#136782 = VECTOR ( 'NONE', #62650, 1000.000000000000000 ) ;
#136783 = CARTESIAN_POINT ( 'NONE',  ( 81.08376352523144703, -6.110000000000001208, -3.741295971395164515E-16 ) ) ;
#136784 = VECTOR ( 'NONE', #68359, 999.9999999999998863 ) ;
#136785 = CARTESIAN_POINT ( 'NONE',  ( 5.510786437626906675, -27.52281430457051314, 5.000000000000000000 ) ) ;
#136786 = PLANE ( 'NONE',  #94741 ) ;
#136787 = CARTESIAN_POINT ( 'NONE',  ( -20.99999999999985079, 16.55218569542900298, 5.000000000000000000 ) ) ;
#136788 = CARTESIAN_POINT ( 'NONE',  ( -33.18398860626899705, 28.73617430169810305, 5.000000000000000000 ) ) ;
#136789 = ORIENTED_EDGE ( 'NONE', *, *, #2054, .T. ) ;
#136790 = AXIS2_PLACEMENT_3D ( 'NONE', #139294, #19619, #84881 ) ;
#136791 = CARTESIAN_POINT ( 'NONE',  ( 0.4644479527036028954, -0.4000000000000004108, 2.317232259782045389 ) ) ;
#136792 = EDGE_CURVE ( 'NONE', #48205, #111455, #40575, .T. ) ;
#136793 = CARTESIAN_POINT ( 'NONE',  ( 5.999999999999967137, 4.931123077392134846, 4.000000000000000000 ) ) ;
#136794 = VERTEX_POINT ( 'NONE', #96320 ) ;
#136795 = CARTESIAN_POINT ( 'NONE',  ( 4.171830600776437414, -20.24070752338407431, 4.000000000000000000 ) ) ;
#136796 = COLOUR_RGB ( '', 0.72549020, 0.75294118, 0.79215686) ;
#136798 = VERTEX_POINT ( 'NONE', #127567 ) ;
#136797 = LINE ( 'NONE', #112903, #59089 ) ;
#136799 = CARTESIAN_POINT ( 'NONE',  ( -48.29974487139158867, -27.71228299555239971, 4.000000000000000000 ) ) ;
#136800 = CARTESIAN_POINT ( 'NONE',  ( -20.29298673570681544, -21.74070752338406720, 4.999753212805217117 ) ) ;
#136801 = CARTESIAN_POINT ( 'NONE',  ( -22.49999999999984013, -7.912538124160678699, 4.000000000000000000 ) ) ;
#136802 = EDGE_CURVE ( 'NONE', #68809, #17816, #39872, .T. ) ;
#136803 = CARTESIAN_POINT ( 'NONE',  ( 0.000000000000000000, 0.000000000000000000, 0.000000000000000000 ) ) ;
#136804 = ORIENTED_EDGE ( 'NONE', *, *, #51537, .F. ) ;
#136805 = EDGE_LOOP ( 'NONE', ( #45810, #110573, #135954 ) ) ;
#136806 = ORIENTED_EDGE ( 'NONE', *, *, #20544, .T. ) ;
#136807 = CARTESIAN_POINT ( 'NONE',  ( 86.62543019189811844, 5.291415217122919401, 3.055000000000002824 ) ) ;
#136808 = VECTOR ( 'NONE', #81783, 1000.000000000000227 ) ;
#136809 = ORIENTED_EDGE ( 'NONE', *, *, #32197, .F. ) ;
#136810 = PLANE ( 'NONE',  #98379 ) ;
#136811 = LINE ( 'NONE', #126630, #138280 ) ;
#136812 = AXIS2_PLACEMENT_3D ( 'NONE', #128769, #49818, #16412 ) ;
#136813 = DIRECTION ( 'NONE',  ( -0.000000000000000000, 0.3543493200069153248, 0.9351131265310292928 ) ) ;
#136814 = CYLINDRICAL_SURFACE ( 'NONE', #43143, 0.5000000000000005551 ) ;
#136815 = ORIENTED_EDGE ( 'NONE', *, *, #129966, .T. ) ;
#136816 = CARTESIAN_POINT ( 'NONE',  ( 103.8125000000000000, 5.819803920172571310, 5.819803920172576639 ) ) ;
#136817 = LINE ( 'NONE', #37528, #53679 ) ;
#136818 = CARTESIAN_POINT ( 'NONE',  ( 76.47459685856476597, 1.637169565754164058, -6.109999999999996767 ) ) ;
#136819 = EDGE_LOOP ( 'NONE', ( #113324, #95761, #32850, #74093 ) ) ;
#136820 = LINE ( 'NONE', #136106, #30401 ) ;
#136821 = EDGE_CURVE ( 'NONE', #28133, #64959, #5756, .T. ) ;
#136822 = CARTESIAN_POINT ( 'NONE',  ( 52.26932219902319332, -49.14999999999999147, -40.92499999999998295 ) ) ;
#136823 = CARTESIAN_POINT ( 'NONE',  ( 0.000000000000000000, 0.000000000000000000, 5.000000000000000000 ) ) ;
#136824 = VECTOR ( 'NONE', #125130, 1000.000000000000000 ) ;
#136825 = VERTEX_POINT ( 'NONE', #94209 ) ;
#136826 = ORIENTED_EDGE ( 'NONE', *, *, #121931, .F. ) ;
#136827 = PLANE ( 'NONE',  #83999 ) ;
#136828 = LINE ( 'NONE', #126650, #105674 ) ;
#136829 = CARTESIAN_POINT ( 'NONE',  ( 11.99999999999990230, 2.587461875839226710, 4.000000000000000000 ) ) ;
#136830 = AXIS2_PLACEMENT_3D ( 'NONE', #29787, #52962, #61745 ) ;
#136831 = LINE ( 'NONE', #60008, #27074 ) ;
#136832 = ADVANCED_FACE ( 'NONE', ( #128293 ), #61626, .F. ) ;
#136833 = CARTESIAN_POINT ( 'NONE',  ( 36.18398860626899705, 28.73617430169812437, 5.000000000000000000 ) ) ;
#136834 = CARTESIAN_POINT ( 'NONE',  ( -5.999999999999954703, 1.552185695429154633, 5.000000000000000000 ) ) ;
#136835 = EDGE_LOOP ( 'NONE', ( #90661, #121589, #11347, #108510, #83576 ) ) ;
#136836 = ORIENTED_EDGE ( 'NONE', *, *, #38363, .T. ) ;
#136837 = CARTESIAN_POINT ( 'NONE',  ( 10.50000000000000000, 0.000000000000000000, 6.094999999999989981 ) ) ;
#136838 = EDGE_CURVE ( 'NONE', #101323, #24388, #107228, .T. ) ;
#136839 = ORIENTED_EDGE ( 'NONE', *, *, #69966, .T. ) ;
#136840 = VECTOR ( 'NONE', #29722, 1000.000000000000000 ) ;
#136841 = VECTOR ( 'NONE', #15369, 1000.000000000000000 ) ;
#136842 = DIRECTION ( 'NONE',  ( -0.000000000000000000, 0.3543493200069153248, 0.9351131265310292928 ) ) ;
#136843 = EDGE_LOOP ( 'NONE', ( #138571, #89723, #1273, #119935 ) ) ;
#136844 = CYLINDRICAL_SURFACE ( 'NONE', #76023, 1.000000000000000888 ) ;
#136845 = DIRECTION ( 'NONE',  ( 0.6830127018922180770, -0.6830127018922204085, -0.2588190451025213501 ) ) ;
#136846 = EDGE_CURVE ( 'NONE', #110710, #40937, #118820, .T. ) ;
#136847 = CARTESIAN_POINT ( 'NONE',  ( -0.7928932188134494297, 9.759292476615621936, 5.000000000000000000 ) ) ;
#136848 = PRESENTATION_LAYER_ASSIGNMENT (  '', '', ( #92867 ) ) ;
#136849 = AXIS2_PLACEMENT_3D ( 'NONE', #77076, #129999, #19795 ) ;
#136850 = VECTOR ( 'NONE', #141388, 1000.000000000000000 ) ;
#136851 = VECTOR ( 'NONE', #64421, 1000.000000000000000 ) ;
#136852 = LINE ( 'NONE', #92616, #88473 ) ;
#136853 = ORIENTED_EDGE ( 'NONE', *, *, #57587, .T. ) ;
#136854 = VECTOR ( 'NONE', #75576, 1000.000000000000000 ) ;
#136855 = CARTESIAN_POINT ( 'NONE',  ( 33.75860074219772855, 21.72500000000000142, 5.000000000000000000 ) ) ;
#136856 = CARTESIAN_POINT ( 'NONE',  ( 4.911592354503321545, 9.902892378096218942E-16, 0.000000000000000000 ) ) ;
#136857 = ORIENTED_EDGE ( 'NONE', *, *, #125911, .T. ) ;
#136859 = ADVANCED_FACE ( 'NONE', ( #6441 ), #72520, .F. ) ;
#136858 = LINE ( 'NONE', #81803, #8808 ) ;
#136860 = ORIENTED_EDGE ( 'NONE', *, *, #77564, .T. ) ;
#136861 = ORIENTED_EDGE ( 'NONE', *, *, #114842, .F. ) ;
#136862 = CARTESIAN_POINT ( 'NONE',  ( -27.18398860626900060, 28.73617430169806042, 5.000000000000000000 ) ) ;
#136863 = ORIENTED_EDGE ( 'NONE', *, *, #81199, .T. ) ;
#136864 = EDGE_LOOP ( 'NONE', ( #107883, #47813, #82178 ) ) ;
#136865 = VECTOR ( 'NONE', #40889, 1000.000000000000000 ) ;
#136866 = CARTESIAN_POINT ( 'NONE',  ( 70.87543019189810423, -5.291415217122920289, -3.055000000000001492 ) ) ;
#136867 = VERTEX_POINT ( 'NONE', #28261 ) ;
#136868 = LINE ( 'NONE', #103503, #46610 ) ;
#136869 = ADVANCED_FACE ( 'NONE', ( #84774 ), #94912, .F. ) ;
#136870 = DIRECTION ( 'NONE',  ( 0.6830127018922181881, 0.6830127018922202975, -0.2588190451025214056 ) ) ;
#136871 = CARTESIAN_POINT ( 'NONE',  ( 107.6254301918981042, 5.291415217122919401, 3.055000000000002824 ) ) ;
#136872 = CARTESIAN_POINT ( 'NONE',  ( 34.92499999999998295, -22.22500000000000142, 4.500000000000000888 ) ) ;
#136873 = VECTOR ( 'NONE', #60940, 1000.000000000000000 ) ;
#136874 = CARTESIAN_POINT ( 'NONE',  ( -34.92500000000001137, 0.8561230773924295434, 4.000000000000000000 ) ) ;
#136876 = CARTESIAN_POINT ( 'NONE',  ( 87.28752705046288440, 0.000000000000000000, -7.949999999999998401 ) ) ;
#136875 = LINE ( 'NONE', #37582, #66466 ) ;
#136877 =( NAMED_UNIT ( * ) PLANE_ANGLE_UNIT ( ) SI_UNIT ( $, .RADIAN. ) );
#136878 = DIRECTION ( 'NONE',  ( 0.000000000000000000, 0.000000000000000000, 1.000000000000000000 ) ) ;
#136879 = EDGE_CURVE ( 'NONE', #74851, #98477, #27178, .T. ) ;
#136880 = EDGE_CURVE ( 'NONE', #23695, #130192, #63756, .T. ) ;
#136881 = VECTOR ( 'NONE', #1651, 1000.000000000000227 ) ;
#136882 = DIRECTION ( 'NONE',  ( 0.3543493200069162685, -0.000000000000000000, -0.9351131265310288487 ) ) ;
#136883 = ORIENTED_EDGE ( 'NONE', *, *, #33995, .T. ) ;
#136884 = VECTOR ( 'NONE', #15706, 1000.000000000000000 ) ;
#136885 = ADVANCED_FACE ( 'NONE', ( #82642 ), #89078, .T. ) ;
#136886 =( NAMED_UNIT ( * ) SI_UNIT ( $, .STERADIAN. ) SOLID_ANGLE_UNIT ( ) );
#136887 = DIRECTION ( 'NONE',  ( 0.7071067811865487940, -0.7071067811865463515, 0.000000000000000000 ) ) ;
#136888 = ORIENTED_EDGE ( 'NONE', *, *, #20544, .F. ) ;
#136889 = VECTOR ( 'NONE', #70242, 1000.000000000000000 ) ;
#136890 = EDGE_LOOP ( 'NONE', ( #31936, #10984, #88623, #125658 ) ) ;
#136891 = LINE ( 'NONE', #13654, #37897 ) ;
#136892 = ORIENTED_EDGE ( 'NONE', *, *, #70977, .F. ) ;
#136893 = DIRECTION ( 'NONE',  ( 0.6830127018922181881, 0.6830127018922202975, -0.2588190451025214056 ) ) ;
#136894 = CARTESIAN_POINT ( 'NONE',  ( 0.000000000000000000, 0.000000000000000000, 5.000000000000000000 ) ) ;
#136895 = AXIS2_PLACEMENT_3D ( 'NONE', #79034, #55840, #100046 ) ;
#136896 = FACE_OUTER_BOUND ( 'NONE', #82243, .T. ) ;
#136897 = EDGE_CURVE ( 'NONE', #45041, #80972, #132600, .T. ) ;
#136898 = CARTESIAN_POINT ( 'NONE',  ( -19.35292824042819504, -2.786763769301527027, 4.186878071398595580 ) ) ;
#136899 = ORIENTED_EDGE ( 'NONE', *, *, #117930, .T. ) ;
#136900 = CARTESIAN_POINT ( 'NONE',  ( 152.4000000000000057, 7.919999999999947526, -18.97500000000001918 ) ) ;
#136901 = ORIENTED_EDGE ( 'NONE', *, *, #136846, .F. ) ;
#136902 = CARTESIAN_POINT ( 'NONE',  ( 9.183988606268997046, 28.73617430169793607, 5.000000000000000000 ) ) ;
#136903 = VECTOR ( 'NONE', #80174, 1000.000000000000000 ) ;
#136904 = CARTESIAN_POINT ( 'NONE',  ( 27.48373647476854842, -5.808823158059035485, -5.808823158059033709 ) ) ;
#136905 = FACE_OUTER_BOUND ( 'NONE', #5052, .T. ) ;
#136906 = CARTESIAN_POINT ( 'NONE',  ( 14.55628666580615693, -9.434540764276121649, -1.149137486816687481 ) ) ;
#136907 = EDGE_LOOP ( 'NONE', ( #93794, #141774, #122134, #62463 ) ) ;
#136908 = ORIENTED_EDGE ( 'NONE', *, *, #107557, .T. ) ;
#136909 = CIRCLE ( 'NONE', #76822, 34.92999999999999972 ) ;
#136910 = ORIENTED_EDGE ( 'NONE', *, *, #18722, .F. ) ;
#136911 = DIRECTION ( 'NONE',  ( 0.000000000000000000, -1.000000000000000000, 0.000000000000000000 ) ) ;
#136912 = CARTESIAN_POINT ( 'NONE',  ( -7.499999999999944045, 9.052185695429077583, 5.000000000000000000 ) ) ;
#136913 = COLOUR_RGB ( '', 0.31764706, 0.68627451, 0.89019608) ;
#136914 = CARTESIAN_POINT ( 'NONE',  ( -33.18398860626899705, 28.73617430169810305, 5.000000000000000000 ) ) ;
#136915 = ORIENTED_EDGE ( 'NONE', *, *, #67297, .T. ) ;
#136916 = DIRECTION ( 'NONE',  ( 0.6830127018922180770, -0.6830127018922204085, -0.2588190451025213501 ) ) ;
#136917 = CARTESIAN_POINT ( 'NONE',  ( 12.18398860626900060, 28.73617430169795739, 5.000000000000000000 ) ) ;
#136918 = DIRECTION ( 'NONE',  ( -0.7071067811865487940, 0.7071067811865463515, 0.000000000000000000 ) ) ;
#136919 = PLANE ( 'NONE',  #37316 ) ;
#136921 = AXIS2_PLACEMENT_3D ( 'NONE', #86169, #73860, #65879 ) ;
#136920 = DIRECTION ( 'NONE',  ( -0.000000000000000000, 0.3543493200069153248, 0.9351131265310292928 ) ) ;
#136922 = ORIENTED_EDGE ( 'NONE', *, *, #52176, .T. ) ;
#136923 = LINE ( 'NONE', #128891, #51005 ) ;
#136924 = AXIS2_PLACEMENT_3D ( 'NONE', #73288, #119595, #31907 ) ;
#136925 = PLANE ( 'NONE',  #125788 ) ;
#136926 = ORIENTED_EDGE ( 'NONE', *, *, #104016, .T. ) ;
#136927 = LINE ( 'NONE', #5672, #134013 ) ;
#136929 = VERTEX_POINT ( 'NONE', #64446 ) ;
#136928 = SURFACE_SIDE_STYLE ('',( #70979 ) ) ;
#136930 = ORIENTED_EDGE ( 'NONE', *, *, #8739, .F. ) ;
#136931 = LINE ( 'NONE', #83270, #23736 ) ;
#136932 = LINE ( 'NONE', #73648, #142736 ) ;
#136933 = DIRECTION ( 'NONE',  ( -0.3543493200069163240, 0.000000000000000000, 0.9351131265310288487 ) ) ;
#136935 = ORIENTED_EDGE ( 'NONE', *, *, #92222, .F. ) ;
#136934 = AXIS2_PLACEMENT_3D ( 'NONE', #115317, #16013, #104477 ) ;
#136936 = DIRECTION ( 'NONE',  ( 0.7071067811865486830, -0.7071067811865464625, -0.000000000000000000 ) ) ;
#136937 = PLANE ( 'NONE',  #10500 ) ;
#136938 = DIRECTION ( 'NONE',  ( -0.3543493200069162685, -0.000000000000000000, -0.9351131265310288487 ) ) ;
#136940 = EDGE_CURVE ( 'NONE', #40695, #29533, #87628, .T. ) ;
#136939 = CARTESIAN_POINT ( 'NONE',  ( 126.9541937171295700, 6.884901960086283523, 3.975000000000002753 ) ) ;
#136941 = CARTESIAN_POINT ( 'NONE',  ( 9.489213562373095101, -27.52281430457062328, 5.000000000000000000 ) ) ;
#136942 = CARTESIAN_POINT ( 'NONE',  ( -8.510786437626906675, -27.52281430457049183, 5.000000000000000000 ) ) ;
#136943 = EDGE_CURVE ( 'NONE', #136524, #67529, #100662, .T. ) ;
#136944 = CARTESIAN_POINT ( 'NONE',  ( -51.48921356237309510, -27.52281430457091460, 5.000000000000000000 ) ) ;
#136945 = CARTESIAN_POINT ( 'NONE',  ( 4.171830600776447184, 3.759292476615678336, 4.000000000000000000 ) ) ;
#136946 = EDGE_CURVE ( 'NONE', #89301, #14297, #56484, .T. ) ;
#136947 = FACE_OUTER_BOUND ( 'NONE', #92975, .T. ) ;
#136948 = CARTESIAN_POINT ( 'NONE',  ( 33.66623647476855297, 7.934999999999990727, -1.457635852685135314E-15 ) ) ;
#136949 = CARTESIAN_POINT ( 'NONE',  ( 4.937069808101886004, 2.126176841940952134, -7.934999999999992504 ) ) ;
#136950 = CARTESIAN_POINT ( 'NONE',  ( -2.292893218813436107, -18.74070752338409562, 5.000000000000000000 ) ) ;
#136951 = VECTOR ( 'NONE', #3342, 1000.000000000000000 ) ;
#136952 = CARTESIAN_POINT ( 'NONE',  ( 7.499999999999947597, -13.53360074219760101, 5.000000000000000000 ) ) ;
#136954 = ADVANCED_FACE ( 'NONE', ( #78196 ), #76044, .F. ) ;
#136953 = DIRECTION ( 'NONE',  ( -0.000000000000000000, 0.000000000000000000, 1.000000000000000000 ) ) ;
#136955 = ORIENTED_EDGE ( 'NONE', *, *, #37521, .F. ) ;
#136956 = ORIENTED_EDGE ( 'NONE', *, *, #49939, .F. ) ;
#136957 = VECTOR ( 'NONE', #82175, 1000.000000000000227 ) ;
#136958 = CARTESIAN_POINT ( 'NONE',  ( 96.08333333333332860, 6.884901960086290629, -3.974999999999994316 ) ) ;
#136959 = VECTOR ( 'NONE', #123677, 1000.000000000000000 ) ;
#136960 = ORIENTED_EDGE ( 'NONE', *, *, #132464, .T. ) ;
#136961 = ORIENTED_EDGE ( 'NONE', *, *, #35061, .F. ) ;
#136962 = CARTESIAN_POINT ( 'NONE',  ( 13.49999999999991296, -4.912538124160707120, 4.000000000000000000 ) ) ;
#136963 = DIRECTION ( 'NONE',  ( 0.7071067811865486830, -0.7071067811865464625, -0.000000000000000000 ) ) ;
#136964 = VECTOR ( 'NONE', #136032, 1000.000000000000000 ) ;
#136965 = AXIS2_PLACEMENT_3D ( 'NONE', #47681, #93279, #102018 ) ;
#136966 = AXIS2_PLACEMENT_3D ( 'NONE', #39796, #60111, #128217 ) ;
#136967 = CARTESIAN_POINT ( 'NONE',  ( 14.47215708364651121, 9.396720740463704757, 1.422595638764767134 ) ) ;
#136968 = ORIENTED_EDGE ( 'NONE', *, *, #10758, .T. ) ;
#136969 = DIRECTION ( 'NONE',  ( -0.7071067811865486830, -0.7071067811865464625, 0.000000000000000000 ) ) ;
#136970 = VECTOR ( 'NONE', #20274, 999.9999999999998863 ) ;
#136971 = DIRECTION ( 'NONE',  ( 0.6830127018922181881, 0.6830127018922202975, -0.2588190451025214056 ) ) ;
#136972 = EDGE_CURVE ( 'NONE', #128651, #127270, #86928, .T. ) ;
#136973 = LINE ( 'NONE', #26773, #20954 ) ;
#136974 = CARTESIAN_POINT ( 'NONE',  ( 125.5000000000000568, -3.922572014496796822, -6.914906274931464480 ) ) ;
#136975 = EDGE_CURVE ( 'NONE', #15400, #78073, #63582, .T. ) ;
#136976 = DIRECTION ( 'NONE',  ( 0.3543493200069162685, -0.000000000000000000, -0.9351131265310288487 ) ) ;
#136977 = DIRECTION ( 'NONE',  ( -0.000000000000000000, 0.000000000000000000, 1.000000000000000000 ) ) ;
#136978 = DIRECTION ( 'NONE',  ( -0.000000000000000000, 0.000000000000000000, 1.000000000000000000 ) ) ;
#136979 = CARTESIAN_POINT ( 'NONE',  ( -33.48921356237309510, -27.52281430457078670, 5.000000000000000000 ) ) ;
#136980 = LINE ( 'NONE', #134873, #46960 ) ;
#136981 = CARTESIAN_POINT ( 'NONE',  ( 34.92499999999998295, 12.95788372223795193, 1.488343219358033487 ) ) ;
#136982 = FACE_OUTER_BOUND ( 'NONE', #46225, .T. ) ;
#136983 = EDGE_CURVE ( 'NONE', #59778, #32290, #53374, .T. ) ;
#136984 = CARTESIAN_POINT ( 'NONE',  ( 11.70025512860841133, -27.71228299555198049, 4.000000000000000000 ) ) ;
#136985 = VERTEX_POINT ( 'NONE', #23052 ) ;
#136986 = VERTEX_POINT ( 'NONE', #21665 ) ;
#136987 = CARTESIAN_POINT ( 'NONE',  ( 107.9170968585647756, 3.054999999999998828, 5.291415217122922066 ) ) ;
#136988 = ORIENTED_EDGE ( 'NONE', *, *, #35430, .T. ) ;
#136989 = DIRECTION ( 'NONE',  ( 0.7071067811865487940, -0.7071067811865463515, 0.000000000000000000 ) ) ;
#136990 = ADVANCED_FACE ( 'NONE', ( #55732 ), #10748, .F. ) ;
#136991 = CARTESIAN_POINT ( 'NONE',  ( -39.48921356237310221, -27.52281430457082934, 5.000000000000000000 ) ) ;
#136992 = ORIENTED_EDGE ( 'NONE', *, *, #85715, .T. ) ;
#136993 = DIRECTION ( 'NONE',  ( 1.000000000000000000, 0.000000000000000000, 0.000000000000000000 ) ) ;
#136994 = DIRECTION ( 'NONE',  ( 0.7071067811865487940, -0.7071067811865463515, 0.000000000000000000 ) ) ;
#136995 = AXIS2_PLACEMENT_3D ( 'NONE', #111530, #76802, #11472 ) ;
#136996 = VECTOR ( 'NONE', #118456, 1000.000000000000000 ) ;
#136997 = CARTESIAN_POINT ( 'NONE',  ( 102.2870968585647802, 3.054999999999997495, 5.291415217122919401 ) ) ;
#136998 = ORIENTED_EDGE ( 'NONE', *, *, #106186, .F. ) ;
#136999 = AXIS2_PLACEMENT_3D ( 'NONE', #5269, #24368, #127066 ) ;
#137000 = EDGE_LOOP ( 'NONE', ( #64299, #56, #34160, #123871 ) ) ;
#137002 = EDGE_CURVE ( 'NONE', #85826, #126030, #142725, .T. ) ;
#137001 = DIRECTION ( 'NONE',  ( -0.6830127018922181881, 0.6830127018922202975, -0.2588190451025214056 ) ) ;
#137003 = DIRECTION ( 'NONE',  ( 0.7071067811865487940, 0.7071067811865463515, 0.000000000000000000 ) ) ;
#137004 = VECTOR ( 'NONE', #42146, 1000.000000000000000 ) ;
#137005 = DIRECTION ( 'NONE',  ( 1.000000000000000000, 0.000000000000000000, 0.000000000000000000 ) ) ;
#137006 = VERTEX_POINT ( 'NONE', #143428 ) ;
#137007 = ORIENTED_EDGE ( 'NONE', *, *, #88009, .T. ) ;
#137008 = VERTEX_POINT ( 'NONE', #98501 ) ;
#137009 = PLANE ( 'NONE',  #76964 ) ;
#137010 = VECTOR ( 'NONE', #13987, 1000.000000000000000 ) ;
#137011 = EDGE_CURVE ( 'NONE', #63240, #44164, #65915, .T. ) ;
#137012 = SURFACE_SIDE_STYLE ('',( #125430 ) ) ;
#137013 = CARTESIAN_POINT ( 'NONE',  ( 13.40832548098992660, -0.7407075233842701500, 14.76736230305383479 ) ) ;
#137014 = VERTEX_POINT ( 'NONE', #42724 ) ;
#137015 = ORIENTED_EDGE ( 'NONE', *, *, #1702, .F. ) ;
#137016 = LINE ( 'NONE', #135599, #61788 ) ;
#137018 = VERTEX_POINT ( 'NONE', #120214 ) ;
#137017 = EDGE_CURVE ( 'NONE', #28064, #119026, #131138, .T. ) ;
#137019 = ORIENTED_EDGE ( 'NONE', *, *, #48230, .F. ) ;
#137020 = VECTOR ( 'NONE', #104333, 1000.000000000000227 ) ;
#137021 = VECTOR ( 'NONE', #8684, 1000.000000000000000 ) ;
#137022 = DIRECTION ( 'NONE',  ( 0.6830127018922180770, -0.6830127018922204085, -0.2588190451025213501 ) ) ;
#137023 = CARTESIAN_POINT ( 'NONE',  ( 34.49999999999975842, -4.796895815300992183, -3.611700055028602918 ) ) ;
#137024 = ORIENTED_EDGE ( 'NONE', *, *, #107449, .F. ) ;
#137025 = DIRECTION ( 'NONE',  ( -0.7071067811865486830, -0.7071067811865464625, 0.000000000000000000 ) ) ;
#137026 = ADVANCED_FACE ( 'NONE', ( #109376 ), #43417, .T. ) ;
#137027 =( GEOMETRIC_REPRESENTATION_CONTEXT ( 3 ) GLOBAL_UNCERTAINTY_ASSIGNED_CONTEXT ( ( #59413 ) ) GLOBAL_UNIT_ASSIGNED_CONTEXT ( ( #120046, #63603, #31663 ) ) REPRESENTATION_CONTEXT ( 'NONE', 'WORKASPACE' ) );
#137028 = CARTESIAN_POINT ( 'NONE',  ( 20.99999999999985079, -8.731860332648823331, -2.120594902707488405 ) ) ;
#137029 = DIRECTION ( 'NONE',  ( -0.7071067811865486830, 0.7071067811865464625, 0.000000000000000000 ) ) ;
#137030 = CARTESIAN_POINT ( 'NONE',  ( 23.99451991528749062, 28.92564299267954908, 4.000000000000000000 ) ) ;
#137031 = FACE_BOUND ( 'NONE', #106058, .T. ) ;
#137032 = ORIENTED_EDGE ( 'NONE', *, *, #35415, .F. ) ;
#137033 = CARTESIAN_POINT ( 'NONE',  ( 20.29289321881331531, 11.25929247661560240, 5.000000000000000000 ) ) ;
#137035 = EDGE_CURVE ( 'NONE', #5277, #74851, #121665, .T. ) ;
#137034 = CARTESIAN_POINT ( 'NONE',  ( 11.99999999999991829, -9.412538124160660047, 4.000000000000000000 ) ) ;
#137036 = PLANE ( 'NONE',  #118630 ) ;
#137037 = ORIENTED_EDGE ( 'NONE', *, *, #95485, .F. ) ;
#137038 = DIRECTION ( 'NONE',  ( -0.000000000000000000, -0.000000000000000000, 1.000000000000000000 ) ) ;
#137039 = VERTEX_POINT ( 'NONE', #600 ) ;
#137040 = ORIENTED_EDGE ( 'NONE', *, *, #6760, .T. ) ;
#137041 = AXIS2_PLACEMENT_3D ( 'NONE', #108212, #41557, #6220 ) ;
#137042 = ORIENTED_EDGE ( 'NONE', *, *, #36171, .T. ) ;
#137043 = CARTESIAN_POINT ( 'NONE',  ( 38.12043019189811588, 3.055000000000001936, -5.291415217122916737 ) ) ;
#137044 = VERTEX_POINT ( 'NONE', #68761 ) ;
#137045 = DIRECTION ( 'NONE',  ( 0.000000000000000000, 0.000000000000000000, -1.000000000000000000 ) ) ;
#137046 = CARTESIAN_POINT ( 'NONE',  ( -34.92500000000001137, 22.22500000000000142, 4.000000000000000000 ) ) ;
#137047 = LINE ( 'NONE', #81993, #65990 ) ;
#137048 = EDGE_CURVE ( 'NONE', #7797, #133878, #102080, .T. ) ;
#137049 = ORIENTED_EDGE ( 'NONE', *, *, #93971, .T. ) ;
#137050 = LINE ( 'NONE', #92819, #76919 ) ;
#137051 =( NAMED_UNIT ( * ) SI_UNIT ( $, .STERADIAN. ) SOLID_ANGLE_UNIT ( ) );
#137052 = VECTOR ( 'NONE', #118368, 1000.000000000000000 ) ;
#137053 = VECTOR ( 'NONE', #133513, 1000.000000000000000 ) ;
#137054 = PLANE ( 'NONE',  #93203 ) ;
#137055 = CIRCLE ( 'NONE', #23632, 9.500000000000000000 ) ;
#137056 = DIRECTION ( 'NONE',  ( -0.6830127018922181881, 0.6830127018922202975, -0.2588190451025214056 ) ) ;
#137057 = FACE_OUTER_BOUND ( 'NONE', #98728, .T. ) ;
#137058 = EDGE_CURVE ( 'NONE', #91883, #21154, #123852, .T. ) ;
#137059 =( NAMED_UNIT ( * ) SI_UNIT ( $, .STERADIAN. ) SOLID_ANGLE_UNIT ( ) );
#137060 = DIRECTION ( 'NONE',  ( -0.3543493200069162685, -0.000000000000000000, -0.9351131265310288487 ) ) ;
#137061 = ORIENTED_EDGE ( 'NONE', *, *, #132200, .F. ) ;
#137062 = EDGE_LOOP ( 'NONE', ( #37869, #127821, #123189, #113252, #41283, #66527, #67532, #60541, #103354, #9177, #108827, #16616 ) ) ;
#137063 = VECTOR ( 'NONE', #98291, 999.9999999999998863 ) ;
#137064 = VERTEX_POINT ( 'NONE', #26654 ) ;
#137065 = MECHANICAL_DESIGN_GEOMETRIC_PRESENTATION_REPRESENTATION (  '', ( #97620 ), #7478 ) ;
#137066 = VERTEX_POINT ( 'NONE', #112250 ) ;
#137067 = STYLED_ITEM ( 'NONE', ( #26814 ), #70809 ) ;
#137068 = SURFACE_STYLE_USAGE ( .BOTH. , #125485 ) ;
#137069 = VERTEX_POINT ( 'NONE', #46309 ) ;
#137070 = ORIENTED_EDGE ( 'NONE', *, *, #1736, .T. ) ;
#137071 = CARTESIAN_POINT ( 'NONE',  ( 23.37053679528800743, 22.22500000000000142, -17.09035809333496658 ) ) ;
#137072 = LINE ( 'NONE', #18838, #31784 ) ;
#137073 = ADVANCED_FACE ( 'NONE', ( #1996 ), #91233, .F. ) ;
#137074 = EDGE_CURVE ( 'NONE', #134215, #816, #47738, .T. ) ;
#137075 = LINE ( 'NONE', #58855, #4539 ) ;
#137076 = VERTEX_POINT ( 'NONE', #89760 ) ;
#137077 = FACE_OUTER_BOUND ( 'NONE', #38230, .T. ) ;
#137078 = ORIENTED_EDGE ( 'NONE', *, *, #91890, .T. ) ;
#137079 = CARTESIAN_POINT ( 'NONE',  ( 25.88982677111770769, -22.22500000000000853, 4.785647885939352975 ) ) ;
#137080 = DIRECTION ( 'NONE',  ( 0.000000000000000000, -1.000000000000000000, 0.000000000000000000 ) ) ;
#137081 = CARTESIAN_POINT ( 'NONE',  ( 1.087903141435219379, 6.871911579029515771, 3.967499999999989146 ) ) ;
#137082 = ORIENTED_EDGE ( 'NONE', *, *, #26787, .F. ) ;
#137084 = LINE ( 'NONE', #124772, #121663 ) ;
#137083 = CARTESIAN_POINT ( 'NONE',  ( 104.3287635252314658, 0.000000000000000000, -6.109999999999999432 ) ) ;
#137085 = CARTESIAN_POINT ( 'NONE',  ( -8.999999999999930722, -9.412538124160660047, 4.000000000000000000 ) ) ;
#137086 = ORIENTED_EDGE ( 'NONE', *, *, #119329, .T. ) ;
#137087 = ORIENTED_EDGE ( 'NONE', *, *, #96700, .F. ) ;
#137088 = DIRECTION ( 'NONE',  ( -0.7071067811865487940, 0.7071067811865463515, -0.000000000000000000 ) ) ;
#137089 = VERTEX_POINT ( 'NONE', #37548 ) ;
#137090 = DIRECTION ( 'NONE',  ( 1.000000000000000000, 0.000000000000000000, 0.000000000000000000 ) ) ;
#137091 = SURFACE_STYLE_FILL_AREA ( #102343 ) ;
#137092 = FACE_OUTER_BOUND ( 'NONE', #44382, .T. ) ;
#137093 = DIRECTION ( 'NONE',  ( -0.000000000000000000, -0.3543493200069152693, 0.9351131265310292928 ) ) ;
#137094 = CARTESIAN_POINT ( 'NONE',  ( -24.32816939922335564, -6.740707523384212863, 4.000000000000000000 ) ) ;
#137095 = ADVANCED_FACE ( 'NONE', ( #134739 ), #12904, .F. ) ;
#137096 = ORIENTED_EDGE ( 'NONE', *, *, #121467, .T. ) ;
#137097 = VECTOR ( 'NONE', #38265, 1000.000000000000000 ) ;
#137098 = DIRECTION ( 'NONE',  ( 0.7071067811865486830, -0.7071067811865464625, -0.000000000000000000 ) ) ;
#137099 = AXIS2_PLACEMENT_3D ( 'NONE', #24861, #69104, #103138 ) ;
#137100 = VECTOR ( 'NONE', #126876, 999.9999999999998863 ) ;
#137101 = CARTESIAN_POINT ( 'NONE',  ( 8.188407645496676324, -2.499999999999998224, 0.000000000000000000 ) ) ;
#137102 = CARTESIAN_POINT ( 'NONE',  ( 34.92499999999998295, 22.22500000000000142, 4.000000000000000000 ) ) ;
#137103 = ORIENTED_EDGE ( 'NONE', *, *, #46361, .F. ) ;
#137104 = DIRECTION ( 'NONE',  ( -0.7071067811865487940, 0.7071067811865463515, 0.000000000000000000 ) ) ;
#137105 = COLOUR_RGB ( '', 0.72549020, 0.75294118, 0.79215686) ;
#137106 = CARTESIAN_POINT ( 'NONE',  ( -12.79289321881336683, -17.24070752338410628, 5.000000000000000000 ) ) ;
#137107 = EDGE_LOOP ( 'NONE', ( #33503, #11619, #88125, #118150 ) ) ;
#137109 = ORIENTED_EDGE ( 'NONE', *, *, #5322, .F. ) ;
#137108 = CARTESIAN_POINT ( 'NONE',  ( 25.97159235450331849, -2.500000000000000444, 3.061616997868384620E-16 ) ) ;
#137110 = EDGE_LOOP ( 'NONE', ( #45007, #94997, #66811, #125925 ) ) ;
#137111 = CARTESIAN_POINT ( 'NONE',  ( 6.758600742197917732, 21.72500000000000142, 5.000000000000000000 ) ) ;
#137112 = LINE ( 'NONE', #28357, #43761 ) ;
#137113 = AXIS2_PLACEMENT_3D ( 'NONE', #76255, #54518, #79139 ) ;
#137114 = EDGE_LOOP ( 'NONE', ( #71599, #84190, #95407, #124064 ) ) ;
#137115 = DIRECTION ( 'NONE',  ( 0.000000000000000000, -1.000000000000000000, 0.000000000000000000 ) ) ;
#137116 = DIRECTION ( 'NONE',  ( 0.6830127018922181881, 0.6830127018922202975, -0.2588190451025214056 ) ) ;
#137117 = ADVANCED_FACE ( 'NONE', ( #80352 ), #45589, .T. ) ;
#137118 = DIRECTION ( 'NONE',  ( -0.7071067811865486830, 0.7071067811865464625, 0.000000000000000000 ) ) ;
#137119 = VERTEX_POINT ( 'NONE', #133995 ) ;
#137120 = DIRECTION ( 'NONE',  ( 0.3543493200069162685, -0.000000000000000000, -0.9351131265310288487 ) ) ;
#137121 = EDGE_CURVE ( 'NONE', #102047, #118149, #61983, .T. ) ;
#137122 = CARTESIAN_POINT ( 'NONE',  ( -65.99451991528749772, 28.92564299267984396, 4.000000000000000000 ) ) ;
#137123 = CARTESIAN_POINT ( 'NONE',  ( 25.39999999999999858, 1.194621026894846283, 17.40906030209848510 ) ) ;
#137124 = VECTOR ( 'NONE', #86568, 1000.000000000000227 ) ;
#137125 = CARTESIAN_POINT ( 'NONE',  ( 1.828169399223516400, 9.759292476615625489, 4.000000000000000000 ) ) ;
#137126 = PLANE ( 'NONE',  #3107 ) ;
#137127 = VECTOR ( 'NONE', #47839, 1000.000000000000000 ) ;
#137128 = CARTESIAN_POINT ( 'NONE',  ( -21.16696429985206152, -22.22500000000000142, 10.21343402916774146 ) ) ;
#137129 = CARTESIAN_POINT ( 'NONE',  ( -15.87485380690756287, -14.24070752338414003, 9.401115078912694045 ) ) ;
#137131 = EDGE_CURVE ( 'NONE', #104041, #91273, #114374, .T. ) ;
#137130 = CARTESIAN_POINT ( 'NONE',  ( -13.95484226663325167, -21.74070752338406720, 21.72585301388581769 ) ) ;
#137133 = EDGE_CURVE ( 'NONE', #61052, #87228, #136124, .T. ) ;
#137132 = EDGE_LOOP ( 'NONE', ( #15710, #41063, #75757, #24923 ) ) ;
#137134 = VERTEX_POINT ( 'NONE', #103477 ) ;
#137135 = EDGE_LOOP ( 'NONE', ( #36601, #76876, #37071, #58286 ) ) ;
#137136 = CARTESIAN_POINT ( 'NONE',  ( 118.2500000000000000, -9.735942053221458872E-16, 7.950000000000000178 ) ) ;
#137137 = ORIENTED_EDGE ( 'NONE', *, *, #123807, .T. ) ;
#137138 = VERTEX_POINT ( 'NONE', #36810 ) ;
#137139 = ORIENTED_EDGE ( 'NONE', *, *, #76609, .T. ) ;
#137140 = AXIS2_PLACEMENT_3D ( 'NONE', #141373, #84179, #86993 ) ;
#137141 = LINE ( 'NONE', #50136, #45599 ) ;
#137142 = DIRECTION ( 'NONE',  ( -0.7071067811865486830, -0.7071067811865464625, 0.000000000000000000 ) ) ;
#137143 = VECTOR ( 'NONE', #52126, 1000.000000000000000 ) ;
#137144 = ORIENTED_EDGE ( 'NONE', *, *, #76, .T. ) ;
#137145 = CARTESIAN_POINT ( 'NONE',  ( -16.49999999999988276, 18.05218569542898521, 5.000000000000000000 ) ) ;
#137146 = CARTESIAN_POINT ( 'NONE',  ( 0.000000000000000000, 0.000000000000000000, 5.000000000000000000 ) ) ;
#137147 = EDGE_CURVE ( 'NONE', #32788, #49753, #81057, .T. ) ;
#137148 = DIRECTION ( 'NONE',  ( -1.000000000000000000, -1.224606353822377258E-16, -0.000000000000000000 ) ) ;
#137149 = CARTESIAN_POINT ( 'NONE',  ( 108.6462635252314186, -4.472830434245840259, 4.472830434245839371 ) ) ;
#137150 = VERTEX_POINT ( 'NONE', #78923 ) ;
#137151 = EDGE_CURVE ( 'NONE', #112625, #96438, #68242, .T. ) ;
#137152 = CARTESIAN_POINT ( 'NONE',  ( -12.83997584945354831, 6.969621038081828424, -30.86176790400288539 ) ) ;
#137153 = CARTESIAN_POINT ( 'NONE',  ( -34.92500000000001137, -14.99387692260790494, 4.000000000000000000 ) ) ;
#137155 = AXIS2_PLACEMENT_3D ( 'NONE', #42854, #34113, #23187 ) ;
#137154 = FACE_OUTER_BOUND ( 'NONE', #142740, .T. ) ;
#137156 = PLANE ( 'NONE',  #136153 ) ;
#137157 = CARTESIAN_POINT ( 'NONE',  ( 181.1500000000000057, -47.62213595499959951, 36.92500000000000426 ) ) ;
#137158 = FACE_OUTER_BOUND ( 'NONE', #34592, .T. ) ;
#137159 = CARTESIAN_POINT ( 'NONE',  ( 34.42499999999998295, 22.22500000000000142, 5.000000000000000000 ) ) ;
#137160 = CARTESIAN_POINT ( 'NONE',  ( 41.64169371712954870, -2.130196079827424871, -7.949999999999999289 ) ) ;
#137161 = EDGE_CURVE ( 'NONE', #88480, #4875, #70900, .T. ) ;
#137162 = DIRECTION ( 'NONE',  ( 0.000000000000000000, -1.000000000000000000, 0.000000000000000000 ) ) ;
#137163 = DIRECTION ( 'NONE',  ( -0.7071067811865486830, -0.7071067811865464625, 0.000000000000000000 ) ) ;
#137164 = ORIENTED_EDGE ( 'NONE', *, *, #59264, .F. ) ;
#137165 = ORIENTED_EDGE ( 'NONE', *, *, #16379, .F. ) ;
#137166 = CARTESIAN_POINT ( 'NONE',  ( 33.08333333333332860, 6.884901960086290629, -3.974999999999994316 ) ) ;
#137167 = ORIENTED_EDGE ( 'NONE', *, *, #126686, .F. ) ;
#137168 = ORIENTED_EDGE ( 'NONE', *, *, #86334, .T. ) ;
#137169 = LINE ( 'NONE', #116829, #30101 ) ;
#137170 = FACE_OUTER_BOUND ( 'NONE', #61301, .T. ) ;
#137171 = ORIENTED_EDGE ( 'NONE', *, *, #42786, .F. ) ;
#137173 = EDGE_CURVE ( 'NONE', #23783, #45084, #1309, .T. ) ;
#137172 = VECTOR ( 'NONE', #92698, 1000.000000000000000 ) ;
#137174 = VECTOR ( 'NONE', #123908, 1000.000000000000227 ) ;
#137175 = VECTOR ( 'NONE', #43770, 1000.000000000000000 ) ;
#137176 = CARTESIAN_POINT ( 'NONE',  ( 7.940000000000001279, -35.14999999999999858, -10.00000000000000178 ) ) ;
#137177 = LINE ( 'NONE', #83515, #83911 ) ;
#137178 = CIRCLE ( 'NONE', #86255, 28.00000000000001776 ) ;
#137179 = LINE ( 'NONE', #114679, #44326 ) ;
#137180 = STYLED_ITEM ( 'NONE', ( #38443 ), #16114 ) ;
#137181 = CARTESIAN_POINT ( 'NONE',  ( 31.93793019189809712, -6.110000000000001208, 1.637169565754158951 ) ) ;
#137182 = EDGE_LOOP ( 'NONE', ( #4625, #37988, #810, #107408 ) ) ;
#137183 = CARTESIAN_POINT ( 'NONE',  ( -6.005480084712508493, 28.92564299267933947, 4.000000000000000000 ) ) ;
#137184 = ORIENTED_EDGE ( 'NONE', *, *, #87866, .T. ) ;
#137185 = MECHANICAL_DESIGN_GEOMETRIC_PRESENTATION_REPRESENTATION (  '', ( #125603 ), #23751 ) ;
#137186 = EDGE_CURVE ( 'NONE', #6272, #7430, #97417, .T. ) ;
#137187 = AXIS2_PLACEMENT_3D ( 'NONE', #26419, #15490, #59772 ) ;
#137188 =( GEOMETRIC_REPRESENTATION_CONTEXT ( 3 ) GLOBAL_UNCERTAINTY_ASSIGNED_CONTEXT ( ( #12642 ) ) GLOBAL_UNIT_ASSIGNED_CONTEXT ( ( #107224, #61623, #82637 ) ) REPRESENTATION_CONTEXT ( 'NONE', 'WORKASPACE' ) );
#137189 = DIRECTION ( 'NONE',  ( -0.6830127018922181881, 0.6830127018922202975, -0.2588190451025214056 ) ) ;
#137190 = CARTESIAN_POINT ( 'NONE',  ( 19.93003974513579024, -0.7407075233842735917, 13.87443053587606201 ) ) ;
#137191 = DIRECTION ( 'NONE',  ( 0.7071067811865487940, -0.7071067811865463515, 0.000000000000000000 ) ) ;
#137192 = CARTESIAN_POINT ( 'NONE',  ( 6.066782984417857350, -2.500000000000000444, 3.061616997868384127E-16 ) ) ;
#137193 = ORIENTED_EDGE ( 'NONE', *, *, #50246, .F. ) ;
#137194 = VERTEX_POINT ( 'NONE', #19168 ) ;
#137195 = PLANE ( 'NONE',  #109535 ) ;
#137196 = FACE_OUTER_BOUND ( 'NONE', #45518, .T. ) ;
#137197 = CARTESIAN_POINT ( 'NONE',  ( -23.99999999999983302, -10.77435723561696435, -9.972017380717172585 ) ) ;
#137198 = EDGE_CURVE ( 'NONE', #1609, #90903, #51099, .T. ) ;
#137199 = EDGE_CURVE ( 'NONE', #62063, #56865, #140242, .T. ) ;
#137200 = EDGE_CURVE ( 'NONE', #15048, #33461, #19867, .T. ) ;
#137201 = AXIS2_PLACEMENT_3D ( 'NONE', #16185, #60477, #103223 ) ;
#137202 = CARTESIAN_POINT ( 'NONE',  ( 44.24543019189810877, -5.291415217122918513, -3.055000000000000160 ) ) ;
#137203 = ORIENTED_EDGE ( 'NONE', *, *, #5394, .T. ) ;
#137204 = CARTESIAN_POINT ( 'NONE',  ( 125.2500000000000000, -9.735942053221458872E-16, 7.950000000000000178 ) ) ;
#137205 = DIRECTION ( 'NONE',  ( -2.781805975412905890E-17, 0.3543493200069152693, 0.9351131265310292928 ) ) ;
#137206 = ORIENTED_EDGE ( 'NONE', *, *, #63803, .F. ) ;
#137207 = VERTEX_POINT ( 'NONE', #98163 ) ;
#137208 = CARTESIAN_POINT ( 'NONE',  ( -14.99999999999989519, 18.08204922493371924, 0.9627537363045218788 ) ) ;
#137209 = ORIENTED_EDGE ( 'NONE', *, *, #29657, .F. ) ;
#137210 = AXIS2_PLACEMENT_3D ( 'NONE', #93889, #17056, #50405 ) ;
#137211 = VERTEX_POINT ( 'NONE', #20575 ) ;
#137212 = VECTOR ( 'NONE', #140988, 1000.000000000000000 ) ;
#137213 = FACE_OUTER_BOUND ( 'NONE', #36142, .T. ) ;
#137214 = DIRECTION ( 'NONE',  ( 0.7071067811865486830, -0.7071067811865464625, -0.000000000000000000 ) ) ;
#137215 = AXIS2_PLACEMENT_3D ( 'NONE', #97368, #920, #54626 ) ;
#137216 = CARTESIAN_POINT ( 'NONE',  ( -34.47516574401891631, 22.22311076525683760, 4.292435211493030423 ) ) ;
#137217 = FACE_BOUND ( 'NONE', #74356, .T. ) ;
#137218 = CARTESIAN_POINT ( 'NONE',  ( 48.48921356237309510, -27.52281430457089328, 5.000000000000000000 ) ) ;
#137219 = DIRECTION ( 'NONE',  ( -1.000000000000000000, -1.224606353822377258E-16, -0.000000000000000000 ) ) ;
#137220 = CARTESIAN_POINT ( 'NONE',  ( -34.92500000000001137, -22.22500000000000142, 4.000000000000000000 ) ) ;
#137221 = FACE_OUTER_BOUND ( 'NONE', #87407, .T. ) ;
#137223 = ORIENTED_EDGE ( 'NONE', *, *, #55785, .T. ) ;
#137222 = DIRECTION ( 'NONE',  ( 0.7071067811865487940, 0.7071067811865463515, -0.000000000000000000 ) ) ;
#137224 = CARTESIAN_POINT ( 'NONE',  ( -11.99999999999990230, 20.58746187583903264, 4.000000000000000000 ) ) ;
#137225 = ORIENTED_EDGE ( 'NONE', *, *, #140217, .T. ) ;
#137226 = EDGE_LOOP ( 'NONE', ( #97051, #9097, #112959, #122844 ) ) ;
#137227 = CARTESIAN_POINT ( 'NONE',  ( 64.07876352523145158, -7.482591942790325086E-16, 6.109999999999998543 ) ) ;
#137228 = VERTEX_POINT ( 'NONE', #53208 ) ;
#137229 = DIRECTION ( 'NONE',  ( -0.6830127018922180770, -0.6830127018922204085, -0.2588190451025213501 ) ) ;
#137230 = DIRECTION ( 'NONE',  ( 1.000000000000000000, 0.000000000000000000, 0.000000000000000000 ) ) ;
#137231 = AXIS2_PLACEMENT_3D ( 'NONE', #5222, #127010, #95101 ) ;
#137232 = ORIENTED_EDGE ( 'NONE', *, *, #122504, .F. ) ;
#137233 = DIRECTION ( 'NONE',  ( -0.6830127018922181881, 0.6830127018922202975, -0.2588190451025214056 ) ) ;
#137234 = VECTOR ( 'NONE', #11959, 1000.000000000000000 ) ;
#137235 =( BOUNDED_CURVE ( )  B_SPLINE_CURVE ( 3, ( #108388, #141802, #86705, #73672 ),
 .UNSPECIFIED., .F., .F. ) 
 B_SPLINE_CURVE_WITH_KNOTS ( ( 4, 4 ),
 ( 1.248621635838844446, 1.295595743666722033 ),
 .UNSPECIFIED. ) 
 CURVE ( )  GEOMETRIC_REPRESENTATION_ITEM ( )  RATIONAL_B_SPLINE_CURVE ( ( 1.000000000000000000, 0.9998161278856747547, 0.9998161278856747547, 1.000000000000000000 ) ) 
 REPRESENTATION_ITEM ( '' )  );
#137236 = CARTESIAN_POINT ( 'NONE',  ( -26.99451991528749417, 28.92564299267956685, 4.000000000000000000 ) ) ;
#137237 = LINE ( 'NONE', #3804, #45915 ) ;
#137238 = CARTESIAN_POINT ( 'NONE',  ( -11.20710678118646442, 3.759292476615676559, 5.000000000000000000 ) ) ;
#137239 = CARTESIAN_POINT ( 'NONE',  ( -5.816011393731002066, 28.73617430169783304, 5.000000000000000000 ) ) ;
#137240 =( NAMED_UNIT ( * ) SI_UNIT ( $, .STERADIAN. ) SOLID_ANGLE_UNIT ( ) );
#137241 = ORIENTED_EDGE ( 'NONE', *, *, #92064, .F. ) ;
#137242 = CONICAL_SURFACE ( 'NONE', #141918, 2.055000000000000604, 0.9599310885968764806 ) ;
#137243 = VERTEX_POINT ( 'NONE', #131507 ) ;
#137244 = DIRECTION ( 'NONE',  ( 0.7071067811865487940, -0.7071067811865463515, 0.000000000000000000 ) ) ;
#137245 =( BOUNDED_CURVE ( )  B_SPLINE_CURVE ( 3, ( #50675, #39089, #94868, #127520 ),
 .UNSPECIFIED., .F., .T. ) 
 B_SPLINE_CURVE_WITH_KNOTS ( ( 4, 4 ),
 ( 4.407062196515976638, 4.453802039120700940 ),
 .UNSPECIFIED. ) 
 CURVE ( )  GEOMETRIC_REPRESENTATION_ITEM ( )  RATIONAL_B_SPLINE_CURVE ( ( 1.000000000000000000, 0.9998179572116046021, 0.9998179572116046021, 1.000000000000000000 ) ) 
 REPRESENTATION_ITEM ( '' )  );
#137246 = DIRECTION ( 'NONE',  ( -0.7071067811865486830, -0.7071067811865464625, 0.000000000000000000 ) ) ;
#137247 = ORIENTED_EDGE ( 'NONE', *, *, #54848, .F. ) ;
#137248 = ORIENTED_EDGE ( 'NONE', *, *, #113549, .F. ) ;
#137249 = ORIENTED_EDGE ( 'NONE', *, *, #2516, .T. ) ;
#137250 = DIRECTION ( 'NONE',  ( -1.000000000000000000, 0.000000000000000000, 0.000000000000000000 ) ) ;
#137251 = CARTESIAN_POINT ( 'NONE',  ( -31.26506670282031664, 12.75929247661558996, 18.34774599283963425 ) ) ;
#137252 = EDGE_CURVE ( 'NONE', #132148, #115093, #64103, .T. ) ;
#137253 = EDGE_CURVE ( 'NONE', #33632, #70176, #83018, .T. ) ;
#137254 = DIRECTION ( 'NONE',  ( -0.7071067811865486830, -0.7071067811865464625, -0.000000000000000000 ) ) ;
#137255 = VECTOR ( 'NONE', #30351, 1000.000000000000227 ) ;
#137256 = ORIENTED_EDGE ( 'NONE', *, *, #17929, .F. ) ;
#137257 = CARTESIAN_POINT ( 'NONE',  ( 22.49999999999984723, 21.05218569542895324, 5.000000000000000000 ) ) ;
#137258 = CARTESIAN_POINT ( 'NONE',  ( 10.71290314143521982, 3.967499999999992699, -6.871911579029513994 ) ) ;
#137259 = CARTESIAN_POINT ( 'NONE',  ( -0.4892135623730947680, -27.52281430457055578, 5.000000000000000000 ) ) ;
#137260 = EDGE_LOOP ( 'NONE', ( #109768, #33685, #64617, #134357 ) ) ;
#137261 = EDGE_CURVE ( 'NONE', #24914, #4889, #142392, .T. ) ;
#137262 = PLANE ( 'NONE',  #52671 ) ;
#137263 = CARTESIAN_POINT ( 'NONE',  ( -6.156123077392362752, -22.22500000000000142, 4.000000000000000000 ) ) ;
#137264 = DIRECTION ( 'NONE',  ( -0.000000000000000000, 0.3543493200069153248, 0.9351131265310292928 ) ) ;
#137266 = ORIENTED_EDGE ( 'NONE', *, *, #14540, .F. ) ;
#137265 = LINE ( 'NONE', #61178, #88890 ) ;
#137267 = FACE_OUTER_BOUND ( 'NONE', #2170, .T. ) ;
#137268 = VERTEX_POINT ( 'NONE', #30028 ) ;
#137269 = FACE_OUTER_BOUND ( 'NONE', #136010, .T. ) ;
#137270 = CARTESIAN_POINT ( 'NONE',  ( -7.140000000000000568, -39.92999999999999261, 19.06900128115122328 ) ) ;
#137271 = VECTOR ( 'NONE', #10988, 1000.000000000000227 ) ;
#137272 = CARTESIAN_POINT ( 'NONE',  ( 108.7708333333333286, -7.949999999999998401, -2.130196079827426203 ) ) ;
#137273 = ADVANCED_FACE ( 'NONE', ( #41625 ), #96686, .T. ) ;
#137275 = VERTEX_POINT ( 'NONE', #106137 ) ;
#137274 = VECTOR ( 'NONE', #20597, 1000.000000000000000 ) ;
#137276 = LINE ( 'NONE', #37237, #103819 ) ;
#137277 = CARTESIAN_POINT ( 'NONE',  ( -4.499999999999959144, -20.94781430457061333, 5.000000000000000000 ) ) ;
#137278 = DIRECTION ( 'NONE',  ( -0.7071067811865486830, -0.7071067811865464625, 0.000000000000000000 ) ) ;
#137279 = DIRECTION ( 'NONE',  ( -0.7071067811865487940, 0.7071067811865463515, 0.000000000000000000 ) ) ;
#137280 = PRESENTATION_LAYER_ASSIGNMENT (  '', '', ( #130022 ) ) ;
#137281 = AXIS2_PLACEMENT_3D ( 'NONE', #64235, #63554, #64963 ) ;
#137282 = VERTEX_POINT ( 'NONE', #74276 ) ;
#137283 = AXIS2_PLACEMENT_3D ( 'NONE', #47568, #89587, #80175 ) ;
#137284 = ADVANCED_FACE ( 'NONE', ( #141673 ), #54942, .T. ) ;
#137285 = DIRECTION ( 'NONE',  ( 0.7071067811865487940, 0.7071067811865463515, -0.000000000000000000 ) ) ;
#137286 = CARTESIAN_POINT ( 'NONE',  ( 33.48921356237309510, -27.52281430457078670, 5.000000000000000000 ) ) ;
#137287 = LINE ( 'NONE', #71317, #74672 ) ;
#137288 = FACE_OUTER_BOUND ( 'NONE', #24118, .T. ) ;
#137289 = LINE ( 'NONE', #16926, #134038 ) ;
#137290 = VERTEX_POINT ( 'NONE', #63426 ) ;
#137291 = EDGE_LOOP ( 'NONE', ( #109814, #111204, #91298, #96433 ) ) ;
#137292 = EDGE_CURVE ( 'NONE', #106881, #129256, #85844, .T. ) ;
#137293 = DIRECTION ( 'NONE',  ( -0.000000000000000000, 6.938893903907221278E-15, -1.000000000000000000 ) ) ;
#137294 = CARTESIAN_POINT ( 'NONE',  ( 12.69999999999999574, -59.76999999999998892, -39.50000000000000000 ) ) ;
#137295 = CARTESIAN_POINT ( 'NONE',  ( 4.207903141435219929, -6.871911579029513106, -3.967499999999993587 ) ) ;
#137296 = LINE ( 'NONE', #37993, #124589 ) ;
#137297 = VECTOR ( 'NONE', #142996, 1000.000000000000000 ) ;
#137298 = PLANE ( 'NONE',  #71581 ) ;
#137299 = PLANE ( 'NONE',  #138655 ) ;
#137300 = DIRECTION ( 'NONE',  ( -0.000000000000000000, 0.3543493200069153248, 0.9351131265310292928 ) ) ;
#137301 = ORIENTED_EDGE ( 'NONE', *, *, #5703, .T. ) ;
#137302 = EDGE_CURVE ( 'NONE', #39873, #140739, #31480, .T. ) ;
#137303 = LINE ( 'NONE', #5323, #99742 ) ;
#137304 = DIRECTION ( 'NONE',  ( 0.7071067811865487940, 0.7071067811865463515, 0.000000000000000000 ) ) ;
#137305 = DIRECTION ( 'NONE',  ( -0.000000000000000000, -0.3543493200069152693, 0.9351131265310292928 ) ) ;
#137306 = CARTESIAN_POINT ( 'NONE',  ( 42.93293019189812298, 1.637169565754156730, 6.110000000000001208 ) ) ;
#137307 = VECTOR ( 'NONE', #115797, 1000.000000000000000 ) ;
#137308 = CARTESIAN_POINT ( 'NONE',  ( 184.1374510928294512, -50.57777258831011125, -35.91905586107257875 ) ) ;
#137309 = ADVANCED_FACE ( 'NONE', ( #8252 ), #29317, .F. ) ;
#137310 = EDGE_CURVE ( 'NONE', #62501, #134514, #75702, .T. ) ;
#137311 = ORIENTED_EDGE ( 'NONE', *, *, #29931, .T. ) ;
#137312 = DIRECTION ( 'NONE',  ( -4.681814790819591790E-17, -0.3543493200069152693, 0.9351131265310292928 ) ) ;
#137313 = VECTOR ( 'NONE', #102526, 1000.000000000000000 ) ;
#137314 = ORIENTED_EDGE ( 'NONE', *, *, #42681, .F. ) ;
#137315 = ORIENTED_EDGE ( 'NONE', *, *, #13378, .T. ) ;
#137316 = CARTESIAN_POINT ( 'NONE',  ( -26.67183060077628909, 11.25929247661560417, 4.000000000000000000 ) ) ;
#137317 = ADVANCED_FACE ( 'NONE', ( #30781 ), #75006, .F. ) ;
#137318 = CARTESIAN_POINT ( 'NONE',  ( -15.19713381108422290, 7.733989266307781385, 4.000000000000000000 ) ) ;
#137319 = CARTESIAN_POINT ( 'NONE',  ( 8.816011393731004731, 28.73617430169781173, 5.000000000000000000 ) ) ;
#137320 = DIRECTION ( 'NONE',  ( -0.6830127018922180770, -0.6830127018922204085, -0.2588190451025213501 ) ) ;
#137321 = ADVANCED_FACE ( 'NONE', ( #130813 ), #119870, .T. ) ;
#137322 = DIRECTION ( 'NONE',  ( 0.7071067811865487940, -0.7071067811865463515, 0.000000000000000000 ) ) ;
#137323 =( LENGTH_UNIT ( ) NAMED_UNIT ( * ) SI_UNIT ( .MILLI., .METRE. ) );
#137324 = ORIENTED_EDGE ( 'NONE', *, *, #121425, .T. ) ;
#137325 = ADVANCED_FACE ( 'NONE', ( #12559 ), #134370, .T. ) ;
#137326 = CARTESIAN_POINT ( 'NONE',  ( -9.770042794577866729, 21.73644205237998150, 5.000000000000000000 ) ) ;
#137327 = CARTESIAN_POINT ( 'NONE',  ( 16.44013779566152778, 3.821174125832445049E-16, 0.000000000000000000 ) ) ;
#137328 = UNCERTAINTY_MEASURE_WITH_UNIT (LENGTH_MEASURE( 1.000000000000000082E-05 ), #94250, 'distance_accuracy_value', 'NONE');
#137329 = CARTESIAN_POINT ( 'NONE',  ( 0.000000000000000000, 0.000000000000000000, 5.000000000000000000 ) ) ;
#137330 = FACE_OUTER_BOUND ( 'NONE', #42485, .T. ) ;
#137331 = CARTESIAN_POINT ( 'NONE',  ( 19.49999999999986500, 10.46639925780215563, 5.000000000000000000 ) ) ;
#137332 = VECTOR ( 'NONE', #72616, 1000.000000000000000 ) ;
#137333 = CARTESIAN_POINT ( 'NONE',  ( 64.53752705046289861, -9.735942053221456900E-16, 7.949999999999998401 ) ) ;
#137334 = DIRECTION ( 'NONE',  ( -0.7071067811865487940, 0.7071067811865463515, -0.000000000000000000 ) ) ;
#137335 = ORIENTED_EDGE ( 'NONE', *, *, #112306, .T. ) ;
#137336 = ORIENTED_EDGE ( 'NONE', *, *, #141730, .F. ) ;
#137337 = CARTESIAN_POINT ( 'NONE',  ( 67.20833333333332860, -3.974999999999999201, -6.884901960086287964 ) ) ;
#137338 = ADVANCED_FACE ( 'NONE', ( #111899 ), #109741, .F. ) ;
#137339 = CYLINDRICAL_SURFACE ( 'NONE', #93342, 0.5000000000000004441 ) ;
#137340 = CARTESIAN_POINT ( 'NONE',  ( 27.18398860626900060, 28.73617430169806042, 5.000000000000000000 ) ) ;
#137342 = AXIS2_PLACEMENT_3D ( 'NONE', #130095, #30791, #75715 ) ;
#137341 = LINE ( 'NONE', #80825, #31260 ) ;
#137343 = VECTOR ( 'NONE', #114487, 999.9999999999998863 ) ;
#137344 = VERTEX_POINT ( 'NONE', #56840 ) ;
#137345 = EDGE_CURVE ( 'NONE', #129516, #45966, #99557, .T. ) ;
#137346 = CARTESIAN_POINT ( 'NONE',  ( 20.99999999999985079, -10.77435723561693415, -9.972017380717277391 ) ) ;
#137347 = CARTESIAN_POINT ( 'NONE',  ( 16.27785539607886633, 2.500000000000000888, 0.000000000000000000 ) ) ;
#137348 = CARTESIAN_POINT ( 'NONE',  ( 60.95876352523143993, 0.000000000000000000, -6.110000000000001208 ) ) ;
#137349 = CARTESIAN_POINT ( 'NONE',  ( 20.67906569311139009, -2.055000000000000160, 2.789133085058097101E-16 ) ) ;
#137350 = ORIENTED_EDGE ( 'NONE', *, *, #39935, .F. ) ;
#137351 = ORIENTED_EDGE ( 'NONE', *, *, #90688, .T. ) ;
#137352 = VECTOR ( 'NONE', #35302, 999.9999999999998863 ) ;
#137353 = FILL_AREA_STYLE ('',( #123087 ) ) ;
#137354 =( NAMED_UNIT ( * ) PLANE_ANGLE_UNIT ( ) SI_UNIT ( $, .RADIAN. ) );
#137355 = LINE ( 'NONE', #27858, #23440 ) ;
#137356 = CARTESIAN_POINT ( 'NONE',  ( -8.510786437626906675, -27.52281430457049183, 5.000000000000000000 ) ) ;
#137357 = CARTESIAN_POINT ( 'NONE',  ( 12.32816939922344268, 2.259292476615688994, 4.000000000000000000 ) ) ;
#137359 = ORIENTED_EDGE ( 'NONE', *, *, #142080, .F. ) ;
#137358 = LINE ( 'NONE', #112732, #73046 ) ;
#137360 = CARTESIAN_POINT ( 'NONE',  ( -16.49999999999988276, -19.53360074219753884, 5.000000000000000000 ) ) ;
#137361 = CARTESIAN_POINT ( 'NONE',  ( 18.79653912142945060, 3.821174125832445049E-16, 0.000000000000000000 ) ) ;
#137362 = VECTOR ( 'NONE', #4618, 1000.000000000000227 ) ;
#137363 = DIRECTION ( 'NONE',  ( 0.7071067811865487940, 0.7071067811865463515, -0.000000000000000000 ) ) ;
#137364 = CARTESIAN_POINT ( 'NONE',  ( -39.18398860626899705, 28.73617430169814568, 5.000000000000000000 ) ) ;
#137365 = EDGE_CURVE ( 'NONE', #110210, #18270, #87993, .T. ) ;
#137366 = EDGE_LOOP ( 'NONE', ( #85386, #126306, #47725, #7899 ) ) ;
#137367 = ADVANCED_FACE ( 'NONE', ( #77839 ), #90874, .T. ) ;
#137368 = EDGE_LOOP ( 'NONE', ( #139973, #91101, #126781, #6589 ) ) ;
#137369 = LINE ( 'NONE', #38059, #66205 ) ;
#137370 = EDGE_CURVE ( 'NONE', #11670, #14791, #80014, .T. ) ;
#137371 = CARTESIAN_POINT ( 'NONE',  ( -19.05499999999999261, 3.130000000000007887, -2.396719511207313368E-16 ) ) ;
#137372 = CARTESIAN_POINT ( 'NONE',  ( -12.69999999999998153, 0.000000000000000000, 0.000000000000000000 ) ) ;
#137373 = FACE_OUTER_BOUND ( 'NONE', #135361, .T. ) ;
#137374 = EDGE_LOOP ( 'NONE', ( #86034, #24360, #142468, #122551 ) ) ;
#137375 = ORIENTED_EDGE ( 'NONE', *, *, #86243, .T. ) ;
#137376 = VECTOR ( 'NONE', #138357, 999.9999999999998863 ) ;
#137377 = CARTESIAN_POINT ( 'NONE',  ( 30.71757738642546798, -21.73023691814492508, 5.000000000000000000 ) ) ;
#137379 = EDGE_CURVE ( 'NONE', #64078, #88422, #57532, .T. ) ;
#137378 = DIRECTION ( 'NONE',  ( 0.6830127018922180770, -0.6830127018922204085, -0.2588190451025213501 ) ) ;
#137380 = AXIS2_PLACEMENT_3D ( 'NONE', #120424, #129921, #76264 ) ;
#137381 = VERTEX_POINT ( 'NONE', #1655 ) ;
#137382 = PLANE ( 'NONE',  #69981 ) ;
#137383 = ORIENTED_EDGE ( 'NONE', *, *, #19575, .F. ) ;
#137384 = DIRECTION ( 'NONE',  ( 1.000000000000000000, 0.000000000000000000, 0.000000000000000000 ) ) ;
#137385 = LINE ( 'NONE', #83001, #61019 ) ;
#137386 = VECTOR ( 'NONE', #52300, 1000.000000000000227 ) ;
#137387 = FACE_BOUND ( 'NONE', #91990, .T. ) ;
#137388 = LINE ( 'NONE', #26475, #96465 ) ;
#137389 = CARTESIAN_POINT ( 'NONE',  ( 12.86840764549667604, 9.139736423841732040E-16, 0.000000000000000000 ) ) ;
#137390 = DIRECTION ( 'NONE',  ( -1.000000000000000000, 0.000000000000000000, -0.000000000000000000 ) ) ;
#137391 = CARTESIAN_POINT ( 'NONE',  ( 5.443598275411213550, -2.499999999999999112, 0.000000000000000000 ) ) ;
#137392 = VECTOR ( 'NONE', #127398, 1000.000000000000000 ) ;
#137393 = LINE ( 'NONE', #39521, #25558 ) ;
#137394 = SHAPE_DEFINITION_REPRESENTATION ( #38839, #58954 ) ;
#137395 = VERTEX_POINT ( 'NONE', #122024 ) ;
#137396 = VECTOR ( 'NONE', #7287, 999.9999999999998863 ) ;
#137397 = ORIENTED_EDGE ( 'NONE', *, *, #107169, .T. ) ;
#137398 = CARTESIAN_POINT ( 'NONE',  ( 97.03709685856479439, -3.054999999999998828, -5.291415217122919401 ) ) ;
#137399 = ORIENTED_EDGE ( 'NONE', *, *, #118440, .F. ) ;
#137400 = CARTESIAN_POINT ( 'NONE',  ( -33.48921356237309510, -27.52281430457078670, 5.000000000000000000 ) ) ;
#137401 = DIRECTION ( 'NONE',  ( -1.000000000000000000, -0.000000000000000000, -0.000000000000000000 ) ) ;
#137402 = VECTOR ( 'NONE', #129386, 1000.000000000000000 ) ;
#137403 = DIRECTION ( 'NONE',  ( -0.7071067811865486830, -0.7071067811865464625, 0.000000000000000000 ) ) ;
#137404 = VERTEX_POINT ( 'NONE', #135107 ) ;
#137405 = DIRECTION ( 'NONE',  ( 0.7071067811865487940, -0.7071067811865463515, 0.000000000000000000 ) ) ;
#137406 = DIRECTION ( 'NONE',  ( 0.7071067811865487940, -0.7071067811865463515, 0.000000000000000000 ) ) ;
#137407 = AXIS2_PLACEMENT_3D ( 'NONE', #12613, #122083, #44588 ) ;
#137408 = CARTESIAN_POINT ( 'NONE',  ( -19.49999999999985789, 22.08746187583901843, 4.000000000000000000 ) ) ;
#137410 = DIRECTION ( 'NONE',  ( -1.000000000000000000, -1.224606353822377258E-16, -0.000000000000000000 ) ) ;
#137409 = FACE_OUTER_BOUND ( 'NONE', #3655, .T. ) ;
#137411 = CARTESIAN_POINT ( 'NONE',  ( -24.33010218547250503, 17.25929247661553845, 19.83885114516076698 ) ) ;
#137412 = CARTESIAN_POINT ( 'NONE',  ( 17.01793588964200055, 8.788317580041921318, 4.329525704382067630 ) ) ;
#137413 = CARTESIAN_POINT ( 'NONE',  ( -1.823340898400253263, 5.259292476615672562, 15.86257073897098380 ) ) ;
#137414 = EDGE_LOOP ( 'NONE', ( #81297, #36773, #104203, #68831 ) ) ;
#137415 = PLANE ( 'NONE',  #86588 ) ;
#137416 = CARTESIAN_POINT ( 'NONE',  ( 36.48921356237310221, -27.52281430457080802, 5.000000000000000000 ) ) ;
#137417 = VECTOR ( 'NONE', #11164, 1000.000000000000227 ) ;
#137418 = EDGE_CURVE ( 'NONE', #77505, #127735, #101721, .T. ) ;
#137419 = EDGE_LOOP ( 'NONE', ( #106245, #57657, #8117, #95466 ) ) ;
#137420 = ORIENTED_EDGE ( 'NONE', *, *, #83332, .F. ) ;
#137421 = EDGE_CURVE ( 'NONE', #71177, #118545, #121324, .T. ) ;
#137422 = EDGE_CURVE ( 'NONE', #89594, #120060, #45940, .T. ) ;
#137423 = EDGE_LOOP ( 'NONE', ( #37547, #91234, #52569, #38841 ) ) ;
#137424 = CARTESIAN_POINT ( 'NONE',  ( 47.25043019189810423, 3.055000000000002824, -5.291415217122919401 ) ) ;
#137425 = EDGE_LOOP ( 'NONE', ( #94705, #100316, #49697 ) ) ;
#137427 = ADVANCED_FACE ( 'NONE', ( #11835 ), #11105, .F. ) ;
#137426 = CONICAL_SURFACE ( 'NONE', #49504, 2.500000000000000444, 0.9599310885968830309 ) ;
#137428 = ADVANCED_FACE ( 'NONE', ( #43780 ), #66257, .F. ) ;
#137429 = VECTOR ( 'NONE', #82517, 1000.000000000000000 ) ;
#137430 = CARTESIAN_POINT ( 'NONE',  ( 15.06663961620376924, 1.633150327867695095, 6.094999999999988205 ) ) ;
#137431 = CARTESIAN_POINT ( 'NONE',  ( -11.58681024782437596, 8.220342448176232608, -30.10827610979940516 ) ) ;
#137432 = ORIENTED_EDGE ( 'NONE', *, *, #119105, .T. ) ;
#137433 = EDGE_CURVE ( 'NONE', #32019, #19651, #33640, .T. ) ;
#137434 = DIRECTION ( 'NONE',  ( -0.7071067811865486830, -0.7071067811865464625, -0.000000000000000000 ) ) ;
#137435 = ORIENTED_EDGE ( 'NONE', *, *, #126109, .F. ) ;
#137436 = CARTESIAN_POINT ( 'NONE',  ( 31.92500000000002203, -22.26999999999999247, -39.50000000000000000 ) ) ;
#137438 = ORIENTED_EDGE ( 'NONE', *, *, #73594, .T. ) ;
#137437 = CARTESIAN_POINT ( 'NONE',  ( 1.031635159221905962, 2.259292476615694323, 13.77329220150637745 ) ) ;
#137439 = ORIENTED_EDGE ( 'NONE', *, *, #142163, .F. ) ;
#137440 = CARTESIAN_POINT ( 'NONE',  ( 30.48921356237309510, -27.52281430457076894, 5.000000000000000000 ) ) ;
#137441 = DIRECTION ( 'NONE',  ( -0.000000000000000000, 0.3543493200069153248, 0.9351131265310292928 ) ) ;
#137442 = EDGE_CURVE ( 'NONE', #136324, #99127, #960, .T. ) ;
#137443 = ORIENTED_EDGE ( 'NONE', *, *, #2516, .F. ) ;
#137444 = CYLINDRICAL_SURFACE ( 'NONE', #55134, 1.898649999999994842 ) ;
#137445 = VERTEX_POINT ( 'NONE', #133651 ) ;
#137446 = VERTEX_POINT ( 'NONE', #34328 ) ;
#137447 = ORIENTED_EDGE ( 'NONE', *, *, #131029, .T. ) ;
#137448 = ORIENTED_EDGE ( 'NONE', *, *, #124330, .T. ) ;
#137449 = CARTESIAN_POINT ( 'NONE',  ( 5.250000000000000000, -7.464222240803106570E-16, -6.094999999999989981 ) ) ;
#137450 = VECTOR ( 'NONE', #114927, 1000.000000000000227 ) ;
#137451 = EDGE_CURVE ( 'NONE', #117979, #66120, #24168, .T. ) ;
#137452 = CARTESIAN_POINT ( 'NONE',  ( -2.999999999999981792, -0.2811185226894372113, -5.995736974527509311 ) ) ;
#137453 = CARTESIAN_POINT ( 'NONE',  ( -34.92500000000001137, -2.337538124160983610, 4.000000000000000000 ) ) ;
#137454 = DIRECTION ( 'NONE',  ( -0.6830127018922180770, -0.6830127018922204085, -0.2588190451025213501 ) ) ;
#137455 = AXIS2_PLACEMENT_3D ( 'NONE', #63397, #8223, #20539 ) ;
#137456 = ORIENTED_EDGE ( 'NONE', *, *, #80975, .T. ) ;
#137457 = ADVANCED_FACE ( 'NONE', ( #137221 ), #70571, .F. ) ;
#137458 = DIRECTION ( 'NONE',  ( -0.7071067811865486830, -0.7071067811865464625, 0.000000000000000000 ) ) ;
#137459 = CARTESIAN_POINT ( 'NONE',  ( 21.12456980810188867, -6.871911579029512218, 3.967499999999996252 ) ) ;
#137460 = DIRECTION ( 'NONE',  ( -0.000000000000000000, 0.000000000000000000, 1.000000000000000000 ) ) ;
#137461 = VECTOR ( 'NONE', #3308, 1000.000000000000000 ) ;
#137462 = CARTESIAN_POINT ( 'NONE',  ( 23.58838509405153161, 22.22500000000000142, 4.777194822843816802 ) ) ;
#137463 = FACE_OUTER_BOUND ( 'NONE', #115408, .T. ) ;
#137464 = ORIENTED_EDGE ( 'NONE', *, *, #139070, .T. ) ;
#137465 = VERTEX_POINT ( 'NONE', #102464 ) ;
#137467 = ORIENTED_EDGE ( 'NONE', *, *, #33416, .F. ) ;
#137466 = EDGE_CURVE ( 'NONE', #5145, #3084, #16101, .T. ) ;
#137468 = LINE ( 'NONE', #60657, #13944 ) ;
#137469 = CARTESIAN_POINT ( 'NONE',  ( 95.45419371712957002, 6.884901960086283523, 3.975000000000002753 ) ) ;
#137470 = UNCERTAINTY_MEASURE_WITH_UNIT (LENGTH_MEASURE( 1.000000000000000082E-05 ), #57085, 'distance_accuracy_value', 'NONE');
#137471 = CARTESIAN_POINT ( 'NONE',  ( -54.18398860626899705, 28.73617430169825226, 5.000000000000000000 ) ) ;
#137472 = CARTESIAN_POINT ( 'NONE',  ( 45.48921356237309510, -27.52281430457087197, 5.000000000000000000 ) ) ;
#137473 = LINE ( 'NONE', #27253, #99125 ) ;
#137474 = CARTESIAN_POINT ( 'NONE',  ( 70.49543019189810877, 5.291415217122917625, 3.055000000000002380 ) ) ;
#137475 = VECTOR ( 'NONE', #132644, 1000.000000000000000 ) ;
#137476 = CARTESIAN_POINT ( 'NONE',  ( 25.49999999999982236, 21.43112307739196254, 4.000000000000000000 ) ) ;
#137477 = EDGE_CURVE ( 'NONE', #20950, #65937, #69945, .T. ) ;
#137478 = DIRECTION ( 'NONE',  ( -0.3543493200069162685, -0.000000000000000000, -0.9351131265310288487 ) ) ;
#137479 = CARTESIAN_POINT ( 'NONE',  ( 66.18398860626901126, 28.73617430169833753, 5.000000000000000000 ) ) ;
#137480 = CARTESIAN_POINT ( 'NONE',  ( -6.489213562373093325, -27.52281430457059841, 5.000000000000000000 ) ) ;
#137481 = EDGE_CURVE ( 'NONE', #94597, #4103, #114715, .T. ) ;
#137482 = CARTESIAN_POINT ( 'NONE',  ( -12.18398860626900060, 28.73617430169795739, 5.000000000000000000 ) ) ;
#137483 = ORIENTED_EDGE ( 'NONE', *, *, #36727, .F. ) ;
#137484 = CARTESIAN_POINT ( 'NONE',  ( -41.99451991528749062, 28.92564299267967343, 4.000000000000000000 ) ) ;
#137485 = VERTEX_POINT ( 'NONE', #15389 ) ;
#137486 = EDGE_CURVE ( 'NONE', #99466, #138500, #13400, .T. ) ;
#137487 = PLANE ( 'NONE',  #50600 ) ;
#137489 = ORIENTED_EDGE ( 'NONE', *, *, #79689, .T. ) ;
#137488 = PLANE ( 'NONE',  #81213 ) ;
#137490 = DIRECTION ( 'NONE',  ( -0.7071067811865486830, -0.7071067811865464625, 0.000000000000000000 ) ) ;
#137491 = CARTESIAN_POINT ( 'NONE',  ( 17.99999999999986855, -19.44781430457062044, 5.000000000000000000 ) ) ;
#137492 = ORIENTED_EDGE ( 'NONE', *, *, #84935, .F. ) ;
#137493 = CARTESIAN_POINT ( 'NONE',  ( 5.848407645496676466, 2.500000000000002220, 3.061616997868384620E-16 ) ) ;
#137494 = ORIENTED_EDGE ( 'NONE', *, *, #83883, .T. ) ;
#137495 = FACE_OUTER_BOUND ( 'NONE', #135340, .T. ) ;
#137496 = ORIENTED_EDGE ( 'NONE', *, *, #67665, .F. ) ;
#137497 = AXIS2_PLACEMENT_3D ( 'NONE', #126510, #135974, #71445 ) ;
#137498 = LINE ( 'NONE', #37477, #45033 ) ;
#137499 = CARTESIAN_POINT ( 'NONE',  ( 98.22502705046289861, 5.819803920172573086, -5.819803920172572198 ) ) ;
#137500 = CARTESIAN_POINT ( 'NONE',  ( 53.99451991528749062, 28.92564299267975869, 4.000000000000000000 ) ) ;
#137501 = VECTOR ( 'NONE', #23157, 1000.000000000000000 ) ;
#137502 = ORIENTED_EDGE ( 'NONE', *, *, #45677, .T. ) ;
#137503 = EDGE_CURVE ( 'NONE', #20582, #105080, #4480, .T. ) ;
#137504 = DIRECTION ( 'NONE',  ( -0.000000000000000000, -1.000000000000000000, -0.000000000000000000 ) ) ;
#137505 = CARTESIAN_POINT ( 'NONE',  ( 12.49289321881344961, -34.94289321881345955, -40.00000000000000000 ) ) ;
#137506 = CARTESIAN_POINT ( 'NONE',  ( 25.95833333333333570, -3.047499999999997211, -5.278424836066143655 ) ) ;
#137507 = DIRECTION ( 'NONE',  ( -0.6830127018922180770, -0.6830127018922204085, -0.2588190451025213501 ) ) ;
#137508 = CARTESIAN_POINT ( 'NONE',  ( 20.36090904532357371, -2.649219295539896990, 4.327832195654623071 ) ) ;
#137509 = VERTEX_POINT ( 'NONE', #27012 ) ;
#137510 = ADVANCED_FACE ( 'NONE', ( #58277 ), #127028, .T. ) ;
#137511 = CIRCLE ( 'NONE', #35608, 5.968999999999998529 ) ;
#137512 = LINE ( 'NONE', #125198, #2618 ) ;
#137513 = ORIENTED_EDGE ( 'NONE', *, *, #74699, .T. ) ;
#137514 = VECTOR ( 'NONE', #74891, 1000.000000000000000 ) ;
#137515 = CARTESIAN_POINT ( 'NONE',  ( 88.66709685856477563, -3.055000000000000160, -5.291415217122921177 ) ) ;
#137516 = DIRECTION ( 'NONE',  ( 0.7071067811865487940, -0.7071067811865463515, 0.000000000000000000 ) ) ;
#137517 = CARTESIAN_POINT ( 'NONE',  ( 166.8575281714868481, 26.96999999999994202, 31.92499999999998295 ) ) ;
#137518 = PLANE ( 'NONE',  #27085 ) ;
#137519 = ORIENTED_EDGE ( 'NONE', *, *, #89920, .T. ) ;
#137520 = CARTESIAN_POINT ( 'NONE',  ( -28.49999999999979039, 16.08746187583907883, 4.000000000000000000 ) ) ;
#137521 = AXIS2_PLACEMENT_3D ( 'NONE', #96327, #16658, #93517 ) ;
#137522 = DIRECTION ( 'NONE',  ( 0.3543493200069162685, -0.000000000000000000, -0.9351131265310288487 ) ) ;
#137523 = ADVANCED_FACE ( 'NONE', ( #80708 ), #66631, .T. ) ;
#137524 = VECTOR ( 'NONE', #88604, 1000.000000000000000 ) ;
#137525 = CARTESIAN_POINT ( 'NONE',  ( -75.18398860626899705, 28.73617430169839793, 5.000000000000000000 ) ) ;
#137527 = EDGE_CURVE ( 'NONE', #125882, #71945, #92992, .T. ) ;
#137526 = CARTESIAN_POINT ( 'NONE',  ( -9.183988606268997046, 28.73617430169793607, 5.000000000000000000 ) ) ;
#137529 = ORIENTED_EDGE ( 'NONE', *, *, #32698, .F. ) ;
#137528 = CARTESIAN_POINT ( 'NONE',  ( -3.005480084712505828, 28.92564299267936079, 4.000000000000000000 ) ) ;
#137530 = CARTESIAN_POINT ( 'NONE',  ( 13.27083333333333393, 6.094999999999991758, 1.633150327867686880 ) ) ;
#137531 = LINE ( 'NONE', #49105, #77815 ) ;
#137532 = CARTESIAN_POINT ( 'NONE',  ( 2.962472949537105826, -7.464222240803106570E-16, -6.094999999999989981 ) ) ;
#137533 = CARTESIAN_POINT ( 'NONE',  ( 2.510786437626908008, -27.52281430457053446, 5.000000000000000000 ) ) ;
#137534 = VECTOR ( 'NONE', #97818, 1000.000000000000000 ) ;
#137535 = ORIENTED_EDGE ( 'NONE', *, *, #115701, .T. ) ;
#137536 = ORIENTED_EDGE ( 'NONE', *, *, #142369, .T. ) ;
#137537 = ORIENTED_EDGE ( 'NONE', *, *, #99190, .F. ) ;
#137538 = CARTESIAN_POINT ( 'NONE',  ( 81.37543019189810423, -5.291415217122920289, -3.055000000000001492 ) ) ;
#137539 = VECTOR ( 'NONE', #82895, 999.9999999999998863 ) ;
#137540 = ORIENTED_EDGE ( 'NONE', *, *, #113271, .T. ) ;
#137541 = LINE ( 'NONE', #26626, #28940 ) ;
#137542 = LINE ( 'NONE', #60726, #61933 ) ;
#137543 = VECTOR ( 'NONE', #88103, 1000.000000000000227 ) ;
#137544 = DIRECTION ( 'NONE',  ( 0.6830127018922180770, -0.6830127018922204085, -0.2588190451025213501 ) ) ;
#137545 = LINE ( 'NONE', #138973, #10699 ) ;
#137546 = VERTEX_POINT ( 'NONE', #58991 ) ;
#137547 = PLANE ( 'NONE',  #46839 ) ;
#137549 = ADVANCED_FACE ( 'NONE', ( #71982, #124903, #48072 ), #105285, .F. ) ;
#137548 = CARTESIAN_POINT ( 'NONE',  ( -4.171830600776438303, -20.24070752338407431, 4.000000000000000000 ) ) ;
#137550 = AXIS2_PLACEMENT_3D ( 'NONE', #128333, #140602, #6478 ) ;
#137551 = EDGE_CURVE ( 'NONE', #60350, #116152, #36471, .T. ) ;
#137552 = EDGE_LOOP ( 'NONE', ( #90566, #137438, #30086, #10031 ) ) ;
#137553 = DIRECTION ( 'NONE',  ( 0.7071067811865487940, -0.7071067811865463515, 0.000000000000000000 ) ) ;
#137554 = DIRECTION ( 'NONE',  ( 0.6830127018922181881, 0.6830127018922202975, -0.2588190451025214056 ) ) ;
#137555 = VECTOR ( 'NONE', #48471, 1000.000000000000227 ) ;
#137556 = LINE ( 'NONE', #33110, #104836 ) ;
#137557 = VERTEX_POINT ( 'NONE', #20397 ) ;
#137558 = ORIENTED_EDGE ( 'NONE', *, *, #98474, .T. ) ;
#137559 = DIRECTION ( 'NONE',  ( 1.000000000000000000, 0.000000000000000000, 0.000000000000000000 ) ) ;
#137560 = EDGE_CURVE ( 'NONE', #20628, #44804, #30610, .T. ) ;
#137561 = DIRECTION ( 'NONE',  ( -0.3543493200069162685, -0.000000000000000000, -0.9351131265310288487 ) ) ;
#137562 = FACE_OUTER_BOUND ( 'NONE', #141403, .T. ) ;
#137563 = LINE ( 'NONE', #38246, #65057 ) ;
#137564 = DIRECTION ( 'NONE',  ( 0.6830127018922180770, -0.6830127018922204085, -0.2588190451025213501 ) ) ;
#137565 = DIRECTION ( 'NONE',  ( 0.6830127018922181881, 0.6830127018922202975, -0.2588190451025214056 ) ) ;
#137566 = ORIENTED_EDGE ( 'NONE', *, *, #118806, .F. ) ;
#137567 = VECTOR ( 'NONE', #50962, 1000.000000000000000 ) ;
#137568 = EDGE_LOOP ( 'NONE', ( #36763, #138387, #135465, #140479 ) ) ;
#137569 = ORIENTED_EDGE ( 'NONE', *, *, #84611, .F. ) ;
#137570 = ORIENTED_EDGE ( 'NONE', *, *, #9643, .T. ) ;
#137571 = DIRECTION ( 'NONE',  ( -1.000000000000000000, -0.000000000000000000, -0.000000000000000000 ) ) ;
#137572 = CARTESIAN_POINT ( 'NONE',  ( -34.92500000000001137, 22.22500000000000142, 4.000000000000000000 ) ) ;
#137573 = VERTEX_POINT ( 'NONE', #72726 ) ;
#137574 = LINE ( 'NONE', #125264, #43622 ) ;
#137575 = CARTESIAN_POINT ( 'NONE',  ( 0.000000000000000000, 0.000000000000000000, 5.000000000000000000 ) ) ;
#137577 = EDGE_CURVE ( 'NONE', #124775, #22382, #52330, .T. ) ;
#137576 = CARTESIAN_POINT ( 'NONE',  ( 4.495848767239241539, 3.061616997868383634E-16, -2.500000000000000444 ) ) ;
#137578 = CARTESIAN_POINT ( 'NONE',  ( 21.15294044719737698, 3.821174125832445049E-16, 0.000000000000000000 ) ) ;
#137579 = LINE ( 'NONE', #105623, #76900 ) ;
#137580 = ORIENTED_EDGE ( 'NONE', *, *, #58965, .F. ) ;
#137581 = EDGE_CURVE ( 'NONE', #4118, #558, #140084, .T. ) ;
#137582 = FACE_OUTER_BOUND ( 'NONE', #106482, .T. ) ;
#137583 = DIRECTION ( 'NONE',  ( -0.6830127018922181881, 0.6830127018922202975, -0.2588190451025214056 ) ) ;
#137584 = ORIENTED_EDGE ( 'NONE', *, *, #44311, .T. ) ;
#137585 = DIRECTION ( 'NONE',  ( 0.7071067811865487940, -0.7071067811865463515, 0.000000000000000000 ) ) ;
#137586 = VERTEX_POINT ( 'NONE', #142229 ) ;
#137588 = ORIENTED_EDGE ( 'NONE', *, *, #79071, .T. ) ;
#137587 = ADVANCED_FACE ( 'NONE', ( #9512 ), #92061, .T. ) ;
#137589 = ADVANCED_FACE ( 'NONE', ( #108826 ), #18241, .F. ) ;
#137590 = CARTESIAN_POINT ( 'NONE',  ( -9.793339364578404371, 21.75929247661549581, 4.998822639870701856 ) ) ;
#137591 = EDGE_LOOP ( 'NONE', ( #90086, #8800, #97078, #126813 ) ) ;
#137592 = ORIENTED_EDGE ( 'NONE', *, *, #126311, .T. ) ;
#137593 = CARTESIAN_POINT ( 'NONE',  ( 71.16709685856477563, -3.055000000000000160, -5.291415217122921177 ) ) ;
#137594 = VECTOR ( 'NONE', #74123, 999.9999999999998863 ) ;
#137595 = ORIENTED_EDGE ( 'NONE', *, *, #89910, .F. ) ;
#137596 = ADVANCED_FACE ( 'NONE', ( #53792 ), #61814, .F. ) ;
#137597 = EDGE_CURVE ( 'NONE', #1418, #140272, #18996, .T. ) ;
#137598 = PLANE ( 'NONE',  #44303 ) ;
#137599 = VECTOR ( 'NONE', #109309, 999.9999999999998863 ) ;
#137601 = EDGE_CURVE ( 'NONE', #29556, #68546, #40764, .T. ) ;
#137600 = DIRECTION ( 'NONE',  ( -0.7071067811865486830, -0.7071067811865464625, -0.000000000000000000 ) ) ;
#137602 = CARTESIAN_POINT ( 'NONE',  ( 105.8754301918981042, -5.291415217122920289, -3.055000000000001492 ) ) ;
#137603 = CARTESIAN_POINT ( 'NONE',  ( -22.49999999999984013, -11.94781430457070392, 5.000000000000000000 ) ) ;
#137604 = VECTOR ( 'NONE', #17136, 1000.000000000000000 ) ;
#137605 = EDGE_CURVE ( 'NONE', #124676, #30730, #129171, .T. ) ;
#137606 = CYLINDRICAL_SURFACE ( 'NONE', #80658, 1.898649999999994842 ) ;
#137607 = DIRECTION ( 'NONE',  ( -0.6830127018922181881, 0.6830127018922202975, -0.2588190451025214056 ) ) ;
#137608 = PLANE ( 'NONE',  #69522 ) ;
#137609 = CARTESIAN_POINT ( 'NONE',  ( 9.489213562373095101, -27.52281430457062328, 5.000000000000000000 ) ) ;
#137610 = ADVANCED_FACE ( 'NONE', ( #108110 ), #129898, .F. ) ;
#137611 = DIRECTION ( 'NONE',  ( -0.7071067811865486830, -0.7071067811865464625, 0.000000000000000000 ) ) ;
#137612 = DIRECTION ( 'NONE',  ( -0.000000000000000000, -0.3543493200069152693, 0.9351131265310292928 ) ) ;
#137613 = FILL_AREA_STYLE_COLOUR ( '', #98405 ) ;
#137614 = EDGE_CURVE ( 'NONE', #7434, #61259, #8775, .T. ) ;
#137615 = ORIENTED_EDGE ( 'NONE', *, *, #49381, .T. ) ;
#137616 = DIRECTION ( 'NONE',  ( -0.000000000000000000, 1.000000000000000000, -0.000000000000000000 ) ) ;
#137618 = PLANE ( 'NONE',  #109977 ) ;
#137617 = VECTOR ( 'NONE', #41894, 1000.000000000000000 ) ;
#137619 = ORIENTED_EDGE ( 'NONE', *, *, #74717, .T. ) ;
#137620 = VERTEX_POINT ( 'NONE', #787 ) ;
#137621 = LINE ( 'NONE', #38301, #3187 ) ;
#137622 = ORIENTED_EDGE ( 'NONE', *, *, #45840, .T. ) ;
#137623 = DIRECTION ( 'NONE',  ( 0.7071067811865487940, -0.7071067811865463515, 0.000000000000000000 ) ) ;
#137624 = DIRECTION ( 'NONE',  ( 0.7071067811865487940, 0.7071067811865463515, -0.000000000000000000 ) ) ;
#137626 = ADVANCED_FACE ( 'NONE', ( #34166 ), #101540, .T. ) ;
#137625 = LINE ( 'NONE', #126708, #52570 ) ;
#137627 = AXIS2_PLACEMENT_3D ( 'NONE', #91113, #103361, #92492 ) ;
#137628 = CARTESIAN_POINT ( 'NONE',  ( 16.49999999999988631, -17.94781430457065952, 5.000000000000000000 ) ) ;
#137629 = DIRECTION ( 'NONE',  ( -0.000000000000000000, 0.3543493200069153248, 0.9351131265310292928 ) ) ;
#137630 = ORIENTED_EDGE ( 'NONE', *, *, #77692, .T. ) ;
#137631 = EDGE_LOOP ( 'NONE', ( #81680, #141759, #79712, #9930 ) ) ;
#137632 = EDGE_CURVE ( 'NONE', #40894, #24671, #132058, .T. ) ;
#137634 = CIRCLE ( 'NONE', #132996, 0.5000000000000004441 ) ;
#137633 = LINE ( 'NONE', #53267, #111699 ) ;
#137635 = VECTOR ( 'NONE', #124945, 1000.000000000000000 ) ;
#137636 = CARTESIAN_POINT ( 'NONE',  ( 30.40040314143521982, -7.934999999999989839, 2.126176841940957907 ) ) ;
#137637 = LINE ( 'NONE', #128872, #23854 ) ;
#137638 = VECTOR ( 'NONE', #57968, 1000.000000000000000 ) ;
#137639 = DIRECTION ( 'NONE',  ( -1.000000000000000000, -1.224606353822377258E-16, -0.000000000000000000 ) ) ;
#137640 = PLANE ( 'NONE',  #120679 ) ;
#137641 = ORIENTED_EDGE ( 'NONE', *, *, #38086, .T. ) ;
#137642 = ORIENTED_EDGE ( 'NONE', *, *, #35240, .T. ) ;
#137643 = EDGE_LOOP ( 'NONE', ( #112984, #83573, #25101, #83037 ) ) ;
#137644 = DIRECTION ( 'NONE',  ( -0.7071067811865486830, -0.7071067811865464625, 0.000000000000000000 ) ) ;
#137645 = DIRECTION ( 'NONE',  ( -1.000000000000000000, -1.224606353822377258E-16, -0.000000000000000000 ) ) ;
#137646 = CARTESIAN_POINT ( 'NONE',  ( -13.22850677138656472, 20.25929247661551358, 7.808871592221738211 ) ) ;
#137647 = DIRECTION ( 'NONE',  ( -0.7071067811865486830, -0.7071067811865464625, 0.000000000000000000 ) ) ;
#137648 =( BOUNDED_CURVE ( )  B_SPLINE_CURVE ( 2, ( #104854, #27279, #71534, #115689, #16390, #60691, #91830, #5519, #83114, #127316, #72286, #17140, #105549 ),
 .UNSPECIFIED., .F., .F. ) 
 B_SPLINE_CURVE_WITH_KNOTS ( ( 3, 2, 2, 2, 2, 2, 3 ),
 ( 0.5166666666666667185, 0.5194444444444444864, 0.5222222222222222543, 0.5250000000000001332, 0.5277777777777779011, 0.5305555555555556690, 0.5333333333333334370 ),
 .UNSPECIFIED. ) 
 CURVE ( )  GEOMETRIC_REPRESENTATION_ITEM ( )  RATIONAL_B_SPLINE_CURVE ( ( 1.000000000000000000, 0.9659258262890683122, 1.000000000000000000, 0.9659258262890683122, 1.000000000000000000, 0.9659258262890683122, 1.000000000000000000, 0.9659258262890683122, 1.000000000000000000, 0.9659258262890683122, 1.000000000000000000, 0.9659258262890669799, 1.000000000000001332 ) ) 
 REPRESENTATION_ITEM ( '' )  );
#137649 = DIRECTION ( 'NONE',  ( 0.5735764363510453823, -0.8191520442889923537, 1.003171929053525486E-16 ) ) ;
#137650 = DIRECTION ( 'NONE',  ( -0.000000000000000000, -0.3543493200069152693, 0.9351131265310292928 ) ) ;
#137651 = AXIS2_PLACEMENT_3D ( 'NONE', #27921, #4680, #29335 ) ;
#137652 = EDGE_CURVE ( 'NONE', #22185, #115243, #78384, .T. ) ;
#137653 = CARTESIAN_POINT ( 'NONE',  ( 34.92499999999998295, 7.701930566820908375, 4.500000000000000888 ) ) ;
#137654 = DIRECTION ( 'NONE',  ( -0.7071067811865486830, -0.7071067811865464625, -0.000000000000000000 ) ) ;
#137655 = CARTESIAN_POINT ( 'NONE',  ( 34.75611968250419181, -9.187065745292510854, 4.955485411084881164 ) ) ;
#137656 = EDGE_CURVE ( 'NONE', #57981, #134318, #66090, .T. ) ;
#137657 = ORIENTED_EDGE ( 'NONE', *, *, #101327, .T. ) ;
#137658 = CARTESIAN_POINT ( 'NONE',  ( -14.20710678118644132, -8.240707523384200428, 5.000000000000000000 ) ) ;
#137659 = LINE ( 'NONE', #38333, #70249 ) ;
#137660 = ORIENTED_EDGE ( 'NONE', *, *, #98533, .F. ) ;
#137661 = EDGE_CURVE ( 'NONE', #132130, #9981, #68258, .T. ) ;
#137662 = LINE ( 'NONE', #24072, #15885 ) ;
#137664 = VERTEX_POINT ( 'NONE', #131328 ) ;
#137663 = CARTESIAN_POINT ( 'NONE',  ( 0.000000000000000000, 0.000000000000000000, 5.000000000000000000 ) ) ;
#137665 = ORIENTED_EDGE ( 'NONE', *, *, #83477, .T. ) ;
#137666 = CARTESIAN_POINT ( 'NONE',  ( -57.18398860626899705, 28.73617430169827358, 5.000000000000000000 ) ) ;
#137667 = DIRECTION ( 'NONE',  ( -1.000000000000000000, 6.938893903907222067E-15, 0.000000000000000000 ) ) ;
#137668 = CARTESIAN_POINT ( 'NONE',  ( 42.48921356237308800, -27.52281430457085065, 5.000000000000000000 ) ) ;
#137669 = EDGE_LOOP ( 'NONE', ( #132341, #122524, #142210, #100341 ) ) ;
#137670 = CARTESIAN_POINT ( 'NONE',  ( -21.48921356237309155, -27.52281430457070499, 5.000000000000000000 ) ) ;
#137671 = UNCERTAINTY_MEASURE_WITH_UNIT (LENGTH_MEASURE( 1.000000000000000082E-05 ), #108838, 'distance_accuracy_value', 'NONE');
#137672 = EDGE_LOOP ( 'NONE', ( #4205, #45714, #129094, #133682 ) ) ;
#137673 = EDGE_CURVE ( 'NONE', #77465, #12213, #121150, .T. ) ;
#137674 = DIRECTION ( 'NONE',  ( -0.3543493200069162685, -0.000000000000000000, -0.9351131265310288487 ) ) ;
#137675 = CARTESIAN_POINT ( 'NONE',  ( 0.3605399447480615582, 0.3999999999999995781, 2.166563668000046405 ) ) ;
#137676 = CARTESIAN_POINT ( 'NONE',  ( 29.51626352523143737, -4.472830434245839371, 4.472830434245839371 ) ) ;
#137677 = CARTESIAN_POINT ( 'NONE',  ( 25.00000000000000000, 0.000000000000000000, 1.749999999999999778 ) ) ;
#137678 = DIRECTION ( 'NONE',  ( 0.7071067811865487940, 0.7071067811865463515, 0.000000000000000000 ) ) ;
#137679 = ADVANCED_FACE ( 'NONE', ( #123334 ), #11651, .F. ) ;
#137680 = DIRECTION ( 'NONE',  ( -0.6830127018922181881, 0.6830127018922202975, -0.2588190451025214056 ) ) ;
#137681 = DIRECTION ( 'NONE',  ( 0.7071067811865487940, 0.7071067811865463515, 0.000000000000000000 ) ) ;
#137682 = CARTESIAN_POINT ( 'NONE',  ( -17.99999999999987566, -7.068876922607736368, 4.000000000000000000 ) ) ;
#137683 = CARTESIAN_POINT ( 'NONE',  ( 33.81206980810188156, 7.934999999999993392, 2.126176841940951689 ) ) ;
#137684 = CARTESIAN_POINT ( 'NONE',  ( 3.624569808101886448, -6.871911579029512218, 3.967499999999996252 ) ) ;
#137685 = LINE ( 'NONE', #53322, #71413 ) ;
#137686 = DIRECTION ( 'NONE',  ( -0.7071067811865486830, -0.7071067811865464625, 0.000000000000000000 ) ) ;
#137687 = CARTESIAN_POINT ( 'NONE',  ( 6.005480084712508493, 28.92564299267933947, 4.000000000000000000 ) ) ;
#137688 = ORIENTED_EDGE ( 'NONE', *, *, #36182, .F. ) ;
#137689 = CIRCLE ( 'NONE', #21964, 2.500000000000000888 ) ;
#137690 = ORIENTED_EDGE ( 'NONE', *, *, #59090, .F. ) ;
#137691 = CARTESIAN_POINT ( 'NONE',  ( 89.08333333333332860, 6.884901960086290629, -3.974999999999994316 ) ) ;
#137692 = EDGE_LOOP ( 'NONE', ( #32198, #2829, #125599, #22779 ) ) ;
#137693 = EDGE_LOOP ( 'NONE', ( #48216, #42767, #107962, #80404 ) ) ;
#137694 = EDGE_CURVE ( 'NONE', #141201, #84993, #32749, .T. ) ;
#137695 = SURFACE_STYLE_FILL_AREA ( #93460 ) ;
#137696 = LINE ( 'NONE', #50660, #101904 ) ;
#137697 = CARTESIAN_POINT ( 'NONE',  ( -6.489213562373093325, -27.52281430457059841, 5.000000000000000000 ) ) ;
#137698 = VERTEX_POINT ( 'NONE', #45080 ) ;
#137699 = DIRECTION ( 'NONE',  ( 1.000000000000000000, 1.224606353822377258E-16, 0.000000000000000000 ) ) ;
#137700 = DIRECTION ( 'NONE',  ( -0.7071067811865486830, -0.7071067811865464625, 0.000000000000000000 ) ) ;
#137701 = CARTESIAN_POINT ( 'NONE',  ( -78.29974487139158157, -27.71228299555260577, 4.000000000000000000 ) ) ;
#137702 = CARTESIAN_POINT ( 'NONE',  ( 126.1800681914572522, 6.167271031922632041, -3.881961135379007111 ) ) ;
#137703 = ADVANCED_FACE ( 'NONE', ( #98683 ), #10244, .F. ) ;
#137704 = DIRECTION ( 'NONE',  ( -0.7071067811865487940, 0.7071067811865463515, 0.000000000000000000 ) ) ;
#137705 = DIRECTION ( 'NONE',  ( -0.7071067811865486830, 0.7071067811865464625, 0.000000000000000000 ) ) ;
#137706 = DIRECTION ( 'NONE',  ( 0.7071067811865487940, -0.7071067811865463515, 0.000000000000000000 ) ) ;
#137707 = DIRECTION ( 'NONE',  ( 0.7071067811865486830, -0.7071067811865464625, -0.000000000000000000 ) ) ;
#137708 = PLANE ( 'NONE',  #44776 ) ;
#137709 = CARTESIAN_POINT ( 'NONE',  ( 34.82816939922329169, 15.75929247661555976, 4.000000000000000000 ) ) ;
#137710 = CARTESIAN_POINT ( 'NONE',  ( 0.000000000000000000, 0.000000000000000000, 5.000000000000000000 ) ) ;
#137711 = CARTESIAN_POINT ( 'NONE',  ( -34.92500000000001137, -13.29806943317885448, 4.500000000000000888 ) ) ;
#137712 = VECTOR ( 'NONE', #45717, 1000.000000000000000 ) ;
#137713 = EDGE_CURVE ( 'NONE', #52975, #16650, #76242, .T. ) ;
#137714 = ORIENTED_EDGE ( 'NONE', *, *, #43413, .T. ) ;
#137715 = ORIENTED_EDGE ( 'NONE', *, *, #115636, .T. ) ;
#137716 = CARTESIAN_POINT ( 'NONE',  ( 111.5629301918981184, 1.637169565754157174, 6.110000000000002984 ) ) ;
#137717 = ORIENTED_EDGE ( 'NONE', *, *, #124181, .F. ) ;
#137718 = AXIS2_PLACEMENT_3D ( 'NONE', #51751, #95944, #138757 ) ;
#137719 = LINE ( 'NONE', #37697, #54791 ) ;
#137720 = CARTESIAN_POINT ( 'NONE',  ( 19.49999999999987210, -7.912538124160673370, 4.000000000000000000 ) ) ;
#137721 = ORIENTED_EDGE ( 'NONE', *, *, #134375, .T. ) ;
#137722 = CARTESIAN_POINT ( 'NONE',  ( 18.17159235450331778, 3.061616997868380183E-16, -2.500000000000001332 ) ) ;
#137724 = EDGE_CURVE ( 'NONE', #88957, #11432, #48, .T. ) ;
#137723 = LINE ( 'NONE', #40548, #81317 ) ;
#137725 = CARTESIAN_POINT ( 'NONE',  ( 106.2245968585647802, -1.637169565754160949, 6.109999999999997655 ) ) ;
#137726 = EDGE_CURVE ( 'NONE', #54291, #76385, #89254, .T. ) ;
#137727 = VECTOR ( 'NONE', #93239, 1000.000000000000000 ) ;
#137728 = EDGE_LOOP ( 'NONE', ( #17823, #95608, #101296, #75929, #139415 ) ) ;
#137729 = CARTESIAN_POINT ( 'NONE',  ( 39.29974487139159578, -27.71228299555233576, 4.000000000000000000 ) ) ;
#137730 = VERTEX_POINT ( 'NONE', #65392 ) ;
#137731 = DIRECTION ( 'NONE',  ( -0.000000000000000000, -0.3543493200069152693, 0.9351131265310292928 ) ) ;
#137732 = CARTESIAN_POINT ( 'NONE',  ( -23.99999999999982947, -10.06887692260771239, 4.000000000000000000 ) ) ;
#137733 = FACE_OUTER_BOUND ( 'NONE', #88877, .T. ) ;
#137734 = ORIENTED_EDGE ( 'NONE', *, *, #7381, .F. ) ;
#137735 = ORIENTED_EDGE ( 'NONE', *, *, #23702, .T. ) ;
#137736 = EDGE_LOOP ( 'NONE', ( #132221, #128050, #129182, #95755 ) ) ;
#137737 = LINE ( 'NONE', #93502, #97724 ) ;
#137738 = ADVANCED_FACE ( 'NONE', ( #54505 ), #133480, .T. ) ;
#137739 = CARTESIAN_POINT ( 'NONE',  ( 27.99999999999999645, -57.14999999999999147, -53.92499999999967741 ) ) ;
#137740 = CARTESIAN_POINT ( 'NONE',  ( 7.067069808101885897, 2.126176841940952134, -7.934999999999992504 ) ) ;
#137741 = LINE ( 'NONE', #45921, #78112 ) ;
#137742 = VECTOR ( 'NONE', #75471, 1000.000000000000000 ) ;
#137743 = STYLED_ITEM ( 'NONE', ( #135672 ), #44864 ) ;
#137744 = CARTESIAN_POINT ( 'NONE',  ( 181.1500000000000057, -3.180000000000061444, 31.92499999999998295 ) ) ;
#137745 = ORIENTED_EDGE ( 'NONE', *, *, #104864, .F. ) ;
#137747 = ORIENTED_EDGE ( 'NONE', *, *, #44024, .T. ) ;
#137746 = AXIS2_PLACEMENT_3D ( 'NONE', #113659, #91238, #124548 ) ;
#137748 = CARTESIAN_POINT ( 'NONE',  ( 20.91508676806225253, -12.74070752338414536, 18.74364270924359133 ) ) ;
#137749 = ORIENTED_EDGE ( 'NONE', *, *, #126388, .F. ) ;
#137750 = VERTEX_POINT ( 'NONE', #57364 ) ;
#137751 = CARTESIAN_POINT ( 'NONE',  ( 18.18398860626898994, 28.73617430169800002, 5.000000000000000000 ) ) ;
#137752 = LINE ( 'NONE', #47904, #32699 ) ;
#137753 = DIRECTION ( 'NONE',  ( -0.7071067811865487940, 0.7071067811865463515, 0.000000000000000000 ) ) ;
#137754 = ORIENTED_EDGE ( 'NONE', *, *, #106448, .T. ) ;
#137755 = DIRECTION ( 'NONE',  ( -0.7071067811865487940, 0.7071067811865463515, 0.000000000000000000 ) ) ;
#137756 = EDGE_CURVE ( 'NONE', #49688, #89590, #49608, .T. ) ;
#137757 = CARTESIAN_POINT ( 'NONE',  ( -32.22995720542186149, 21.73644205237997440, 5.000000000000000888 ) ) ;
#137758 = CARTESIAN_POINT ( 'NONE',  ( 24.70710678118637915, 11.25929247661560240, 5.000000000000000000 ) ) ;
#137759 = CARTESIAN_POINT ( 'NONE',  ( 10.49999999999993605, -1.912538124160735542, 4.000000000000000000 ) ) ;
#137760 = ORIENTED_EDGE ( 'NONE', *, *, #128662, .T. ) ;
#137761 = LINE ( 'NONE', #137030, #132116 ) ;
#137762 = FACE_BOUND ( 'NONE', #49862, .T. ) ;
#137763 = EDGE_LOOP ( 'NONE', ( #116418, #80650, #89707, #75251 ) ) ;
#137764 = DIRECTION ( 'NONE',  ( 0.000000000000000000, -1.000000000000000000, 0.000000000000000000 ) ) ;
#137765 = DIRECTION ( 'NONE',  ( -0.6830127018922180770, -0.6830127018922204085, -0.2588190451025213501 ) ) ;
#137766 = FACE_OUTER_BOUND ( 'NONE', #78925, .T. ) ;
#137767 = EDGE_LOOP ( 'NONE', ( #13077, #54656, #40581, #1057 ) ) ;
#137768 = DIRECTION ( 'NONE',  ( -0.7071067811865486830, -0.7071067811865464625, -0.000000000000000000 ) ) ;
#137769 = ORIENTED_EDGE ( 'NONE', *, *, #28833, .T. ) ;
#137770 = VERTEX_POINT ( 'NONE', #36304 ) ;
#137771 = VERTEX_POINT ( 'NONE', #115233 ) ;
#137772 = EDGE_CURVE ( 'NONE', #37438, #49326, #60959, .T. ) ;
#137773 = CARTESIAN_POINT ( 'NONE',  ( 36.95376352523144448, -6.109999999999998543, -3.741295971395162543E-16 ) ) ;
#137774 = ORIENTED_EDGE ( 'NONE', *, *, #27952, .F. ) ;
#137775 = LINE ( 'NONE', #37753, #90021 ) ;
#137776 = EDGE_CURVE ( 'NONE', #49544, #44266, #113126, .T. ) ;
#137777 = CARTESIAN_POINT ( 'NONE',  ( 25.49999999999982236, -4.216083040037233332, -7.486842126848716639 ) ) ;
#137778 = LINE ( 'NONE', #72559, #51990 ) ;
#137779 = ADVANCED_FACE ( 'NONE', ( #27538 ), #16674, .F. ) ;
#137780 = CARTESIAN_POINT ( 'NONE',  ( 29.99451991528749417, 28.92564299267958816, 4.000000000000000000 ) ) ;
#137781 = DIRECTION ( 'NONE',  ( -1.000000000000000000, -1.224606353822377258E-16, -0.000000000000000000 ) ) ;
#137782 = EDGE_CURVE ( 'NONE', #23467, #140739, #115970, .T. ) ;
#137783 = CARTESIAN_POINT ( 'NONE',  ( 1.499999999999984013, 12.43112307739206024, 4.000000000000000000 ) ) ;
#137784 = DIRECTION ( 'NONE',  ( 0.7071067811865487940, 0.7071067811865463515, 0.000000000000000000 ) ) ;
#137785 = CARTESIAN_POINT ( 'NONE',  ( 34.92499999999998295, -21.72500000000000142, 5.000000000000000000 ) ) ;
#137786 = DIRECTION ( 'NONE',  ( 0.7071067811865486830, -0.7071067811865464625, -0.000000000000000000 ) ) ;
#137787 = DIRECTION ( 'NONE',  ( -0.7071067811865486830, -0.7071067811865464625, -0.000000000000000000 ) ) ;
#137788 = EDGE_CURVE ( 'NONE', #17208, #84616, #133009, .T. ) ;
#137789 = EDGE_LOOP ( 'NONE', ( #26956, #70939, #68636, #21046 ) ) ;
#137790 = ORIENTED_EDGE ( 'NONE', *, *, #124686, .F. ) ;
#137791 = ORIENTED_EDGE ( 'NONE', *, *, #24427, .F. ) ;
#137792 = ORIENTED_EDGE ( 'NONE', *, *, #84800, .F. ) ;
#137793 = DIRECTION ( 'NONE',  ( 1.000000000000000000, 0.000000000000000000, 0.000000000000000000 ) ) ;
#137794 = ORIENTED_EDGE ( 'NONE', *, *, #113326, .F. ) ;
#137795 = ORIENTED_EDGE ( 'NONE', *, *, #50463, .F. ) ;
#137796 = LINE ( 'NONE', #38471, #127799 ) ;
#137798 = ADVANCED_FACE ( 'NONE', ( #102986 ), #81980, .F. ) ;
#137797 = CARTESIAN_POINT ( 'NONE',  ( -29.99999999999979394, -4.447814304570784749, 5.000000000000000000 ) ) ;
#137799 = ADVANCED_FACE ( 'NONE', ( #80535 ), #38445, .F. ) ;
#137800 = CARTESIAN_POINT ( 'NONE',  ( -34.92499999999997584, 0.4299755680429860338, -27.68972139052992532 ) ) ;
#137801 = VERTEX_POINT ( 'NONE', #35622 ) ;
#137802 = DIRECTION ( 'NONE',  ( 0.7071067811865487940, -0.7071067811865463515, 0.000000000000000000 ) ) ;
#137803 = ORIENTED_EDGE ( 'NONE', *, *, #138310, .T. ) ;
#137804 = ADVANCED_FACE ( 'NONE', ( #79852 ), #126850, .F. ) ;
#137805 = DIRECTION ( 'NONE',  ( 0.6830127018922181881, 0.6830127018922202975, -0.2588190451025214056 ) ) ;
#137806 = AXIS2_PLACEMENT_3D ( 'NONE', #28769, #117166, #73015 ) ;
#137807 = LINE ( 'NONE', #28328, #91287 ) ;
#137808 = CARTESIAN_POINT ( 'NONE',  ( 0.5045698081018860082, 6.871911579029510442, -3.967499999999998916 ) ) ;
#137809 = VERTEX_POINT ( 'NONE', #3622 ) ;
#137811 = LINE ( 'NONE', #39200, #89295 ) ;
#137810 = CARTESIAN_POINT ( 'NONE',  ( 98.93293019189812298, 1.637169565754156730, 6.110000000000001208 ) ) ;
#137812 =( BOUNDED_CURVE ( )  B_SPLINE_CURVE ( 2, ( #49542, #116191, #92275, #73413, #39365, #26335, #127800, #38635, #82866, #95136, #71278, #126346, #127052 ),
 .UNSPECIFIED., .F., .T. ) 
 B_SPLINE_CURVE_WITH_KNOTS ( ( 3, 2, 2, 2, 2, 2, 3 ),
 ( 0.4500000000000000111, 0.4583333333333333148, 0.4666666666666666741, 0.4749999999999999778, 0.4833333333333333370, 0.4916666666666666408, 0.5000000000000000000 ),
 .UNSPECIFIED. ) 
 CURVE ( )  GEOMETRIC_REPRESENTATION_ITEM ( )  RATIONAL_B_SPLINE_CURVE ( ( 1.000000000000000000, 0.9659258262890683122, 1.000000000000000000, 0.9659258262890683122, 1.000000000000000000, 0.9659258262890683122, 1.000000000000000000, 0.9659258262890683122, 1.000000000000000000, 0.9659258262890683122, 1.000000000000000000, 0.9659258262890683122, 1.000000000000000000 ) ) 
 REPRESENTATION_ITEM ( '' )  );
#137813 = VECTOR ( 'NONE', #61069, 999.9999999999998863 ) ;
#137814 = FACE_OUTER_BOUND ( 'NONE', #56738, .T. ) ;
#137815 = ORIENTED_EDGE ( 'NONE', *, *, #44222, .T. ) ;
#137816 = ORIENTED_EDGE ( 'NONE', *, *, #120380, .F. ) ;
#137817 = DIRECTION ( 'NONE',  ( -0.000000000000000000, 0.000000000000000000, 1.000000000000000000 ) ) ;
#137818 = ORIENTED_EDGE ( 'NONE', *, *, #59614, .T. ) ;
#137819 = SURFACE_SIDE_STYLE ('',( #94285 ) ) ;
#137820 = FACE_OUTER_BOUND ( 'NONE', #25711, .T. ) ;
#137821 = CARTESIAN_POINT ( 'NONE',  ( -11.81601139373100651, 28.73617430169779041, 5.000000000000000000 ) ) ;
#137822 = CARTESIAN_POINT ( 'NONE',  ( 183.9257687383477560, -48.73293412427588578, -38.67339632249938575 ) ) ;
#137823 = ORIENTED_EDGE ( 'NONE', *, *, #94990, .F. ) ;
#137824 = LINE ( 'NONE', #125516, #76019 ) ;
#137825 = AXIS2_PLACEMENT_3D ( 'NONE', #103737, #50825, #5848 ) ;
#137826 = LINE ( 'NONE', #126224, #85834 ) ;
#137827 = CARTESIAN_POINT ( 'NONE',  ( 12.19999999999999574, -60.26999999999998892, 25.00000000000000000 ) ) ;
#137828 = EDGE_CURVE ( 'NONE', #65645, #30899, #24697, .T. ) ;
#137829 = ORIENTED_EDGE ( 'NONE', *, *, #50333, .T. ) ;
#137830 = FACE_OUTER_BOUND ( 'NONE', #47952, .T. ) ;
#137831 = CARTESIAN_POINT ( 'NONE',  ( -26.99999999999980460, -13.06887692260767686, 4.000000000000000000 ) ) ;
#137832 = EDGE_LOOP ( 'NONE', ( #138165, #33317, #106906, #80376 ) ) ;
#137834 = VERTEX_POINT ( 'NONE', #47919 ) ;
#137833 = DIRECTION ( 'NONE',  ( 0.7071067811865486830, -0.7071067811865463515, 0.000000000000000000 ) ) ;
#137835 = ORIENTED_EDGE ( 'NONE', *, *, #125672, .T. ) ;
#137836 = DIRECTION ( 'NONE',  ( 0.000000000000000000, -1.000000000000000000, 0.000000000000000000 ) ) ;
#137837 = DIRECTION ( 'NONE',  ( -0.000000000000000000, -0.000000000000000000, -1.000000000000000000 ) ) ;
#137838 = ORIENTED_EDGE ( 'NONE', *, *, #139058, .T. ) ;
#137839 = CARTESIAN_POINT ( 'NONE',  ( 11.56505274454301357, 3.061616997868383634E-16, -2.500000000000000444 ) ) ;
#137840 = UNCERTAINTY_MEASURE_WITH_UNIT (LENGTH_MEASURE( 1.000000000000000082E-05 ), #139915, 'distance_accuracy_value', 'NONE');
#137841 = EDGE_CURVE ( 'NONE', #5588, #1674, #92084, .T. ) ;
#137842 = VECTOR ( 'NONE', #88319, 999.9999999999998863 ) ;
#137843 = VECTOR ( 'NONE', #38126, 1000.000000000000000 ) ;
#137844 = VECTOR ( 'NONE', #88864, 1000.000000000000000 ) ;
#137845 = DIRECTION ( 'NONE',  ( 0.000000000000000000, -1.000000000000000000, 0.000000000000000000 ) ) ;
#137846 = ORIENTED_EDGE ( 'NONE', *, *, #90310, .T. ) ;
#137847 = CIRCLE ( 'NONE', #15078, 2.552699999999994418 ) ;
#137848 = CARTESIAN_POINT ( 'NONE',  ( 18.48921356237309510, -27.52281430457068367, 5.000000000000000000 ) ) ;
#137849 = DIRECTION ( 'NONE',  ( 0.7071067811865486830, -0.7071067811865464625, -0.000000000000000000 ) ) ;
#137850 = EDGE_CURVE ( 'NONE', #84275, #22022, #92807, .T. ) ;
#137851 = FACE_OUTER_BOUND ( 'NONE', #33434, .T. ) ;
#137852 = CARTESIAN_POINT ( 'NONE',  ( -34.92500000000001137, -4.487538124160448838, 4.000000000000000000 ) ) ;
#137853 = DIRECTION ( 'NONE',  ( -0.7071067811865486830, -0.7071067811865464625, -0.000000000000000000 ) ) ;
#137854 = DIRECTION ( 'NONE',  ( 0.7071067811865486830, -0.7071067811865464625, -0.000000000000000000 ) ) ;
#137855 = CARTESIAN_POINT ( 'NONE',  ( 26.19059147121573972, 3.175000000000004263, -5.499261314031186565 ) ) ;
#137856 = CARTESIAN_POINT ( 'NONE',  ( -34.49999999999975842, 4.464255608400450548, 4.994342998332166772 ) ) ;
#137857 = DIRECTION ( 'NONE',  ( 0.6830127018922181881, 0.6830127018922202975, -0.2588190451025214056 ) ) ;
#137858 = ORIENTED_EDGE ( 'NONE', *, *, #15934, .F. ) ;
#137859 = ORIENTED_EDGE ( 'NONE', *, *, #17761, .T. ) ;
#137860 = ORIENTED_EDGE ( 'NONE', *, *, #78620, .T. ) ;
#137861 = CARTESIAN_POINT ( 'NONE',  ( 117.3750000000000000, 7.950000000000000178, 1.460391307983218535E-15 ) ) ;
#137862 = VERTEX_POINT ( 'NONE', #135618 ) ;
#137863 = ORIENTED_EDGE ( 'NONE', *, *, #73594, .F. ) ;
#137864 = EDGE_CURVE ( 'NONE', #43048, #130061, #49352, .T. ) ;
#137865 = EDGE_LOOP ( 'NONE', ( #37751, #96434, #108921, #86463 ) ) ;
#137866 = LINE ( 'NONE', #16775, #54898 ) ;
#137867 = CARTESIAN_POINT ( 'NONE',  ( -15.29974487139158867, -27.71228299555216879, 4.000000000000000000 ) ) ;
#137868 = ORIENTED_EDGE ( 'NONE', *, *, #100328, .T. ) ;
#137869 = DIRECTION ( 'NONE',  ( 0.000000000000000000, 1.000000000000000000, 0.000000000000000000 ) ) ;
#137870 = FACE_OUTER_BOUND ( 'NONE', #2563, .T. ) ;
#137871 = DIRECTION ( 'NONE',  ( 0.000000000000000000, -1.000000000000000000, 0.000000000000000000 ) ) ;
#137872 = DIRECTION ( 'NONE',  ( 0.000000000000000000, -1.000000000000000000, 0.000000000000000000 ) ) ;
#137873 = CARTESIAN_POINT ( 'NONE',  ( 112.8754301918981042, -5.291415217122920289, -3.055000000000001492 ) ) ;
#137874 = EDGE_CURVE ( 'NONE', #73824, #71954, #103658, .T. ) ;
#137875 = ORIENTED_EDGE ( 'NONE', *, *, #143232, .F. ) ;
#137876 = CARTESIAN_POINT ( 'NONE',  ( -25.00442415654155681, 3.591886032380943838, 4.000000000000000000 ) ) ;
#137877 = CARTESIAN_POINT ( 'NONE',  ( -21.18398860626899349, 28.73617430169802134, 5.000000000000000000 ) ) ;
#137878 = CARTESIAN_POINT ( 'NONE',  ( -23.99999999999984013, 12.25461709320618553, -10.07315571508702767 ) ) ;
#137879 = CARTESIAN_POINT ( 'NONE',  ( 82.18336038379619879, -2.130196079827426203, 7.949999999999996625 ) ) ;
#137880 = LINE ( 'NONE', #38552, #130888 ) ;
#137881 = DIRECTION ( 'NONE',  ( 0.000000000000000000, 1.000000000000000000, 0.000000000000000000 ) ) ;
#137882 = CARTESIAN_POINT ( 'NONE',  ( 42.37086038379622721, 6.884901960086289741, -3.974999999999993427 ) ) ;
#137883 = LINE ( 'NONE', #94351, #88483 ) ;
#137884 = CARTESIAN_POINT ( 'NONE',  ( 31.78501580275790772, -3.740707523384241728, 15.76143240460131700 ) ) ;
#137885 = ORIENTED_EDGE ( 'NONE', *, *, #124940, .T. ) ;
#137886 = ORIENTED_EDGE ( 'NONE', *, *, #98152, .T. ) ;
#137887 = CARTESIAN_POINT ( 'NONE',  ( 36.29166666666666430, 3.975000000000003642, -6.884901960086285300 ) ) ;
#137888 = ORIENTED_EDGE ( 'NONE', *, *, #104489, .T. ) ;
#137889 = DIRECTION ( 'NONE',  ( 0.7071067811865487940, -0.7071067811865463515, 0.000000000000000000 ) ) ;
#137890 = DIRECTION ( 'NONE',  ( -0.7071067811865487940, 0.7071067811865463515, -0.000000000000000000 ) ) ;
#137891 = ORIENTED_EDGE ( 'NONE', *, *, #116290, .F. ) ;
#137892 = DIRECTION ( 'NONE',  ( -0.7071067811865487940, 0.7071067811865463515, -0.000000000000000000 ) ) ;
#137893 = FACE_OUTER_BOUND ( 'NONE', #26589, .T. ) ;
#137894 = DIRECTION ( 'NONE',  ( -1.000000000000000000, -0.000000000000000000, -0.000000000000000000 ) ) ;
#137895 = CARTESIAN_POINT ( 'NONE',  ( 7.499999999999954703, -17.94781430457064531, 5.000000000000000000 ) ) ;
#137896 = CARTESIAN_POINT ( 'NONE',  ( 128.0995968585647802, -6.109999999999997655, -1.637169565754160283 ) ) ;
#137897 = EDGE_CURVE ( 'NONE', #90786, #27619, #81253, .T. ) ;
#137898 = ORIENTED_EDGE ( 'NONE', *, *, #93771, .F. ) ;
#137899 = DIRECTION ( 'NONE',  ( 0.7071067811865487940, 0.7071067811865463515, 0.000000000000000000 ) ) ;
#137900 = ORIENTED_EDGE ( 'NONE', *, *, #119514, .F. ) ;
#137901 = DIRECTION ( 'NONE',  ( 0.7071067811865486830, -0.7071067811865464625, -0.000000000000000000 ) ) ;
#137902 = CARTESIAN_POINT ( 'NONE',  ( 2.207106781186525701, 12.75929247661558996, 5.000000000000000000 ) ) ;
#137903 = CARTESIAN_POINT ( 'NONE',  ( 24.96654721599509941, 3.964575861396866685, 4.000000000000000000 ) ) ;
#137904 = DIRECTION ( 'NONE',  ( 0.7071067811865487940, 0.7071067811865463515, 0.000000000000000000 ) ) ;
#137906 = EDGE_CURVE ( 'NONE', #32667, #105469, #45944, .T. ) ;
#137905 = ORIENTED_EDGE ( 'NONE', *, *, #94769, .T. ) ;
#137907 = CARTESIAN_POINT ( 'NONE',  ( 55.27126352523143282, 4.472830434245839371, 4.472830434245842035 ) ) ;
#137908 = EDGE_LOOP ( 'NONE', ( #61159, #66175, #61800, #76220, #71604, #16018, #52159, #3011 ) ) ;
#137909 = LINE ( 'NONE', #38583, #33202 ) ;
#137910 = EDGE_CURVE ( 'NONE', #80031, #104227, #104392, .T. ) ;
#137911 = LINE ( 'NONE', #17526, #115639 ) ;
#137912 = CARTESIAN_POINT ( 'NONE',  ( -30.18398860626900060, 28.73617430169808173, 5.000000000000000000 ) ) ;
#137913 = CYLINDRICAL_SURFACE ( 'NONE', #85723, 2.500000000000000000 ) ;
#137914 = CARTESIAN_POINT ( 'NONE',  ( 50.07876352523145158, -7.482591942790325086E-16, 6.109999999999998543 ) ) ;
#137915 = VERTEX_POINT ( 'NONE', #119527 ) ;
#137916 = VECTOR ( 'NONE', #10556, 1000.000000000000000 ) ;
#137917 = DIRECTION ( 'NONE',  ( -0.000000000000000000, -0.3543493200069152693, 0.9351131265310292928 ) ) ;
#137918 = CARTESIAN_POINT ( 'NONE',  ( -19.93618820135885272, -0.2700000000000093991, -36.39086428169088094 ) ) ;
#137919 = VERTEX_POINT ( 'NONE', #41279 ) ;
#137920 = ORIENTED_EDGE ( 'NONE', *, *, #106209, .F. ) ;
#137921 = LINE ( 'NONE', #37165, #60901 ) ;
#137922 = ORIENTED_EDGE ( 'NONE', *, *, #12879, .T. ) ;
#137923 = EDGE_CURVE ( 'NONE', #2809, #64090, #19534, .T. ) ;
#137924 = CARTESIAN_POINT ( 'NONE',  ( -5.994519915287488843, 28.92564299267942118, 4.000000000000000000 ) ) ;
#137925 = ORIENTED_EDGE ( 'NONE', *, *, #122522, .F. ) ;
#137926 = LINE ( 'NONE', #71974, #92246 ) ;
#137927 = DIRECTION ( 'NONE',  ( -0.7071067811865486830, -0.7071067811865464625, 0.000000000000000000 ) ) ;
#137928 = CARTESIAN_POINT ( 'NONE',  ( -14.20710678118645376, 12.75929247661558996, 5.000000000000000000 ) ) ;
#137929 = FACE_BOUND ( 'NONE', #5651, .T. ) ;
#137930 = LINE ( 'NONE', #5934, #38757 ) ;
#137931 = SURFACE_STYLE_FILL_AREA ( #104575 ) ;
#137932 = CARTESIAN_POINT ( 'NONE',  ( 8.999999999999934275, -13.06887692260767686, 4.000000000000000000 ) ) ;
#137933 = ORIENTED_EDGE ( 'NONE', *, *, #51248, .F. ) ;
#137934 =( NAMED_UNIT ( * ) PLANE_ANGLE_UNIT ( ) SI_UNIT ( $, .RADIAN. ) );
#137936 = ORIENTED_EDGE ( 'NONE', *, *, #20026, .T. ) ;
#137935 = CARTESIAN_POINT ( 'NONE',  ( 184.1500000000000057, 26.96999999999993847, -34.92499999999998295 ) ) ;
#137937 = ORIENTED_EDGE ( 'NONE', *, *, #115290, .F. ) ;
#137938 = CARTESIAN_POINT ( 'NONE',  ( 22.49999999999984368, -20.56887692260760048, 4.000000000000000000 ) ) ;
#137939 = AXIS2_PLACEMENT_3D ( 'NONE', #46827, #91014, #55520 ) ;
#137940 = ORIENTED_EDGE ( 'NONE', *, *, #80098, .T. ) ;
#137941 = EDGE_CURVE ( 'NONE', #53245, #142744, #64473, .T. ) ;
#137944 = VERTEX_POINT ( 'NONE', #52854 ) ;
#137943 = EDGE_CURVE ( 'NONE', #110128, #42427, #42024, .T. ) ;
#137942 = VECTOR ( 'NONE', #48751, 1000.000000000000227 ) ;
#137945 = CARTESIAN_POINT ( 'NONE',  ( 66.26626352523145158, 4.472830434245838482, -4.472830434245837594 ) ) ;
#137946 = ORIENTED_EDGE ( 'NONE', *, *, #133117, .F. ) ;
#137947 = VECTOR ( 'NONE', #14584, 1000.000000000000227 ) ;
#137948 = LINE ( 'NONE', #18251, #95071 ) ;
#137949 = EDGE_CURVE ( 'NONE', #79680, #136698, #98082, .T. ) ;
#137950 = FACE_OUTER_BOUND ( 'NONE', #34785, .T. ) ;
#137951 = ORIENTED_EDGE ( 'NONE', *, *, #32894, .F. ) ;
#137952 = VECTOR ( 'NONE', #108365, 1000.000000000000000 ) ;
#137953 = EDGE_CURVE ( 'NONE', #85512, #18266, #39159, .T. ) ;
#137954 = EDGE_CURVE ( 'NONE', #85156, #8752, #139205, .T. ) ;
#137955 = CARTESIAN_POINT ( 'NONE',  ( -34.92500000000001137, -6.791953661863761482, 15.99560845316869795 ) ) ;
#137956 = DIRECTION ( 'NONE',  ( 0.7071067811865486830, -0.7071067811865464625, -0.000000000000000000 ) ) ;
#137957 = DIRECTION ( 'NONE',  ( 1.000000000000000000, 0.000000000000000000, 0.000000000000000000 ) ) ;
#137958 = ORIENTED_EDGE ( 'NONE', *, *, #111888, .T. ) ;
#137959 = ORIENTED_EDGE ( 'NONE', *, *, #45813, .T. ) ;
#137960 = CARTESIAN_POINT ( 'NONE',  ( 0.000000000000000000, -4.870000000000014317, -10.00000000000000178 ) ) ;
#137961 = LINE ( 'NONE', #135131, #37407 ) ;
#137962 = EDGE_LOOP ( 'NONE', ( #59697, #51806, #25286, #754 ) ) ;
#137963 = ORIENTED_EDGE ( 'NONE', *, *, #63060, .T. ) ;
#137964 = ORIENTED_EDGE ( 'NONE', *, *, #30964, .T. ) ;
#137965 = DIRECTION ( 'NONE',  ( -0.000000000000000000, 0.000000000000000000, 1.000000000000000000 ) ) ;
#137967 = ADVANCED_FACE ( 'NONE', ( #140588 ), #141311, .F. ) ;
#137966 = DIRECTION ( 'NONE',  ( 0.6830127018922180770, -0.6830127018922204085, -0.2588190451025213501 ) ) ;
#137968 = EDGE_CURVE ( 'NONE', #41375, #108415, #116710, .T. ) ;
#137969 = CARTESIAN_POINT ( 'NONE',  ( -5.999999999999952927, -21.41253812416053748, 4.000000000000000000 ) ) ;
#137970 = ORIENTED_EDGE ( 'NONE', *, *, #40069, .F. ) ;
#137971 = LINE ( 'NONE', #81468, #94895 ) ;
#137972 = EDGE_CURVE ( 'NONE', #122347, #114208, #30422, .T. ) ;
#137973 = PLANE ( 'NONE',  #4958 ) ;
#137974 = CARTESIAN_POINT ( 'NONE',  ( 8.671236474768553748, 0.000000000000000000, 7.934999999999990727 ) ) ;
#137975 = CARTESIAN_POINT ( 'NONE',  ( 12.00548008471251293, 28.92564299267929684, 4.000000000000000000 ) ) ;
#137976 = ORIENTED_EDGE ( 'NONE', *, *, #22790, .F. ) ;
#137977 = CARTESIAN_POINT ( 'NONE',  ( 6.524001385854438340, 22.03583458319437582, 4.979811245910090278 ) ) ;
#137978 = LINE ( 'NONE', #40803, #21163 ) ;
#137979 = LINE ( 'NONE', #50258, #135468 ) ;
#137980 = EDGE_CURVE ( 'NONE', #63953, #54435, #117392, .T. ) ;
#137982 = VERTEX_POINT ( 'NONE', #18809 ) ;
#137981 = DIRECTION ( 'NONE',  ( -0.7071067811865487940, 0.7071067811865463515, 0.000000000000000000 ) ) ;
#137983 = PLANE ( 'NONE',  #102622 ) ;
#137984 = ORIENTED_EDGE ( 'NONE', *, *, #142821, .T. ) ;
#137985 = CARTESIAN_POINT ( 'NONE',  ( 26.99999999999981526, 13.93112307739204603, 4.000000000000000000 ) ) ;
#137986 = DIRECTION ( 'NONE',  ( -0.7071067811865486830, -0.7071067811865464625, 0.000000000000000000 ) ) ;
#137987 = LINE ( 'NONE', #116930, #33239 ) ;
#137988 = ORIENTED_EDGE ( 'NONE', *, *, #7381, .T. ) ;
#137989 = DIRECTION ( 'NONE',  ( -0.7071067811865486830, -0.7071067811865464625, 0.000000000000000000 ) ) ;
#137990 = CARTESIAN_POINT ( 'NONE',  ( 14.99999999999989519, -19.06887692260762179, 4.000000000000000000 ) ) ;
#137991 = FACE_OUTER_BOUND ( 'NONE', #43604, .T. ) ;
#137992 = ADVANCED_FACE ( 'NONE', ( #130462 ), #7923, .T. ) ;
#137993 = EDGE_LOOP ( 'NONE', ( #81440, #74902, #122338, #32669 ) ) ;
#137994 = CARTESIAN_POINT ( 'NONE',  ( -34.92500000000001137, -14.14387692260741325, 4.000000000000000000 ) ) ;
#137995 = CARTESIAN_POINT ( 'NONE',  ( 11.56505274454301357, 4.584330080086930965E-16, 0.000000000000000000 ) ) ;
#137996 = DIRECTION ( 'NONE',  ( -1.000000000000000000, -0.000000000000000000, -0.000000000000000000 ) ) ;
#137997 = CARTESIAN_POINT ( 'NONE',  ( 0.000000000000000000, -60.00000000000000000, -4.000000000000000000 ) ) ;
#137998 = ORIENTED_EDGE ( 'NONE', *, *, #18616, .T. ) ;
#137999 = EDGE_CURVE ( 'NONE', #29164, #113129, #74657, .T. ) ;
#138000 = VERTEX_POINT ( 'NONE', #28285 ) ;
#138001 = LINE ( 'NONE', #3858, #125933 ) ;
#138002 = DIRECTION ( 'NONE',  ( -0.7071067811865486830, -0.7071067811865464625, 0.000000000000000000 ) ) ;
#138003 = EDGE_CURVE ( 'NONE', #41816, #18858, #105800, .T. ) ;
#138004 = CARTESIAN_POINT ( 'NONE',  ( 3.916236474768553411, -7.934999999999990727, 4.858786175617117713E-16 ) ) ;
#138005 = VECTOR ( 'NONE', #129504, 1000.000000000000000 ) ;
#138006 = LINE ( 'NONE', #16933, #59828 ) ;
#138007 = LINE ( 'NONE', #92326, #25293 ) ;
#138008 = CARTESIAN_POINT ( 'NONE',  ( -17.99999999999987210, 13.93112307739204070, 4.000000000000000000 ) ) ;
#138009 = FACE_OUTER_BOUND ( 'NONE', #64604, .T. ) ;
#138010 = AXIS2_PLACEMENT_3D ( 'NONE', #78531, #56816, #1635 ) ;
#138011 = ORIENTED_EDGE ( 'NONE', *, *, #101956, .F. ) ;
#138012 = DIRECTION ( 'NONE',  ( -0.7071067811865486830, -0.7071067811865464625, 0.000000000000000000 ) ) ;
#138013 = LINE ( 'NONE', #39424, #26147 ) ;
#138014 = DIRECTION ( 'NONE',  ( -0.000000000000000000, 0.000000000000000000, 1.000000000000000000 ) ) ;
#138015 = CARTESIAN_POINT ( 'NONE',  ( 44.39126352523143737, -4.472830434245839371, -4.472830434245839371 ) ) ;
#138016 = CARTESIAN_POINT ( 'NONE',  ( -0.7700427945779352301, 21.73644205237998150, 5.000000000000000888 ) ) ;
#138017 = VERTEX_POINT ( 'NONE', #18065 ) ;
#138018 = PRESENTATION_STYLE_ASSIGNMENT (( #6024 ) ) ;
#138019 = ORIENTED_EDGE ( 'NONE', *, *, #132337, .T. ) ;
#138020 = VECTOR ( 'NONE', #79417, 1000.000000000000227 ) ;
#138021 = VERTEX_POINT ( 'NONE', #118100 ) ;
#138022 = DIRECTION ( 'NONE',  ( -0.3543493200069162685, -0.000000000000000000, -0.9351131265310288487 ) ) ;
#138023 = DIRECTION ( 'NONE',  ( -0.3543493200069162685, -0.000000000000000000, -0.9351131265310288487 ) ) ;
#138024 = LINE ( 'NONE', #48882, #41980 ) ;
#138025 = PLANE ( 'NONE',  #46419 ) ;
#138026 = VECTOR ( 'NONE', #82612, 1000.000000000000000 ) ;
#138027 = CARTESIAN_POINT ( 'NONE',  ( 19.05000000000000071, 3.174999999999997158, 4.000000000000000000 ) ) ;
#138028 = CARTESIAN_POINT ( 'NONE',  ( 10.50000000000000000, 0.000000000000000000, 6.094999999999989981 ) ) ;
#138029 = EDGE_CURVE ( 'NONE', #44190, #142002, #8606, .T. ) ;
#138030 = ORIENTED_EDGE ( 'NONE', *, *, #140707, .T. ) ;
#138031 = DIRECTION ( 'NONE',  ( 0.6830127018922181881, 0.6830127018922202975, -0.2588190451025214056 ) ) ;
#138032 = CARTESIAN_POINT ( 'NONE',  ( 13.49999999999991473, 7.087461875839172087, 4.000000000000000000 ) ) ;
#138033 = DIRECTION ( 'NONE',  ( -0.7071067811865486830, -0.7071067811865464625, 0.000000000000000000 ) ) ;
#138034 = LINE ( 'NONE', #13367, #59003 ) ;
#138035 = VECTOR ( 'NONE', #36445, 1000.000000000000000 ) ;
#138036 = CARTESIAN_POINT ( 'NONE',  ( 33.70710678118631165, -9.740707523384182664, 5.000000000000000000 ) ) ;
#138037 = CARTESIAN_POINT ( 'NONE',  ( 65.12086038379621300, -6.884901960086286188, 3.974999999999997424 ) ) ;
#138038 = AXIS2_PLACEMENT_3D ( 'NONE', #136238, #36926, #81175 ) ;
#138039 = CARTESIAN_POINT ( 'NONE',  ( -34.92500000000001137, -22.22500000000000142, 4.500000000000000888 ) ) ;
#138040 = VERTEX_POINT ( 'NONE', #118845 ) ;
#138041 = EDGE_LOOP ( 'NONE', ( #4783, #99587, #114088, #67408 ) ) ;
#138042 = CARTESIAN_POINT ( 'NONE',  ( 67.35416666666664298, -2.130196079827425315, -7.950000000000001066 ) ) ;
#138043 = CARTESIAN_POINT ( 'NONE',  ( -54.48921356237310221, -27.52281430457093236, 5.000000000000000000 ) ) ;
#138044 = AXIS2_PLACEMENT_3D ( 'NONE', #95778, #40014, #139325 ) ;
#138045 = DIRECTION ( 'NONE',  ( 0.6830127018922181881, 0.6830127018922202975, -0.2588190451025214056 ) ) ;
#138046 = LINE ( 'NONE', #40701, #89102 ) ;
#138047 = EDGE_CURVE ( 'NONE', #31906, #65260, #7196, .T. ) ;
#138048 = AXIS2_PLACEMENT_3D ( 'NONE', #80618, #3026, #13882 ) ;
#138049 = ORIENTED_EDGE ( 'NONE', *, *, #47032, .T. ) ;
#138050 = CARTESIAN_POINT ( 'NONE',  ( 24.70710678118637915, 17.25929247661554555, 5.000000000000000000 ) ) ;
#138051 = CARTESIAN_POINT ( 'NONE',  ( 22.49999999999984723, 16.77039438581781639, 0.4657186855307219875 ) ) ;
#138052 = CARTESIAN_POINT ( 'NONE',  ( 54.10459685856476852, 1.637169565754164946, -6.109999999999999432 ) ) ;
#138053 = DIRECTION ( 'NONE',  ( -0.000000000000000000, 0.000000000000000000, 1.000000000000000000 ) ) ;
#138054 = ORIENTED_EDGE ( 'NONE', *, *, #49320, .F. ) ;
#138055 = ORIENTED_EDGE ( 'NONE', *, *, #70984, .F. ) ;
#138056 = FACE_OUTER_BOUND ( 'NONE', #25116, .T. ) ;
#138057 = CARTESIAN_POINT ( 'NONE',  ( -26.29289321881326558, 2.259292476615690770, 5.000000000000000000 ) ) ;
#138058 = DIRECTION ( 'NONE',  ( -0.7071067811865486830, -0.7071067811865464625, 0.000000000000000000 ) ) ;
#138059 = LINE ( 'NONE', #5373, #129632 ) ;
#138060 = EDGE_CURVE ( 'NONE', #45656, #121222, #139917, .T. ) ;
#138061 = LINE ( 'NONE', #106103, #136782 ) ;
#138063 = VERTEX_POINT ( 'NONE', #96345 ) ;
#138062 = DIRECTION ( 'NONE',  ( -0.7071067811865487940, 0.7071067811865463515, 0.000000000000000000 ) ) ;
#138064 = EDGE_CURVE ( 'NONE', #35117, #91654, #63779, .T. ) ;
#138065 = CARTESIAN_POINT ( 'NONE',  ( 81.48921356237309510, -27.52281430457112066, 5.000000000000000000 ) ) ;
#138066 = CYLINDRICAL_SURFACE ( 'NONE', #31549, 7.950000000000000178 ) ;
#138067 = LINE ( 'NONE', #37332, #139752 ) ;
#138068 = DIRECTION ( 'NONE',  ( -0.7071067811865486830, -0.7071067811865464625, 0.000000000000000000 ) ) ;
#138069 = VERTEX_POINT ( 'NONE', #78219 ) ;
#138070 = EDGE_LOOP ( 'NONE', ( #116230, #10990, #78051, #12525 ) ) ;
#138071 = EDGE_CURVE ( 'NONE', #115946, #99168, #134022, .T. ) ;
#138072 = PLANE ( 'NONE',  #91550 ) ;
#138073 = PLANE ( 'NONE',  #20931 ) ;
#138074 = CARTESIAN_POINT ( 'NONE',  ( 28.88982677111768638, -22.22500000000000142, 4.785647885939353863 ) ) ;
#138075 = CARTESIAN_POINT ( 'NONE',  ( 110.4750270504628702, -5.819803920172573086, 5.819803920172573086 ) ) ;
#138076 = DIRECTION ( 'NONE',  ( 1.000000000000000000, 0.000000000000000000, 0.000000000000000000 ) ) ;
#138077 = ORIENTED_EDGE ( 'NONE', *, *, #93148, .F. ) ;
#138078 = ORIENTED_EDGE ( 'NONE', *, *, #107993, .T. ) ;
#138079 = VECTOR ( 'NONE', #80296, 1000.000000000000000 ) ;
#138080 = FACE_OUTER_BOUND ( 'NONE', #120652, .T. ) ;
#138081 = VERTEX_POINT ( 'NONE', #78948 ) ;
#138082 = EDGE_CURVE ( 'NONE', #871, #43439, #21685, .T. ) ;
#138083 =( BOUNDED_CURVE ( )  B_SPLINE_CURVE ( 2, ( #30951, #75872, #119339, #11278, #109195, #9879, #55552, #54149, #32363, #21489, #98339, #76607, #88905 ),
 .UNSPECIFIED., .F., .F. ) 
 B_SPLINE_CURVE_WITH_KNOTS ( ( 3, 2, 2, 2, 2, 2, 3 ),
 ( 0.6166666666666666963, 0.6194444444444444642, 0.6222222222222222321, 0.6250000000000000000, 0.6277777777777777679, 0.6305555555555555358, 0.6333333333333333037 ),
 .UNSPECIFIED. ) 
 CURVE ( )  GEOMETRIC_REPRESENTATION_ITEM ( )  RATIONAL_B_SPLINE_CURVE ( ( 1.000000000000000000, 0.9659258262890683122, 1.000000000000000000, 0.9659258262890683122, 1.000000000000000000, 0.9659258262890683122, 1.000000000000000000, 0.9659258262890683122, 1.000000000000000000, 0.9659258262890683122, 1.000000000000000000, 0.9659258262890683122, 1.000000000000000000 ) ) 
 REPRESENTATION_ITEM ( '' )  );
#138084 = ORIENTED_EDGE ( 'NONE', *, *, #76517, .T. ) ;
#138085 = CARTESIAN_POINT ( 'NONE',  ( -68.99451991528748351, 28.92564299267986172, 4.000000000000000000 ) ) ;
#138086 = ORIENTED_EDGE ( 'NONE', *, *, #33594, .T. ) ;
#138087 = CARTESIAN_POINT ( 'NONE',  ( 62.35002705046287730, -5.819803920172573086, -5.819803920172573086 ) ) ;
#138089 = AXIS2_PLACEMENT_3D ( 'NONE', #119270, #42477, #8345 ) ;
#138088 = CARTESIAN_POINT ( 'NONE',  ( 24.79289321881329045, -5.240707523384227073, 5.000000000000000000 ) ) ;
#138090 = EDGE_CURVE ( 'NONE', #37148, #38733, #110098, .T. ) ;
#138091 = EDGE_CURVE ( 'NONE', #72213, #33945, #123157, .T. ) ;
#138092 =( BOUNDED_CURVE ( )  B_SPLINE_CURVE ( 3, ( #139833, #27442, #116616, #140499 ),
 .UNSPECIFIED., .F., .T. ) 
 B_SPLINE_CURVE_WITH_KNOTS ( ( 4, 4 ),
 ( 5.920967161967927161, 7.341195215986571654 ),
 .UNSPECIFIED. ) 
 CURVE ( )  GEOMETRIC_REPRESENTATION_ITEM ( )  RATIONAL_B_SPLINE_CURVE ( ( 1.000000000000000000, 0.8388583629366757055, 0.8388583629366757055, 1.000000000000000000 ) ) 
 REPRESENTATION_ITEM ( '' )  );
#138093 = FACE_BOUND ( 'NONE', #125660, .T. ) ;
#138094 = FILL_AREA_STYLE_COLOUR ( '', #98756 ) ;
#138095 = LINE ( 'NONE', #72888, #111497 ) ;
#138097 = ORIENTED_EDGE ( 'NONE', *, *, #126915, .T. ) ;
#138096 = LINE ( 'NONE', #38084, #126821 ) ;
#138098 = LINE ( 'NONE', #48963, #46412 ) ;
#138099 = ITEM_DEFINED_TRANSFORMATION ( 'NONE', 'NONE', #37734,  #127880 ) ;
#138101 = VERTEX_POINT ( 'NONE', #31843 ) ;
#138100 = VECTOR ( 'NONE', #53988, 999.9999999999998863 ) ;
#138102 = ORIENTED_EDGE ( 'NONE', *, *, #137048, .T. ) ;
#138103 = CARTESIAN_POINT ( 'NONE',  ( 95.72459685856476597, -1.637169565754160949, 6.109999999999997655 ) ) ;
#138104 = VERTEX_POINT ( 'NONE', #110797 ) ;
#138105 = LINE ( 'NONE', #95302, #53584 ) ;
#138106 = EDGE_CURVE ( 'NONE', #95146, #107914, #20951, .T. ) ;
#138107 = FACE_OUTER_BOUND ( 'NONE', #40229, .T. ) ;
#138108 = CARTESIAN_POINT ( 'NONE',  ( -18.18398860626898994, 28.73617430169800002, 5.000000000000000000 ) ) ;
#138109 = EDGE_CURVE ( 'NONE', #71394, #23245, #76810, .T. ) ;
#138110 = EDGE_CURVE ( 'NONE', #81346, #101337, #108648, .T. ) ;
#138111 = DIRECTION ( 'NONE',  ( -0.000000000000000000, -0.3543493200069152693, 0.9351131265310292928 ) ) ;
#138112 = ORIENTED_EDGE ( 'NONE', *, *, #123921, .F. ) ;
#138113 = PLANE ( 'NONE',  #92343 ) ;
#138114 = DIRECTION ( 'NONE',  ( -0.000000000000000000, 0.000000000000000000, 1.000000000000000000 ) ) ;
#138115 = AXIS2_PLACEMENT_3D ( 'NONE', #82478, #40414, #41102 ) ;
#138116 = CARTESIAN_POINT ( 'NONE',  ( -29.99999999999978684, -11.35517001088074274, -1.126524801160180056 ) ) ;
#138118 = CARTESIAN_POINT ( 'NONE',  ( 24.39999999999999858, -7.600000000000061817, 28.92499999999998650 ) ) ;
#138117 = PLANE ( 'NONE',  #143119 ) ;
#138119 = CARTESIAN_POINT ( 'NONE',  ( 0.000000000000000000, 0.000000000000000000, 5.000000000000000000 ) ) ;
#138120 = FACE_OUTER_BOUND ( 'NONE', #106760, .T. ) ;
#138121 = DIRECTION ( 'NONE',  ( -0.000000000000000000, -0.3543493200069152693, 0.9351131265310292928 ) ) ;
#138122 = ORIENTED_EDGE ( 'NONE', *, *, #124268, .T. ) ;
#138123 = ADVANCED_FACE ( 'NONE', ( #120233 ), #97809, .F. ) ;
#138124 = CARTESIAN_POINT ( 'NONE',  ( -6.707106781186496391, -0.7407075233842753681, 5.000000000000000000 ) ) ;
#138125 = LINE ( 'NONE', #58482, #83578 ) ;
#138126 = ORIENTED_EDGE ( 'NONE', *, *, #116709, .T. ) ;
#138128 = ORIENTED_EDGE ( 'NONE', *, *, #53000, .F. ) ;
#138127 = MECHANICAL_DESIGN_GEOMETRIC_PRESENTATION_REPRESENTATION (  '', ( #8408 ), #22390 ) ;
#138129 = EDGE_CURVE ( 'NONE', #8853, #51846, #99208, .T. ) ;
#138131 = ORIENTED_EDGE ( 'NONE', *, *, #71448, .F. ) ;
#138130 = ADVANCED_FACE ( 'NONE', ( #33318 ), #77520, .F. ) ;
#138132 = CARTESIAN_POINT ( 'NONE',  ( 48.41709685856476852, 3.054999999999998828, 5.291415217122922066 ) ) ;
#138133 = ORIENTED_EDGE ( 'NONE', *, *, #70898, .F. ) ;
#138134 = VECTOR ( 'NONE', #31290, 1000.000000000000000 ) ;
#138135 = VECTOR ( 'NONE', #5026, 1000.000000000000227 ) ;
#138136 = VECTOR ( 'NONE', #176, 999.9999999999998863 ) ;
#138137 = EDGE_CURVE ( 'NONE', #73159, #949, #132624, .T. ) ;
#138138 = CARTESIAN_POINT ( 'NONE',  ( 19.87913961620377279, -5.278424836066145431, -3.047499999999993658 ) ) ;
#138139 = CARTESIAN_POINT ( 'NONE',  ( -14.67277584711400351, 8.043494102545141189, -27.98791813066781131 ) ) ;
#138140 = ADVANCED_FACE ( 'NONE', ( #65217 ), #1329, .F. ) ;
#138141 = ORIENTED_EDGE ( 'NONE', *, *, #64686, .F. ) ;
#138142 = DIRECTION ( 'NONE',  ( 0.5735764363510451602, 0.8191520442889924647, 0.000000000000000000 ) ) ;
#138143 = ORIENTED_EDGE ( 'NONE', *, *, #43504, .F. ) ;
#138144 = CARTESIAN_POINT ( 'NONE',  ( -53.99451991528749062, 28.92564299267975869, 4.000000000000000000 ) ) ;
#138145 = VECTOR ( 'NONE', #100600, 1000.000000000000114 ) ;
#138146 = DIRECTION ( 'NONE',  ( -0.7071067811865486830, -0.7071067811865464625, 0.000000000000000000 ) ) ;
#138147 = EDGE_CURVE ( 'NONE', #31910, #80563, #66626, .T. ) ;
#138149 = ORIENTED_EDGE ( 'NONE', *, *, #50685, .T. ) ;
#138148 = DIRECTION ( 'NONE',  ( -0.000000000000000000, 0.3543493200069153248, 0.9351131265310292928 ) ) ;
#138150 = ORIENTED_EDGE ( 'NONE', *, *, #48087, .T. ) ;
#138151 = DIRECTION ( 'NONE',  ( -0.6830127018922180770, -0.6830127018922204085, -0.2588190451025213501 ) ) ;
#138152 = FACE_OUTER_BOUND ( 'NONE', #2712, .T. ) ;
#138153 = DIRECTION ( 'NONE',  ( 0.7071067811865487940, -0.7071067811865463515, 0.000000000000000000 ) ) ;
#138154 = ORIENTED_EDGE ( 'NONE', *, *, #122223, .T. ) ;
#138155 = DIRECTION ( 'NONE',  ( -0.7071067811865487940, 0.7071067811865463515, -0.000000000000000000 ) ) ;
#138156 = ORIENTED_EDGE ( 'NONE', *, *, #44201, .F. ) ;
#138157 = VERTEX_POINT ( 'NONE', #86944 ) ;
#138158 = ORIENTED_EDGE ( 'NONE', *, *, #19765, .F. ) ;
#138159 = VERTEX_POINT ( 'NONE', #99959 ) ;
#138160 = CARTESIAN_POINT ( 'NONE',  ( -34.92500000000001137, 21.72500000000000142, 5.000000000000000000 ) ) ;
#138161 = EDGE_CURVE ( 'NONE', #9514, #116559, #44917, .T. ) ;
#138162 = DIRECTION ( 'NONE',  ( 1.000000000000000000, 0.000000000000000000, 0.000000000000000000 ) ) ;
#138163 = CARTESIAN_POINT ( 'NONE',  ( -57.18398860626899705, 28.73617430169827358, 5.000000000000000000 ) ) ;
#138164 = CARTESIAN_POINT ( 'NONE',  ( -44.99451991528749772, 28.92564299267969474, 4.000000000000000000 ) ) ;
#138165 = ORIENTED_EDGE ( 'NONE', *, *, #23138, .F. ) ;
#138166 = ORIENTED_EDGE ( 'NONE', *, *, #120742, .F. ) ;
#138167 = CARTESIAN_POINT ( 'NONE',  ( -17.70025512860841488, -27.71228299555193786, 4.000000000000000000 ) ) ;
#138168 = ADVANCED_FACE ( 'NONE', ( #54346 ), #122404, .F. ) ;
#138169 = EDGE_CURVE ( 'NONE', #7759, #61677, #33997, .T. ) ;
#138170 = DIRECTION ( 'NONE',  ( -0.000000000000000000, 0.000000000000000000, 1.000000000000000000 ) ) ;
#138171 = DIRECTION ( 'NONE',  ( -1.000000000000000000, 2.223259271439533943E-14, 0.000000000000000000 ) ) ;
#138172 = CARTESIAN_POINT ( 'NONE',  ( -19.21071296386495675, 9.141836041257182188, 4.000000000000000000 ) ) ;
#138173 = DIRECTION ( 'NONE',  ( -1.000000000000000000, -1.224606353822377258E-16, -0.000000000000000000 ) ) ;
#138174 = ORIENTED_EDGE ( 'NONE', *, *, #65932, .F. ) ;
#138175 = ORIENTED_EDGE ( 'NONE', *, *, #91564, .F. ) ;
#138176 = ORIENTED_EDGE ( 'NONE', *, *, #131926, .T. ) ;
#138177 = CARTESIAN_POINT ( 'NONE',  ( 56.99451991528749062, 28.92564299267978001, 4.000000000000000000 ) ) ;
#138178 = CARTESIAN_POINT ( 'NONE',  ( 94.57919371712955581, 3.975000000000002753, -6.884901960086283523 ) ) ;
#138179 = DIRECTION ( 'NONE',  ( -0.7071067811865486830, -0.7071067811865464625, -0.000000000000000000 ) ) ;
#138180 = VECTOR ( 'NONE', #54463, 1000.000000000000000 ) ;
#138181 = CARTESIAN_POINT ( 'NONE',  ( -7.940000000000007496, -39.92999999999999261, -12.24789999999999957 ) ) ;
#138182 = EDGE_CURVE ( 'NONE', #140758, #38440, #100680, .T. ) ;
#138183 = CARTESIAN_POINT ( 'NONE',  ( 3.187477005606029756, -48.82538788374344563, -38.96958855984476600 ) ) ;
#138184 = CARTESIAN_POINT ( 'NONE',  ( 76.76626352523142316, 4.472830434245839371, -4.472830434245839371 ) ) ;
#138185 = LINE ( 'NONE', #61383, #62611 ) ;
#138186 = FACE_OUTER_BOUND ( 'NONE', #5207, .T. ) ;
#138187 = LINE ( 'NONE', #117125, #52439 ) ;
#138188 = CARTESIAN_POINT ( 'NONE',  ( 22.35824297541125816, 15.75929247661555088, 19.34181609438694238 ) ) ;
#138189 = LINE ( 'NONE', #48316, #20964 ) ;
#138190 = CIRCLE ( 'NONE', #75695, 5.968999999999998529 ) ;
#138191 = ORIENTED_EDGE ( 'NONE', *, *, #39267, .T. ) ;
#138192 = CARTESIAN_POINT ( 'NONE',  ( -42.48921356237308800, -27.52281430457085065, 5.000000000000000000 ) ) ;
#138193 = ORIENTED_EDGE ( 'NONE', *, *, #71336, .T. ) ;
#138194 = CARTESIAN_POINT ( 'NONE',  ( -60.29974487139158867, -27.71228299555248142, 4.000000000000000000 ) ) ;
#138196 = EDGE_LOOP ( 'NONE', ( #39991, #89351, #36307, #95564 ) ) ;
#138195 = DIRECTION ( 'NONE',  ( -0.000000000000000000, 0.3543493200069153248, 0.9351131265310292928 ) ) ;
#138197 = AXIS2_PLACEMENT_3D ( 'NONE', #110087, #131146, #97797 ) ;
#138198 = DIRECTION ( 'NONE',  ( -0.7071067811865486830, -0.7071067811865464625, -0.000000000000000000 ) ) ;
#138199 = CARTESIAN_POINT ( 'NONE',  ( -69.48921356237309510, -27.52281430457103895, 5.000000000000000000 ) ) ;
#138200 = ORIENTED_EDGE ( 'NONE', *, *, #121138, .F. ) ;
#138201 = ORIENTED_EDGE ( 'NONE', *, *, #114239, .T. ) ;
#138202 = CARTESIAN_POINT ( 'NONE',  ( 34.92499999999998295, -22.22500000000000142, 4.500000000000000888 ) ) ;
#138203 = VERTEX_POINT ( 'NONE', #114394 ) ;
#138204 = LINE ( 'NONE', #26582, #126317 ) ;
#138205 = VECTOR ( 'NONE', #65405, 1000.000000000000000 ) ;
#138206 = CARTESIAN_POINT ( 'NONE',  ( 90.64169371712954160, -2.130196079827424871, -7.949999999999999289 ) ) ;
#138207 = FACE_OUTER_BOUND ( 'NONE', #130711, .T. ) ;
#138208 = DIRECTION ( 'NONE',  ( 1.000000000000000000, 0.000000000000000000, 0.000000000000000000 ) ) ;
#138209 = ORIENTED_EDGE ( 'NONE', *, *, #91129, .T. ) ;
#138210 = VECTOR ( 'NONE', #63424, 1000.000000000000227 ) ;
#138211 = CARTESIAN_POINT ( 'NONE',  ( -15.79289321881334551, -20.24070752338407431, 5.000000000000000000 ) ) ;
#138212 = ADVANCED_FACE ( 'NONE', ( #15064 ), #70235, .F. ) ;
#138213 = CARTESIAN_POINT ( 'NONE',  ( 20.99999999999985079, -21.41253812416053748, 4.000000000000000000 ) ) ;
#138214 = CARTESIAN_POINT ( 'NONE',  ( 25.22916666666666785, -6.094999999999989093, 1.633150327867691765 ) ) ;
#138215 = DIRECTION ( 'NONE',  ( -1.000000000000000000, -1.224606353822377258E-16, -0.000000000000000000 ) ) ;
#138216 = CARTESIAN_POINT ( 'NONE',  ( -33.18398860626899705, 28.73617430169810305, 5.000000000000000000 ) ) ;
#138217 = ORIENTED_EDGE ( 'NONE', *, *, #21651, .T. ) ;
#138218 = LINE ( 'NONE', #7681, #141739 ) ;
#138219 = VERTEX_POINT ( 'NONE', #25968 ) ;
#138220 = CARTESIAN_POINT ( 'NONE',  ( 83.41709685856477563, 3.054999999999998828, 5.291415217122922066 ) ) ;
#138221 = LINE ( 'NONE', #4789, #121805 ) ;
#138222 = CARTESIAN_POINT ( 'NONE',  ( 69.18398860626899705, 28.73617430169835529, 5.000000000000000000 ) ) ;
#138223 = CARTESIAN_POINT ( 'NONE',  ( -15.32816939922342492, -3.740707523384241728, 4.000000000000000000 ) ) ;
#138224 = ORIENTED_EDGE ( 'NONE', *, *, #65542, .T. ) ;
#138225 = LINE ( 'NONE', #84573, #41933 ) ;
#138226 = EDGE_CURVE ( 'NONE', #6909, #90219, #91251, .T. ) ;
#138227 = LINE ( 'NONE', #125211, #18776 ) ;
#138228 = VECTOR ( 'NONE', #95634, 1000.000000000000000 ) ;
#138229 = LINE ( 'NONE', #49100, #113383 ) ;
#138230 = EDGE_CURVE ( 'NONE', #108448, #44918, #41249, .T. ) ;
#138231 = DIRECTION ( 'NONE',  ( 0.7071067811865487940, 0.7071067811865463515, -0.000000000000000000 ) ) ;
#138233 = VERTEX_POINT ( 'NONE', #82494 ) ;
#138232 = DIRECTION ( 'NONE',  ( 0.7071067811865487940, 0.7071067811865463515, 0.000000000000000000 ) ) ;
#138234 = DIRECTION ( 'NONE',  ( 0.7071067811865487940, 0.7071067811865463515, -0.000000000000000000 ) ) ;
#138235 = CARTESIAN_POINT ( 'NONE',  ( -34.42500000000000426, 10.54139925780190801, 5.000000000000000000 ) ) ;
#138236 = CARTESIAN_POINT ( 'NONE',  ( 27.53159235450332076, 9.902892378096218942E-16, 0.000000000000000000 ) ) ;
#138237 = AXIS2_PLACEMENT_3D ( 'NONE', #47559, #90282, #44704 ) ;
#138238 = LINE ( 'NONE', #51954, #109464 ) ;
#138240 = EDGE_CURVE ( 'NONE', #92832, #117294, #81078, .T. ) ;
#138239 = AXIS2_PLACEMENT_3D ( 'NONE', #29141, #119677, #94384 ) ;
#138242 = VERTEX_POINT ( 'NONE', #47756 ) ;
#138241 = EDGE_CURVE ( 'NONE', #97535, #140583, #103497, .T. ) ;
#138243 = VERTEX_POINT ( 'NONE', #48428 ) ;
#138244 = CARTESIAN_POINT ( 'NONE',  ( 76.70876352523144703, -7.482591942790329030E-16, 6.110000000000001208 ) ) ;
#138245 = EDGE_LOOP ( 'NONE', ( #17504, #46519, #37045, #130140, #62032, #12671 ) ) ;
#138246 = ADVANCED_FACE ( 'NONE', ( #36144 ), #68091, .T. ) ;
#138247 = SURFACE_STYLE_USAGE ( .BOTH. , #94006 ) ;
#138248 = AXIS2_PLACEMENT_3D ( 'NONE', #101980, #122277, #66510 ) ;
#138250 = VECTOR ( 'NONE', #127737, 1000.000000000000000 ) ;
#138249 = FACE_OUTER_BOUND ( 'NONE', #11764, .T. ) ;
#138251 = CARTESIAN_POINT ( 'NONE',  ( 8.000000000000007105, 0.000000000000000000, 1.142820323027522456 ) ) ;
#138252 = EDGE_LOOP ( 'NONE', ( #128208, #33149, #84781, #67398, #84776, #139842, #112414, #88277, #107025, #1154, #48984, #82031, #97867, #134017, #40436, #62731, #112091, #12410 ) ) ;
#138253 = CARTESIAN_POINT ( 'NONE',  ( 0.000000000000000000, 0.000000000000000000, 5.000000000000000000 ) ) ;
#138254 = CARTESIAN_POINT ( 'NONE',  ( -32.29289321881321939, -0.7407075233842753681, 5.000000000000000000 ) ) ;
#138255 = EDGE_CURVE ( 'NONE', #76898, #33831, #4870, .T. ) ;
#138256 = ORIENTED_EDGE ( 'NONE', *, *, #121909, .T. ) ;
#138257 = PLANE ( 'NONE',  #46710 ) ;
#138258 = CARTESIAN_POINT ( 'NONE',  ( 34.20419371712955581, -6.884901960086285300, -3.975000000000000089 ) ) ;
#138259 = FACE_OUTER_BOUND ( 'NONE', #98916, .T. ) ;
#138260 = EDGE_CURVE ( 'NONE', #112045, #78508, #57917, .T. ) ;
#138261 = ORIENTED_EDGE ( 'NONE', *, *, #23410, .F. ) ;
#138262 = VERTEX_POINT ( 'NONE', #37570 ) ;
#138263 = CARTESIAN_POINT ( 'NONE',  ( 30.18398860626900060, 28.73617430169808173, 5.000000000000000000 ) ) ;
#138264 = CARTESIAN_POINT ( 'NONE',  ( 29.99999999999999645, 2.375000000000000000, 0.000000000000000000 ) ) ;
#138265 = DIRECTION ( 'NONE',  ( -0.6830127018922181881, 0.6830127018922202975, -0.2588190451025214056 ) ) ;
#138266 = DIRECTION ( 'NONE',  ( 0.000000000000000000, -1.000000000000000000, 0.000000000000000000 ) ) ;
#138267 = CARTESIAN_POINT ( 'NONE',  ( -2.206660635421508143, 21.75929247661549937, 4.998822639870708073 ) ) ;
#138268 = AXIS2_PLACEMENT_3D ( 'NONE', #22557, #79880, #103014 ) ;
#138269 = EDGE_CURVE ( 'NONE', #14195, #10130, #47070, .T. ) ;
#138270 = CARTESIAN_POINT ( 'NONE',  ( 53.01669371712955581, 7.950000000000000178, -2.130196079827421318 ) ) ;
#138271 =( BOUNDED_CURVE ( )  B_SPLINE_CURVE ( 3, ( #57558, #13285, #101748, #124217 ),
 .UNSPECIFIED., .F., .T. ) 
 B_SPLINE_CURVE_WITH_KNOTS ( ( 4, 4 ),
 ( 2.228251278275057867, 2.286295730127291037 ),
 .UNSPECIFIED. ) 
 CURVE ( )  GEOMETRIC_REPRESENTATION_ITEM ( )  RATIONAL_B_SPLINE_CURVE ( ( 1.000000000000000000, 0.9997192565072046122, 0.9997192565072046122, 1.000000000000000000 ) ) 
 REPRESENTATION_ITEM ( '' )  );
#138272 = CARTESIAN_POINT ( 'NONE',  ( 26.99999999999980815, 4.931123077392136622, 4.000000000000000000 ) ) ;
#138273 =( LENGTH_UNIT ( ) NAMED_UNIT ( * ) SI_UNIT ( .MILLI., .METRE. ) );
#138274 = ORIENTED_EDGE ( 'NONE', *, *, #141008, .F. ) ;
#138275 = VECTOR ( 'NONE', #62932, 1000.000000000000000 ) ;
#138276 = ORIENTED_EDGE ( 'NONE', *, *, #91531, .F. ) ;
#138277 = ORIENTED_EDGE ( 'NONE', *, *, #92476, .F. ) ;
#138278 = EDGE_LOOP ( 'NONE', ( #87673, #72713, #72940, #120831 ) ) ;
#138279 = ADVANCED_FACE ( 'NONE', ( #26675 ), #101377, .F. ) ;
#138280 = VECTOR ( 'NONE', #71570, 999.9999999999998863 ) ;
#138281 = DIRECTION ( 'NONE',  ( -0.7071067811865487940, 0.7071067811865463515, -0.000000000000000000 ) ) ;
#138282 = EDGE_CURVE ( 'NONE', #67593, #2749, #135460, .T. ) ;
#138283 = PRESENTATION_STYLE_ASSIGNMENT (( #117910 ) ) ;
#138284 = EDGE_LOOP ( 'NONE', ( #39150, #13888, #72228, #136988 ) ) ;
#138285 = CARTESIAN_POINT ( 'NONE',  ( -15.70701326429294475, -21.74070752338406365, 4.999753212805219782 ) ) ;
#138286 = CARTESIAN_POINT ( 'NONE',  ( -2.700255128608413990, -27.71228299555204089, 4.000000000000000000 ) ) ;
#138287 = EDGE_CURVE ( 'NONE', #19965, #109971, #90518, .T. ) ;
#138288 = DIRECTION ( 'NONE',  ( -0.000000000000000000, 0.3543493200069153248, 0.9351131265310292928 ) ) ;
#138289 = AXIS2_PLACEMENT_3D ( 'NONE', #8532, #142673, #52781 ) ;
#138290 = DIRECTION ( 'NONE',  ( -1.000000000000000000, -1.224606353822377258E-16, -0.000000000000000000 ) ) ;
#138291 = DIRECTION ( 'NONE',  ( -0.6830127018922181881, 0.6830127018922202975, -0.2588190451025214056 ) ) ;
#138292 = ORIENTED_EDGE ( 'NONE', *, *, #64775, .F. ) ;
#138293 = ADVANCED_FACE ( 'NONE', ( #35454 ), #134761, .F. ) ;
#138294 = CARTESIAN_POINT ( 'NONE',  ( 13.13598696172163116, 3.061616997868383634E-16, -2.500000000000000444 ) ) ;
#138295 = LINE ( 'NONE', #102819, #55853 ) ;
#138296 = ORIENTED_EDGE ( 'NONE', *, *, #70412, .F. ) ;
#138297 = CARTESIAN_POINT ( 'NONE',  ( 27.48921356237309155, -27.52281430457074762, 5.000000000000000000 ) ) ;
#138298 = VERTEX_POINT ( 'NONE', #79688 ) ;
#138299 = EDGE_LOOP ( 'NONE', ( #39224, #121010, #19246, #121333, #53737 ) ) ;
#138300 = CARTESIAN_POINT ( 'NONE',  ( 12.14997294953710849, -4.461849672132299105, 4.461849672132299993 ) ) ;
#138301 = ORIENTED_EDGE ( 'NONE', *, *, #128798, .F. ) ;
#138302 = ORIENTED_EDGE ( 'NONE', *, *, #61151, .T. ) ;
#138303 = CARTESIAN_POINT ( 'NONE',  ( 77.29209685856477563, -5.291415217122921177, 3.054999999999999272 ) ) ;
#138304 = VERTEX_POINT ( 'NONE', #58658 ) ;
#138305 = DIRECTION ( 'NONE',  ( -0.6830127018922181881, 0.6830127018922202975, -0.2588190451025214056 ) ) ;
#138306 = CARTESIAN_POINT ( 'NONE',  ( 6.489213562373093325, -27.52281430457059841, 5.000000000000000000 ) ) ;
#138307 = VECTOR ( 'NONE', #95111, 1000.000000000000000 ) ;
#138308 = CARTESIAN_POINT ( 'NONE',  ( 108.3545968585647614, -1.637169565754161615, 6.110000000000000320 ) ) ;
#138309 = FACE_OUTER_BOUND ( 'NONE', #99071, .T. ) ;
#138310 = EDGE_CURVE ( 'NONE', #45577, #33663, #102824, .T. ) ;
#138311 = CARTESIAN_POINT ( 'NONE',  ( -3.792893218813431222, 6.759292476615651246, 5.000000000000000000 ) ) ;
#138312 = FACE_OUTER_BOUND ( 'NONE', #282, .T. ) ;
#138313 = EDGE_CURVE ( 'NONE', #122295, #75714, #129162, .T. ) ;
#138314 = DIRECTION ( 'NONE',  ( -0.6830127018922181881, 0.6830127018922202975, -0.2588190451025214056 ) ) ;
#138315 =( LENGTH_UNIT ( ) NAMED_UNIT ( * ) SI_UNIT ( .MILLI., .METRE. ) );
#138316 = DIRECTION ( 'NONE',  ( 0.000000000000000000, 0.000000000000000000, 1.000000000000000000 ) ) ;
#138317 = ORIENTED_EDGE ( 'NONE', *, *, #116127, .F. ) ;
#138318 = FILL_AREA_STYLE_COLOUR ( '', #83072 ) ;
#138319 = LINE ( 'NONE', #5629, #1198 ) ;
#138320 = ORIENTED_EDGE ( 'NONE', *, *, #119556, .T. ) ;
#138321 = ORIENTED_EDGE ( 'NONE', *, *, #108139, .T. ) ;
#138322 = LINE ( 'NONE', #31527, #47350 ) ;
#138323 = ORIENTED_EDGE ( 'NONE', *, *, #94915, .T. ) ;
#138324 = TOROIDAL_SURFACE ( 'NONE', #136038, 25.00000000000002487, 3.000000000000000000 ) ;
#138325 = DIRECTION ( 'NONE',  ( -0.7071067811865486830, 0.7071067811865464625, 0.000000000000000000 ) ) ;
#138326 = CARTESIAN_POINT ( 'NONE',  ( 33.18398860626899705, 28.73617430169810305, 5.000000000000000000 ) ) ;
#138327 = VECTOR ( 'NONE', #13426, 1000.000000000000000 ) ;
#138328 = FACE_OUTER_BOUND ( 'NONE', #20619, .T. ) ;
#138329 = FACE_OUTER_BOUND ( 'NONE', #127990, .T. ) ;
#138330 = VERTEX_POINT ( 'NONE', #24530 ) ;
#138331 = FILL_AREA_STYLE_COLOUR ( '', #85906 ) ;
#138332 = VERTEX_POINT ( 'NONE', #94761 ) ;
#138333 = AXIS2_PLACEMENT_3D ( 'NONE', #34707, #57911, #78944 ) ;
#138334 = VECTOR ( 'NONE', #2748, 1000.000000000000227 ) ;
#138335 = ADVANCED_FACE ( 'NONE', ( #83948 ), #105632, .T. ) ;
#138336 = AXIS2_PLACEMENT_3D ( 'NONE', #120187, #109352, #121638 ) ;
#138337 = CARTESIAN_POINT ( 'NONE',  ( 1.728736474768552522, 5.808823158059031044, -5.808823158059038150 ) ) ;
#138338 = CARTESIAN_POINT ( 'NONE',  ( 90.64169371712954160, -2.130196079827424871, -7.949999999999998401 ) ) ;
#138339 = CARTESIAN_POINT ( 'NONE',  ( -48.29974487139158867, -27.71228299555239971, 4.000000000000000000 ) ) ;
#138340 = CARTESIAN_POINT ( 'NONE',  ( 30.70701326429282929, -21.74070752338406365, 4.999753212805224223 ) ) ;
#138341 = ORIENTED_EDGE ( 'NONE', *, *, #52343, .T. ) ;
#138342 = EDGE_LOOP ( 'NONE', ( #108068, #55731, #26700, #136725, #68347, #134086 ) ) ;
#138343 = ORIENTED_EDGE ( 'NONE', *, *, #5526, .T. ) ;
#138344 = LINE ( 'NONE', #17947, #123700 ) ;
#138345 = DIRECTION ( 'NONE',  ( 1.000000000000000000, 0.000000000000000000, 0.000000000000000000 ) ) ;
#138346 = VECTOR ( 'NONE', #125954, 1000.000000000000000 ) ;
#138347 = CARTESIAN_POINT ( 'NONE',  ( 5.700255128608413102, -27.71228299555201957, 4.000000000000000000 ) ) ;
#138348 = FILL_AREA_STYLE_COLOUR ( '', #77409 ) ;
#138349 = ADVANCED_FACE ( 'NONE', ( #129541 ), #27363, .F. ) ;
#138350 = CARTESIAN_POINT ( 'NONE',  ( -36.18398860626899705, 28.73617430169812437, 5.000000000000000000 ) ) ;
#138351 = FACE_OUTER_BOUND ( 'NONE', #142293, .T. ) ;
#138352 = CARTESIAN_POINT ( 'NONE',  ( 25.19159235450331735, -2.500000000000000000, 3.061616997868384127E-16 ) ) ;
#138353 = CARTESIAN_POINT ( 'NONE',  ( -6.489213562373093325, -27.52281430457059841, 5.000000000000000000 ) ) ;
#138354 = CARTESIAN_POINT ( 'NONE',  ( 0.000000000000000000, 0.000000000000000000, 5.000000000000000000 ) ) ;
#138355 = ORIENTED_EDGE ( 'NONE', *, *, #47489, .F. ) ;
#138356 = CARTESIAN_POINT ( 'NONE',  ( 28.49999999999980460, 0.4497235411627734103, -5.599840258123474968 ) ) ;
#138357 = DIRECTION ( 'NONE',  ( 0.7071067811865487940, 0.7071067811865463515, 0.000000000000000000 ) ) ;
#138358 = ORIENTED_EDGE ( 'NONE', *, *, #57775, .F. ) ;
#138359 = CARTESIAN_POINT ( 'NONE',  ( -18.32816939922339472, -12.74070752338414891, 4.000000000000000000 ) ) ;
#138361 = EDGE_LOOP ( 'NONE', ( #135666, #47944, #128768, #55349 ) ) ;
#138360 = CARTESIAN_POINT ( 'NONE',  ( 55.47768537941234257, -49.13871568196521622, -40.16438383193002437 ) ) ;
#138362 = CARTESIAN_POINT ( 'NONE',  ( 6.005480084712508493, 28.92564299267933947, 4.000000000000000000 ) ) ;
#138364 = VECTOR ( 'NONE', #22887, 1000.000000000000227 ) ;
#138363 = CARTESIAN_POINT ( 'NONE',  ( 4.499999999999972466, 21.43112307739196609, 4.000000000000000000 ) ) ;
#138365 = ORIENTED_EDGE ( 'NONE', *, *, #76244, .T. ) ;
#138366 = LINE ( 'NONE', #136214, #134606 ) ;
#138367 = EDGE_LOOP ( 'NONE', ( #21630, #31012, #91097 ) ) ;
#138368 = DIRECTION ( 'NONE',  ( -0.7071067811865487940, 0.7071067811865463515, 0.000000000000000000 ) ) ;
#138369 = CARTESIAN_POINT ( 'NONE',  ( -27.18398860626900060, 28.73617430169806042, 5.000000000000000000 ) ) ;
#138370 = CARTESIAN_POINT ( 'NONE',  ( 117.9125270504628986, -7.949999999999998401, -4.867971026610728450E-16 ) ) ;
#138371 = VECTOR ( 'NONE', #15797, 999.9999999999998863 ) ;
#138372 = CARTESIAN_POINT ( 'NONE',  ( -15.79289321881334551, -5.240707523384225297, 5.000000000000000000 ) ) ;
#138373 = DIRECTION ( 'NONE',  ( -0.7071067811865487940, 0.7071067811865463515, 0.000000000000000000 ) ) ;
#138374 = FACE_OUTER_BOUND ( 'NONE', #8605, .T. ) ;
#138375 = DIRECTION ( 'NONE',  ( -0.7071067811865487940, 0.7071067811865463515, -0.000000000000000000 ) ) ;
#138376 = CARTESIAN_POINT ( 'NONE',  ( -27.75860074219777118, 21.72500000000000142, 5.000000000000000000 ) ) ;
#138377 = CARTESIAN_POINT ( 'NONE',  ( 28.85373647476855652, -5.808823158059035485, -5.808823158059033709 ) ) ;
#138378 = CARTESIAN_POINT ( 'NONE',  ( 11.06206980810188689, -7.934999999999990727, -2.126176841940955242 ) ) ;
#138379 = CARTESIAN_POINT ( 'NONE',  ( -16.80981832425541356, -18.74070752338408852, 7.910009926591547114 ) ) ;
#138380 = CARTESIAN_POINT ( 'NONE',  ( 34.42499999999998295, 7.541399257801974620, 5.000000000000000000 ) ) ;
#138381 = CARTESIAN_POINT ( 'NONE',  ( 34.49999999999975842, 15.05432934483078888, 4.994342998332163219 ) ) ;
#138382 = ORIENTED_EDGE ( 'NONE', *, *, #111751, .F. ) ;
#138383 = ORIENTED_EDGE ( 'NONE', *, *, #113442, .F. ) ;
#138384 = CARTESIAN_POINT ( 'NONE',  ( 79.31250000000000000, 5.819803920172571310, 5.819803920172575751 ) ) ;
#138386 = EDGE_LOOP ( 'NONE', ( #50877, #18011, #16387, #83853 ) ) ;
#138385 = DIRECTION ( 'NONE',  ( 0.000000000000000000, -1.000000000000000000, 0.000000000000000000 ) ) ;
#138387 = ORIENTED_EDGE ( 'NONE', *, *, #4742, .T. ) ;
#138388 = PRODUCT_DEFINITION_SHAPE ( 'NONE', 'NONE',  #143571 ) ;
#138389 = EDGE_CURVE ( 'NONE', #12163, #41563, #60782, .T. ) ;
#138390 = LINE ( 'NONE', #125382, #106526 ) ;
#138391 = LINE ( 'NONE', #140516, #131108 ) ;
#138392 = ORIENTED_EDGE ( 'NONE', *, *, #133181, .F. ) ;
#138393 = PLANE ( 'NONE',  #101920 ) ;
#138394 = CARTESIAN_POINT ( 'NONE',  ( -9.707106781186480404, 17.25929247661554911, 5.000000000000000000 ) ) ;
#138395 = EDGE_CURVE ( 'NONE', #58880, #32751, #83904, .T. ) ;
#138396 = EDGE_CURVE ( 'NONE', #27314, #141369, #28107, .T. ) ;
#138398 = AXIS2_PLACEMENT_3D ( 'NONE', #121510, #9140, #130994 ) ;
#138397 = CARTESIAN_POINT ( 'NONE',  ( -11.99999999999991296, 1.931123077392161935, 4.000000000000000000 ) ) ;
#138399 = DIRECTION ( 'NONE',  ( -0.000000000000000000, -0.3543493200069152693, 0.9351131265310292928 ) ) ;
#138400 = ADVANCED_FACE ( 'NONE', ( #139017 ), #83073, .T. ) ;
#138401 = EDGE_CURVE ( 'NONE', #94913, #105827, #41119, .T. ) ;
#138402 = DIRECTION ( 'NONE',  ( 0.6830127018922180770, -0.6830127018922204085, -0.2588190451025213501 ) ) ;
#138403 = DIRECTION ( 'NONE',  ( 1.000000000000000000, 0.000000000000000000, 0.000000000000000000 ) ) ;
#138404 = CARTESIAN_POINT ( 'NONE',  ( -10.62823445044378268, -8.240707523384203981, 11.38925528200755011 ) ) ;
#138405 = DIRECTION ( 'NONE',  ( 0.3543493200069163240, 0.000000000000000000, 0.9351131265310288487 ) ) ;
#138406 = DIRECTION ( 'NONE',  ( 0.000000000000000000, -1.000000000000000000, 0.000000000000000000 ) ) ;
#138407 = CARTESIAN_POINT ( 'NONE',  ( 15.48921356237309510, -27.52281430457066236, 5.000000000000000000 ) ) ;
#138408 = DIRECTION ( 'NONE',  ( 0.000000000000000000, 0.000000000000000000, 1.000000000000000000 ) ) ;
#138409 = DIRECTION ( 'NONE',  ( 0.5735764363510451602, 0.8191520442889924647, 0.000000000000000000 ) ) ;
#138410 = EDGE_CURVE ( 'NONE', #131245, #89344, #6539, .T. ) ;
#138411 = EDGE_CURVE ( 'NONE', #77035, #109693, #140902, .T. ) ;
#138412 = ORIENTED_EDGE ( 'NONE', *, *, #107449, .T. ) ;
#138413 = ORIENTED_EDGE ( 'NONE', *, *, #48125, .T. ) ;
#138414 = CARTESIAN_POINT ( 'NONE',  ( 104.5629301918981184, 1.637169565754157174, 6.110000000000002984 ) ) ;
#138415 = VECTOR ( 'NONE', #53224, 999.9999999999998863 ) ;
#138416 = ORIENTED_EDGE ( 'NONE', *, *, #9105, .T. ) ;
#138417 = EDGE_CURVE ( 'NONE', #27246, #142384, #117926, .T. ) ;
#138418 = PLANE ( 'NONE',  #131241 ) ;
#138419 = ADVANCED_FACE ( 'NONE', ( #7754 ), #74490, .F. ) ;
#138420 = DIRECTION ( 'NONE',  ( -0.7071067811865487940, 0.7071067811865463515, 0.000000000000000000 ) ) ;
#138421 = ORIENTED_EDGE ( 'NONE', *, *, #112470, .T. ) ;
#138422 = DIRECTION ( 'NONE',  ( -0.7071067811865486830, -0.7071067811865464625, -0.000000000000000000 ) ) ;
#138423 = CYLINDRICAL_SURFACE ( 'NONE', #90621, 2.500000000000000444 ) ;
#138424 = ADVANCED_FACE ( 'NONE', ( #135908 ), #125025, .F. ) ;
#138425 = VECTOR ( 'NONE', #103774, 1000.000000000000000 ) ;
#138426 = CARTESIAN_POINT ( 'NONE',  ( 107.0995968585648086, -6.109999999999997655, -1.637169565754160283 ) ) ;
#138427 = ORIENTED_EDGE ( 'NONE', *, *, #126232, .T. ) ;
#138428 = FACE_OUTER_BOUND ( 'NONE', #49443, .T. ) ;
#138429 = ORIENTED_EDGE ( 'NONE', *, *, #62999, .F. ) ;
#138430 = CARTESIAN_POINT ( 'NONE',  ( 28.17183060077627843, -17.24070752338409918, 4.000000000000000000 ) ) ;
#138431 = DIRECTION ( 'NONE',  ( 0.7071067811865487940, 0.7071067811865463515, 0.000000000000000000 ) ) ;
#138432 = CARTESIAN_POINT ( 'NONE',  ( 32.47599861414528277, 22.03583458319438648, 4.979811245910084061 ) ) ;
#138433 =( GEOMETRIC_REPRESENTATION_CONTEXT ( 3 ) GLOBAL_UNCERTAINTY_ASSIGNED_CONTEXT ( ( #60659 ) ) GLOBAL_UNIT_ASSIGNED_CONTEXT ( ( #123568, #24227, #124243 ) ) REPRESENTATION_CONTEXT ( 'NONE', 'WORKASPACE' ) );
#138434 = CARTESIAN_POINT ( 'NONE',  ( -15.48921356237309510, -27.52281430457066236, 5.000000000000000000 ) ) ;
#138435 = ADVANCED_FACE ( 'NONE', ( #127157 ), #35915, .F. ) ;
#138436 = ORIENTED_EDGE ( 'NONE', *, *, #19281, .T. ) ;
#138437 = EDGE_LOOP ( 'NONE', ( #103721, #10866, #118808, #6556 ) ) ;
#138438 = VECTOR ( 'NONE', #100309, 1000.000000000000000 ) ;
#138439 = ORIENTED_EDGE ( 'NONE', *, *, #44796, .T. ) ;
#138440 = CARTESIAN_POINT ( 'NONE',  ( -15.18398860626900237, 28.73617430169797871, 5.000000000000000000 ) ) ;
#138441 = CARTESIAN_POINT ( 'NONE',  ( -57.29974487139158157, -27.71228299555246011, 4.000000000000000000 ) ) ;
#138442 = CARTESIAN_POINT ( 'NONE',  ( 7.212903141435218934, 3.967499999999992699, -6.871911579029513994 ) ) ;
#138443 = ADVANCED_FACE ( 'NONE', ( #48915 ), #69241, .T. ) ;
#138444 = VECTOR ( 'NONE', #22528, 1000.000000000000000 ) ;
#138445 = CARTESIAN_POINT ( 'NONE',  ( -24.48921356237309510, -27.52281430457072631, 5.000000000000000000 ) ) ;
#138446 = DIRECTION ( 'NONE',  ( -0.000000000000000000, -0.000000000000000000, 1.000000000000000000 ) ) ;
#138447 = ORIENTED_EDGE ( 'NONE', *, *, #141757, .F. ) ;
#138448 = ORIENTED_EDGE ( 'NONE', *, *, #10527, .T. ) ;
#138449 = DIRECTION ( 'NONE',  ( 0.7071067811865487940, -0.7071067811865463515, 0.000000000000000000 ) ) ;
#138450 = ORIENTED_EDGE ( 'NONE', *, *, #107001, .T. ) ;
#138451 = ORIENTED_EDGE ( 'NONE', *, *, #97038, .T. ) ;
#138452 = ADVANCED_FACE ( 'NONE', ( #136606, #13386 ), #38739, .T. ) ;
#138453 = CARTESIAN_POINT ( 'NONE',  ( 113.8079301918981088, -6.109999999999998543, 1.637169565754158507 ) ) ;
#138454 = EDGE_CURVE ( 'NONE', #5991, #19902, #3912, .T. ) ;
#138455 = PLANE ( 'NONE',  #4881 ) ;
#138456 = LINE ( 'NONE', #94919, #47227 ) ;
#138457 = VERTEX_POINT ( 'NONE', #24983 ) ;
#138458 = CARTESIAN_POINT ( 'NONE',  ( 17.99999999999987566, -12.41253812416062985, 4.000000000000000000 ) ) ;
#138459 = EDGE_CURVE ( 'NONE', #94920, #62368, #115535, .T. ) ;
#138460 = LINE ( 'NONE', #72534, #140455 ) ;
#138461 = LINE ( 'NONE', #53600, #76134 ) ;
#138462 = DIRECTION ( 'NONE',  ( -0.000000000000000000, 0.3543493200069153248, 0.9351131265310292928 ) ) ;
#138463 = ORIENTED_EDGE ( 'NONE', *, *, #134826, .F. ) ;
#138465 = EDGE_CURVE ( 'NONE', #72863, #12885, #3233, .T. ) ;
#138464 = VECTOR ( 'NONE', #73466, 1000.000000000000000 ) ;
#138466 = LINE ( 'NONE', #105792, #104220 ) ;
#138467 = FACE_BOUND ( 'NONE', #20821, .T. ) ;
#138468 = VERTEX_POINT ( 'NONE', #59107 ) ;
#138469 = FACE_OUTER_BOUND ( 'NONE', #137631, .T. ) ;
#138470 = DIRECTION ( 'NONE',  ( 0.3543493200069162685, -0.000000000000000000, -0.9351131265310288487 ) ) ;
#138471 = PLANE ( 'NONE',  #32990 ) ;
#138472 = ORIENTED_EDGE ( 'NONE', *, *, #34693, .T. ) ;
#138473 = CARTESIAN_POINT ( 'NONE',  ( 1.592112669765240796, 0.4000000000000001887, -2.358007193124714629 ) ) ;
#138474 = ORIENTED_EDGE ( 'NONE', *, *, #11063, .T. ) ;
#138475 = VECTOR ( 'NONE', #121164, 1000.000000000000000 ) ;
#138476 = ORIENTED_EDGE ( 'NONE', *, *, #46836, .T. ) ;
#138477 = EDGE_CURVE ( 'NONE', #102772, #82836, #103263, .T. ) ;
#138478 = ORIENTED_EDGE ( 'NONE', *, *, #84442, .T. ) ;
#138479 = CARTESIAN_POINT ( 'NONE',  ( 30.09959685856477662, -6.109999999999997655, -1.637169565754160283 ) ) ;
#138480 = VERTEX_POINT ( 'NONE', #135226 ) ;
#138481 = CARTESIAN_POINT ( 'NONE',  ( -39.48921356237310221, -27.52281430457082934, 5.000000000000000000 ) ) ;
#138482 = DIRECTION ( 'NONE',  ( 0.7071067811865487940, 0.7071067811865463515, -0.000000000000000000 ) ) ;
#138483 = CARTESIAN_POINT ( 'NONE',  ( 0.7071067811865398012, -15.74070752338413115, 5.000000000000000000 ) ) ;
#138484 = EDGE_CURVE ( 'NONE', #47660, #77866, #47524, .T. ) ;
#138485 = CARTESIAN_POINT ( 'NONE',  ( 36.18398860626899705, 28.73617430169812437, 5.000000000000000000 ) ) ;
#138486 = DIRECTION ( 'NONE',  ( 1.301042606982605074E-16, -1.000000000000000000, 0.000000000000000000 ) ) ;
#138487 = AXIS2_PLACEMENT_3D ( 'NONE', #60050, #26689, #2783 ) ;
#138488 =( BOUNDED_CURVE ( )  B_SPLINE_CURVE ( 3, ( #61969, #49675, #5393, #106125 ),
 .UNSPECIFIED., .F., .F. ) 
 B_SPLINE_CURVE_WITH_KNOTS ( ( 4, 4 ),
 ( 4.350170835173026163, 4.500739107949192075 ),
 .UNSPECIFIED. ) 
 CURVE ( )  GEOMETRIC_REPRESENTATION_ITEM ( )  RATIONAL_B_SPLINE_CURVE ( ( 1.000000000000000000, 0.9981116584018963067, 0.9981116584018963067, 1.000000000000000000 ) ) 
 REPRESENTATION_ITEM ( '' )  );
#138489 = DIRECTION ( 'NONE',  ( 0.7071067811865487940, 0.7071067811865463515, 0.000000000000000000 ) ) ;
#138490 = VECTOR ( 'NONE', #45326, 1000.000000000000000 ) ;
#138491 = CARTESIAN_POINT ( 'NONE',  ( 76.25000000000000000, -9.735942053221458872E-16, 7.950000000000000178 ) ) ;
#138492 = LINE ( 'NONE', #29009, #103830 ) ;
#138493 = DIRECTION ( 'NONE',  ( 0.6830127018922180770, -0.6830127018922204085, -0.2588190451025213501 ) ) ;
#138494 = ORIENTED_EDGE ( 'NONE', *, *, #138589, .T. ) ;
#138495 = VERTEX_POINT ( 'NONE', #113423 ) ;
#138496 = ORIENTED_EDGE ( 'NONE', *, *, #88595, .T. ) ;
#138497 = ORIENTED_EDGE ( 'NONE', *, *, #121527, .F. ) ;
#138498 = LINE ( 'NONE', #118869, #105016 ) ;
#138499 = ORIENTED_EDGE ( 'NONE', *, *, #15485, .T. ) ;
#138500 = VERTEX_POINT ( 'NONE', #137349 ) ;
#138501 = FACE_OUTER_BOUND ( 'NONE', #31912, .T. ) ;
#138502 = ADVANCED_FACE ( 'NONE', ( #103959 ), #72119, .F. ) ;
#138503 = LINE ( 'NONE', #93568, #85623 ) ;
#138504 = ORIENTED_EDGE ( 'NONE', *, *, #18023, .T. ) ;
#138505 = CARTESIAN_POINT ( 'NONE',  ( 28.17665910159955800, 5.259292476615669010, 15.86257073897091452 ) ) ;
#138506 = ORIENTED_EDGE ( 'NONE', *, *, #54268, .T. ) ;
#138507 = CARTESIAN_POINT ( 'NONE',  ( 34.92499999999997584, 20.71849043720405348, 4.759050581649322709 ) ) ;
#138508 = ADVANCED_FACE ( 'NONE', ( #125763 ), #26436, .F. ) ;
#138509 = DIRECTION ( 'NONE',  ( -0.000000000000000000, -0.3543493200069152693, 0.9351131265310292928 ) ) ;
#138510 =( LENGTH_UNIT ( ) NAMED_UNIT ( * ) SI_UNIT ( .MILLI., .METRE. ) );
#138511 = ORIENTED_EDGE ( 'NONE', *, *, #81944, .T. ) ;
#138513 = DIRECTION ( 'NONE',  ( 0.7071067811865487940, -0.7071067811865463515, 0.000000000000000000 ) ) ;
#138512 = CARTESIAN_POINT ( 'NONE',  ( 105.3495968585647944, 6.109999999999997655, 1.637169565754163836 ) ) ;
#138514 = CARTESIAN_POINT ( 'NONE',  ( 15.98911971346040062, -22.02621442084248216, 4.990779571109220214 ) ) ;
#138515 = CARTESIAN_POINT ( 'NONE',  ( 20.99999999999985789, -8.151047557385048492, -8.977947279169846695 ) ) ;
#138516 = ORIENTED_EDGE ( 'NONE', *, *, #133030, .F. ) ;
#138517 = EDGE_LOOP ( 'NONE', ( #125329, #108497, #37429, #83295 ) ) ;
#138518 = LINE ( 'NONE', #39205, #14871 ) ;
#138519 = ORIENTED_EDGE ( 'NONE', *, *, #42876, .T. ) ;
#138520 =( NAMED_UNIT ( * ) SI_UNIT ( $, .STERADIAN. ) SOLID_ANGLE_UNIT ( ) );
#138521 = LINE ( 'NONE', #127647, #125041 ) ;
#138522 = PLANE ( 'NONE',  #17559 ) ;
#138523 = CARTESIAN_POINT ( 'NONE',  ( 3.183988606268992161, 28.73617430169789699, 5.000000000000000000 ) ) ;
#138524 = CARTESIAN_POINT ( 'NONE',  ( -20.99999999999984368, 4.384688058510544550, -7.090945410444732033 ) ) ;
#138526 = ADVANCED_FACE ( 'NONE', ( #59791 ), #82265, .F. ) ;
#138525 = ORIENTED_EDGE ( 'NONE', *, *, #138147, .F. ) ;
#138527 = CARTESIAN_POINT ( 'NONE',  ( -22.17183060077632106, 15.75929247661555443, 4.000000000000000000 ) ) ;
#138528 = EDGE_CURVE ( 'NONE', #44417, #38530, #49648, .T. ) ;
#138529 = SURFACE_STYLE_USAGE ( .BOTH. , #58884 ) ;
#138530 = DIRECTION ( 'NONE',  ( -0.7071067811865486830, -0.7071067811865464625, -0.000000000000000000 ) ) ;
#138531 = ORIENTED_EDGE ( 'NONE', *, *, #91600, .T. ) ;
#138532 = CARTESIAN_POINT ( 'NONE',  ( -34.42500000000001137, -21.72500000000000142, 4.500000000000000888 ) ) ;
#138533 = AXIS2_PLACEMENT_3D ( 'NONE', #7909, #131144, #31829 ) ;
#138534 =( GEOMETRIC_REPRESENTATION_CONTEXT ( 3 ) GLOBAL_UNCERTAINTY_ASSIGNED_CONTEXT ( ( #9955 ) ) GLOBAL_UNIT_ASSIGNED_CONTEXT ( ( #59728, #19574, #114080 ) ) REPRESENTATION_CONTEXT ( 'NONE', 'WORKASPACE' ) );
#138535 = DIRECTION ( 'NONE',  ( -0.7071067811865487940, 0.7071067811865463515, -0.000000000000000000 ) ) ;
#138536 = ORIENTED_EDGE ( 'NONE', *, *, #68873, .T. ) ;
#138537 = VECTOR ( 'NONE', #119008, 1000.000000000000000 ) ;
#138539 = VERTEX_POINT ( 'NONE', #2502 ) ;
#138538 = LINE ( 'NONE', #139273, #134289 ) ;
#138540 = EDGE_CURVE ( 'NONE', #47195, #35346, #46817, .T. ) ;
#138541 = ORIENTED_EDGE ( 'NONE', *, *, #88229, .T. ) ;
#138542 = CARTESIAN_POINT ( 'NONE',  ( 1.015767586731733507, 13.72868181898487450, -24.38142353947347374 ) ) ;
#138543 = AXIS2_PLACEMENT_3D ( 'NONE', #21699, #110113, #86258 ) ;
#138544 = ORIENTED_EDGE ( 'NONE', *, *, #47193, .F. ) ;
#138545 = LINE ( 'NONE', #39235, #48920 ) ;
#138546 = AXIS2_PLACEMENT_3D ( 'NONE', #45611, #142747, #12216 ) ;
#138547 = CARTESIAN_POINT ( 'NONE',  ( 26.16170612452603095, -6.740707523384216415, 16.75550250614873704 ) ) ;
#138548 = EDGE_LOOP ( 'NONE', ( #28669, #24117, #133183, #21967 ) ) ;
#138549 = DIRECTION ( 'NONE',  ( 0.7071067811865487940, -0.7071067811865463515, 0.000000000000000000 ) ) ;
#138550 = DIRECTION ( 'NONE',  ( -0.7071067811865486830, -0.7071067811865464625, -0.000000000000000000 ) ) ;
#138551 = DIRECTION ( 'NONE',  ( 0.7071067811865486830, -0.7071067811865464625, -0.000000000000000000 ) ) ;
#138552 = DIRECTION ( 'NONE',  ( -0.7071067811865487940, 0.7071067811865463515, -0.000000000000000000 ) ) ;
#138553 = DIRECTION ( 'NONE',  ( 8.673617379884034239E-17, -1.000000000000000000, 0.000000000000000000 ) ) ;
#138555 = VECTOR ( 'NONE', #12631, 1000.000000000000227 ) ;
#138554 = LINE ( 'NONE', #140672, #74456 ) ;
#138556 = CARTESIAN_POINT ( 'NONE',  ( 29.99999999999979039, 16.55218569542899587, 5.000000000000000000 ) ) ;
#138557 = DIRECTION ( 'NONE',  ( 0.7071067811865487940, 0.7071067811865463515, -0.000000000000000000 ) ) ;
#138558 = FACE_OUTER_BOUND ( 'NONE', #92617, .T. ) ;
#138559 = ORIENTED_EDGE ( 'NONE', *, *, #70748, .T. ) ;
#138560 = EDGE_LOOP ( 'NONE', ( #68872, #137448, #17895, #90333, #37280 ) ) ;
#138561 = ORIENTED_EDGE ( 'NONE', *, *, #16145, .F. ) ;
#138562 = CARTESIAN_POINT ( 'NONE',  ( 110.2291666666666714, 7.950000000000001954, -2.130196079827421762 ) ) ;
#138563 = VECTOR ( 'NONE', #138373, 1000.000000000000000 ) ;
#138564 = ORIENTED_EDGE ( 'NONE', *, *, #139650, .T. ) ;
#138565 = ORIENTED_EDGE ( 'NONE', *, *, #72655, .F. ) ;
#138566 = ORIENTED_EDGE ( 'NONE', *, *, #2288, .F. ) ;
#138567 = DIRECTION ( 'NONE',  ( -0.6830127018922180770, -0.6830127018922204085, -0.2588190451025213501 ) ) ;
#138568 = AXIS2_PLACEMENT_3D ( 'NONE', #13712, #24614, #102907 ) ;
#138569 = EDGE_CURVE ( 'NONE', #1190, #47403, #58403, .T. ) ;
#138570 = DIRECTION ( 'NONE',  ( -0.7071067811865486830, -0.7071067811865464625, -0.000000000000000000 ) ) ;
#138571 = ORIENTED_EDGE ( 'NONE', *, *, #78606, .T. ) ;
#138572 = CARTESIAN_POINT ( 'NONE',  ( -1.171830600776462061, 0.7592924766157069794, 4.000000000000000000 ) ) ;
#138573 = DIRECTION ( 'NONE',  ( 0.7071067811865486830, -0.7071067811865464625, -0.000000000000000000 ) ) ;
#138574 = VECTOR ( 'NONE', #118117, 1000.000000000000000 ) ;
#138575 = CARTESIAN_POINT ( 'NONE',  ( 34.96659967656956525, 6.759292476615656575, 12.28218704918530157 ) ) ;
#138576 = PLANE ( 'NONE',  #78916 ) ;
#138577 = CARTESIAN_POINT ( 'NONE',  ( 114.6254301918981042, 5.291415217122919401, 3.055000000000002824 ) ) ;
#138578 = EDGE_LOOP ( 'NONE', ( #39194, #7364, #82008 ) ) ;
#138579 = ADVANCED_FACE ( 'NONE', ( #46019 ), #101075, .F. ) ;
#138580 = CARTESIAN_POINT ( 'NONE',  ( 6.852250093007166143, 4.584330080086930965E-16, 0.000000000000000000 ) ) ;
#138581 = LINE ( 'NONE', #102748, #102522 ) ;
#138582 = DIRECTION ( 'NONE',  ( -0.7071067811865487940, 0.7071067811865463515, -0.000000000000000000 ) ) ;
#138583 = CARTESIAN_POINT ( 'NONE',  ( 17.22560490425083657, 3.061616997868387579E-16, -2.500000000000000444 ) ) ;
#138584 = CARTESIAN_POINT ( 'NONE',  ( 21.48921356237309155, -27.52281430457070499, 5.000000000000000000 ) ) ;
#138585 = DIRECTION ( 'NONE',  ( 0.6830127018922181881, 0.6830127018922202975, -0.2588190451025214056 ) ) ;
#138586 = CARTESIAN_POINT ( 'NONE',  ( 38.43336038379620589, 2.130196079827431532, -7.949999999999997513 ) ) ;
#138587 = DIRECTION ( 'NONE',  ( 0.000000000000000000, -1.000000000000000000, 0.000000000000000000 ) ) ;
#138588 = ADVANCED_FACE ( 'NONE', ( #12637 ), #124266, .F. ) ;
#138589 = EDGE_CURVE ( 'NONE', #86852, #111653, #24248, .T. ) ;
#138590 = CARTESIAN_POINT ( 'NONE',  ( -1.499999999999987566, 4.466399257802216027, 5.000000000000000000 ) ) ;
#138591 = ORIENTED_EDGE ( 'NONE', *, *, #31583, .T. ) ;
#138592 = VERTEX_POINT ( 'NONE', #59749 ) ;
#138593 = CARTESIAN_POINT ( 'NONE',  ( 33.22916666666665719, 7.950000000000001954, -2.130196079827421762 ) ) ;
#138594 = EDGE_CURVE ( 'NONE', #125403, #87604, #135863, .T. ) ;
#138595 = VERTEX_POINT ( 'NONE', #35146 ) ;
#138596 = CARTESIAN_POINT ( 'NONE',  ( -48.18398860626899705, 28.73617430169820608, 5.000000000000000000 ) ) ;
#138597 = EDGE_CURVE ( 'NONE', #25329, #78673, #25659, .T. ) ;
#138598 = CYLINDRICAL_SURFACE ( 'NONE', #64087, 0.5000000000000004441 ) ;
#138599 = CIRCLE ( 'NONE', #66981, 2.055000000000001048 ) ;
#138600 = ADVANCED_FACE ( 'NONE', ( #34407 ), #124977, .F. ) ;
#138601 = DIRECTION ( 'NONE',  ( -1.000000000000000000, -0.000000000000000000, -0.000000000000000000 ) ) ;
#138603 = VECTOR ( 'NONE', #11019, 1000.000000000000000 ) ;
#138602 = CARTESIAN_POINT ( 'NONE',  ( 34.49999999999976552, 22.01701374228158414, 2.453858888625551682 ) ) ;
#138604 = LINE ( 'NONE', #66054, #92936 ) ;
#138605 = CARTESIAN_POINT ( 'NONE',  ( -34.49999999999974420, -12.08601207473291161, -10.46905243149086040 ) ) ;
#138606 = EDGE_CURVE ( 'NONE', #132022, #9514, #36544, .T. ) ;
#138607 = CARTESIAN_POINT ( 'NONE',  ( 32.08376352523143993, -6.110000000000001208, -3.741295971395164515E-16 ) ) ;
#138609 = EDGE_CURVE ( 'NONE', #115069, #108682, #113371, .T. ) ;
#138608 = ORIENTED_EDGE ( 'NONE', *, *, #75384, .T. ) ;
#138610 = DIRECTION ( 'NONE',  ( 0.7071067811865486830, -0.7071067811865464625, -0.000000000000000000 ) ) ;
#138611 = ORIENTED_EDGE ( 'NONE', *, *, #90930, .T. ) ;
#138612 = CARTESIAN_POINT ( 'NONE',  ( 7.251592354503322291, 2.500000000000001332, 0.000000000000000000 ) ) ;
#138613 = CARTESIAN_POINT ( 'NONE',  ( 30.48921356237309510, -27.52281430457076894, 5.000000000000000000 ) ) ;
#138614 = CARTESIAN_POINT ( 'NONE',  ( 7.799999601179139042, 0.000000000000000000, 2.500000000000000444 ) ) ;
#138615 = EDGE_CURVE ( 'NONE', #56866, #102362, #114106, .T. ) ;
#138616 = CARTESIAN_POINT ( 'NONE',  ( 64.00000000000000000, 0.000000000000000000, -7.950000000000000178 ) ) ;
#138617 = ORIENTED_EDGE ( 'NONE', *, *, #122596, .T. ) ;
#138618 = CARTESIAN_POINT ( 'NONE',  ( 50.89626352523143993, 4.472830434245840259, -4.472830434245839371 ) ) ;
#138619 = EDGE_CURVE ( 'NONE', #12982, #59289, #4558, .T. ) ;
#138620 = ORIENTED_EDGE ( 'NONE', *, *, #114383, .T. ) ;
#138621 = LINE ( 'NONE', #59646, #40134 ) ;
#138622 = DIRECTION ( 'NONE',  ( 0.7071067811865486830, -0.7071067811865464625, -0.000000000000000000 ) ) ;
#138623 = LINE ( 'NONE', #83538, #133483 ) ;
#138624 = DIRECTION ( 'NONE',  ( -0.3543493200069162685, -0.000000000000000000, -0.9351131265310288487 ) ) ;
#138625 = EDGE_CURVE ( 'NONE', #47652, #46980, #3189, .T. ) ;
#138626 = B_SPLINE_CURVE_WITH_KNOTS ( 'NONE', 3,
 ( #97670, #78791, #77388, #100541 ),
 .UNSPECIFIED., .F., .F.,
 ( 4, 4 ),
 ( 0.000000000000000000, 0.001115544020566811706 ),
 .UNSPECIFIED. ) ;
#138627 = CARTESIAN_POINT ( 'NONE',  ( 47.89126352523143737, -4.472830434245839371, -4.472830434245839371 ) ) ;
#138628 = VERTEX_POINT ( 'NONE', #90950 ) ;
#138629 = LINE ( 'NONE', #39320, #139152 ) ;
#138630 = CARTESIAN_POINT ( 'NONE',  ( 18.32840764549667512, 3.061616997868380183E-16, -2.500000000000001332 ) ) ;
#138631 = ORIENTED_EDGE ( 'NONE', *, *, #92325, .F. ) ;
#138632 = ORIENTED_EDGE ( 'NONE', *, *, #43197, .T. ) ;
#138633 = LINE ( 'NONE', #26999, #90993 ) ;
#138634 = VERTEX_POINT ( 'NONE', #37264 ) ;
#138635 = DIRECTION ( 'NONE',  ( -0.6830127018922181881, 0.6830127018922202975, -0.2588190451025214056 ) ) ;
#138636 = VERTEX_POINT ( 'NONE', #57610 ) ;
#138637 = DIRECTION ( 'NONE',  ( 0.7071067811865486830, -0.7071067811865464625, -0.000000000000000000 ) ) ;
#138638 = ADVANCED_FACE ( 'NONE', ( #46767 ), #135178, .F. ) ;
#138639 = CARTESIAN_POINT ( 'NONE',  ( 11.99999999999991296, 4.965500833774338929, -4.007596771432684335 ) ) ;
#138640 = VECTOR ( 'NONE', #59164, 1000.000000000000000 ) ;
#138641 = AXIS2_PLACEMENT_3D ( 'NONE', #129580, #108515, #86819 ) ;
#138642 = VECTOR ( 'NONE', #118829, 1000.000000000000000 ) ;
#138643 = LINE ( 'NONE', #39336, #76685 ) ;
#138644 = VECTOR ( 'NONE', #5040, 1000.000000000000114 ) ;
#138645 = FACE_BOUND ( 'NONE', #49426, .T. ) ;
#138646 = DIRECTION ( 'NONE',  ( -1.000000000000000000, -0.000000000000000000, -0.000000000000000000 ) ) ;
#138647 = LINE ( 'NONE', #139387, #28203 ) ;
#138648 = CARTESIAN_POINT ( 'NONE',  ( 0.000000000000000000, 4.384688058510565867, -7.090945410444685848 ) ) ;
#138649 = VERTEX_POINT ( 'NONE', #102539 ) ;
#138650 = CARTESIAN_POINT ( 'NONE',  ( 12.18398860626900060, 28.73617430169795739, 5.000000000000000000 ) ) ;
#138652 = EDGE_LOOP ( 'NONE', ( #106770, #114757, #27853, #5330 ) ) ;
#138651 = LINE ( 'NONE', #136485, #87515 ) ;
#138653 = ORIENTED_EDGE ( 'NONE', *, *, #95309, .T. ) ;
#138654 = AXIS2_PLACEMENT_3D ( 'NONE', #94782, #37589, #40453 ) ;
#138655 = AXIS2_PLACEMENT_3D ( 'NONE', #127105, #7455, #117632 ) ;
#138656 = CARTESIAN_POINT ( 'NONE',  ( 26.99999999999981526, 9.631307414974347836, -9.079085613539479738 ) ) ;
#138657 = EDGE_CURVE ( 'NONE', #63684, #89873, #91641, .T. ) ;
#138658 = ORIENTED_EDGE ( 'NONE', *, *, #47925, .F. ) ;
#138659 = ORIENTED_EDGE ( 'NONE', *, *, #95539, .T. ) ;
#138660 = CARTESIAN_POINT ( 'NONE',  ( 63.64126352523144448, 4.472830434245835818, 4.472830434245840259 ) ) ;
#138661 = ORIENTED_EDGE ( 'NONE', *, *, #43953, .T. ) ;
#138662 = DIRECTION ( 'NONE',  ( 0.000000000000000000, 0.000000000000000000, 1.000000000000000000 ) ) ;
#138663 = DIRECTION ( 'NONE',  ( 0.7071067811865487940, 0.7071067811865463515, -0.000000000000000000 ) ) ;
#138664 = EDGE_CURVE ( 'NONE', #13692, #105661, #59062, .T. ) ;
#138665 = ORIENTED_EDGE ( 'NONE', *, *, #13916, .F. ) ;
#138666 = DIRECTION ( 'NONE',  ( 0.7071067811865487940, 0.7071067811865463515, -0.000000000000000000 ) ) ;
#138667 = VECTOR ( 'NONE', #115139, 1000.000000000000114 ) ;
#138668 = AXIS2_PLACEMENT_3D ( 'NONE', #138933, #138208, #83116 ) ;
#138669 = CARTESIAN_POINT ( 'NONE',  ( 35.41666666666666430, -6.884901960086287076, -3.975000000000000977 ) ) ;
#138670 = EDGE_CURVE ( 'NONE', #99164, #36084, #103215, .T. ) ;
#138671 = CARTESIAN_POINT ( 'NONE',  ( 44.99451991528749772, 28.92564299267969474, 4.000000000000000000 ) ) ;
#138672 = DIRECTION ( 'NONE',  ( 0.7071067811865487940, 0.7071067811865463515, 0.000000000000000000 ) ) ;
#138673 = PLANE ( 'NONE',  #135018 ) ;
#138674 = FACE_OUTER_BOUND ( 'NONE', #115955, .T. ) ;
#138675 = ORIENTED_EDGE ( 'NONE', *, *, #66744, .F. ) ;
#138676 = AXIS2_PLACEMENT_3D ( 'NONE', #16765, #104478, #6550 ) ;
#138677 = EDGE_LOOP ( 'NONE', ( #86480, #19195, #103708, #45758 ) ) ;
#138678 = AXIS2_PLACEMENT_3D ( 'NONE', #97568, #110567, #10547 ) ;
#138679 = CARTESIAN_POINT ( 'NONE',  ( -34.49999999999975131, 1.087461875839228931, 4.000000000000000000 ) ) ;
#138680 = CARTESIAN_POINT ( 'NONE',  ( 184.1500000000000057, -57.15000000000003411, 15.92499999999935589 ) ) ;
#138681 = ORIENTED_EDGE ( 'NONE', *, *, #49954, .F. ) ;
#138682 = AXIS2_PLACEMENT_3D ( 'NONE', #118734, #86122, #28887 ) ;
#138683 = ORIENTED_EDGE ( 'NONE', *, *, #48536, .F. ) ;
#138684 = VECTOR ( 'NONE', #64356, 1000.000000000000000 ) ;
#138685 = ORIENTED_EDGE ( 'NONE', *, *, #128341, .T. ) ;
#138686 = DIRECTION ( 'NONE',  ( -0.7071067811865487940, 0.7071067811865463515, 0.000000000000000000 ) ) ;
#138687 = CARTESIAN_POINT ( 'NONE',  ( 45.48921356237309510, -27.52281430457087197, 5.000000000000000000 ) ) ;
#138688 = EDGE_CURVE ( 'NONE', #62399, #103400, #48146, .T. ) ;
#138689 = CARTESIAN_POINT ( 'NONE',  ( 29.87500000000000000, 7.950000000000000178, 1.460391307983218535E-15 ) ) ;
#138690 = ORIENTED_EDGE ( 'NONE', *, *, #69978, .T. ) ;
#138691 = AXIS2_PLACEMENT_3D ( 'NONE', #2103, #69583, #113766 ) ;
#138692 = CARTESIAN_POINT ( 'NONE',  ( -8.282422613574265569, -21.73023691814493219, 5.000000000000000888 ) ) ;
#138693 = VECTOR ( 'NONE', #45456, 1000.000000000000000 ) ;
#138694 = FACE_OUTER_BOUND ( 'NONE', #107235, .T. ) ;
#138695 = CARTESIAN_POINT ( 'NONE',  ( 9.983736474768551972, -5.808823158059035485, -5.808823158059033709 ) ) ;
#138696 = DIRECTION ( 'NONE',  ( 0.6830127018922180770, -0.6830127018922204085, -0.2588190451025213501 ) ) ;
#138697 = VERTEX_POINT ( 'NONE', #61211 ) ;
#138698 = LINE ( 'NONE', #116919, #84557 ) ;
#138699 = CYLINDRICAL_SURFACE ( 'NONE', #51194, 2.500000000000000444 ) ;
#138700 = LINE ( 'NONE', #81477, #84556 ) ;
#138701 = CONICAL_SURFACE ( 'NONE', #134148, 2.500000000000000888, 0.9599310885968822538 ) ;
#138703 = ORIENTED_EDGE ( 'NONE', *, *, #23051, .T. ) ;
#138702 = CARTESIAN_POINT ( 'NONE',  ( -51.48921356237309510, -27.52281430457091460, 5.000000000000000000 ) ) ;
#138704 = DIRECTION ( 'NONE',  ( 0.6830127018922181881, 0.6830127018922202975, -0.2588190451025214056 ) ) ;
#138705 = ORIENTED_EDGE ( 'NONE', *, *, #128746, .T. ) ;
#138706 = DIRECTION ( 'NONE',  ( 0.6830127018922180770, -0.6830127018922204085, -0.2588190451025213501 ) ) ;
#138707 = CARTESIAN_POINT ( 'NONE',  ( 3.250000000000000000, 0.000000000000000000, 0.000000000000000000 ) ) ;
#138708 = FACE_OUTER_BOUND ( 'NONE', #103594, .T. ) ;
#138709 = ORIENTED_EDGE ( 'NONE', *, *, #101268, .F. ) ;
#138710 = EDGE_CURVE ( 'NONE', #34731, #115267, #51721, .T. ) ;
#138711 = LINE ( 'NONE', #39395, #142218 ) ;
#138712 = DIRECTION ( 'NONE',  ( -1.000000000000000000, -0.000000000000000000, -0.000000000000000000 ) ) ;
#138713 = CARTESIAN_POINT ( 'NONE',  ( -17.81601139373099940, 28.73617430169775133, 5.000000000000000000 ) ) ;
#138714 = ORIENTED_EDGE ( 'NONE', *, *, #126130, .T. ) ;
#138715 = DIRECTION ( 'NONE',  ( 1.000000000000000000, 0.000000000000000000, 0.000000000000000000 ) ) ;
#138716 = DIRECTION ( 'NONE',  ( 0.7071067811865487940, 0.7071067811865463515, 0.000000000000000000 ) ) ;
#138717 = DIRECTION ( 'NONE',  ( 0.000000000000000000, -1.000000000000000000, 0.000000000000000000 ) ) ;
#138718 = LINE ( 'NONE', #51711, #86509 ) ;
#138719 = ORIENTED_EDGE ( 'NONE', *, *, #58095, .F. ) ;
#138720 = EDGE_CURVE ( 'NONE', #14551, #24719, #104646, .T. ) ;
#138721 = VERTEX_POINT ( 'NONE', #138008 ) ;
#138722 = CARTESIAN_POINT ( 'NONE',  ( -25.49999999999982236, 6.431123077392117082, 4.000000000000000000 ) ) ;
#138723 =( BOUNDED_CURVE ( )  B_SPLINE_CURVE ( 3, ( #22748, #33693, #40461, #19392 ),
 .UNSPECIFIED., .F., .T. ) 
 B_SPLINE_CURVE_WITH_KNOTS ( ( 4, 4 ),
 ( 1.208578181583236821, 1.359146454359482892 ),
 .UNSPECIFIED. ) 
 CURVE ( )  GEOMETRIC_REPRESENTATION_ITEM ( )  RATIONAL_B_SPLINE_CURVE ( ( 1.000000000000000000, 0.9981116584018941973, 0.9981116584018941973, 1.000000000000000000 ) ) 
 REPRESENTATION_ITEM ( '' )  );
#138724 = CARTESIAN_POINT ( 'NONE',  ( 5.957903141435219929, 6.871911579029515771, 3.967499999999989146 ) ) ;
#138725 = CARTESIAN_POINT ( 'NONE',  ( 0.000000000000000000, 0.000000000000000000, 5.000000000000000000 ) ) ;
#138726 = CARTESIAN_POINT ( 'NONE',  ( 57.48921356237308800, -27.52281430457095368, 5.000000000000000000 ) ) ;
#138727 = CARTESIAN_POINT ( 'NONE',  ( -19.49999999999985789, -17.56887692260763245, 4.000000000000000000 ) ) ;
#138728 = DIRECTION ( 'NONE',  ( 0.7071067811865487940, -0.7071067811865463515, 0.000000000000000000 ) ) ;
#138729 = VERTEX_POINT ( 'NONE', #50290 ) ;
#138730 = DIRECTION ( 'NONE',  ( -0.7071067811865486830, -0.7071067811865464625, 0.000000000000000000 ) ) ;
#138731 = DIRECTION ( 'NONE',  ( -1.000000000000000000, -1.224606353822377258E-16, -0.000000000000000000 ) ) ;
#138732 = DIRECTION ( 'NONE',  ( 0.6830127018922181881, 0.6830127018922202975, -0.2588190451025214056 ) ) ;
#138733 = CARTESIAN_POINT ( 'NONE',  ( 0.1839886062690032631, 28.73617430169787568, 5.000000000000000000 ) ) ;
#138734 = CARTESIAN_POINT ( 'NONE',  ( 43.80793019189810877, -6.109999999999999432, 1.637169565754158507 ) ) ;
#138735 = CARTESIAN_POINT ( 'NONE',  ( 183.8105469881216436, -51.90335959434332125, -39.28179725402795697 ) ) ;
#138736 = ORIENTED_EDGE ( 'NONE', *, *, #80508, .T. ) ;
#138737 = CARTESIAN_POINT ( 'NONE',  ( 31.43336038379622366, 2.130196079827431532, -7.949999999999996625 ) ) ;
#138738 = ORIENTED_EDGE ( 'NONE', *, *, #46623, .F. ) ;
#138739 = ORIENTED_EDGE ( 'NONE', *, *, #84611, .T. ) ;
#138740 = CARTESIAN_POINT ( 'NONE',  ( -9.005480084712511157, 28.92564299267931816, 4.000000000000000000 ) ) ;
#138741 = VECTOR ( 'NONE', #49360, 1000.000000000000000 ) ;
#138742 = VECTOR ( 'NONE', #125714, 1000.000000000000000 ) ;
#138743 = VECTOR ( 'NONE', #117015, 1000.000000000000000 ) ;
#138744 = CARTESIAN_POINT ( 'NONE',  ( 184.1500000000000057, -30.18000000000009564, 12.69999999999954454 ) ) ;
#138746 = EDGE_CURVE ( 'NONE', #27605, #63895, #115485, .T. ) ;
#138745 = DIRECTION ( 'NONE',  ( 0.7071067811865486830, -0.7071067811865464625, -0.000000000000000000 ) ) ;
#138747 = AXIS2_PLACEMENT_3D ( 'NONE', #60024, #15055, #27353 ) ;
#138748 = PLANE ( 'NONE',  #62536 ) ;
#138749 = CARTESIAN_POINT ( 'NONE',  ( 22.25000000000000000, 0.000000000000000000, 0.000000000000000000 ) ) ;
#138750 = DIRECTION ( 'NONE',  ( -0.6830127018922181881, 0.6830127018922202975, -0.2588190451025214056 ) ) ;
#138751 = ORIENTED_EDGE ( 'NONE', *, *, #102476, .T. ) ;
#138752 = CARTESIAN_POINT ( 'NONE',  ( 13.17183060077638501, 12.75929247661559351, 4.000000000000000000 ) ) ;
#138753 = PLANE ( 'NONE',  #116263 ) ;
#138754 = UNCERTAINTY_MEASURE_WITH_UNIT (LENGTH_MEASURE( 1.000000000000000082E-05 ), #36118, 'distance_accuracy_value', 'NONE');
#138755 = AXIS2_PLACEMENT_3D ( 'NONE', #10155, #118918, #9407 ) ;
#138756 = FACE_OUTER_BOUND ( 'NONE', #87090, .T. ) ;
#138757 = DIRECTION ( 'NONE',  ( -0.7071067811865486830, -0.7071067811865464625, 0.000000000000000000 ) ) ;
#138758 = LINE ( 'NONE', #29258, #59685 ) ;
#138759 = CARTESIAN_POINT ( 'NONE',  ( 65.85002705046288440, -5.819803920172572198, -5.819803920172572198 ) ) ;
#138760 = ADVANCED_FACE ( 'NONE', ( #62591 ), #63331, .F. ) ;
#138761 = CARTESIAN_POINT ( 'NONE',  ( 19.37176554955603436, -8.240707523384200428, 11.38925528200748083 ) ) ;
#138762 = ORIENTED_EDGE ( 'NONE', *, *, #13588, .T. ) ;
#138763 = ORIENTED_EDGE ( 'NONE', *, *, #86269, .T. ) ;
#138764 = CARTESIAN_POINT ( 'NONE',  ( 62.54166666666666430, -3.975000000000002753, 6.884901960086286188 ) ) ;
#138765 = DIRECTION ( 'NONE',  ( 1.000000000000000000, 3.115803279706882722E-16, -0.000000000000000000 ) ) ;
#138766 = EDGE_CURVE ( 'NONE', #22463, #94800, #73468, .T. ) ;
#138767 = PLANE ( 'NONE',  #129544 ) ;
#138768 = EDGE_CURVE ( 'NONE', #113921, #53394, #49599, .T. ) ;
#138769 = STYLED_ITEM ( 'NONE', ( #107147 ), #47523 ) ;
#138770 = VECTOR ( 'NONE', #85907, 1000.000000000000000 ) ;
#138771 = EDGE_LOOP ( 'NONE', ( #111024, #27494, #120663, #39523 ) ) ;
#138772 = ADVANCED_FACE ( 'NONE', ( #52402 ), #137299, .T. ) ;
#138773 = DIRECTION ( 'NONE',  ( -0.6830127018922180770, -0.6830127018922204085, -0.2588190451025213501 ) ) ;
#138774 = VECTOR ( 'NONE', #83505, 1000.000000000000000 ) ;
#138775 = CARTESIAN_POINT ( 'NONE',  ( -25.39999999999996305, 0.000000000000000000, 0.000000000000000000 ) ) ;
#138776 = CARTESIAN_POINT ( 'NONE',  ( 55.70876352523143282, -7.482591942790329030E-16, 6.110000000000001208 ) ) ;
#138777 = DIRECTION ( 'NONE',  ( -0.6830127018922180770, -0.6830127018922204085, -0.2588190451025213501 ) ) ;
#138778 = ORIENTED_EDGE ( 'NONE', *, *, #104009, .T. ) ;
#138779 = ORIENTED_EDGE ( 'NONE', *, *, #114842, .T. ) ;
#138780 = DIRECTION ( 'NONE',  ( 0.000000000000000000, 1.000000000000000000, 0.000000000000000000 ) ) ;
#138781 = VECTOR ( 'NONE', #118990, 1000.000000000000000 ) ;
#138782 = AXIS2_PLACEMENT_3D ( 'NONE', #1744, #38015, #48161 ) ;
#138783 = DIRECTION ( 'NONE',  ( 0.000000000000000000, 0.3543493200069153248, 0.9351131265310291818 ) ) ;
#138784 = PLANE ( 'NONE',  #53578 ) ;
#138785 = VECTOR ( 'NONE', #139994, 1000.000000000000000 ) ;
#138786 = EDGE_CURVE ( 'NONE', #75123, #64810, #18317, .T. ) ;
#138787 = DIRECTION ( 'NONE',  ( 0.7071067811865487940, -0.7071067811865463515, 0.000000000000000000 ) ) ;
#138788 = EDGE_CURVE ( 'NONE', #69645, #66281, #84365, .T. ) ;
#138789 = CARTESIAN_POINT ( 'NONE',  ( 13.49999999999990763, 19.46639925780206326, 5.000000000000000000 ) ) ;
#138791 = EDGE_LOOP ( 'NONE', ( #30100, #58947, #99065, #103488 ) ) ;
#138790 = DIRECTION ( 'NONE',  ( -0.000000000000000000, 0.000000000000000000, 1.000000000000000000 ) ) ;
#138792 = VECTOR ( 'NONE', #117529, 1000.000000000000000 ) ;
#138793 = LINE ( 'NONE', #39480, #87753 ) ;
#138794 = DIRECTION ( 'NONE',  ( 0.7071067811865487940, -0.7071067811865463515, 0.000000000000000000 ) ) ;
#138795 = CARTESIAN_POINT ( 'NONE',  ( -5.999999999999952927, 2.587461875839218273, 4.000000000000000000 ) ) ;
#138796 = CIRCLE ( 'NONE', #131851, 2.500000000000000444 ) ;
#138797 = DIRECTION ( 'NONE',  ( -0.3543493200069162685, -0.000000000000000000, -0.9351131265310288487 ) ) ;
#138798 = VECTOR ( 'NONE', #87359, 1000.000000000000000 ) ;
#138799 = EDGE_CURVE ( 'NONE', #54517, #137275, #27087, .T. ) ;
#138800 = ORIENTED_EDGE ( 'NONE', *, *, #110418, .T. ) ;
#138801 = ORIENTED_EDGE ( 'NONE', *, *, #81092, .F. ) ;
#138802 = DIRECTION ( 'NONE',  ( -0.7071067811865487940, 0.7071067811865463515, 0.000000000000000000 ) ) ;
#138803 = DIRECTION ( 'NONE',  ( -0.7071067811865486830, -0.7071067811865464625, 0.000000000000000000 ) ) ;
#138804 = CARTESIAN_POINT ( 'NONE',  ( 41.99451991528749062, 28.92564299267967343, 4.000000000000000000 ) ) ;
#138805 = CYLINDRICAL_SURFACE ( 'NONE', #57146, 2.500000000000000444 ) ;
#138806 = LINE ( 'NONE', #117026, #54835 ) ;
#138807 = VERTEX_POINT ( 'NONE', #106776 ) ;
#138809 = EDGE_CURVE ( 'NONE', #130071, #9641, #94477, .T. ) ;
#138808 = ORIENTED_EDGE ( 'NONE', *, *, #55110, .F. ) ;
#138810 = DIRECTION ( 'NONE',  ( 0.7071067811865487940, 0.7071067811865463515, 0.000000000000000000 ) ) ;
#138811 = LINE ( 'NONE', #27163, #139382 ) ;
#138812 = ORIENTED_EDGE ( 'NONE', *, *, #108773, .F. ) ;
#138813 = ORIENTED_EDGE ( 'NONE', *, *, #66637, .T. ) ;
#138814 = CARTESIAN_POINT ( 'NONE',  ( -20.39513766812466855, 21.75929247661549937, 21.32995629748191035 ) ) ;
#138815 = VERTEX_POINT ( 'NONE', #50999 ) ;
#138816 = CARTESIAN_POINT ( 'NONE',  ( 31.49999999999978684, -1.912538124160739095, 4.000000000000000000 ) ) ;
#138817 = EDGE_CURVE ( 'NONE', #75424, #65015, #72071, .T. ) ;
#138818 = CARTESIAN_POINT ( 'NONE',  ( -29.84387692260737879, -22.22500000000000142, 4.000000000000000000 ) ) ;
#138819 = FACE_BOUND ( 'NONE', #102610, .T. ) ;
#138820 = DIRECTION ( 'NONE',  ( -0.6830127018922181881, 0.6830127018922202975, -0.2588190451025214056 ) ) ;
#138821 = DIRECTION ( 'NONE',  ( 0.6830127018922180770, -0.6830127018922204085, -0.2588190451025214056 ) ) ;
#138823 = ORIENTED_EDGE ( 'NONE', *, *, #106150, .T. ) ;
#138822 = DIRECTION ( 'NONE',  ( 0.3543493200069162685, -0.000000000000000000, -0.9351131265310288487 ) ) ;
#138824 = DIRECTION ( 'NONE',  ( -1.000000000000000000, -0.000000000000000000, -0.000000000000000000 ) ) ;
#138826 = EDGE_CURVE ( 'NONE', #109128, #14910, #71328, .T. ) ;
#138825 = SHAPE_DEFINITION_REPRESENTATION ( #34012, #39429 ) ;
#138827 = ORIENTED_EDGE ( 'NONE', *, *, #49249, .F. ) ;
#138828 = ORIENTED_EDGE ( 'NONE', *, *, #72524, .T. ) ;
#138829 = CARTESIAN_POINT ( 'NONE',  ( 92.07876352523145158, -7.482591942790325086E-16, 6.109999999999998543 ) ) ;
#138830 = VERTEX_POINT ( 'NONE', #85038 ) ;
#138831 = CARTESIAN_POINT ( 'NONE',  ( 34.92499999999998295, 22.22500000000000142, 4.500000000000000888 ) ) ;
#138832 = LINE ( 'NONE', #114884, #81788 ) ;
#138833 = DIRECTION ( 'NONE',  ( -0.7071067811865487940, 0.7071067811865463515, 0.000000000000000000 ) ) ;
#138834 = CARTESIAN_POINT ( 'NONE',  ( -29.99451991528749417, 28.92564299267958816, 4.000000000000000000 ) ) ;
#138835 = VERTEX_POINT ( 'NONE', #138727 ) ;
#138836 = CARTESIAN_POINT ( 'NONE',  ( 11.99999999999991296, 16.55218569542899587, 5.000000000000000000 ) ) ;
#138837 = DIRECTION ( 'NONE',  ( -0.7071067811865487940, 0.7071067811865463515, -0.000000000000000000 ) ) ;
#138838 = EDGE_CURVE ( 'NONE', #50212, #64365, #24580, .T. ) ;
#138839 = FACE_OUTER_BOUND ( 'NONE', #75016, .T. ) ;
#138841 = LINE ( 'NONE', #94589, #100603 ) ;
#138840 = CARTESIAN_POINT ( 'NONE',  ( -31.49999999999977973, 10.46639925780216096, 5.000000000000000000 ) ) ;
#138842 = FACE_OUTER_BOUND ( 'NONE', #68912, .T. ) ;
#138843 = FACE_OUTER_BOUND ( 'NONE', #64137, .T. ) ;
#138844 = PRESENTATION_LAYER_ASSIGNMENT (  '', '', ( #32250 ) ) ;
#138845 = VECTOR ( 'NONE', #12453, 1000.000000000000227 ) ;
#138846 = CARTESIAN_POINT ( 'NONE',  ( 15.55937119539439806, -22.22500000000000142, 24.13041545083173034 ) ) ;
#138847 = VECTOR ( 'NONE', #25556, 1000.000000000000000 ) ;
#138848 = VERTEX_POINT ( 'NONE', #39417 ) ;
#138849 = DIRECTION ( 'NONE',  ( 0.6830127018922180770, -0.6830127018922204085, -0.2588190451025213501 ) ) ;
#138850 = CARTESIAN_POINT ( 'NONE',  ( -25.49999999999982236, 15.05218569542901896, 5.000000000000000000 ) ) ;
#138851 = VECTOR ( 'NONE', #116899, 1000.000000000000000 ) ;
#138852 = VERTEX_POINT ( 'NONE', #28540 ) ;
#138853 = VERTEX_POINT ( 'NONE', #72798 ) ;
#138854 = EDGE_CURVE ( 'NONE', #48007, #64418, #116952, .T. ) ;
#138855 = VERTEX_POINT ( 'NONE', #106048 ) ;
#138856 = CARTESIAN_POINT ( 'NONE',  ( 40.68793019189811133, 6.110000000000002984, -1.637169565754156730 ) ) ;
#138857 = ORIENTED_EDGE ( 'NONE', *, *, #48087, .F. ) ;
#138858 = PRESENTATION_LAYER_ASSIGNMENT (  '', '', ( #57851 ) ) ;
#138859 = VECTOR ( 'NONE', #137649, 999.9999999999998863 ) ;
#138860 = CARTESIAN_POINT ( 'NONE',  ( 20.17080628287043709, -3.047499999999997211, -5.278424836066143655 ) ) ;
#138861 = CARTESIAN_POINT ( 'NONE',  ( -6.325809920431304967, 11.42897679595730231, -27.74950860237164818 ) ) ;
#138862 = EDGE_LOOP ( 'NONE', ( #87743, #60487, #99979, #7231 ) ) ;
#138863 = PLANE ( 'NONE',  #112906 ) ;
#138864 = ORIENTED_EDGE ( 'NONE', *, *, #80488, .T. ) ;
#138865 = CARTESIAN_POINT ( 'NONE',  ( -12.18398860626900060, 28.73617430169795739, 5.000000000000000000 ) ) ;
#138866 = CONICAL_SURFACE ( 'NONE', #83288, 2.500000000000000444, 0.9599310885968830309 ) ;
#138867 = CARTESIAN_POINT ( 'NONE',  ( 9.328169399223460445, 17.25929247661554911, 4.000000000000000000 ) ) ;
#138869 = ORIENTED_EDGE ( 'NONE', *, *, #141052, .T. ) ;
#138868 = PLANE ( 'NONE',  #47117 ) ;
#138870 = EDGE_LOOP ( 'NONE', ( #84367, #7620, #10937, #81634 ) ) ;
#138871 = CARTESIAN_POINT ( 'NONE',  ( 3.000000000000000000, -43.14999999999999147, 31.92499999999998295 ) ) ;
#138872 = CARTESIAN_POINT ( 'NONE',  ( 1.827855086967997700, 4.202752102959690472E-16, 0.000000000000000000 ) ) ;
#138873 = ORIENTED_EDGE ( 'NONE', *, *, #105393, .F. ) ;
#138874 = VECTOR ( 'NONE', #6233, 1000.000000000000114 ) ;
#138875 = CARTESIAN_POINT ( 'NONE',  ( 21.18398860626899349, 28.73617430169802134, 5.000000000000000000 ) ) ;
#138876 = VERTEX_POINT ( 'NONE', #6715 ) ;
#138878 = VERTEX_POINT ( 'NONE', #32091 ) ;
#138877 = EDGE_CURVE ( 'NONE', #66944, #116320, #95193, .T. ) ;
#138879 = ORIENTED_EDGE ( 'NONE', *, *, #99089, .F. ) ;
#138880 = ORIENTED_EDGE ( 'NONE', *, *, #25789, .T. ) ;
#138881 = DIRECTION ( 'NONE',  ( -0.000000000000000000, 0.3543493200069153248, 0.9351131265310292928 ) ) ;
#138882 = VECTOR ( 'NONE', #58410, 999.9999999999998863 ) ;
#138883 = VECTOR ( 'NONE', #38543, 1000.000000000000000 ) ;
#138884 = DIRECTION ( 'NONE',  ( -0.000000000000000000, 0.000000000000000000, 1.000000000000000000 ) ) ;
#138885 = VECTOR ( 'NONE', #131066, 1000.000000000000227 ) ;
#138887 = EDGE_CURVE ( 'NONE', #15770, #59525, #76319, .T. ) ;
#138886 = DIRECTION ( 'NONE',  ( 0.7071067811865486830, -0.7071067811865464625, -0.000000000000000000 ) ) ;
#138888 = DIRECTION ( 'NONE',  ( -0.000000000000000000, 0.3543493200069153248, 0.9351131265310292928 ) ) ;
#138889 = ORIENTED_EDGE ( 'NONE', *, *, #24165, .F. ) ;
#138890 = VECTOR ( 'NONE', #47940, 999.9999999999998863 ) ;
#138891 = EDGE_CURVE ( 'NONE', #38043, #124291, #130718, .T. ) ;
#138892 = DIRECTION ( 'NONE',  ( -0.6830127018922180770, -0.6830127018922204085, -0.2588190451025213501 ) ) ;
#138893 = ORIENTED_EDGE ( 'NONE', *, *, #129002, .T. ) ;
#138894 = AXIS2_PLACEMENT_3D ( 'NONE', #104689, #48179, #15503 ) ;
#138895 = CARTESIAN_POINT ( 'NONE',  ( 15.79289321881335084, -17.24070752338411339, 5.000000000000000000 ) ) ;
#138896 = CARTESIAN_POINT ( 'NONE',  ( 31.77040314143522082, -7.934999999999989839, 2.126176841940957907 ) ) ;
#138897 = CARTESIAN_POINT ( 'NONE',  ( -19.05000000000000071, 3.174999999999997158, 4.000000000000000000 ) ) ;
#138898 = CARTESIAN_POINT ( 'NONE',  ( 95.50000000000000000, 0.000000000000000000, -7.950000000000000178 ) ) ;
#138899 = DIRECTION ( 'NONE',  ( 0.7071067811865487940, -0.7071067811865463515, 0.000000000000000000 ) ) ;
#138900 = VERTEX_POINT ( 'NONE', #33550 ) ;
#138901 = ORIENTED_EDGE ( 'NONE', *, *, #119882, .F. ) ;
#138902 = ORIENTED_EDGE ( 'NONE', *, *, #2345, .F. ) ;
#138903 = LINE ( 'NONE', #29398, #83413 ) ;
#138904 = LINE ( 'NONE', #51897, #104345 ) ;
#138905 = CARTESIAN_POINT ( 'NONE',  ( 7.940000000000001279, -60.26999999999998892, -10.00000000000000178 ) ) ;
#138906 = DIRECTION ( 'NONE',  ( -1.000000000000000000, -0.000000000000000000, -0.000000000000000000 ) ) ;
#138907 = CARTESIAN_POINT ( 'NONE',  ( 3.483440076893626003, -49.11775834062216006, -40.20665288735838061 ) ) ;
#138908 = CARTESIAN_POINT ( 'NONE',  ( 76.32876352523145158, 0.000000000000000000, -6.109999999999999432 ) ) ;
#138909 = EDGE_CURVE ( 'NONE', #32788, #68309, #55283, .T. ) ;
#138910 = DIRECTION ( 'NONE',  ( -0.3543493200069162685, -0.000000000000000000, -0.9351131265310288487 ) ) ;
#138911 = DIRECTION ( 'NONE',  ( -0.000000000000000000, 0.3543493200069153248, 0.9351131265310292928 ) ) ;
#138912 = DIRECTION ( 'NONE',  ( -1.000000000000000000, -1.369518533665900312E-16, 0.000000000000000000 ) ) ;
#138913 = CARTESIAN_POINT ( 'NONE',  ( 8.999999999999932498, -16.02097659208071079, -11.96015758381210858 ) ) ;
#138914 = CARTESIAN_POINT ( 'NONE',  ( 20.67183060077632817, 11.25929247661560950, 4.000000000000000000 ) ) ;
#138915 = ORIENTED_EDGE ( 'NONE', *, *, #3760, .T. ) ;
#138916 = AXIS2_PLACEMENT_3D ( 'NONE', #72757, #116911, #94437 ) ;
#138917 = LINE ( 'NONE', #39615, #142514 ) ;
#138918 = ORIENTED_EDGE ( 'NONE', *, *, #7640, .T. ) ;
#138919 = DIRECTION ( 'NONE',  ( -0.7071067811865486830, -0.7071067811865464625, 0.000000000000000000 ) ) ;
#138921 = ORIENTED_EDGE ( 'NONE', *, *, #64017, .F. ) ;
#138920 = CARTESIAN_POINT ( 'NONE',  ( 34.49999999999975842, -16.53574439159934073, 4.994342998332164107 ) ) ;
#138922 = LINE ( 'NONE', #51198, #127410 ) ;
#138923 = CARTESIAN_POINT ( 'NONE',  ( -18.41161490594819128, 22.22500000000000497, 4.777194822843813249 ) ) ;
#138924 = ORIENTED_EDGE ( 'NONE', *, *, #83151, .T. ) ;
#138925 = EDGE_LOOP ( 'NONE', ( #16410, #74724, #127372, #35370 ) ) ;
#138926 = LINE ( 'NONE', #39627, #67500 ) ;
#138927 = CARTESIAN_POINT ( 'NONE',  ( 6.792893218813413014, -11.24070752338416668, 5.000000000000000000 ) ) ;
#138928 = CLOSED_SHELL ( 'NONE', ( #85908, #87219, #124334, #137367, #142677, #4446, #17831, #78953, #65850, #61288, #19000, #86701, #100539, #58688, #141866, #22071, #13097, #94684, #92682, #29445, #123605, #124041, #94396, #31608, #75928, #111728, #89958, #90577, #38755, #2275, #49831, #62442, #67274, #56047, #25138, #7080, #24951, #137273, #121572, #56986, #109933, #2957, #96325, #45085, #143442, #133411, #60067, #81849, #23415, #56976, #64122, #75942, #32378, #46297, #109292, #4835, #113684, #24776, #128267, #73004, #61469, #71541, #20896, #133140, #29561, #42337, #94385, #85360, #112298, #97082, #132196, #138452, #14749, #132396, #142841, #55171, #31085, #112888, #23266, #119162, #69094, #5358, #107662, #41295, #33562, #45052 ) ) ;
#138929 = LINE ( 'NONE', #119285, #19511 ) ;
#138930 = CARTESIAN_POINT ( 'NONE',  ( 89.91252705046289861, -7.949999999999998401, -4.867971026610728450E-16 ) ) ;
#138931 = DIRECTION ( 'NONE',  ( 0.7071067811865487940, 0.7071067811865463515, 0.000000000000000000 ) ) ;
#138932 = EDGE_CURVE ( 'NONE', #12211, #126178, #97306, .T. ) ;
#138933 = CARTESIAN_POINT ( 'NONE',  ( 25.39999999999999858, -43.14999999999999147, -40.92499999999998295 ) ) ;
#138934 = ORIENTED_EDGE ( 'NONE', *, *, #29931, .F. ) ;
#138935 = DIRECTION ( 'NONE',  ( -1.000000000000000000, -0.000000000000000000, -0.000000000000000000 ) ) ;
#138936 = ADVANCED_FACE ( 'NONE', ( #98067 ), #86487, .F. ) ;
#138937 = DIRECTION ( 'NONE',  ( 0.6830127018922181881, 0.6830127018922202975, -0.2588190451025214056 ) ) ;
#138938 = CARTESIAN_POINT ( 'NONE',  ( 19.83333333333333570, 5.278424836066143655, -3.047499999999997655 ) ) ;
#138939 = DIRECTION ( 'NONE',  ( 0.7071067811865487940, 0.7071067811865463515, 0.000000000000000000 ) ) ;
#138940 = EDGE_LOOP ( 'NONE', ( #123772, #121918, #33148 ) ) ;
#138941 = EDGE_CURVE ( 'NONE', #69925, #15594, #109645, .T. ) ;
#138942 = EDGE_CURVE ( 'NONE', #23069, #58856, #8843, .T. ) ;
#138943 = DIRECTION ( 'NONE',  ( -0.6830127018922180770, -0.6830127018922204085, -0.2588190451025213501 ) ) ;
#138944 = ORIENTED_EDGE ( 'NONE', *, *, #140564, .F. ) ;
#138945 = VECTOR ( 'NONE', #109257, 999.9999999999998863 ) ;
#138946 = CARTESIAN_POINT ( 'NONE',  ( 85.02126352523144703, -4.472830434245839371, -4.472830434245840259 ) ) ;
#138947 = FACE_OUTER_BOUND ( 'NONE', #116023, .T. ) ;
#138948 = LINE ( 'NONE', #138222, #88648 ) ;
#138949 = CARTESIAN_POINT ( 'NONE',  ( -7.499999999999951150, 0.4311230773921780335, 4.000000000000000000 ) ) ;
#138950 = VERTEX_POINT ( 'NONE', #88629 ) ;
#138951 = VECTOR ( 'NONE', #99415, 1000.000000000000000 ) ;
#138952 = VECTOR ( 'NONE', #61023, 1000.000000000000000 ) ;
#138953 = VECTOR ( 'NONE', #87700, 1000.000000000000000 ) ;
#138954 = DIRECTION ( 'NONE',  ( -0.000000000000000000, -0.3543493200069152693, 0.9351131265310292928 ) ) ;
#138955 =( BOUNDED_CURVE ( )  B_SPLINE_CURVE ( 3, ( #67820, #92354, #137326, #59083 ),
 .UNSPECIFIED., .F., .T. ) 
 B_SPLINE_CURVE_WITH_KNOTS ( ( 4, 4 ),
 ( 5.005968288816728951, 5.074607125596323876 ),
 .UNSPECIFIED. ) 
 CURVE ( )  GEOMETRIC_REPRESENTATION_ITEM ( )  RATIONAL_B_SPLINE_CURVE ( ( 1.000000000000000000, 0.9996074310407766506, 0.9996074310407766506, 1.000000000000000000 ) ) 
 REPRESENTATION_ITEM ( '' )  );
#138956 = DIRECTION ( 'NONE',  ( -0.000000000000000000, -0.3543493200069152693, 0.9351131265310292928 ) ) ;
#138957 = EDGE_CURVE ( 'NONE', #94195, #90453, #25305, .T. ) ;
#138958 = CARTESIAN_POINT ( 'NONE',  ( 33.70710678118631165, 8.259292476615639700, 5.000000000000000000 ) ) ;
#138959 = ADVANCED_FACE ( 'NONE', ( #44428 ), #75606, .F. ) ;
#138961 = VERTEX_POINT ( 'NONE', #108902 ) ;
#138960 = DIRECTION ( 'NONE',  ( 0.5735764363510451602, 0.8191520442889924647, 0.000000000000000000 ) ) ;
#138962 = LINE ( 'NONE', #104138, #76171 ) ;
#138963 = CARTESIAN_POINT ( 'NONE',  ( 2.999999999999985345, 5.587461875839184522, 4.000000000000000000 ) ) ;
#138964 = AXIS2_PLACEMENT_3D ( 'NONE', #29427, #117842, #119981 ) ;
#138965 = CARTESIAN_POINT ( 'NONE',  ( 59.77083333333332860, -7.949999999999998401, -2.130196079827426203 ) ) ;
#138966 = ORIENTED_EDGE ( 'NONE', *, *, #83978, .T. ) ;
#138967 = EDGE_LOOP ( 'NONE', ( #3486, #7343, #94101, #103783, #107429 ) ) ;
#138968 = CARTESIAN_POINT ( 'NONE',  ( 74.81293019189809002, -1.637169565754159617, -6.110000000000001208 ) ) ;
#138969 = ORIENTED_EDGE ( 'NONE', *, *, #73675, .F. ) ;
#138970 = ADVANCED_FACE ( 'NONE', ( #77751 ), #42275, .T. ) ;
#138971 = VECTOR ( 'NONE', #108565, 1000.000000000000000 ) ;
#138972 = CARTESIAN_POINT ( 'NONE',  ( -2.149948714589740462, -8.240707523384200428, 17.25253755692238400 ) ) ;
#138973 = CARTESIAN_POINT ( 'NONE',  ( -35.75830541574791255, 0.7592924766157104211, 14.37146558664990970 ) ) ;
#138974 = ORIENTED_EDGE ( 'NONE', *, *, #5213, .T. ) ;
#138975 = ADVANCED_FACE ( 'NONE', ( #85743 ), #30682, .F. ) ;
#138976 = DIRECTION ( 'NONE',  ( 0.7071067811865486830, -0.7071067811865464625, -0.000000000000000000 ) ) ;
#138977 = PLANE ( 'NONE',  #132346 ) ;
#138978 = AXIS2_PLACEMENT_3D ( 'NONE', #85804, #131470, #31442 ) ;
#138979 = ORIENTED_EDGE ( 'NONE', *, *, #113439, .T. ) ;
#138980 = CARTESIAN_POINT ( 'NONE',  ( 21.48921356237309155, -27.52281430457070499, 5.000000000000000000 ) ) ;
#138981 = CIRCLE ( 'NONE', #51013, 6.350000000000008527 ) ;
#138982 = DIRECTION ( 'NONE',  ( -0.000000000000000000, 0.000000000000000000, 1.000000000000000000 ) ) ;
#138983 = EDGE_CURVE ( 'NONE', #106767, #129767, #53868, .T. ) ;
#138984 = DIRECTION ( 'NONE',  ( -0.7071067811865486830, -0.7071067811865464625, 0.000000000000000000 ) ) ;
#138985 = VECTOR ( 'NONE', #114280, 1000.000000000000000 ) ;
#138986 = VERTEX_POINT ( 'NONE', #140828 ) ;
#138987 = VERTEX_POINT ( 'NONE', #142301 ) ;
#138988 = AXIS2_PLACEMENT_3D ( 'NONE', #116422, #62064, #95371 ) ;
#138989 = DIRECTION ( 'NONE',  ( -0.7071067811865486830, -0.7071067811865464625, -0.000000000000000000 ) ) ;
#138990 = PLANE ( 'NONE',  #131901 ) ;
#138991 = EDGE_CURVE ( 'NONE', #60821, #128385, #98754, .T. ) ;
#138992 = CARTESIAN_POINT ( 'NONE',  ( 0.2997448713915885632, -27.71228299555206220, 4.000000000000000000 ) ) ;
#138993 = DIRECTION ( 'NONE',  ( -0.000000000000000000, 0.3543493200069153248, 0.9351131265310292928 ) ) ;
#138994 = EDGE_CURVE ( 'NONE', #2806, #37814, #142989, .T. ) ;
#138995 = DIRECTION ( 'NONE',  ( 0.000000000000000000, 0.000000000000000000, 1.000000000000000000 ) ) ;
#138996 = DIRECTION ( 'NONE',  ( -0.3543493200069162685, -0.000000000000000000, -0.9351131265310288487 ) ) ;
#138997 = EDGE_CURVE ( 'NONE', #131795, #96830, #132138, .T. ) ;
#138998 = ORIENTED_EDGE ( 'NONE', *, *, #92720, .T. ) ;
#138999 = EDGE_LOOP ( 'NONE', ( #93852, #124737, #2561, #25187 ) ) ;
#139000 = VERTEX_POINT ( 'NONE', #11013 ) ;
#139001 = ORIENTED_EDGE ( 'NONE', *, *, #7950, .F. ) ;
#139002 = VECTOR ( 'NONE', #80803, 1000.000000000000000 ) ;
#139003 = CARTESIAN_POINT ( 'NONE',  ( 56.99451991528749062, 28.92564299267978001, 4.000000000000000000 ) ) ;
#139004 = VERTEX_POINT ( 'NONE', #21920 ) ;
#139005 = CARTESIAN_POINT ( 'NONE',  ( 6.229065384000522343, 0.000000000000000000, 2.500000000000000444 ) ) ;
#139006 = CARTESIAN_POINT ( 'NONE',  ( 2.999999999999978240, -16.60178936734448385, 0.8616154019347568305 ) ) ;
#139007 = PLANE ( 'NONE',  #31810 ) ;
#139008 = CARTESIAN_POINT ( 'NONE',  ( 27.53159235450332076, 9.902892378096218942E-16, 0.000000000000000000 ) ) ;
#139009 = AXIS2_PLACEMENT_3D ( 'NONE', #55073, #10115, #89816 ) ;
#139010 = CARTESIAN_POINT ( 'NONE',  ( 27.00000000000000711, -6.919509820621859042, -2.766677502517353116 ) ) ;
#139011 = VERTEX_POINT ( 'NONE', #66165 ) ;
#139012 = DIRECTION ( 'NONE',  ( -0.7071067811865486830, 0.7071067811865464625, 0.000000000000000000 ) ) ;
#139013 = LINE ( 'NONE', #118673, #16465 ) ;
#139014 = ORIENTED_EDGE ( 'NONE', *, *, #18591, .T. ) ;
#139015 = CARTESIAN_POINT ( 'NONE',  ( 20.30673006690388505, -3.740707523384244837, 12.88036043432862954 ) ) ;
#139016 = ORIENTED_EDGE ( 'NONE', *, *, #121183, .F. ) ;
#139017 = FACE_OUTER_BOUND ( 'NONE', #30263, .T. ) ;
#139018 = ORIENTED_EDGE ( 'NONE', *, *, #98340, .F. ) ;
#139019 = ORIENTED_EDGE ( 'NONE', *, *, #35215, .F. ) ;
#139020 = CARTESIAN_POINT ( 'NONE',  ( 69.12543019189809002, 5.291415217122919401, 3.055000000000002824 ) ) ;
#139022 = ORIENTED_EDGE ( 'NONE', *, *, #71021, .F. ) ;
#139021 = AXIS2_PLACEMENT_3D ( 'NONE', #8353, #30882, #9813 ) ;
#139023 = FACE_OUTER_BOUND ( 'NONE', #12257, .T. ) ;
#139024 = PLANE ( 'NONE',  #65851 ) ;
#139025 = CARTESIAN_POINT ( 'NONE',  ( 111.1254301918981042, 5.291415217122919401, 3.055000000000002824 ) ) ;
#139026 = LINE ( 'NONE', #39730, #28612 ) ;
#139027 = ADVANCED_FACE ( 'NONE', ( #56746 ), #81330, .F. ) ;
#139028 = FACE_OUTER_BOUND ( 'NONE', #88823, .T. ) ;
#139029 = PLANE ( 'NONE',  #61498 ) ;
#139030 = VECTOR ( 'NONE', #100402, 1000.000000000000000 ) ;
#139031 = PLANE ( 'NONE',  #33129 ) ;
#139032 =( NAMED_UNIT ( * ) SI_UNIT ( $, .STERADIAN. ) SOLID_ANGLE_UNIT ( ) );
#139034 = CARTESIAN_POINT ( 'NONE',  ( 77.07919371712957002, 3.975000000000002753, -6.884901960086283523 ) ) ;
#139033 = VECTOR ( 'NONE', #131150, 1000.000000000000000 ) ;
#139036 = ORIENTED_EDGE ( 'NONE', *, *, #92771, .T. ) ;
#139035 = VECTOR ( 'NONE', #59812, 1000.000000000000227 ) ;
#139037 = DIRECTION ( 'NONE',  ( 1.000000000000000000, 0.000000000000000000, 0.000000000000000000 ) ) ;
#139038 = EDGE_LOOP ( 'NONE', ( #79228, #133977, #30085, #63113, #75772 ) ) ;
#139039 = ORIENTED_EDGE ( 'NONE', *, *, #112198, .F. ) ;
#139040 = DIRECTION ( 'NONE',  ( 0.7071067811865487940, 0.7071067811865463515, 0.000000000000000000 ) ) ;
#139041 = VECTOR ( 'NONE', #25269, 1000.000000000000000 ) ;
#139042 = ORIENTED_EDGE ( 'NONE', *, *, #24859, .T. ) ;
#139043 = VECTOR ( 'NONE', #25283, 1000.000000000000227 ) ;
#139044 = AXIS2_PLACEMENT_3D ( 'NONE', #91766, #135991, #134593 ) ;
#139045 = LINE ( 'NONE', #28854, #580 ) ;
#139046 = PLANE ( 'NONE',  #6176 ) ;
#139047 = ADVANCED_FACE ( 'NONE', ( #68332 ), #112503, .F. ) ;
#139048 = DIRECTION ( 'NONE',  ( -0.000000000000000000, 0.000000000000000000, 1.000000000000000000 ) ) ;
#139049 = LINE ( 'NONE', #121382, #83481 ) ;
#139050 = ORIENTED_EDGE ( 'NONE', *, *, #455, .F. ) ;
#139051 = ADVANCED_FACE ( 'NONE', ( #134267 ), #125538, .F. ) ;
#139052 = CARTESIAN_POINT ( 'NONE',  ( 0.07239000078485262335, -48.13855614192807764, 37.56434003615987649 ) ) ;
#139054 = ORIENTED_EDGE ( 'NONE', *, *, #125969, .F. ) ;
#139053 = AXIS2_PLACEMENT_3D ( 'NONE', #101477, #81180, #12324 ) ;
#139055 = CARTESIAN_POINT ( 'NONE',  ( 6.978736474768552966, -5.808823158059033709, 5.808823158059035485 ) ) ;
#139056 = DIRECTION ( 'NONE',  ( 0.3543493200069162685, -0.000000000000000000, -0.9351131265310288487 ) ) ;
#139057 = FACE_OUTER_BOUND ( 'NONE', #55783, .T. ) ;
#139058 = EDGE_CURVE ( 'NONE', #1414, #68140, #14619, .T. ) ;
#139059 = DIRECTION ( 'NONE',  ( -0.7071067811865486830, -0.7071067811865464625, 0.000000000000000000 ) ) ;
#139060 = ORIENTED_EDGE ( 'NONE', *, *, #131282, .T. ) ;
#139061 = ORIENTED_EDGE ( 'NONE', *, *, #87391, .F. ) ;
#139062 = ORIENTED_EDGE ( 'NONE', *, *, #99933, .T. ) ;
#139064 = AXIS2_PLACEMENT_3D ( 'NONE', #106971, #75101, #51907 ) ;
#139063 = DIRECTION ( 'NONE',  ( 0.3543493200069163795, -9.265275131829747941E-33, -0.9351131265310288487 ) ) ;
#139065 = DIRECTION ( 'NONE',  ( -0.000000000000000000, 0.3543493200069153248, 0.9351131265310292928 ) ) ;
#139066 = FACE_OUTER_BOUND ( 'NONE', #121214, .T. ) ;
#139067 = LINE ( 'NONE', #130337, #35810 ) ;
#139068 = CARTESIAN_POINT ( 'NONE',  ( -14.29289321881335795, -18.74070752338409562, 5.000000000000000000 ) ) ;
#139069 = DIRECTION ( 'NONE',  ( -0.7071067811865486830, 0.7071067811865464625, 0.000000000000000000 ) ) ;
#139070 = EDGE_CURVE ( 'NONE', #38741, #12574, #48394, .T. ) ;
#139071 = VECTOR ( 'NONE', #141461, 1000.000000000000000 ) ;
#139072 = VECTOR ( 'NONE', #1663, 999.9999999999998863 ) ;
#139073 = CARTESIAN_POINT ( 'NONE',  ( -39.29974487139159578, -27.71228299555233576, 4.000000000000000000 ) ) ;
#139074 = SURFACE_SIDE_STYLE ('',( #130343 ) ) ;
#139075 =( NAMED_UNIT ( * ) PLANE_ANGLE_UNIT ( ) SI_UNIT ( $, .RADIAN. ) );
#139076 = AXIS2_PLACEMENT_3D ( 'NONE', #70513, #24106, #125569 ) ;
#139077 = VERTEX_POINT ( 'NONE', #46591 ) ;
#139078 = DIRECTION ( 'NONE',  ( -0.7071067811865487940, 0.7071067811865463515, -0.000000000000000000 ) ) ;
#139079 = EDGE_CURVE ( 'NONE', #83776, #119750, #90776, .T. ) ;
#139081 = VECTOR ( 'NONE', #35879, 999.9999999999998863 ) ;
#139080 = LINE ( 'NONE', #27426, #137376 ) ;
#139082 = VERTEX_POINT ( 'NONE', #69751 ) ;
#139083 = CARTESIAN_POINT ( 'NONE',  ( -5.671830600776429421, 17.25929247661554911, 4.000000000000000000 ) ) ;
#139085 = ORIENTED_EDGE ( 'NONE', *, *, #31327, .F. ) ;
#139084 = DIRECTION ( 'NONE',  ( 1.000000000000000000, 0.000000000000000000, 0.000000000000000000 ) ) ;
#139086 = VECTOR ( 'NONE', #20656, 1000.000000000000227 ) ;
#139087 = FACE_OUTER_BOUND ( 'NONE', #90478, .T. ) ;
#139088 = LINE ( 'NONE', #120137, #131828 ) ;
#139089 = EDGE_CURVE ( 'NONE', #95876, #54517, #135692, .T. ) ;
#139090 = ORIENTED_EDGE ( 'NONE', *, *, #44607, .F. ) ;
#139092 = ADVANCED_FACE ( 'NONE', ( #114628 ), #36379, .F. ) ;
#139091 = PLANE ( 'NONE',  #51292 ) ;
#139093 = UNCERTAINTY_MEASURE_WITH_UNIT (LENGTH_MEASURE( 1.000000000000000082E-05 ), #79225, 'distance_accuracy_value', 'NONE');
#139094 = ORIENTED_EDGE ( 'NONE', *, *, #132283, .T. ) ;
#139095 = DIRECTION ( 'NONE',  ( 0.7071067811865486830, -0.7071067811865464625, -0.000000000000000000 ) ) ;
#139096 = CARTESIAN_POINT ( 'NONE',  ( 124.0375270504628986, -9.735942053221456900E-16, 7.949999999999998401 ) ) ;
#139097 = CARTESIAN_POINT ( 'NONE',  ( 54.48921356237310221, -27.52281430457093236, 5.000000000000000000 ) ) ;
#139098 = AXIS2_PLACEMENT_3D ( 'NONE', #77936, #35159, #123601 ) ;
#139099 = LINE ( 'NONE', #118001, #62196 ) ;
#139100 = CARTESIAN_POINT ( 'NONE',  ( -45.48921356237309510, -27.52281430457087197, 5.000000000000000000 ) ) ;
#139102 = EDGE_CURVE ( 'NONE', #12275, #83894, #133555, .T. ) ;
#139101 = DIRECTION ( 'NONE',  ( -0.3543493200069162685, -0.000000000000000000, -0.9351131265310288487 ) ) ;
#139103 = LINE ( 'NONE', #41191, #55276 ) ;
#139105 = VECTOR ( 'NONE', #95592, 1000.000000000000000 ) ;
#139104 = CARTESIAN_POINT ( 'NONE',  ( 27.39540314143522437, 2.126176841940962348, 7.934999999999989839 ) ) ;
#139106 = CARTESIAN_POINT ( 'NONE',  ( 6.978736474768552966, -5.808823158059033709, 5.808823158059035485 ) ) ;
#139107 = CARTESIAN_POINT ( 'NONE',  ( 29.99999999999979750, -10.44781430457071814, 5.000000000000000000 ) ) ;
#139108 = CARTESIAN_POINT ( 'NONE',  ( 6.489213562373093325, -27.52281430457059841, 5.000000000000000000 ) ) ;
#139109 = DIRECTION ( 'NONE',  ( 0.000000000000000000, 0.000000000000000000, 1.000000000000000000 ) ) ;
#139110 = EDGE_LOOP ( 'NONE', ( #35280, #130840, #26165, #50867 ) ) ;
#139112 = EDGE_LOOP ( 'NONE', ( #6511, #71427, #65584, #16148 ) ) ;
#139111 = EDGE_CURVE ( 'NONE', #94938, #48357, #58900, .T. ) ;
#139113 = ADVANCED_FACE ( 'NONE', ( #103060 ), #3696, .F. ) ;
#139114 = CARTESIAN_POINT ( 'NONE',  ( 85.72916666666664298, 7.950000000000001954, -2.130196079827421762 ) ) ;
#139115 = ORIENTED_EDGE ( 'NONE', *, *, #47240, .F. ) ;
#139116 = CARTESIAN_POINT ( 'NONE',  ( 0.000000000000000000, 2.375000000000000000, 0.000000000000000000 ) ) ;
#139117 = CARTESIAN_POINT ( 'NONE',  ( 23.08747294953710494, -6.094999999999989981, 3.732111120401553285E-16 ) ) ;
#139118 =( GEOMETRIC_REPRESENTATION_CONTEXT ( 3 ) GLOBAL_UNCERTAINTY_ASSIGNED_CONTEXT ( ( #17290 ) ) GLOBAL_UNIT_ASSIGNED_CONTEXT ( ( #128184, #6328, #74521 ) ) REPRESENTATION_CONTEXT ( 'NONE', 'WORKASPACE' ) );
#139119 = CARTESIAN_POINT ( 'NONE',  ( 31.14169371712956291, -2.130196079827424871, -7.949999999999998401 ) ) ;
#139120 = ORIENTED_EDGE ( 'NONE', *, *, #9603, .T. ) ;
#139121 = FACE_OUTER_BOUND ( 'NONE', #62823, .T. ) ;
#139122 = EDGE_CURVE ( 'NONE', #85885, #14857, #122653, .T. ) ;
#139123 = DIRECTION ( 'NONE',  ( 0.7071067811865487940, 0.7071067811865463515, 0.000000000000000000 ) ) ;
#139124 = PLANE ( 'NONE',  #14011 ) ;
#139125 = CARTESIAN_POINT ( 'NONE',  ( -32.67183060077625356, -21.74070752338406010, 4.000000000000000000 ) ) ;
#139126 = EDGE_CURVE ( 'NONE', #126258, #81493, #5128, .T. ) ;
#139127 = EDGE_CURVE ( 'NONE', #96060, #15871, #71885, .T. ) ;
#139128 = DIRECTION ( 'NONE',  ( -1.000000000000000000, -0.000000000000000000, -0.000000000000000000 ) ) ;
#139129 = CARTESIAN_POINT ( 'NONE',  ( 0.000000000000000000, 0.000000000000000000, 5.000000000000000000 ) ) ;
#139130 = PLANE ( 'NONE',  #45729 ) ;
#139131 = CARTESIAN_POINT ( 'NONE',  ( 30.79289321881324781, -5.240707523384230626, 5.000000000000000000 ) ) ;
#139132 = AXIS2_PLACEMENT_3D ( 'NONE', #70662, #48885, #15488 ) ;
#139133 = PLANE ( 'NONE',  #28498 ) ;
#139134 = CARTESIAN_POINT ( 'NONE',  ( 13.49999999999991473, 3.073033219394640803, -6.593910359670939414 ) ) ;
#139135 = LINE ( 'NONE', #105741, #56847 ) ;
#139136 =( BOUNDED_CURVE ( )  B_SPLINE_CURVE ( 3, ( #24467, #55156, #143555, #21803 ),
 .UNSPECIFIED., .F., .T. ) 
 B_SPLINE_CURVE_WITH_KNOTS ( ( 4, 4 ),
 ( 2.779374508378132713, 4.199602562396797190 ),
 .UNSPECIFIED. ) 
 CURVE ( )  GEOMETRIC_REPRESENTATION_ITEM ( )  RATIONAL_B_SPLINE_CURVE ( ( 1.000000000000000000, 0.8388583629366712646, 0.8388583629366712646, 1.000000000000000000 ) ) 
 REPRESENTATION_ITEM ( '' )  );
#139137 = CARTESIAN_POINT ( 'NONE',  ( 56.00844637038723306, -48.60795469097144661, 38.18754904900261238 ) ) ;
#139138 = VERTEX_POINT ( 'NONE', #61719 ) ;
#139139 = ORIENTED_EDGE ( 'NONE', *, *, #19927, .T. ) ;
#139140 = CARTESIAN_POINT ( 'NONE',  ( 100.3337635252314328, 6.110000000000001208, 1.122388791418549305E-15 ) ) ;
#139141 = ORIENTED_EDGE ( 'NONE', *, *, #72908, .F. ) ;
#139142 = EDGE_CURVE ( 'NONE', #91989, #115804, #95742, .T. ) ;
#139143 = MANIFOLD_SOLID_BREP ( 'Boss-Extrude1', #71883 ) ;
#139144 = DIRECTION ( 'NONE',  ( -0.7071067811865486830, -0.7071067811865464625, 0.000000000000000000 ) ) ;
#139145 = CARTESIAN_POINT ( 'NONE',  ( 25.49999999999982236, 18.05218569542898521, 5.000000000000000000 ) ) ;
#139146 = VERTEX_POINT ( 'NONE', #126926 ) ;
#139148 = EDGE_CURVE ( 'NONE', #67859, #123554, #7280, .T. ) ;
#139147 = VECTOR ( 'NONE', #80413, 1000.000000000000000 ) ;
#139149 = FACE_OUTER_BOUND ( 'NONE', #74620, .T. ) ;
#139150 = DIRECTION ( 'NONE',  ( 0.7071067811865486830, -0.7071067811865464625, -0.000000000000000000 ) ) ;
#139151 = CIRCLE ( 'NONE', #99793, 2.337566348077130929 ) ;
#139152 = VECTOR ( 'NONE', #84271, 1000.000000000000000 ) ;
#139153 = CARTESIAN_POINT ( 'NONE',  ( 90.91209685856478018, 5.291415217122921177, -3.054999999999994831 ) ) ;
#139154 = ORIENTED_EDGE ( 'NONE', *, *, #32906, .F. ) ;
#139155 = LINE ( 'NONE', #129672, #92903 ) ;
#139156 = ORIENTED_EDGE ( 'NONE', *, *, #73334, .F. ) ;
#139157 = LINE ( 'NONE', #73884, #24473 ) ;
#139158 = AXIS2_PLACEMENT_3D ( 'NONE', #55261, #56730, #134987 ) ;
#139159 = VECTOR ( 'NONE', #41543, 1000.000000000000227 ) ;
#139160 = FACE_OUTER_BOUND ( 'NONE', #26554, .T. ) ;
#139161 = VECTOR ( 'NONE', #56210, 1000.000000000000000 ) ;
#139162 = VECTOR ( 'NONE', #88077, 1000.000000000000227 ) ;
#139163 = PLANE ( 'NONE',  #1397 ) ;
#139164 = DIRECTION ( 'NONE',  ( -0.000000000000000000, 0.000000000000000000, 1.000000000000000000 ) ) ;
#139165 = CIRCLE ( 'NONE', #97527, 2.055000000000001048 ) ;
#139166 = ORIENTED_EDGE ( 'NONE', *, *, #107461, .T. ) ;
#139167 = ORIENTED_EDGE ( 'NONE', *, *, #14043, .F. ) ;
#139168 = ORIENTED_EDGE ( 'NONE', *, *, #52803, .T. ) ;
#139169 = CARTESIAN_POINT ( 'NONE',  ( 9.758600742197899081, 21.72500000000000853, 5.000000000000000000 ) ) ;
#139170 = CARTESIAN_POINT ( 'NONE',  ( 11.99451991528749417, 28.92564299267946382, 4.000000000000000000 ) ) ;
#139171 = CARTESIAN_POINT ( 'NONE',  ( 6.775403141435219823, -2.126176841940958351, -7.934999999999988951 ) ) ;
#139172 = VECTOR ( 'NONE', #44847, 1000.000000000000000 ) ;
#139173 = CARTESIAN_POINT ( 'NONE',  ( 25.17183060077628909, -11.24070752338417556, 4.000000000000000000 ) ) ;
#139174 = ADVANCED_FACE ( 'NONE', ( #17462 ), #39240, .F. ) ;
#139176 = EDGE_CURVE ( 'NONE', #54517, #124390, #10587, .T. ) ;
#139175 = FILL_AREA_STYLE ('',( #17363 ) ) ;
#139177 = VERTEX_POINT ( 'NONE', #92885 ) ;
#139178 = EDGE_LOOP ( 'NONE', ( #16283, #120411, #114386, #85354 ) ) ;
#139179 = VECTOR ( 'NONE', #59159, 1000.000000000000000 ) ;
#139180 = EDGE_CURVE ( 'NONE', #31468, #54110, #50780, .T. ) ;
#139181 = CARTESIAN_POINT ( 'NONE',  ( -3.284736659904287315, 22.22500000000000142, 16.98967855471618904 ) ) ;
#139182 = ORIENTED_EDGE ( 'NONE', *, *, #75340, .F. ) ;
#139183 = ORIENTED_EDGE ( 'NONE', *, *, #117666, .F. ) ;
#139184 = AXIS2_PLACEMENT_3D ( 'NONE', #81525, #26408, #73306 ) ;
#139185 = CARTESIAN_POINT ( 'NONE',  ( 115.2662635252314374, 4.472830434245838482, -4.472830434245837594 ) ) ;
#139186 = VECTOR ( 'NONE', #28458, 1000.000000000000000 ) ;
#139187 = VECTOR ( 'NONE', #128610, 1000.000000000000000 ) ;
#139188 = CARTESIAN_POINT ( 'NONE',  ( -66.18398860626901126, 28.73617430169833753, 5.000000000000000000 ) ) ;
#139189 = CARTESIAN_POINT ( 'NONE',  ( 21.96495920677946856, -2.033836129387410985, 4.000000000000000000 ) ) ;
#139190 = EDGE_LOOP ( 'NONE', ( #58689, #40551, #118974, #29324 ) ) ;
#139191 = DIRECTION ( 'NONE',  ( 0.3543493200069162685, -0.000000000000000000, -0.9351131265310288487 ) ) ;
#139192 = PRESENTATION_LAYER_ASSIGNMENT (  '', '', ( #72049 ) ) ;
#139193 = DIRECTION ( 'NONE',  ( -0.3543493200069162685, -0.000000000000000000, -0.9351131265310288487 ) ) ;
#139194 = CARTESIAN_POINT ( 'NONE',  ( 20.99999999999985789, 19.55218569542897100, 5.000000000000000000 ) ) ;
#139195 = AXIS2_PLACEMENT_3D ( 'NONE', #5860, #113938, #135015 ) ;
#139196 = LINE ( 'NONE', #128994, #83734 ) ;
#139197 = ORIENTED_EDGE ( 'NONE', *, *, #136476, .F. ) ;
#139198 = LINE ( 'NONE', #28986, #116160 ) ;
#139199 = CARTESIAN_POINT ( 'NONE',  ( -8.229957205422008926, 21.73644205237997795, 5.000000000000000000 ) ) ;
#139200 = ORIENTED_EDGE ( 'NONE', *, *, #72946, .T. ) ;
#139201 = CARTESIAN_POINT ( 'NONE',  ( 25.39999999999999858, -5.131256043349313067, -6.052638797879072108 ) ) ;
#139202 = DIRECTION ( 'NONE',  ( 0.7071067811865486830, -0.7071067811865464625, -0.000000000000000000 ) ) ;
#139203 = AXIS2_PLACEMENT_3D ( 'NONE', #125542, #74005, #120313 ) ;
#139204 = VERTEX_POINT ( 'NONE', #105188 ) ;
#139205 = LINE ( 'NONE', #72548, #89894 ) ;
#139206 = ORIENTED_EDGE ( 'NONE', *, *, #17918, .T. ) ;
#139207 = ORIENTED_EDGE ( 'NONE', *, *, #7118, .T. ) ;
#139208 = VERTEX_POINT ( 'NONE', #50115 ) ;
#139209 = CARTESIAN_POINT ( 'NONE',  ( 27.91209685856478728, 5.291415217122921177, -3.054999999999994831 ) ) ;
#139210 = VECTOR ( 'NONE', #73719, 1000.000000000000114 ) ;
#139211 = DIRECTION ( 'NONE',  ( 0.6830127018922181881, 0.6830127018922202975, -0.2588190451025214056 ) ) ;
#139212 = DIRECTION ( 'NONE',  ( 0.6830127018922180770, -0.6830127018922204085, -0.2588190451025213501 ) ) ;
#139213 = DIRECTION ( 'NONE',  ( 1.000000000000000000, 1.224606353822377258E-16, 0.000000000000000000 ) ) ;
#139214 = CYLINDRICAL_SURFACE ( 'NONE', #14918, 2.500000000000000000 ) ;
#139215 = DIRECTION ( 'NONE',  ( 0.7071067811865487940, 0.7071067811865463515, 0.000000000000000000 ) ) ;
#139217 = FACE_OUTER_BOUND ( 'NONE', #86683, .T. ) ;
#139216 = VECTOR ( 'NONE', #139688, 1000.000000000000000 ) ;
#139218 = AXIS2_PLACEMENT_3D ( 'NONE', #101263, #67975, #120862 ) ;
#139219 = CARTESIAN_POINT ( 'NONE',  ( -5.671830600776438303, 14.25929247661558286, 4.000000000000000000 ) ) ;
#139220 = CARTESIAN_POINT ( 'NONE',  ( -24.18398860626899705, 28.73617430169804265, 5.000000000000000000 ) ) ;
#139221 = DIRECTION ( 'NONE',  ( 0.6830127018922180770, -0.6830127018922204085, -0.2588190451025213501 ) ) ;
#139222 = LINE ( 'NONE', #59522, #123526 ) ;
#139223 = ORIENTED_EDGE ( 'NONE', *, *, #40854, .F. ) ;
#139224 = ORIENTED_EDGE ( 'NONE', *, *, #138029, .F. ) ;
#139225 = VERTEX_POINT ( 'NONE', #6542 ) ;
#139226 = VECTOR ( 'NONE', #71149, 999.9999999999998863 ) ;
#139227 = EDGE_LOOP ( 'NONE', ( #34546, #48335, #94691, #20884 ) ) ;
#139228 = FACE_OUTER_BOUND ( 'NONE', #141919, .T. ) ;
#139229 = VERTEX_POINT ( 'NONE', #139284 ) ;
#139231 = ORIENTED_EDGE ( 'NONE', *, *, #111962, .F. ) ;
#139230 = EDGE_CURVE ( 'NONE', #113151, #17161, #39976, .T. ) ;
#139232 = DIRECTION ( 'NONE',  ( 0.6830127018922180770, -0.6830127018922204085, -0.2588190451025213501 ) ) ;
#139233 = LINE ( 'NONE', #39931, #50315 ) ;
#139234 = ADVANCED_FACE ( 'NONE', ( #4382 ), #84870, .F. ) ;
#139235 = EDGE_CURVE ( 'NONE', #142570, #48699, #29066, .T. ) ;
#139236 = FACE_OUTER_BOUND ( 'NONE', #120525, .T. ) ;
#139237 = EDGE_LOOP ( 'NONE', ( #70556, #141600 ) ) ;
#139238 = CARTESIAN_POINT ( 'NONE',  ( 24.14562793195489121, 0.06350461447051275465, 4.871950940718897449 ) ) ;
#139239 = VECTOR ( 'NONE', #91352, 1000.000000000000000 ) ;
#139240 = ORIENTED_EDGE ( 'NONE', *, *, #34882, .F. ) ;
#139242 = EDGE_CURVE ( 'NONE', #109272, #63778, #126241, .T. ) ;
#139241 = CARTESIAN_POINT ( 'NONE',  ( 34.92499999999998295, 20.81665438641024224, 4.500000000000000888 ) ) ;
#139243 = EDGE_CURVE ( 'NONE', #28105, #35225, #52240, .T. ) ;
#139244 = DIRECTION ( 'NONE',  ( 1.000000000000000000, 0.000000000000000000, 0.000000000000000000 ) ) ;
#139245 = CARTESIAN_POINT ( 'NONE',  ( 12.31706980810188412, -2.126176841940956130, 7.934999999999991616 ) ) ;
#139246 = ORIENTED_EDGE ( 'NONE', *, *, #101732, .T. ) ;
#139247 = CARTESIAN_POINT ( 'NONE',  ( 98.78709685856479439, 3.054999999999997939, 5.291415217122920289 ) ) ;
#139248 = ADVANCED_FACE ( 'NONE', ( #121058 ), #131965, .F. ) ;
#139249 = CARTESIAN_POINT ( 'NONE',  ( -59.99451991528749772, 28.92564299267980132, 4.000000000000000000 ) ) ;
#139250 = DIRECTION ( 'NONE',  ( -0.7071067811865487940, 0.7071067811865463515, 0.000000000000000000 ) ) ;
#139251 = VERTEX_POINT ( 'NONE', #96421 ) ;
#139252 = ORIENTED_EDGE ( 'NONE', *, *, #113792, .F. ) ;
#139253 = CARTESIAN_POINT ( 'NONE',  ( 10.52840764549667618, 9.139736423841732040E-16, 0.000000000000000000 ) ) ;
#139254 = ORIENTED_EDGE ( 'NONE', *, *, #140645, .T. ) ;
#139255 = DIRECTION ( 'NONE',  ( 0.7071067811865486830, -0.7071067811865464625, -0.000000000000000000 ) ) ;
#139256 = VECTOR ( 'NONE', #127277, 1000.000000000000000 ) ;
#139257 = CARTESIAN_POINT ( 'NONE',  ( -34.49999999999975842, -13.53574439159936915, 4.994342998332166772 ) ) ;
#139258 = CARTESIAN_POINT ( 'NONE',  ( 15.18398860626900237, 28.73617430169797871, 5.000000000000000000 ) ) ;
#139259 = EDGE_LOOP ( 'NONE', ( #75938, #36024, #97208, #132149 ) ) ;
#139260 = VECTOR ( 'NONE', #101025, 1000.000000000000227 ) ;
#139261 = DIRECTION ( 'NONE',  ( 0.7071067811865486830, -0.7071067811865464625, -0.000000000000000000 ) ) ;
#139262 = ADVANCED_FACE ( 'NONE', ( #109480 ), #43509, .T. ) ;
#139263 = AXIS2_PLACEMENT_3D ( 'NONE', #95998, #109007, #41624 ) ;
#139264 = DIRECTION ( 'NONE',  ( 0.7071067811865487940, 0.7071067811865463515, 0.000000000000000000 ) ) ;
#139265 = CARTESIAN_POINT ( 'NONE',  ( -20.31999820585105709, -22.22500000000000142, 10.53438114343992105 ) ) ;
#139266 = ORIENTED_EDGE ( 'NONE', *, *, #54043, .F. ) ;
#139267 = CARTESIAN_POINT ( 'NONE',  ( -20.99451991528748707, 28.92564299267952777, 4.000000000000000000 ) ) ;
#139268 = VECTOR ( 'NONE', #73983, 999.9999999999998863 ) ;
#139269 = VECTOR ( 'NONE', #35369, 1000.000000000000000 ) ;
#139270 = VECTOR ( 'NONE', #49302, 1000.000000000000227 ) ;
#139271 = PLANE ( 'NONE',  #123525 ) ;
#139272 = ORIENTED_EDGE ( 'NONE', *, *, #106045, .T. ) ;
#139274 = ORIENTED_EDGE ( 'NONE', *, *, #109865, .T. ) ;
#139273 = CARTESIAN_POINT ( 'NONE',  ( 33.48921356237309510, -27.52281430457078670, 5.000000000000000000 ) ) ;
#139275 = ORIENTED_EDGE ( 'NONE', *, *, #137161, .F. ) ;
#139276 = CARTESIAN_POINT ( 'NONE',  ( -14.81601139373099585, 28.73617430169776910, 5.000000000000000000 ) ) ;
#139277 = AXIS2_PLACEMENT_3D ( 'NONE', #17674, #3237, #103268 ) ;
#139278 =( NAMED_UNIT ( * ) SI_UNIT ( $, .STERADIAN. ) SOLID_ANGLE_UNIT ( ) );
#139279 = EDGE_CURVE ( 'NONE', #110441, #74437, #10846, .T. ) ;
#139280 = ORIENTED_EDGE ( 'NONE', *, *, #37611, .F. ) ;
#139281 = LINE ( 'NONE', #127675, #90506 ) ;
#139282 = UNCERTAINTY_MEASURE_WITH_UNIT (LENGTH_MEASURE( 1.000000000000000082E-05 ), #60207, 'distance_accuracy_value', 'NONE');
#139283 = DIRECTION ( 'NONE',  ( 0.7071067811865486830, -0.7071067811865464625, -0.000000000000000000 ) ) ;
#139284 = CARTESIAN_POINT ( 'NONE',  ( -32.99999999999977263, -7.068876922607736368, 4.000000000000000000 ) ) ;
#139285 = VECTOR ( 'NONE', #32946, 1000.000000000000000 ) ;
#139286 = CARTESIAN_POINT ( 'NONE',  ( -57.18398860626899705, 28.73617430169827358, 5.000000000000000000 ) ) ;
#139287 = DIRECTION ( 'NONE',  ( 0.7071067811865487940, -0.7071067811865463515, 0.000000000000000000 ) ) ;
#139288 = FACE_OUTER_BOUND ( 'NONE', #131037, .T. ) ;
#139290 = EDGE_CURVE ( 'NONE', #109637, #97476, #7998, .T. ) ;
#139289 = CARTESIAN_POINT ( 'NONE',  ( 1.516262732464673579, 3.821174125832445049E-16, 0.000000000000000000 ) ) ;
#139291 = PLANE ( 'NONE',  #139184 ) ;
#139292 = DIRECTION ( 'NONE',  ( 1.000000000000000000, 0.000000000000000000, 0.000000000000000000 ) ) ;
#139293 = PLANE ( 'NONE',  #34454 ) ;
#139294 = CARTESIAN_POINT ( 'NONE',  ( 0.5685132242927012358, 4.584330080086930965E-16, 0.000000000000000000 ) ) ;
#139295 = CARTESIAN_POINT ( 'NONE',  ( -2.671830600776452957, -6.740707523384211086, 4.000000000000000000 ) ) ;
#139296 = VERTEX_POINT ( 'NONE', #64546 ) ;
#139297 = AXIS2_PLACEMENT_3D ( 'NONE', #73912, #6454, #115962 ) ;
#139298 = ORIENTED_EDGE ( 'NONE', *, *, #10873, .F. ) ;
#139299 = ORIENTED_EDGE ( 'NONE', *, *, #80030, .F. ) ;
#139300 = EDGE_CURVE ( 'NONE', #13156, #58219, #42107, .T. ) ;
#139301 = CARTESIAN_POINT ( 'NONE',  ( 110.5208333333333428, 7.949999999999999289, 2.130196079827431532 ) ) ;
#139302 = VECTOR ( 'NONE', #91216, 1000.000000000000000 ) ;
#139303 = ORIENTED_EDGE ( 'NONE', *, *, #86194, .T. ) ;
#139304 = EDGE_LOOP ( 'NONE', ( #53972, #86550, #3117, #1866, #70407, #98654 ) ) ;
#139305 = EDGE_CURVE ( 'NONE', #126557, #41413, #30505, .T. ) ;
#139306 = AXIS2_PLACEMENT_3D ( 'NONE', #55971, #13826, #43628 ) ;
#139307 = ORIENTED_EDGE ( 'NONE', *, *, #133494, .T. ) ;
#139308 = DIRECTION ( 'NONE',  ( -0.3543493200069162685, -0.000000000000000000, -0.9351131265310288487 ) ) ;
#139309 = FACE_OUTER_BOUND ( 'NONE', #38302, .T. ) ;
#139310 = AXIS2_PLACEMENT_3D ( 'NONE', #71714, #101459, #90605 ) ;
#139311 = ORIENTED_EDGE ( 'NONE', *, *, #104208, .F. ) ;
#139312 = DIRECTION ( 'NONE',  ( 0.3543493200069162685, -0.000000000000000000, -0.9351131265310288487 ) ) ;
#139313 = EDGE_CURVE ( 'NONE', #54270, #131755, #86317, .T. ) ;
#139314 = PRESENTATION_STYLE_ASSIGNMENT (( #95042 ) ) ;
#139315 = DIRECTION ( 'NONE',  ( 0.000000000000000000, -1.000000000000000000, 0.000000000000000000 ) ) ;
#139316 = PLANE ( 'NONE',  #67425 ) ;
#139317 = CARTESIAN_POINT ( 'NONE',  ( 101.2087635252314470, -7.482591942790329030E-16, 6.110000000000001208 ) ) ;
#139318 = VERTEX_POINT ( 'NONE', #31220 ) ;
#139320 = CARTESIAN_POINT ( 'NONE',  ( -4.657369210609531684, 11.96381612452156418, -27.29251722484990239 ) ) ;
#139319 = APPLICATION_CONTEXT ( 'automotive_design' ) ;
#139321 = FACE_OUTER_BOUND ( 'NONE', #85877, .T. ) ;
#139322 = CARTESIAN_POINT ( 'NONE',  ( 82.32919371712955581, -3.975000000000001865, 6.884901960086284411 ) ) ;
#139323 = DIRECTION ( 'NONE',  ( -0.7071067811865486830, -0.7071067811865464625, -0.000000000000000000 ) ) ;
#139324 = CARTESIAN_POINT ( 'NONE',  ( 42.18398860626899705, 28.73617430169816700, 5.000000000000000000 ) ) ;
#139325 = DIRECTION ( 'NONE',  ( -0.7071067811865486830, -0.7071067811865464625, 0.000000000000000000 ) ) ;
#139326 = CARTESIAN_POINT ( 'NONE',  ( 38.87086038379622721, 6.884901960086289741, -3.974999999999993427 ) ) ;
#139327 = LINE ( 'NONE', #141436, #74516 ) ;
#139328 = DIRECTION ( 'NONE',  ( -1.000000000000000000, -0.000000000000000000, -0.000000000000000000 ) ) ;
#139329 = ORIENTED_EDGE ( 'NONE', *, *, #137365, .F. ) ;
#139330 = EDGE_LOOP ( 'NONE', ( #140822, #38410, #120851, #6798 ) ) ;
#139331 = CARTESIAN_POINT ( 'NONE',  ( 127.1670968585647756, -3.055000000000000160, -5.291415217122921177 ) ) ;
#139332 = EDGE_LOOP ( 'NONE', ( #93230, #73907, #63241, #9220 ) ) ;
#139333 = EDGE_CURVE ( 'NONE', #83478, #16704, #74737, .T. ) ;
#139334 = DIRECTION ( 'NONE',  ( -0.7071067811865486830, -0.7071067811865464625, 0.000000000000000000 ) ) ;
#139335 = VECTOR ( 'NONE', #103791, 1000.000000000000000 ) ;
#139336 = DIRECTION ( 'NONE',  ( -0.7071067811865487940, 0.7071067811865463515, -0.000000000000000000 ) ) ;
#139337 = VECTOR ( 'NONE', #124100, 1000.000000000000000 ) ;
#139338 = LINE ( 'NONE', #50872, #140595 ) ;
#139339 = CARTESIAN_POINT ( 'NONE',  ( 31.49999999999977973, -7.533600742197658739, 5.000000000000000000 ) ) ;
#139340 = CARTESIAN_POINT ( 'NONE',  ( -66.18398860626901126, 28.73617430169833753, 5.000000000000000000 ) ) ;
#139341 = DIRECTION ( 'NONE',  ( -8.817971600062198362E-18, -0.3543493200069152693, 0.9351131265310292928 ) ) ;
#139342 = CARTESIAN_POINT ( 'NONE',  ( 122.1204301918981230, 3.055000000000001936, -5.291415217122916737 ) ) ;
#139343 = ADVANCED_FACE ( 'NONE', ( #97129 ), #130538, .T. ) ;
#139344 = ORIENTED_EDGE ( 'NONE', *, *, #128128, .F. ) ;
#139345 = VECTOR ( 'NONE', #135476, 1000.000000000000227 ) ;
#139346 = DIRECTION ( 'NONE',  ( 0.000000000000000000, -1.000000000000000000, 0.000000000000000000 ) ) ;
#139347 = VERTEX_POINT ( 'NONE', #42819 ) ;
#139348 = PRESENTATION_LAYER_ASSIGNMENT (  '', '', ( #18956 ) ) ;
#139349 = LINE ( 'NONE', #51609, #57771 ) ;
#139350 = LINE ( 'NONE', #40725, #137942 ) ;
#139351 = CARTESIAN_POINT ( 'NONE',  ( -33.79333936457824450, 21.75929247661549581, 4.998822639870701856 ) ) ;
#139352 = DIRECTION ( 'NONE',  ( -1.000000000000000000, -0.000000000000000000, -0.000000000000000000 ) ) ;
#139353 = EDGE_LOOP ( 'NONE', ( #86409, #7945, #87082, #73319 ) ) ;
#139354 = EDGE_CURVE ( 'NONE', #128836, #110463, #87015, .T. ) ;
#139355 = CARTESIAN_POINT ( 'NONE',  ( 47.10459685856477563, 1.637169565754164946, -6.109999999999999432 ) ) ;
#139356 = ORIENTED_EDGE ( 'NONE', *, *, #40914, .T. ) ;
#139357 = PLANE ( 'NONE',  #123535 ) ;
#139358 = DIRECTION ( 'NONE',  ( 0.000000000000000000, -1.000000000000000000, 0.000000000000000000 ) ) ;
#139359 = CARTESIAN_POINT ( 'NONE',  ( -33.48921356237309510, -27.52281430457078670, 5.000000000000000000 ) ) ;
#139360 = CARTESIAN_POINT ( 'NONE',  ( 32.20666063542130075, 21.75929247661549937, 4.998822639870702744 ) ) ;
#139361 = VECTOR ( 'NONE', #35913, 999.9999999999998863 ) ;
#139362 = EDGE_CURVE ( 'NONE', #117708, #47726, #31921, .T. ) ;
#139364 = ADVANCED_FACE ( 'NONE', ( #24605 ), #55837, .F. ) ;
#139363 = CARTESIAN_POINT ( 'NONE',  ( 50.80793019189810167, -6.109999999999998543, 1.637169565754158063 ) ) ;
#139365 = VERTEX_POINT ( 'NONE', #134101 ) ;
#139366 = DIRECTION ( 'NONE',  ( -0.7071067811865486830, -0.7071067811865464625, -0.000000000000000000 ) ) ;
#139367 = LINE ( 'NONE', #129158, #45642 ) ;
#139368 = EDGE_LOOP ( 'NONE', ( #139584, #25584, #2534, #132589 ) ) ;
#139369 = ORIENTED_EDGE ( 'NONE', *, *, #92487, .F. ) ;
#139370 = LINE ( 'NONE', #136466, #114141 ) ;
#139371 = VECTOR ( 'NONE', #67796, 1000.000000000000227 ) ;
#139372 = AXIS2_PLACEMENT_3D ( 'NONE', #108861, #35660, #103696 ) ;
#139373 = ORIENTED_EDGE ( 'NONE', *, *, #46707, .F. ) ;
#139374 =( BOUNDED_CURVE ( )  B_SPLINE_CURVE ( 3, ( #106214, #73626, #105511, #48295 ),
 .UNSPECIFIED., .F., .F. ) 
 B_SPLINE_CURVE_WITH_KNOTS ( ( 4, 4 ),
 ( 5.143245962375956992, 6.645403452391244414 ),
 .UNSPECIFIED. ) 
 CURVE ( )  GEOMETRIC_REPRESENTATION_ITEM ( )  RATIONAL_B_SPLINE_CURVE ( ( 1.000000000000000000, 0.8206354192515227242, 0.8206354192515227242, 1.000000000000000000 ) ) 
 REPRESENTATION_ITEM ( '' )  );
#139375 = AXIS2_PLACEMENT_3D ( 'NONE', #133476, #34163, #2190 ) ;
#139376 = ADVANCED_FACE ( 'NONE', ( #46411 ), #136219, .F. ) ;
#139377 = DIRECTION ( 'NONE',  ( 1.000000000000000000, 1.224606353822377258E-16, 0.000000000000000000 ) ) ;
#139378 = ORIENTED_EDGE ( 'NONE', *, *, #101954, .F. ) ;
#139379 = CARTESIAN_POINT ( 'NONE',  ( -34.92500000000001137, -14.24070752338414003, 4.255531930566244903 ) ) ;
#139380 = VECTOR ( 'NONE', #73515, 1000.000000000000000 ) ;
#139381 = AXIS2_PLACEMENT_3D ( 'NONE', #83108, #69388, #50484 ) ;
#139382 = VECTOR ( 'NONE', #40226, 1000.000000000000227 ) ;
#139383 = DIRECTION ( 'NONE',  ( -1.000000000000000000, -1.224606353822377258E-16, -0.000000000000000000 ) ) ;
#139384 = FACE_BOUND ( 'NONE', #131059, .T. ) ;
#139385 = EDGE_CURVE ( 'NONE', #28277, #68408, #35531, .T. ) ;
#139386 = DIRECTION ( 'NONE',  ( -0.6830127018922180770, -0.6830127018922204085, -0.2588190451025213501 ) ) ;
#139387 = CARTESIAN_POINT ( 'NONE',  ( 47.99451991528749062, 28.92564299267971251, 4.000000000000000000 ) ) ;
#139388 = LINE ( 'NONE', #5936, #96526 ) ;
#139389 = ORIENTED_EDGE ( 'NONE', *, *, #132424, .F. ) ;
#139391 = ORIENTED_EDGE ( 'NONE', *, *, #46362, .F. ) ;
#139390 = DIRECTION ( 'NONE',  ( -1.000000000000000000, -0.000000000000000000, -0.000000000000000000 ) ) ;
#139392 = ORIENTED_EDGE ( 'NONE', *, *, #72710, .T. ) ;
#139393 = CARTESIAN_POINT ( 'NONE',  ( -20.81601139373100295, 28.73617430169773002, 5.000000000000000000 ) ) ;
#139394 = EDGE_LOOP ( 'NONE', ( #90544, #28974, #117834, #15414 ) ) ;
#139395 = CARTESIAN_POINT ( 'NONE',  ( 52.41209685856478018, 5.291415217122921177, -3.054999999999994831 ) ) ;
#139396 = ORIENTED_EDGE ( 'NONE', *, *, #92445, .T. ) ;
#139397 = DIRECTION ( 'NONE',  ( 0.7071067811865487940, -0.7071067811865463515, 0.000000000000000000 ) ) ;
#139398 = CARTESIAN_POINT ( 'NONE',  ( -7.140000000000001457, -35.14999999999999147, -39.50000000000000000 ) ) ;
#139399 = ORIENTED_EDGE ( 'NONE', *, *, #1632, .T. ) ;
#139400 = FILL_AREA_STYLE_COLOUR ( '', #97781 ) ;
#139401 = VECTOR ( 'NONE', #102652, 1000.000000000000227 ) ;
#139402 = VECTOR ( 'NONE', #95283, 1000.000000000000000 ) ;
#139403 = FACE_OUTER_BOUND ( 'NONE', #113264, .T. ) ;
#139404 = LINE ( 'NONE', #5258, #129178 ) ;
#139405 = CARTESIAN_POINT ( 'NONE',  ( -31.49999999999977973, 7.087461875839173864, 4.000000000000000000 ) ) ;
#139406 = AXIS2_PLACEMENT_3D ( 'NONE', #50774, #64499, #95692 ) ;
#139407 = LINE ( 'NONE', #50945, #107132 ) ;
#139408 = PRESENTATION_STYLE_ASSIGNMENT (( #82171 ) ) ;
#139409 = ORIENTED_EDGE ( 'NONE', *, *, #127110, .T. ) ;
#139410 = EDGE_LOOP ( 'NONE', ( #61665, #135605, #44376, #4693 ) ) ;
#139411 = AXIS2_PLACEMENT_3D ( 'NONE', #90420, #3385, #125921 ) ;
#139412 = CARTESIAN_POINT ( 'NONE',  ( 20.31663961620377279, -1.633150327867672447, -6.094999999999999751 ) ) ;
#139413 = DIRECTION ( 'NONE',  ( -0.6830127018922180770, -0.6830127018922204085, -0.2588190451025213501 ) ) ;
#139414 = VERTEX_POINT ( 'NONE', #113760 ) ;
#139415 = ORIENTED_EDGE ( 'NONE', *, *, #87944, .F. ) ;
#139416 = ORIENTED_EDGE ( 'NONE', *, *, #134408, .F. ) ;
#139417 = DIRECTION ( 'NONE',  ( -0.7071067811865487940, 0.7071067811865463515, -0.000000000000000000 ) ) ;
#139418 = ADVANCED_FACE ( 'NONE', ( #89165 ), #58731, .T. ) ;
#139419 = CARTESIAN_POINT ( 'NONE',  ( 32.20710678118632586, 3.759292476615680112, 5.000000000000000000 ) ) ;
#139420 = VERTEX_POINT ( 'NONE', #34080 ) ;
#139421 = FACE_OUTER_BOUND ( 'NONE', #76661, .T. ) ;
#139422 = EDGE_CURVE ( 'NONE', #128690, #125706, #122477, .T. ) ;
#139423 = EDGE_CURVE ( 'NONE', #131140, #40695, #113029, .T. ) ;
#139424 = EDGE_CURVE ( 'NONE', #133750, #40271, #77592, .T. ) ;
#139425 = CARTESIAN_POINT ( 'NONE',  ( 4.587903141435219823, 6.871911579029515771, 3.967499999999989146 ) ) ;
#139426 = DIRECTION ( 'NONE',  ( 0.3543493200069163240, -0.000000000000000000, 0.9351131265310288487 ) ) ;
#139427 = EDGE_CURVE ( 'NONE', #113106, #80820, #66697, .T. ) ;
#139428 = ORIENTED_EDGE ( 'NONE', *, *, #12349, .T. ) ;
#139429 = CARTESIAN_POINT ( 'NONE',  ( 2.999999999999975131, -22.22500000000000853, 4.412002311790043763 ) ) ;
#139430 = ADVANCED_FACE ( 'NONE', ( #79032 ), #102189, .F. ) ;
#139431 = CARTESIAN_POINT ( 'NONE',  ( -15.18398860626900237, 28.73617430169797871, 5.000000000000000000 ) ) ;
#139432 = AXIS2_PLACEMENT_3D ( 'NONE', #62129, #61447, #117181 ) ;
#139433 = B_SPLINE_CURVE_WITH_KNOTS ( 'NONE', 3,
 ( #107773, #109223, #75891, #9901, #52689, #77355, #98362, #43981, #33142, #8434, #120805, #22194, #110622, #55577 ),
 .UNSPECIFIED., .F., .F.,
 ( 4, 2, 2, 2, 2, 2, 4 ),
 ( 0.002080057358902690293, 0.002339902428862985096, 0.002599747498823280333, 0.003119437638743870374, 0.003379282708704165611, 0.003639127778664460414, 0.004158817918585050455 ),
 .UNSPECIFIED. ) ;
#139434 = CARTESIAN_POINT ( 'NONE',  ( 19.82816939922339117, -5.240707523384228850, 4.000000000000000000 ) ) ;
#139436 = VERTEX_POINT ( 'NONE', #90595 ) ;
#139435 = CARTESIAN_POINT ( 'NONE',  ( -13.49999999999990230, -4.912538124160707120, 4.000000000000000000 ) ) ;
#139438 = CIRCLE ( 'NONE', #83869, 2.500000000000000888 ) ;
#139437 = CARTESIAN_POINT ( 'NONE',  ( 10.10830628287044064, 1.633150327867697316, -6.094999999999986429 ) ) ;
#139439 = ORIENTED_EDGE ( 'NONE', *, *, #47557, .F. ) ;
#139440 = ADVANCED_FACE ( 'NONE', ( #92002 ), #2846, .F. ) ;
#139441 = LINE ( 'NONE', #119753, #40383 ) ;
#139442 = FACE_OUTER_BOUND ( 'NONE', #97775, .T. ) ;
#139443 = CARTESIAN_POINT ( 'NONE',  ( 109.3541666666666714, -2.130196079827425759, -7.950000000000000178 ) ) ;
#139444 = VERTEX_POINT ( 'NONE', #56582 ) ;
#139445 = EDGE_CURVE ( 'NONE', #17061, #68847, #100748, .T. ) ;
#139446 = CARTESIAN_POINT ( 'NONE',  ( 13.49159235450332162, 3.061616997868380183E-16, -2.500000000000001332 ) ) ;
#139447 = FACE_OUTER_BOUND ( 'NONE', #28988, .T. ) ;
#139448 = DIRECTION ( 'NONE',  ( -0.7071067811865486830, -0.7071067811865464625, -0.000000000000000000 ) ) ;
#139449 = VECTOR ( 'NONE', #68841, 1000.000000000000000 ) ;
#139450 = ORIENTED_EDGE ( 'NONE', *, *, #112816, .T. ) ;
#139451 = CARTESIAN_POINT ( 'NONE',  ( 23.99999999999983658, -10.06887692260771239, 4.000000000000000000 ) ) ;
#139452 = DIRECTION ( 'NONE',  ( -0.000000000000000000, -0.3543493200069152693, 0.9351131265310292928 ) ) ;
#139453 = LINE ( 'NONE', #84352, #127964 ) ;
#139454 = EDGE_CURVE ( 'NONE', #125425, #86499, #47144, .T. ) ;
#139455 = DIRECTION ( 'NONE',  ( 1.000000000000000000, 0.000000000000000000, 0.000000000000000000 ) ) ;
#139456 = LINE ( 'NONE', #115476, #27521 ) ;
#139457 = ORIENTED_EDGE ( 'NONE', *, *, #54339, .F. ) ;
#139458 = ORIENTED_EDGE ( 'NONE', *, *, #137002, .T. ) ;
#139459 = VECTOR ( 'NONE', #92536, 1000.000000000000000 ) ;
#139460 = CARTESIAN_POINT ( 'NONE',  ( -13.82816939922343380, 15.75929247661555443, 4.000000000000000000 ) ) ;
#139461 =( LENGTH_UNIT ( ) NAMED_UNIT ( * ) SI_UNIT ( .MILLI., .METRE. ) );
#139462 = EDGE_CURVE ( 'NONE', #49148, #104848, #14452, .T. ) ;
#139463 = CARTESIAN_POINT ( 'NONE',  ( 11.79123647476855297, -9.717572351234235426E-16, -7.934999999999990727 ) ) ;
#139464 = CARTESIAN_POINT ( 'NONE',  ( 0.1839886062690032631, 28.73617430169787568, 5.000000000000000000 ) ) ;
#139465 = DIRECTION ( 'NONE',  ( 0.000000000000000000, -1.000000000000000000, 0.000000000000000000 ) ) ;
#139466 = CARTESIAN_POINT ( 'NONE',  ( 17.99451991528748351, 28.92564299267950645, 4.000000000000000000 ) ) ;
#139467 = VERTEX_POINT ( 'NONE', #25309 ) ;
#139468 = CARTESIAN_POINT ( 'NONE',  ( -41.99451991528749062, 28.92564299267967343, 4.000000000000000000 ) ) ;
#139469 = LINE ( 'NONE', #116249, #44328 ) ;
#139470 = CARTESIAN_POINT ( 'NONE',  ( -25.39999999999996305, 0.000000000000000000, 0.000000000000000000 ) ) ;
#139471 = AXIS2_PLACEMENT_3D ( 'NONE', #88276, #42647, #96245 ) ;
#139472 = VECTOR ( 'NONE', #91964, 999.9999999999998863 ) ;
#139473 = VECTOR ( 'NONE', #23220, 1000.000000000000000 ) ;
#139474 = DIRECTION ( 'NONE',  ( -0.7071067811865487940, 0.7071067811865463515, 0.000000000000000000 ) ) ;
#139475 = CARTESIAN_POINT ( 'NONE',  ( 43.51626352523143737, -4.472830434245839371, 4.472830434245839371 ) ) ;
#139476 = CARTESIAN_POINT ( 'NONE',  ( 69.18398860626899705, 28.73617430169835529, 5.000000000000000000 ) ) ;
#139477 = VECTOR ( 'NONE', #51868, 999.9999999999998863 ) ;
#139478 = VECTOR ( 'NONE', #25396, 1000.000000000000000 ) ;
#139479 = VERTEX_POINT ( 'NONE', #13000 ) ;
#139480 = CARTESIAN_POINT ( 'NONE',  ( 24.29974487139158867, -27.71228299555223273, 4.000000000000000000 ) ) ;
#139481 = EDGE_LOOP ( 'NONE', ( #5148, #17514, #124464, #49477, #53546 ) ) ;
#139482 = EDGE_CURVE ( 'NONE', #74762, #64647, #101449, .T. ) ;
#139483 = ORIENTED_EDGE ( 'NONE', *, *, #26518, .T. ) ;
#139484 = VECTOR ( 'NONE', #91529, 1000.000000000000000 ) ;
#139485 = VECTOR ( 'NONE', #73495, 1000.000000000000227 ) ;
#139486 = PLANE ( 'NONE',  #121814 ) ;
#139487 = EDGE_CURVE ( 'NONE', #70593, #119701, #135532, .T. ) ;
#139488 = LINE ( 'NONE', #138744, #131951 ) ;
#139489 = DIRECTION ( 'NONE',  ( -0.7071067811865486830, -0.7071067811865464625, 0.000000000000000000 ) ) ;
#139490 = DIRECTION ( 'NONE',  ( -0.7071067811865486830, -0.7071067811865464625, 0.000000000000000000 ) ) ;
#139491 = CARTESIAN_POINT ( 'NONE',  ( -32.99999999999976552, -22.22500000000000142, 4.412002311790046427 ) ) ;
#139492 = CARTESIAN_POINT ( 'NONE',  ( -25.39999999999996305, 0.000000000000000000, 0.000000000000000000 ) ) ;
#139493 = ORIENTED_EDGE ( 'NONE', *, *, #127569, .T. ) ;
#139494 = CARTESIAN_POINT ( 'NONE',  ( 1.886621248228312897, 1.817244688922907692, -5.954744489827652032 ) ) ;
#139495 = CARTESIAN_POINT ( 'NONE',  ( 1.629999999999999893, -0.3999999999999997446, -2.500000000000000000 ) ) ;
#139496 = DIRECTION ( 'NONE',  ( 0.7071067811865486830, -0.7071067811865464625, -0.000000000000000000 ) ) ;
#139497 = LINE ( 'NONE', #126422, #11449 ) ;
#139498 = FACE_OUTER_BOUND ( 'NONE', #134995, .T. ) ;
#139499 = ADVANCED_FACE ( 'NONE', ( #26749 ), #70999, .T. ) ;
#139500 = LINE ( 'NONE', #29965, #124442 ) ;
#139501 = CARTESIAN_POINT ( 'NONE',  ( 67.16252705046288440, 7.949999999999998401, 1.460391307983218338E-15 ) ) ;
#139502 = DIRECTION ( 'NONE',  ( 0.3543493200069162685, -0.000000000000000000, -0.9351131265310288487 ) ) ;
#139503 = VERTEX_POINT ( 'NONE', #137677 ) ;
#139504 = ORIENTED_EDGE ( 'NONE', *, *, #79802, .F. ) ;
#139505 = CARTESIAN_POINT ( 'NONE',  ( 54.66666666666667140, 6.884901960086285300, 3.975000000000003642 ) ) ;
#139506 = DIRECTION ( 'NONE',  ( -0.000000000000000000, 0.000000000000000000, 1.000000000000000000 ) ) ;
#139507 = ADVANCED_FACE ( 'NONE', ( #26049 ), #28900, .F. ) ;
#139508 = CARTESIAN_POINT ( 'NONE',  ( -34.92500000000001137, -22.22500000000000142, 4.000000000000000000 ) ) ;
#139509 = DIRECTION ( 'NONE',  ( 0.000000000000000000, 1.000000000000000000, 6.938893903907228378E-15 ) ) ;
#139510 = ORIENTED_EDGE ( 'NONE', *, *, #33742, .T. ) ;
#139511 = PLANE ( 'NONE',  #69952 ) ;
#139512 = CARTESIAN_POINT ( 'NONE',  ( 60.08376352523143993, -6.110000000000001208, -3.741295971395164515E-16 ) ) ;
#139513 = AXIS2_PLACEMENT_3D ( 'NONE', #6166, #138884, #96056 ) ;
#139514 = ORIENTED_EDGE ( 'NONE', *, *, #122719, .F. ) ;
#139515 = LINE ( 'NONE', #94520, #24825 ) ;
#139516 = ORIENTED_EDGE ( 'NONE', *, *, #20646, .T. ) ;
#139517 = ORIENTED_EDGE ( 'NONE', *, *, #123057, .T. ) ;
#139518 = VECTOR ( 'NONE', #28931, 1000.000000000000000 ) ;
#139519 = DIRECTION ( 'NONE',  ( -0.5735764363510501562, 0.8191520442889890230, 1.003171929053521419E-16 ) ) ;
#139520 = CARTESIAN_POINT ( 'NONE',  ( -12.32816939922344979, -0.7407075233842701500, 4.000000000000000000 ) ) ;
#139521 = LINE ( 'NONE', #130040, #62904 ) ;
#139522 = CARTESIAN_POINT ( 'NONE',  ( 152.4000000000000057, 25.96999999999993847, -33.92499999999998295 ) ) ;
#139523 = ADVANCED_FACE ( 'NONE', ( #127490 ), #62252, .F. ) ;
#139524 = LINE ( 'NONE', #6068, #95172 ) ;
#139527 = ADVANCED_FACE ( 'NONE', ( #72446 ), #117304, .F. ) ;
#139526 = ORIENTED_EDGE ( 'NONE', *, *, #107764, .T. ) ;
#139525 = CARTESIAN_POINT ( 'NONE',  ( 99.68336038379621300, -2.130196079827426203, 7.949999999999996625 ) ) ;
#139528 = LINE ( 'NONE', #16238, #64570 ) ;
#139529 = EDGE_CURVE ( 'NONE', #13042, #70498, #103578, .T. ) ;
#139530 = CARTESIAN_POINT ( 'NONE',  ( -29.58838509405148187, 22.22499999999999787, 4.777194822843818578 ) ) ;
#139531 = PLANE ( 'NONE',  #56363 ) ;
#139532 = CARTESIAN_POINT ( 'NONE',  ( 62.99451991528749772, 28.92564299267982264, 4.000000000000000000 ) ) ;
#139533 = VERTEX_POINT ( 'NONE', #60118 ) ;
#139534 = VERTEX_POINT ( 'NONE', #38351 ) ;
#139535 =( BOUNDED_CURVE ( )  B_SPLINE_CURVE ( 3, ( #95501, #73763, #38994, #115795 ),
 .UNSPECIFIED., .F., .T. ) 
 B_SPLINE_CURVE_WITH_KNOTS ( ( 4, 4 ),
 ( 5.005968288816727174, 5.074607125596344304 ),
 .UNSPECIFIED. ) 
 CURVE ( )  GEOMETRIC_REPRESENTATION_ITEM ( )  RATIONAL_B_SPLINE_CURVE ( ( 1.000000000000000000, 0.9996074310407763175, 0.9996074310407763175, 1.000000000000000000 ) ) 
 REPRESENTATION_ITEM ( '' )  );
#139536 = PRESENTATION_STYLE_ASSIGNMENT (( #6790 ) ) ;
#139537 = CARTESIAN_POINT ( 'NONE',  ( 73.99543019189810877, 5.291415217122916737, 3.055000000000001936 ) ) ;
#139538 = DIRECTION ( 'NONE',  ( -0.000000000000000000, 0.3543493200069153248, 0.9351131265310292928 ) ) ;
#139539 = AXIS2_PLACEMENT_3D ( 'NONE', #35228, #80159, #23603 ) ;
#139540 = CARTESIAN_POINT ( 'NONE',  ( -51.29974487139158867, -27.71228299555242103, 4.000000000000000000 ) ) ;
#139541 = CARTESIAN_POINT ( 'NONE',  ( -36.18398860626899705, 28.73617430169812437, 5.000000000000000000 ) ) ;
#139542 = ORIENTED_EDGE ( 'NONE', *, *, #48825, .T. ) ;
#139543 = ORIENTED_EDGE ( 'NONE', *, *, #41636, .T. ) ;
#139544 = VECTOR ( 'NONE', #95408, 999.9999999999998863 ) ;
#139545 = CARTESIAN_POINT ( 'NONE',  ( 0.000000000000000000, 9.735942053221458872E-16, -7.950000000000000178 ) ) ;
#139546 = ORIENTED_EDGE ( 'NONE', *, *, #39360, .T. ) ;
#139547 = ORIENTED_EDGE ( 'NONE', *, *, #49458, .F. ) ;
#139548 = ADVANCED_FACE ( 'NONE', ( #104284 ), #4949, .F. ) ;
#139549 = ORIENTED_EDGE ( 'NONE', *, *, #81693, .T. ) ;
#139550 = DIRECTION ( 'NONE',  ( 0.000000000000000000, -0.3543493200069153248, 0.9351131265310292928 ) ) ;
#139551 = VECTOR ( 'NONE', #1122, 999.9999999999998863 ) ;
#139552 = FACE_BOUND ( 'NONE', #121875, .T. ) ;
#139553 = ADVANCED_FACE ( 'NONE', ( #93442 ), #81891, .F. ) ;
#139554 = FACE_OUTER_BOUND ( 'NONE', #105745, .T. ) ;
#139555 = DIRECTION ( 'NONE',  ( -1.000000000000000000, 0.000000000000000000, -0.000000000000000000 ) ) ;
#139556 = AXIS2_PLACEMENT_3D ( 'NONE', #138584, #84904, #74037 ) ;
#139557 = DIRECTION ( 'NONE',  ( 0.000000000000000000, 0.000000000000000000, 1.000000000000000000 ) ) ;
#139559 = VERTEX_POINT ( 'NONE', #51373 ) ;
#139558 = CARTESIAN_POINT ( 'NONE',  ( 21.29974487139158512, -27.71228299555221142, 4.000000000000000000 ) ) ;
#139560 = APPLICATION_PROTOCOL_DEFINITION ( 'draft international standard', 'automotive_design', 1998, #72652 ) ;
#139561 = ORIENTED_EDGE ( 'NONE', *, *, #117751, .T. ) ;
#139562 = VERTEX_POINT ( 'NONE', #138372 ) ;
#139563 = CARTESIAN_POINT ( 'NONE',  ( 83.76626352523145158, 4.472830434245838482, -4.472830434245837594 ) ) ;
#139564 = ORIENTED_EDGE ( 'NONE', *, *, #102443, .F. ) ;
#139565 = DIRECTION ( 'NONE',  ( -0.7071067811865487940, 0.7071067811865463515, 0.000000000000000000 ) ) ;
#139566 = DIRECTION ( 'NONE',  ( -0.7071067811865487940, 0.7071067811865463515, 0.000000000000000000 ) ) ;
#139567 = DIRECTION ( 'NONE',  ( 0.7071067811865487940, 0.7071067811865463515, 0.000000000000000000 ) ) ;
#139568 = AXIS2_PLACEMENT_3D ( 'NONE', #72785, #63319, #116938 ) ;
#139569 = VECTOR ( 'NONE', #122016, 1000.000000000000227 ) ;
#139570 = AXIS2_PLACEMENT_3D ( 'NONE', #20283, #117448, #107994 ) ;
#139571 = AXIS2_PLACEMENT_3D ( 'NONE', #43102, #140952, #30801 ) ;
#139572 = LINE ( 'NONE', #95306, #142094 ) ;
#139573 = ORIENTED_EDGE ( 'NONE', *, *, #134041, .T. ) ;
#139574 = DIRECTION ( 'NONE',  ( -1.000000000000000000, -0.000000000000000000, -0.000000000000000000 ) ) ;
#139575 = CARTESIAN_POINT ( 'NONE',  ( -25.39999999999996305, 0.000000000000000000, 2.500000000000000000 ) ) ;
#139576 = DIRECTION ( 'NONE',  ( -0.7071067811865486830, -0.7071067811865464625, -0.000000000000000000 ) ) ;
#139577 = DIRECTION ( 'NONE',  ( -0.6830127018922181881, 0.6830127018922202975, -0.2588190451025214056 ) ) ;
#139578 = CARTESIAN_POINT ( 'NONE',  ( -0.005480084712502889671, 28.92564299267938210, 4.000000000000000000 ) ) ;
#139579 = CARTESIAN_POINT ( 'NONE',  ( -29.99999999999979394, -4.068876922607771895, 4.000000000000000000 ) ) ;
#139580 = VECTOR ( 'NONE', #139056, 1000.000000000000227 ) ;
#139581 = AXIS2_PLACEMENT_3D ( 'NONE', #99133, #143377, #50853 ) ;
#139582 = PRESENTATION_LAYER_ASSIGNMENT (  '', '', ( #44598 ) ) ;
#139583 = CARTESIAN_POINT ( 'NONE',  ( 42.29974487139158157, -27.71228299555235708, 4.000000000000000000 ) ) ;
#139584 = ORIENTED_EDGE ( 'NONE', *, *, #18728, .F. ) ;
#139585 = FACE_OUTER_BOUND ( 'NONE', #90612, .T. ) ;
#139586 = LINE ( 'NONE', #51840, #9528 ) ;
#139587 = ORIENTED_EDGE ( 'NONE', *, *, #133719, .T. ) ;
#139588 = ORIENTED_EDGE ( 'NONE', *, *, #48026, .T. ) ;
#139589 = VERTEX_POINT ( 'NONE', #5686 ) ;
#139590 = CARTESIAN_POINT ( 'NONE',  ( 45.35459685856476142, -1.637169565754161615, 6.110000000000000320 ) ) ;
#139591 = ORIENTED_EDGE ( 'NONE', *, *, #23737, .F. ) ;
#139592 = EDGE_CURVE ( 'NONE', #11459, #11206, #125361, .T. ) ;
#139593 = CIRCLE ( 'NONE', #9883, 2.999999999999990674 ) ;
#139594 = CARTESIAN_POINT ( 'NONE',  ( 12.29580628287044242, -5.278424836066144543, 3.047499999999995879 ) ) ;
#139595 = EDGE_CURVE ( 'NONE', #141889, #47375, #7096, .T. ) ;
#139596 = VERTEX_POINT ( 'NONE', #17295 ) ;
#139597 = ADVANCED_FACE ( 'NONE', ( #27441 ), #6369, .F. ) ;
#139598 = LINE ( 'NONE', #18456, #20263 ) ;
#139600 = ORIENTED_EDGE ( 'NONE', *, *, #106262, .T. ) ;
#139599 = EDGE_CURVE ( 'NONE', #28845, #5408, #48505, .T. ) ;
#139601 = LINE ( 'NONE', #84491, #25607 ) ;
#139602 = DIRECTION ( 'NONE',  ( 0.000000000000000000, 0.000000000000000000, 1.000000000000000000 ) ) ;
#139604 = ORIENTED_EDGE ( 'NONE', *, *, #27374, .F. ) ;
#139603 = CARTESIAN_POINT ( 'NONE',  ( 11.81601139373100651, 28.73617430169779041, 5.000000000000000000 ) ) ;
#139605 = ORIENTED_EDGE ( 'NONE', *, *, #105266, .T. ) ;
#139606 = EDGE_CURVE ( 'NONE', #22337, #21537, #70311, .T. ) ;
#139607 = DIRECTION ( 'NONE',  ( -0.5735764363510507113, 0.8191520442889885789, 1.003171929053520926E-16 ) ) ;
#139608 = VERTEX_POINT ( 'NONE', #39057 ) ;
#139609 = CARTESIAN_POINT ( 'NONE',  ( 33.18398860626899705, 28.73617430169810305, 5.000000000000000000 ) ) ;
#139610 = VERTEX_POINT ( 'NONE', #81152 ) ;
#139611 = ORIENTED_EDGE ( 'NONE', *, *, #47991, .F. ) ;
#139612 = VECTOR ( 'NONE', #46754, 1000.000000000000000 ) ;
#139613 = VERTEX_POINT ( 'NONE', #61559 ) ;
#139614 = EDGE_CURVE ( 'NONE', #93248, #87033, #80905, .T. ) ;
#139615 = ORIENTED_EDGE ( 'NONE', *, *, #132469, .T. ) ;
#139616 = CARTESIAN_POINT ( 'NONE',  ( -25.49999999999982236, -10.53360074219763298, 5.000000000000000000 ) ) ;
#139617 = AXIS2_PLACEMENT_3D ( 'NONE', #117864, #141073, #52638 ) ;
#139618 = CARTESIAN_POINT ( 'NONE',  ( 27.32816939922334143, 5.259292476615661904, 4.000000000000000000 ) ) ;
#139619 = EDGE_CURVE ( 'NONE', #967, #105072, #128222, .T. ) ;
#139620 = DIRECTION ( 'NONE',  ( 1.000000000000000000, 0.000000000000000000, 0.000000000000000000 ) ) ;
#139621 = CARTESIAN_POINT ( 'NONE',  ( 23.99999999999982592, 8.587461875839158765, 4.000000000000000000 ) ) ;
#139622 = EDGE_CURVE ( 'NONE', #17540, #20222, #9120, .T. ) ;
#139623 = ORIENTED_EDGE ( 'NONE', *, *, #17777, .F. ) ;
#139624 = CARTESIAN_POINT ( 'NONE',  ( -21.29974487139158512, -27.71228299555221142, 4.000000000000000000 ) ) ;
#139625 = ORIENTED_EDGE ( 'NONE', *, *, #66331, .T. ) ;
#139626 = CARTESIAN_POINT ( 'NONE',  ( -15.18398860626900237, 28.73617430169797871, 5.000000000000000000 ) ) ;
#139627 = EDGE_CURVE ( 'NONE', #132130, #130144, #84704, .T. ) ;
#139628 = VECTOR ( 'NONE', #21020, 999.9999999999998863 ) ;
#139629 = CARTESIAN_POINT ( 'NONE',  ( 33.08290314143522437, 3.967499999999992699, -6.871911579029513994 ) ) ;
#139630 = DIRECTION ( 'NONE',  ( 0.7071067811865486830, -0.7071067811865464625, -0.000000000000000000 ) ) ;
#139631 = ORIENTED_EDGE ( 'NONE', *, *, #111734, .F. ) ;
#139632 = CARTESIAN_POINT ( 'NONE',  ( 4.658131166821905644, 0.000000000000000000, 2.500000000000000444 ) ) ;
#139633 = DIRECTION ( 'NONE',  ( -0.000000000000000000, 0.000000000000000000, 1.000000000000000000 ) ) ;
#139634 = ORIENTED_EDGE ( 'NONE', *, *, #89533, .F. ) ;
#139635 = ORIENTED_EDGE ( 'NONE', *, *, #117727, .T. ) ;
#139636 = VECTOR ( 'NONE', #79295, 1000.000000000000227 ) ;
#139637 = ORIENTED_EDGE ( 'NONE', *, *, #22162, .T. ) ;
#139638 = PLANE ( 'NONE',  #46402 ) ;
#139639 = PLANE ( 'NONE',  #4754 ) ;
#139640 = CARTESIAN_POINT ( 'NONE',  ( 0.000000000000000000, 0.000000000000000000, 5.000000000000000000 ) ) ;
#139641 = VECTOR ( 'NONE', #79791, 1000.000000000000000 ) ;
#139642 = CARTESIAN_POINT ( 'NONE',  ( 12.72281430457050710, -21.72500000000000142, 5.000000000000000000 ) ) ;
#139643 = CARTESIAN_POINT ( 'NONE',  ( 45.18398860626900415, 28.73617430169818832, 5.000000000000000000 ) ) ;
#139644 = CARTESIAN_POINT ( 'NONE',  ( 72.53709685856478018, -3.054999999999999272, -5.291415217122919401 ) ) ;
#139645 = LINE ( 'NONE', #85207, #76599 ) ;
#139646 = CARTESIAN_POINT ( 'NONE',  ( 4.362461875838996583, 22.22500000000000142, 4.000000000000000000 ) ) ;
#139647 = CARTESIAN_POINT ( 'NONE',  ( -7.060677813783901691, -39.92999999999999972, 19.30339710675713150 ) ) ;
#139648 = CARTESIAN_POINT ( 'NONE',  ( 63.48921356237309510, -27.52281430457099631, 5.000000000000000000 ) ) ;
#139649 = LINE ( 'NONE', #137482, #78963 ) ;
#139650 = EDGE_CURVE ( 'NONE', #106359, #61904, #109306, .T. ) ;
#139651 = ORIENTED_EDGE ( 'NONE', *, *, #33706, .T. ) ;
#139652 = AXIS2_PLACEMENT_3D ( 'NONE', #46106, #69277, #13417 ) ;
#139653 = CARTESIAN_POINT ( 'NONE',  ( -12.20000000000000817, -1.670812611072399357E-15, -39.50000000000000000 ) ) ;
#139654 = VERTEX_POINT ( 'NONE', #85395 ) ;
#139655 = LINE ( 'NONE', #28733, #11331 ) ;
#139657 = ORIENTED_EDGE ( 'NONE', *, *, #104694, .T. ) ;
#139656 = CARTESIAN_POINT ( 'NONE',  ( 8.994519915287490619, 28.92564299267944250, 4.000000000000000000 ) ) ;
#139658 = CARTESIAN_POINT ( 'NONE',  ( 26.58838509405149964, 22.22500000000000497, 4.777194822843814137 ) ) ;
#139659 = DIRECTION ( 'NONE',  ( 0.7071067811865486830, -0.7071067811865464625, -0.000000000000000000 ) ) ;
#139660 = VERTEX_POINT ( 'NONE', #42655 ) ;
#139662 = VERTEX_POINT ( 'NONE', #7834 ) ;
#139661 = AXIS2_PLACEMENT_3D ( 'NONE', #138236, #17847, #62839 ) ;
#139663 = SURFACE_STYLE_USAGE ( .BOTH. , #128060 ) ;
#139664 = DIRECTION ( 'NONE',  ( 0.000000000000000000, 0.000000000000000000, -1.000000000000000000 ) ) ;
#139665 = CARTESIAN_POINT ( 'NONE',  ( 39.09667064187382124, -2.240707523384260824, 15.26439735382761498 ) ) ;
#139666 = EDGE_CURVE ( 'NONE', #43833, #330, #52079, .T. ) ;
#139667 = CARTESIAN_POINT ( 'NONE',  ( 95.01669371712955581, 7.950000000000001066, -2.130196079827421318 ) ) ;
#139668 = CARTESIAN_POINT ( 'NONE',  ( -5.576721541936426441, 11.25929247661560950, 17.85071094206586295 ) ) ;
#139669 =( NAMED_UNIT ( * ) SI_UNIT ( $, .STERADIAN. ) SOLID_ANGLE_UNIT ( ) );
#139670 = VERTEX_POINT ( 'NONE', #96253 ) ;
#139671 = CARTESIAN_POINT ( 'NONE',  ( -28.25154412867557951, -11.24070752338417201, 10.39518518046015849 ) ) ;
#139672 = ADVANCED_FACE ( 'NONE', ( #64379 ), #128911, .T. ) ;
#139673 = DIRECTION ( 'NONE',  ( -0.7071067811865486830, -0.7071067811865464625, 0.000000000000000000 ) ) ;
#139674 = CARTESIAN_POINT ( 'NONE',  ( 34.56250000000000000, 4.461849672132300881, 4.461849672132299105 ) ) ;
#139675 = PLANE ( 'NONE',  #76910 ) ;
#139676 = ORIENTED_EDGE ( 'NONE', *, *, #18717, .F. ) ;
#139677 = VECTOR ( 'NONE', #86433, 1000.000000000000227 ) ;
#139678 = CARTESIAN_POINT ( 'NONE',  ( 22.49999999999984368, -1.695981523266237634, 4.571483868317931964 ) ) ;
#139679 = VERTEX_POINT ( 'NONE', #97714 ) ;
#139680 = EDGE_CURVE ( 'NONE', #121606, #127483, #108550, .T. ) ;
#139681 = CARTESIAN_POINT ( 'NONE',  ( 88.22959685856474721, -6.110000000000000320, -1.637169565754161393 ) ) ;
#139682 = CARTESIAN_POINT ( 'NONE',  ( 14.68342038867201360, -6.740707523384212863, 11.88629033278120950 ) ) ;
#139684 = DIRECTION ( 'NONE',  ( -0.7071067811865486830, -0.7071067811865464625, -0.000000000000000000 ) ) ;
#139683 = AXIS2_PLACEMENT_3D ( 'NONE', #58970, #103123, #122726 ) ;
#139685 = AXIS2_PLACEMENT_3D ( 'NONE', #79489, #135273, #122201 ) ;
#139686 = CARTESIAN_POINT ( 'NONE',  ( -34.92500000000001137, -22.22500000000000142, 4.500000000000000888 ) ) ;
#139687 = ORIENTED_EDGE ( 'NONE', *, *, #112470, .F. ) ;
#139688 = DIRECTION ( 'NONE',  ( -1.000000000000000000, 0.000000000000000000, 0.000000000000000000 ) ) ;
#139689 = AXIS2_PLACEMENT_3D ( 'NONE', #27750, #60419, #36495 ) ;
#139690 = LINE ( 'NONE', #15000, #41880 ) ;
#139691 = DIRECTION ( 'NONE',  ( 0.000000000000000000, 0.000000000000000000, -1.000000000000000000 ) ) ;
#139692 = EDGE_CURVE ( 'NONE', #99513, #10686, #107851, .T. ) ;
#139695 = EDGE_CURVE ( 'NONE', #8484, #14445, #73706, .T. ) ;
#139694 = VERTEX_POINT ( 'NONE', #86137 ) ;
#139693 = CARTESIAN_POINT ( 'NONE',  ( 45.29974487139158867, -27.71228299555237840, 4.000000000000000000 ) ) ;
#139696 = DIRECTION ( 'NONE',  ( 0.3543493200069163240, 0.000000000000000000, 0.9351131265310288487 ) ) ;
#139697 = FACE_OUTER_BOUND ( 'NONE', #57970, .T. ) ;
#139698 = CARTESIAN_POINT ( 'NONE',  ( 1.381925232626255884, -0.1896660010837854515, 6.713074767373758966 ) ) ;
#139699 = EDGE_LOOP ( 'NONE', ( #80672, #27312, #127508, #73696 ) ) ;
#139700 = VERTEX_POINT ( 'NONE', #8517 ) ;
#139701 = CARTESIAN_POINT ( 'NONE',  ( 72.77126352523144703, 4.472830434245839371, 4.472830434245842035 ) ) ;
#139702 = VECTOR ( 'NONE', #95201, 1000.000000000000000 ) ;
#139703 = EDGE_LOOP ( 'NONE', ( #73433, #126167, #138738, #98584 ) ) ;
#139704 = LINE ( 'NONE', #107029, #36426 ) ;
#139705 = LINE ( 'NONE', #16433, #22286 ) ;
#139706 = EDGE_LOOP ( 'NONE', ( #114778, #33524, #36148, #96951 ) ) ;
#139707 = DIRECTION ( 'NONE',  ( 0.7071067811865487940, 0.7071067811865463515, 0.000000000000000000 ) ) ;
#139708 = CARTESIAN_POINT ( 'NONE',  ( 34.92499999999998295, -14.66188269655938825, 18.97781875781096161 ) ) ;
#139709 = VECTOR ( 'NONE', #138148, 1000.000000000000000 ) ;
#139710 = VERTEX_POINT ( 'NONE', #107155 ) ;
#139711 = ADVANCED_FACE ( 'NONE', ( #98435 ), #142656, .F. ) ;
#139712 = VECTOR ( 'NONE', #90682, 999.9999999999998863 ) ;
#139713 = DIRECTION ( 'NONE',  ( 0.6830127018922181881, 0.6830127018922202975, -0.2588190451025214056 ) ) ;
#139714 = CARTESIAN_POINT ( 'NONE',  ( 24.55388970886357569, 5.485012786255876627, 4.000000000000000000 ) ) ;
#139715 = CARTESIAN_POINT ( 'NONE',  ( -12.69999999999998153, 0.000000000000000000, 2.500000000000000444 ) ) ;
#139716 = VERTEX_POINT ( 'NONE', #54949 ) ;
#139718 = VERTEX_POINT ( 'NONE', #43349 ) ;
#139717 = CIRCLE ( 'NONE', #114221, 2.500000000000000444 ) ;
#139719 = ADVANCED_FACE ( 'NONE', ( #63691 ), #87560, .F. ) ;
#139720 = ADVANCED_FACE ( 'NONE', ( #117999 ), #130365, .F. ) ;
#139721 = DIRECTION ( 'NONE',  ( -0.7071067811865486830, -0.7071067811865464625, 0.000000000000000000 ) ) ;
#139722 = DIRECTION ( 'NONE',  ( -0.7071067811865486830, -0.7071067811865464625, 0.000000000000000000 ) ) ;
#139723 = CARTESIAN_POINT ( 'NONE',  ( -29.18650864602343731, -15.74070752338412049, 8.904080028139009784 ) ) ;
#139724 = DIRECTION ( 'NONE',  ( 0.7071067811865486830, -0.7071067811865464625, -0.000000000000000000 ) ) ;
#139725 = CARTESIAN_POINT ( 'NONE',  ( 52.28752705046288440, 0.000000000000000000, -7.949999999999998401 ) ) ;
#139726 = AXIS2_PLACEMENT_3D ( 'NONE', #36641, #25768, #133139 ) ;
#139727 = PLANE ( 'NONE',  #65118 ) ;
#139728 = SURFACE_SIDE_STYLE ('',( #140406 ) ) ;
#139729 = EDGE_LOOP ( 'NONE', ( #107103, #126682, #114967, #21468, #118052, #109546 ) ) ;
#139730 = VECTOR ( 'NONE', #90364, 1000.000000000000000 ) ;
#139732 = ORIENTED_EDGE ( 'NONE', *, *, #67741, .T. ) ;
#139731 = VECTOR ( 'NONE', #138142, 1000.000000000000000 ) ;
#139733 = ORIENTED_EDGE ( 'NONE', *, *, #130756, .F. ) ;
#139734 = ORIENTED_EDGE ( 'NONE', *, *, #114521, .F. ) ;
#139735 = AXIS2_PLACEMENT_3D ( 'NONE', #68710, #121621, #90443 ) ;
#139736 = CARTESIAN_POINT ( 'NONE',  ( 181.1499999999998067, -47.62213595499959951, 36.92500000000000426 ) ) ;
#139737 = ADVANCED_FACE ( 'NONE', ( #33907 ), #69393, .T. ) ;
#139738 = CARTESIAN_POINT ( 'NONE',  ( -9.328169399223462221, -9.740707523384187994, 4.000000000000000000 ) ) ;
#139739 = ORIENTED_EDGE ( 'NONE', *, *, #99190, .T. ) ;
#139740 = DIRECTION ( 'NONE',  ( 0.000000000000000000, 0.000000000000000000, -1.000000000000000000 ) ) ;
#139741 = CARTESIAN_POINT ( 'NONE',  ( 48.48921356237309510, -27.52281430457089328, 5.000000000000000000 ) ) ;
#139742 = DIRECTION ( 'NONE',  ( 0.000000000000000000, 1.000000000000000000, 0.000000000000000000 ) ) ;
#139743 = AXIS2_PLACEMENT_3D ( 'NONE', #135261, #58440, #136643 ) ;
#139744 = LINE ( 'NONE', #104192, #32918 ) ;
#139745 = ORIENTED_EDGE ( 'NONE', *, *, #78473, .T. ) ;
#139746 = CARTESIAN_POINT ( 'NONE',  ( 50.29166666666666430, 3.975000000000003642, -6.884901960086285300 ) ) ;
#139747 = ORIENTED_EDGE ( 'NONE', *, *, #124875, .T. ) ;
#139748 = CARTESIAN_POINT ( 'NONE',  ( -18.18398860626898994, 28.73617430169800002, 5.000000000000000000 ) ) ;
#139749 = VERTEX_POINT ( 'NONE', #56408 ) ;
#139750 = CARTESIAN_POINT ( 'NONE',  ( -72.48921356237309510, -27.52281430457106026, 5.000000000000000000 ) ) ;
#139751 = VERTEX_POINT ( 'NONE', #99860 ) ;
#139752 = VECTOR ( 'NONE', #81572, 1000.000000000000000 ) ;
#139753 = CARTESIAN_POINT ( 'NONE',  ( 75.10459685856476142, 1.637169565754164946, -6.109999999999999432 ) ) ;
#139754 = ORIENTED_EDGE ( 'NONE', *, *, #63442, .T. ) ;
#139755 = ORIENTED_EDGE ( 'NONE', *, *, #86896, .T. ) ;
#139756 = CARTESIAN_POINT ( 'NONE',  ( -33.29974487139158867, -27.71228299555229313, 4.000000000000000000 ) ) ;
#139757 = ADVANCED_FACE ( 'NONE', ( #122300 ), #89008, .T. ) ;
#139758 = VECTOR ( 'NONE', #98377, 1000.000000000000000 ) ;
#139759 = CARTESIAN_POINT ( 'NONE',  ( -12.69999999999998153, 3.061616997868383634E-16, -2.500000000000000444 ) ) ;
#139760 = CARTESIAN_POINT ( 'NONE',  ( 112.0004301918981042, -3.055000000000002380, 5.291415217122920289 ) ) ;
#139761 = CARTESIAN_POINT ( 'NONE',  ( 44.99451991528749772, 28.92564299267969474, 4.000000000000000000 ) ) ;
#139762 = EDGE_CURVE ( 'NONE', #4396, #137207, #78623, .T. ) ;
#139763 = LINE ( 'NONE', #40445, #7340 ) ;
#139764 = CARTESIAN_POINT ( 'NONE',  ( 20.99999999999985789, 13.93112307739204248, 4.000000000000000000 ) ) ;
#139765 = FACE_OUTER_BOUND ( 'NONE', #124214, .T. ) ;
#139766 = ADVANCED_FACE ( 'NONE', ( #133231 ), #91154, .F. ) ;
#139767 = EDGE_CURVE ( 'NONE', #85083, #10004, #20753, .T. ) ;
#139768 = AXIS2_PLACEMENT_3D ( 'NONE', #137575, #28816, #62161 ) ;
#139769 = CARTESIAN_POINT ( 'NONE',  ( 14.70692117890024697, 2.500000000000000444, 0.000000000000000000 ) ) ;
#139770 = CARTESIAN_POINT ( 'NONE',  ( 77.66252705046289861, 7.949999999999998401, 1.460391307983218338E-15 ) ) ;
#139771 = VERTEX_POINT ( 'NONE', #124470 ) ;
#139772 = CARTESIAN_POINT ( 'NONE',  ( 156.1499999999997783, -52.14999999999999147, -34.92499999999975557 ) ) ;
#139773 = CARTESIAN_POINT ( 'NONE',  ( -66.48921356237309510, -27.52281430457101763, 5.000000000000000000 ) ) ;
#139774 = VERTEX_POINT ( 'NONE', #36057 ) ;
#139775 = ORIENTED_EDGE ( 'NONE', *, *, #95027, .F. ) ;
#139776 = ORIENTED_EDGE ( 'NONE', *, *, #78486, .F. ) ;
#139777 = VERTEX_POINT ( 'NONE', #132533 ) ;
#139778 = DIRECTION ( 'NONE',  ( 0.6830127018922180770, -0.6830127018922204085, -0.2588190451025213501 ) ) ;
#139779 = CARTESIAN_POINT ( 'NONE',  ( 5.816011393731002066, 28.73617430169783304, 5.000000000000000000 ) ) ;
#139780 = ADVANCED_FACE ( 'NONE', ( #25139 ), #78844, .F. ) ;
#139781 = FACE_OUTER_BOUND ( 'NONE', #93341, .T. ) ;
#139782 = EDGE_CURVE ( 'NONE', #121662, #9178, #12829, .T. ) ;
#139783 = DIRECTION ( 'NONE',  ( 0.3543493200069163240, -0.000000000000000000, -0.9351131265310288487 ) ) ;
#139784 = EDGE_LOOP ( 'NONE', ( #10837, #95841, #76466, #10246, #62454, #59632 ) ) ;
#139785 = DIRECTION ( 'NONE',  ( 0.000000000000000000, -1.000000000000000000, 0.000000000000000000 ) ) ;
#139786 = ORIENTED_EDGE ( 'NONE', *, *, #87087, .F. ) ;
#139787 = VECTOR ( 'NONE', #70230, 1000.000000000000000 ) ;
#139788 = ADVANCED_FACE ( 'NONE', ( #1923 ), #46229, .T. ) ;
#139789 = AXIS2_PLACEMENT_3D ( 'NONE', #55842, #98599, #142829 ) ;
#139790 = CARTESIAN_POINT ( 'NONE',  ( 1.582903141435219485, 3.967499999999992699, -6.871911579029513994 ) ) ;
#139791 = DIRECTION ( 'NONE',  ( -0.6830127018922181881, 0.6830127018922202975, -0.2588190451025214056 ) ) ;
#139792 = DIRECTION ( 'NONE',  ( -0.7071067811865486830, 0.7071067811865464625, 0.000000000000000000 ) ) ;
#139793 = CARTESIAN_POINT ( 'NONE',  ( 14.11557571622218532, -9.244271043508256014, 2.203030002273714594 ) ) ;
#139794 = ORIENTED_EDGE ( 'NONE', *, *, #14014, .T. ) ;
#139795 = ORIENTED_EDGE ( 'NONE', *, *, #75742, .T. ) ;
#139796 = ORIENTED_EDGE ( 'NONE', *, *, #55093, .T. ) ;
#139797 = CARTESIAN_POINT ( 'NONE',  ( 15.29974487139158867, -27.71228299555216879, 4.000000000000000000 ) ) ;
#139798 = EDGE_CURVE ( 'NONE', #97591, #26803, #24437, .T. ) ;
#139799 = PLANE ( 'NONE',  #126047 ) ;
#139800 = DIRECTION ( 'NONE',  ( -0.7071067811865486830, 0.7071067811865463515, 0.000000000000000000 ) ) ;
#139801 = AXIS2_PLACEMENT_3D ( 'NONE', #64699, #129215, #85708 ) ;
#139802 = DIRECTION ( 'NONE',  ( -0.7071067811865486830, -0.7071067811865464625, 0.000000000000000000 ) ) ;
#139803 = CARTESIAN_POINT ( 'NONE',  ( -12.69999999999998153, 0.000000000000000000, 0.000000000000000000 ) ) ;
#139804 = LINE ( 'NONE', #73804, #139162 ) ;
#139805 = DIRECTION ( 'NONE',  ( 1.000000000000000000, 0.000000000000000000, 0.000000000000000000 ) ) ;
#139806 = VECTOR ( 'NONE', #63310, 1000.000000000000000 ) ;
#139807 = CARTESIAN_POINT ( 'NONE',  ( 27.70876352523143993, -7.482591942790329030E-16, 6.110000000000001208 ) ) ;
#139808 = CARTESIAN_POINT ( 'NONE',  ( -19.49999999999986500, -1.592773361805389865, -6.492772025301184691 ) ) ;
#139809 = SURFACE_STYLE_USAGE ( .BOTH. , #17956 ) ;
#139810 = VERTEX_POINT ( 'NONE', #13536 ) ;
#139811 = DIRECTION ( 'NONE',  ( 0.7071067811865487940, 0.7071067811865463515, -0.000000000000000000 ) ) ;
#139812 = ADVANCED_FACE ( 'NONE', ( #46967 ), #135375, .F. ) ;
#139813 = DIRECTION ( 'NONE',  ( 0.5735764363510451602, 0.8191520442889924647, 0.000000000000000000 ) ) ;
#139814 = EDGE_LOOP ( 'NONE', ( #56356, #117584, #41941, #57665 ) ) ;
#139815 =( BOUNDED_CURVE ( )  B_SPLINE_CURVE ( 3, ( #127172, #5380, #38053, #71387 ),
 .UNSPECIFIED., .F., .T. ) 
 B_SPLINE_CURVE_WITH_KNOTS ( ( 4, 4 ),
 ( 5.143245962375964986, 6.645403452391247079 ),
 .UNSPECIFIED. ) 
 CURVE ( )  GEOMETRIC_REPRESENTATION_ITEM ( )  RATIONAL_B_SPLINE_CURVE ( ( 1.000000000000000000, 0.8206354192515239454, 0.8206354192515239454, 1.000000000000000000 ) ) 
 REPRESENTATION_ITEM ( '' )  );
#139816 = AXIS2_PLACEMENT_3D ( 'NONE', #30672, #19058, #140817 ) ;
#139817 = CARTESIAN_POINT ( 'NONE',  ( 36.48921356237310221, -27.52281430457080802, 5.000000000000000000 ) ) ;
#139819 = ORIENTED_EDGE ( 'NONE', *, *, #44396, .F. ) ;
#139818 = CARTESIAN_POINT ( 'NONE',  ( -7.828169399223476432, 12.75929247661558996, 4.000000000000000000 ) ) ;
#139820 = CARTESIAN_POINT ( 'NONE',  ( 5.380000000000000782, 9.521314400968980422E-16, 0.000000000000000000 ) ) ;
#139821 = EDGE_CURVE ( 'NONE', #68994, #1274, #59948, .T. ) ;
#139822 = ADVANCED_FACE ( 'NONE', ( #104110 ), #81713, .F. ) ;
#139823 = ORIENTED_EDGE ( 'NONE', *, *, #137527, .F. ) ;
#139824 = DIRECTION ( 'NONE',  ( -0.6830127018922181881, 0.6830127018922202975, -0.2588190451025214056 ) ) ;
#139825 = AXIS2_PLACEMENT_3D ( 'NONE', #27259, #138912, #128044 ) ;
#139826 = ORIENTED_EDGE ( 'NONE', *, *, #35661, .T. ) ;
#139827 = VECTOR ( 'NONE', #19543, 1000.000000000000000 ) ;
#139828 = CARTESIAN_POINT ( 'NONE',  ( -12.20000000000000462, -21.76999999999999247, -40.00000000000000000 ) ) ;
#139829 = EDGE_CURVE ( 'NONE', #112546, #98060, #4773, .T. ) ;
#139830 = CARTESIAN_POINT ( 'NONE',  ( 124.4750270504628844, -5.819803920172572198, 5.819803920172572198 ) ) ;
#139832 = CIRCLE ( 'NONE', #5442, 5.968999999999998529 ) ;
#139831 = DIRECTION ( 'NONE',  ( 0.6830127018922180770, -0.6830127018922204085, -0.2588190451025213501 ) ) ;
#139833 = CARTESIAN_POINT ( 'NONE',  ( 34.92499999999998295, 17.81665438641027777, 4.500000000000000888 ) ) ;
#139834 = DIRECTION ( 'NONE',  ( 0.6830127018922181881, 0.6830127018922202975, -0.2588190451025214056 ) ) ;
#139835 = DIRECTION ( 'NONE',  ( 0.7071067811865487940, 0.7071067811865463515, 0.000000000000000000 ) ) ;
#139836 = LINE ( 'NONE', #116619, #124704 ) ;
#139837 = CARTESIAN_POINT ( 'NONE',  ( 5.979166666666666075, 6.094999999999988205, -1.633150327867694651 ) ) ;
#139838 = CARTESIAN_POINT ( 'NONE',  ( 11.93706980810188512, 2.126176841940952134, -7.934999999999992504 ) ) ;
#139839 = CIRCLE ( 'NONE', #114348, 28.00000000000002487 ) ;
#139840 = PLANE ( 'NONE',  #113818 ) ;
#139841 = DIRECTION ( 'NONE',  ( -0.000000000000000000, 0.3543493200069153248, 0.9351131265310292928 ) ) ;
#139842 = ORIENTED_EDGE ( 'NONE', *, *, #9908, .T. ) ;
#139843 = ORIENTED_EDGE ( 'NONE', *, *, #35640, .T. ) ;
#139844 = CARTESIAN_POINT ( 'NONE',  ( 79.16666666666665719, 6.884901960086285300, 3.975000000000003642 ) ) ;
#139845 = PLANE ( 'NONE',  #4972 ) ;
#139846 = ORIENTED_EDGE ( 'NONE', *, *, #13305, .T. ) ;
#139847 = CARTESIAN_POINT ( 'NONE',  ( 90.78752705046288440, 0.000000000000000000, -7.949999999999998401 ) ) ;
#139848 = DIRECTION ( 'NONE',  ( 0.7071067811865487940, -0.7071067811865463515, 0.000000000000000000 ) ) ;
#139849 = VECTOR ( 'NONE', #102519, 1000.000000000000000 ) ;
#139850 = DIRECTION ( 'NONE',  ( -0.000000000000000000, 0.000000000000000000, 1.000000000000000000 ) ) ;
#139851 = ORIENTED_EDGE ( 'NONE', *, *, #90930, .F. ) ;
#139852 = CARTESIAN_POINT ( 'NONE',  ( -26.99999999999980815, -13.97847968911263017, -0.1324546996127407283 ) ) ;
#139853 = CARTESIAN_POINT ( 'NONE',  ( 55.18164086290596515, -52.14999999999999147, -41.64500000000001023 ) ) ;
#139854 = SURFACE_SIDE_STYLE ('',( #131813 ) ) ;
#139855 = VERTEX_POINT ( 'NONE', #117143 ) ;
#139856 = CYLINDRICAL_SURFACE ( 'NONE', #136921, 0.5000000000000004441 ) ;
#139857 = CARTESIAN_POINT ( 'NONE',  ( -30.18398860626900060, 28.73617430169808173, 5.000000000000000000 ) ) ;
#139858 = DIRECTION ( 'NONE',  ( 1.000000000000000000, 0.000000000000000000, 0.000000000000000000 ) ) ;
#139859 = DIRECTION ( 'NONE',  ( 0.7071067811865487940, -0.7071067811865463515, 0.000000000000000000 ) ) ;
#139860 = DIRECTION ( 'NONE',  ( -0.7071067811865486830, -0.7071067811865464625, -0.000000000000000000 ) ) ;
#139861 = CARTESIAN_POINT ( 'NONE',  ( 56.52198303709688787, -46.44627868284401728, 35.89947574910241457 ) ) ;
#139862 = B_SPLINE_CURVE_WITH_KNOTS ( 'NONE', 3,
 ( #116255, #113380, #16946, #14070, #138735, #127870, #136563, #81517, #61220, #137308, #39430, #102547 ),
 .UNSPECIFIED., .F., .F.,
 ( 4, 2, 2, 2, 2, 4 ),
 ( 0.000000000000000000, 0.001816333612422253588, 0.002724500418633388731, 0.003632667224844524090, 0.005449000837266803482, 0.007265334449689082007 ),
 .UNSPECIFIED. ) ;
#139863 = ORIENTED_EDGE ( 'NONE', *, *, #67548, .T. ) ;
#139864 = VERTEX_POINT ( 'NONE', #125913 ) ;
#139865 = CARTESIAN_POINT ( 'NONE',  ( 101.3545968585647614, -1.637169565754161615, 6.110000000000000320 ) ) ;
#139866 = VECTOR ( 'NONE', #55417, 1000.000000000000227 ) ;
#139867 = ORIENTED_EDGE ( 'NONE', *, *, #103953, .F. ) ;
#139868 = CARTESIAN_POINT ( 'NONE',  ( 21.77612515620402078, 2.500000000000000888, 0.000000000000000000 ) ) ;
#139869 = DIRECTION ( 'NONE',  ( -0.7071067811865486830, -0.7071067811865464625, 0.000000000000000000 ) ) ;
#139870 = ORIENTED_EDGE ( 'NONE', *, *, #127197, .F. ) ;
#139871 = LINE ( 'NONE', #40547, #123168 ) ;
#139873 = TOROIDAL_SURFACE ( 'NONE', #946, 25.00000000000002487, 3.000000000000000000 ) ;
#139872 = DIRECTION ( 'NONE',  ( -0.000000000000000000, 0.3543493200069153248, 0.9351131265310292928 ) ) ;
#139874 = CARTESIAN_POINT ( 'NONE',  ( 99.80793019189812298, -6.109999999999998543, 1.637169565754158063 ) ) ;
#139875 = ORIENTED_EDGE ( 'NONE', *, *, #118068, .F. ) ;
#139876 = CARTESIAN_POINT ( 'NONE',  ( 17.27718569542927796, -21.72500000000000142, 5.000000000000000000 ) ) ;
#139877 = VERTEX_POINT ( 'NONE', #59253 ) ;
#139878 = DIRECTION ( 'NONE',  ( -0.7071067811865486830, -0.7071067811865464625, -0.000000000000000000 ) ) ;
#139879 = CARTESIAN_POINT ( 'NONE',  ( -26.67183060077628198, -12.74070752338415602, 4.000000000000000000 ) ) ;
#139880 = LINE ( 'NONE', #29905, #76337 ) ;
#139881 = ORIENTED_EDGE ( 'NONE', *, *, #59136, .F. ) ;
#139882 = EDGE_LOOP ( 'NONE', ( #140676, #29486, #124197, #15324 ) ) ;
#139883 = EDGE_CURVE ( 'NONE', #38066, #135973, #116452, .T. ) ;
#139884 = VERTEX_POINT ( 'NONE', #38893 ) ;
#139885 = DIRECTION ( 'NONE',  ( -0.7071067811865487940, 0.7071067811865463515, -0.000000000000000000 ) ) ;
#139886 = ADVANCED_FACE ( 'NONE', ( #70829 ), #15659, .F. ) ;
#139887 = CARTESIAN_POINT ( 'NONE',  ( 18.45983838949729261, 18.75929247661552779, 8.305906642995529054 ) ) ;
#139888 = CARTESIAN_POINT ( 'NONE',  ( 12.90040314143521982, -7.934999999999988951, 2.126176841940957907 ) ) ;
#139889 = VECTOR ( 'NONE', #11302, 1000.000000000000000 ) ;
#139890 = CARTESIAN_POINT ( 'NONE',  ( 12.70710678118646619, 14.25929247661557220, 5.000000000000000000 ) ) ;
#139891 = AXIS2_PLACEMENT_3D ( 'NONE', #121958, #32861, #66895 ) ;
#139892 = ORIENTED_EDGE ( 'NONE', *, *, #48773, .F. ) ;
#139894 = VERTEX_POINT ( 'NONE', #48339 ) ;
#139893 = EDGE_CURVE ( 'NONE', #126064, #16024, #83860, .T. ) ;
#139895 = CARTESIAN_POINT ( 'NONE',  ( -42.48921356237308800, -27.52281430457085065, 5.000000000000000000 ) ) ;
#139896 = ORIENTED_EDGE ( 'NONE', *, *, #59276, .F. ) ;
#139897 = ORIENTED_EDGE ( 'NONE', *, *, #131117, .F. ) ;
#139898 = EDGE_CURVE ( 'NONE', #86742, #131471, #47669, .T. ) ;
#139899 = LINE ( 'NONE', #95643, #49493 ) ;
#139900 = ORIENTED_EDGE ( 'NONE', *, *, #114923, .F. ) ;
#139901 = VECTOR ( 'NONE', #26021, 1000.000000000000000 ) ;
#139902 = CARTESIAN_POINT ( 'NONE',  ( 5.700255128608413102, -27.71228299555201957, 4.000000000000000000 ) ) ;
#139903 = AXIS2_PLACEMENT_3D ( 'NONE', #93677, #137189, #84251 ) ;
#139904 = DIRECTION ( 'NONE',  ( 0.7071067811865487940, 0.7071067811865463515, -0.000000000000000000 ) ) ;
#139905 = DIRECTION ( 'NONE',  ( 0.7071067811865486830, -0.7071067811865464625, -0.000000000000000000 ) ) ;
#139906 = EDGE_CURVE ( 'NONE', #64904, #6181, #92529, .T. ) ;
#139907 = PLANE ( 'NONE',  #46708 ) ;
#139908 = EDGE_LOOP ( 'NONE', ( #91825, #56034, #9289, #7927 ) ) ;
#139909 = LINE ( 'NONE', #110092, #34845 ) ;
#139910 = FACE_BOUND ( 'NONE', #116925, .T. ) ;
#139912 = ORIENTED_EDGE ( 'NONE', *, *, #75771, .T. ) ;
#139911 = VECTOR ( 'NONE', #31357, 1000.000000000000114 ) ;
#139913 = CARTESIAN_POINT ( 'NONE',  ( 2.613322195557306049, -2.055000000000000160, 0.000000000000000000 ) ) ;
#139914 = DIRECTION ( 'NONE',  ( 0.000000000000000000, -1.000000000000000000, 0.000000000000000000 ) ) ;
#139915 =( LENGTH_UNIT ( ) NAMED_UNIT ( * ) SI_UNIT ( .MILLI., .METRE. ) );
#139916 = EDGE_LOOP ( 'NONE', ( #123540, #16205, #42294, #79539 ) ) ;
#139917 = LINE ( 'NONE', #40595, #27369 ) ;
#139918 = ORIENTED_EDGE ( 'NONE', *, *, #80690, .F. ) ;
#139919 = ORIENTED_EDGE ( 'NONE', *, *, #113563, .F. ) ;
#139920 = ORIENTED_EDGE ( 'NONE', *, *, #25981, .F. ) ;
#139921 =( GEOMETRIC_REPRESENTATION_CONTEXT ( 3 ) GLOBAL_UNCERTAINTY_ASSIGNED_CONTEXT ( ( #107327 ) ) GLOBAL_UNIT_ASSIGNED_CONTEXT ( ( #65044, #99049, #119375 ) ) REPRESENTATION_CONTEXT ( 'NONE', 'WORKASPACE' ) );
#139922 = CARTESIAN_POINT ( 'NONE',  ( 31.99543019189811233, 5.291415217122916737, 3.055000000000001936 ) ) ;
#139923 = LINE ( 'NONE', #1334, #54461 ) ;
#139924 = AXIS2_PLACEMENT_3D ( 'NONE', #73092, #109792, #105660 ) ;
#139925 = DIRECTION ( 'NONE',  ( -0.000000000000000000, 0.3543493200069153248, 0.9351131265310292928 ) ) ;
#139926 = LINE ( 'NONE', #83388, #114336 ) ;
#139927 = DIRECTION ( 'NONE',  ( -0.7071067811865486830, 0.7071067811865464625, 0.000000000000000000 ) ) ;
#139928 = DIRECTION ( 'NONE',  ( -1.734723475976806848E-16, 1.000000000000000000, 0.000000000000000000 ) ) ;
#139929 = ADVANCED_FACE ( 'NONE', ( #138207 ), #50489, .T. ) ;
#139930 = CARTESIAN_POINT ( 'NONE',  ( 30.18398860626900060, 28.73617430169808173, 5.000000000000000000 ) ) ;
#139931 = CARTESIAN_POINT ( 'NONE',  ( -48.48921356237309510, -27.52281430457089328, 5.000000000000000000 ) ) ;
#139932 = FACE_OUTER_BOUND ( 'NONE', #140339, .T. ) ;
#139933 = EDGE_CURVE ( 'NONE', #105597, #69571, #137648, .T. ) ;
#139934 = EDGE_CURVE ( 'NONE', #92161, #71721, #6212, .T. ) ;
#139935 = DIRECTION ( 'NONE',  ( -0.7071067811865486830, -0.7071067811865464625, 0.000000000000000000 ) ) ;
#139936 = CARTESIAN_POINT ( 'NONE',  ( -16.49999999999988987, 16.18958161055400780, -11.56426086740815151 ) ) ;
#139937 = CARTESIAN_POINT ( 'NONE',  ( 10.37176554955608943, -8.240707523384196875, 11.38925528200750215 ) ) ;
#139938 = VERTEX_POINT ( 'NONE', #39633 ) ;
#139939 = EDGE_LOOP ( 'NONE', ( #87903, #64764, #127240, #75112 ) ) ;
#139940 = ORIENTED_EDGE ( 'NONE', *, *, #51179, .F. ) ;
#139941 = ORIENTED_EDGE ( 'NONE', *, *, #66692, .T. ) ;
#139942 = CYLINDRICAL_SURFACE ( 'NONE', #30957, 1.320799999999990870 ) ;
#139943 = ORIENTED_EDGE ( 'NONE', *, *, #59863, .F. ) ;
#139944 = ADVANCED_FACE ( 'NONE', ( #28746 ), #72989, .F. ) ;
#139945 = ORIENTED_EDGE ( 'NONE', *, *, #68920, .F. ) ;
#139946 = LINE ( 'NONE', #53638, #86187 ) ;
#139947 = CARTESIAN_POINT ( 'NONE',  ( 22.53999999999999915, -2.055000000000000160, 2.789133085058098087E-16 ) ) ;
#139948 = ADVANCED_FACE ( 'NONE', ( #70140 ), #53324, .F. ) ;
#139949 = EDGE_CURVE ( 'NONE', #92353, #133121, #106252, .T. ) ;
#139950 = DIRECTION ( 'NONE',  ( -0.7071067811865486830, -0.7071067811865464625, 0.000000000000000000 ) ) ;
#139951 = ORIENTED_EDGE ( 'NONE', *, *, #2977, .F. ) ;
#139952 = CARTESIAN_POINT ( 'NONE',  ( -48.48921356237309510, -27.52281430457089328, 5.000000000000000000 ) ) ;
#139953 = VERTEX_POINT ( 'NONE', #41032 ) ;
#139954 = LINE ( 'NONE', #61680, #113864 ) ;
#139955 = DIRECTION ( 'NONE',  ( -0.000000000000000000, -0.000000000000000000, 1.000000000000000000 ) ) ;
#139956 = CARTESIAN_POINT ( 'NONE',  ( 10.56706980810188945, 2.126176841940952134, -7.934999999999993392 ) ) ;
#139957 = ORIENTED_EDGE ( 'NONE', *, *, #9258, .T. ) ;
#139958 = CARTESIAN_POINT ( 'NONE',  ( 90.62043019189810877, 3.055000000000002380, -5.291415217122917625 ) ) ;
#139959 = ADVANCED_FACE ( 'NONE', ( #20696 ), #85235, .F. ) ;
#139960 = CARTESIAN_POINT ( 'NONE',  ( -54.18398860626899705, 28.73617430169825226, 5.000000000000000000 ) ) ;
#139961 = DIRECTION ( 'NONE',  ( 0.5735764363510448272, -0.8191520442889927978, 1.003171929053526103E-16 ) ) ;
#139962 = LINE ( 'NONE', #115279, #136840 ) ;
#139963 = ORIENTED_EDGE ( 'NONE', *, *, #13968, .T. ) ;
#139964 = ORIENTED_EDGE ( 'NONE', *, *, #49954, .T. ) ;
#139965 = LINE ( 'NONE', #9380, #88901 ) ;
#139966 = VERTEX_POINT ( 'NONE', #62094 ) ;
#139967 = CARTESIAN_POINT ( 'NONE',  ( -15.79289321881334551, -8.240707523384191546, 5.000000000000000000 ) ) ;
#139968 = DIRECTION ( 'NONE',  ( -0.3543493200069162685, -0.000000000000000000, -0.9351131265310288487 ) ) ;
#139969 = EDGE_CURVE ( 'NONE', #140092, #128013, #120377, .T. ) ;
#139970 = FACE_OUTER_BOUND ( 'NONE', #90668, .T. ) ;
#139971 = CARTESIAN_POINT ( 'NONE',  ( 181.1500000013235478, -47.86718710719702585, -37.19897551713905415 ) ) ;
#139973 = ORIENTED_EDGE ( 'NONE', *, *, #62518, .F. ) ;
#139972 = VECTOR ( 'NONE', #73932, 1000.000000000000000 ) ;
#139974 = CARTESIAN_POINT ( 'NONE',  ( 18.63425672184678916, 2.500000000000000444, 0.000000000000000000 ) ) ;
#139975 = DIRECTION ( 'NONE',  ( -0.000000000000000000, -0.3543493200069152693, 0.9351131265310292928 ) ) ;
#139976 = DIRECTION ( 'NONE',  ( 2.781805975412905274E-17, -0.3543493200069152138, 0.9351131265310292928 ) ) ;
#139977 = EDGE_LOOP ( 'NONE', ( #3798, #129770, #125131, #122587 ) ) ;
#139978 = CARTESIAN_POINT ( 'NONE',  ( -12.69999999999998153, 0.000000000000000000, 2.500000000000000444 ) ) ;
#139979 = DIRECTION ( 'NONE',  ( -0.5735764363510503783, -0.8191520442889886899, 0.000000000000000000 ) ) ;
#139980 = ORIENTED_EDGE ( 'NONE', *, *, #119303, .F. ) ;
#139982 = VERTEX_POINT ( 'NONE', #129458 ) ;
#139981 = LINE ( 'NONE', #65282, #41769 ) ;
#139983 = VERTEX_POINT ( 'NONE', #7671 ) ;
#139984 = DIRECTION ( 'NONE',  ( 0.7071067811865487940, 0.7071067811865463515, -0.000000000000000000 ) ) ;
#139986 = EDGE_CURVE ( 'NONE', #96522, #26845, #130200, .T. ) ;
#139985 = LINE ( 'NONE', #40660, #133999 ) ;
#139987 = AXIS2_PLACEMENT_3D ( 'NONE', #102489, #28491, #48097 ) ;
#139988 = VERTEX_POINT ( 'NONE', #85965 ) ;
#139989 = DIRECTION ( 'NONE',  ( 0.3543493200069162685, -0.000000000000000000, -0.9351131265310288487 ) ) ;
#139990 = EDGE_CURVE ( 'NONE', #78734, #85083, #141795, .T. ) ;
#139991 = CARTESIAN_POINT ( 'NONE',  ( 5.281315875828549444, -9.629649721936179265E-32, 2.500000000000000444 ) ) ;
#139992 = EDGE_CURVE ( 'NONE', #44425, #43477, #62810, .T. ) ;
#139993 = AXIS2_PLACEMENT_3D ( 'NONE', #61584, #108577, #41951 ) ;
#139994 = DIRECTION ( 'NONE',  ( -0.7071067811865486830, -0.7071067811865464625, -0.000000000000000000 ) ) ;
#139996 = CARTESIAN_POINT ( 'NONE',  ( 31.33333333333332504, -6.884901960086287964, 3.974999999999998312 ) ) ;
#139995 = AXIS2_PLACEMENT_3D ( 'NONE', #126423, #69222, #60501 ) ;
#139997 = DIRECTION ( 'NONE',  ( 0.7071067811865487940, -0.7071067811865463515, 0.000000000000000000 ) ) ;
#139998 = DIRECTION ( 'NONE',  ( 0.6830127018922181881, 0.6830127018922202975, -0.2588190451025214056 ) ) ;
#139999 = DIRECTION ( 'NONE',  ( -0.6830127018922180770, -0.6830127018922204085, -0.2588190451025213501 ) ) ;
#140000 = LINE ( 'NONE', #84202, #58350 ) ;
#140001 = CARTESIAN_POINT ( 'NONE',  ( 0.000000000000000000, 0.000000000000000000, 5.000000000000000000 ) ) ;
#140002 = DIRECTION ( 'NONE',  ( -1.000000000000000000, -1.224606353822377258E-16, -0.000000000000000000 ) ) ;
#140003 = ORIENTED_EDGE ( 'NONE', *, *, #42781, .T. ) ;
#140004 = EDGE_LOOP ( 'NONE', ( #137168, #129329, #103149, #48849 ) ) ;
#140005 = ORIENTED_EDGE ( 'NONE', *, *, #102774, .F. ) ;
#140006 = CARTESIAN_POINT ( 'NONE',  ( 110.3750000000000000, 7.950000000000000178, 1.460391307983218535E-15 ) ) ;
#140007 = EDGE_LOOP ( 'NONE', ( #11421, #77630, #51647, #55323 ) ) ;
#140008 = AXIS2_PLACEMENT_3D ( 'NONE', #51899, #96761, #95374 ) ;
#140009 = ORIENTED_EDGE ( 'NONE', *, *, #58177, .T. ) ;
#140010 = ORIENTED_EDGE ( 'NONE', *, *, #55768, .F. ) ;
#140011 = CARTESIAN_POINT ( 'NONE',  ( 48.29974487139158867, -27.71228299555239971, 4.000000000000000000 ) ) ;
#140012 = CARTESIAN_POINT ( 'NONE',  ( -13.17183060077638324, -8.240707523384200428, 4.000000000000000000 ) ) ;
#140013 = ORIENTED_EDGE ( 'NONE', *, *, #38428, .T. ) ;
#140014 = CARTESIAN_POINT ( 'NONE',  ( 33.18398860626899705, 28.73617430169810305, 5.000000000000000000 ) ) ;
#140015 = CARTESIAN_POINT ( 'NONE',  ( -9.489213562373095101, -27.52281430457062328, 5.000000000000000000 ) ) ;
#140016 = CARTESIAN_POINT ( 'NONE',  ( -5.816011393731002066, 28.73617430169783304, 5.000000000000000000 ) ) ;
#140017 = DIRECTION ( 'NONE',  ( 0.3543493200069162685, -0.000000000000000000, -0.9351131265310288487 ) ) ;
#140018 = CARTESIAN_POINT ( 'NONE',  ( 101.5004301918981042, -3.055000000000002380, 5.291415217122920289 ) ) ;
#140019 = ORIENTED_EDGE ( 'NONE', *, *, #90832, .F. ) ;
#140020 = CARTESIAN_POINT ( 'NONE',  ( 22.49999999999984723, -16.53360074219757081, 5.000000000000000000 ) ) ;
#140021 = DIRECTION ( 'NONE',  ( -0.3543493200069162685, -0.000000000000000000, -0.9351131265310288487 ) ) ;
#140022 = DIRECTION ( 'NONE',  ( -0.000000000000000000, -0.3543493200069152693, 0.9351131265310292928 ) ) ;
#140023 = DIRECTION ( 'NONE',  ( 0.7071067811865487940, 0.7071067811865463515, -0.000000000000000000 ) ) ;
#140024 = CARTESIAN_POINT ( 'NONE',  ( -12.79289321881336861, -8.240707523384198652, 5.000000000000000000 ) ) ;
#140025 = FACE_OUTER_BOUND ( 'NONE', #108614, .T. ) ;
#140026 = DIRECTION ( 'NONE',  ( -1.000000000000000000, -1.224606353822377258E-16, -0.000000000000000000 ) ) ;
#140027 = DIRECTION ( 'NONE',  ( 0.3543493200069162685, -0.000000000000000000, -0.9351131265310288487 ) ) ;
#140028 = VECTOR ( 'NONE', #44134, 1000.000000000000227 ) ;
#140029 =( NAMED_UNIT ( * ) PLANE_ANGLE_UNIT ( ) SI_UNIT ( $, .RADIAN. ) );
#140030 = ORIENTED_EDGE ( 'NONE', *, *, #41528, .F. ) ;
#140031 = ORIENTED_EDGE ( 'NONE', *, *, #2054, .F. ) ;
#140032 = VECTOR ( 'NONE', #21004, 1000.000000000000000 ) ;
#140033 = CARTESIAN_POINT ( 'NONE',  ( 29.14583333333332504, 2.130196079827431976, -7.949999999999999289 ) ) ;
#140034 = ORIENTED_EDGE ( 'NONE', *, *, #5824, .T. ) ;
#140035 = AXIS2_PLACEMENT_3D ( 'NONE', #54904, #110654, #99814 ) ;
#140036 = DIRECTION ( 'NONE',  ( -0.000000000000000000, 0.3543493200069153248, 0.9351131265310292928 ) ) ;
#140037 = DIRECTION ( 'NONE',  ( 0.7071067811865486830, -0.7071067811865464625, -0.000000000000000000 ) ) ;
#140038 = CARTESIAN_POINT ( 'NONE',  ( 34.92499999999998295, -19.19990548397263552, 4.759050581649326261 ) ) ;
#140039 = PLANE ( 'NONE',  #118633 ) ;
#140040 = DIRECTION ( 'NONE',  ( 0.000000000000000000, 1.000000000000000000, 1.286409696682840916E-16 ) ) ;
#140041 = SURFACE_STYLE_USAGE ( .BOTH. , #7336 ) ;
#140042 = CARTESIAN_POINT ( 'NONE',  ( 122.4120968585647802, 5.291415217122921177, -3.054999999999994831 ) ) ;
#140043 = EDGE_LOOP ( 'NONE', ( #92092, #108286, #23877, #94491, #88381 ) ) ;
#140044 = CARTESIAN_POINT ( 'NONE',  ( 23.99451991528749062, 28.92564299267954908, 4.000000000000000000 ) ) ;
#140045 = ORIENTED_EDGE ( 'NONE', *, *, #128014, .T. ) ;
#140046 = CARTESIAN_POINT ( 'NONE',  ( 9.995075227787999950, -5.240707523384225297, 12.38332538355493817 ) ) ;
#140047 = DIRECTION ( 'NONE',  ( 0.7071067811865486830, -0.7071067811865464625, -0.000000000000000000 ) ) ;
#140048 = CARTESIAN_POINT ( 'NONE',  ( 17.53719725875415847, 4.202752102959690472E-16, 0.000000000000000000 ) ) ;
#140049 = EDGE_CURVE ( 'NONE', #112107, #132154, #51207, .T. ) ;
#140050 = DIRECTION ( 'NONE',  ( -0.7071067811865486830, -0.7071067811865464625, 0.000000000000000000 ) ) ;
#140051 = VERTEX_POINT ( 'NONE', #74395 ) ;
#140052 = CARTESIAN_POINT ( 'NONE',  ( 41.85459685856477563, -1.637169565754161615, 6.110000000000000320 ) ) ;
#140053 = EDGE_CURVE ( 'NONE', #22619, #65995, #96797, .T. ) ;
#140054 = VERTEX_POINT ( 'NONE', #141046 ) ;
#140055 = FACE_OUTER_BOUND ( 'NONE', #135006, .T. ) ;
#140056 = CARTESIAN_POINT ( 'NONE',  ( 21.18398860626899349, 28.73617430169802134, 5.000000000000000000 ) ) ;
#140057 = CARTESIAN_POINT ( 'NONE',  ( 11.20666063542144286, 21.75929247661549937, 4.998822639870701856 ) ) ;
#140058 = CARTESIAN_POINT ( 'NONE',  ( 21.18398860626899349, 28.73617430169802134, 5.000000000000000000 ) ) ;
#140059 = ADVANCED_FACE ( 'NONE', ( #75119 ), #54092, .F. ) ;
#140060 = EDGE_CURVE ( 'NONE', #58311, #10476, #19975, .T. ) ;
#140061 = ADVANCED_FACE ( 'NONE', ( #17821 ), #108383, .F. ) ;
#140062 = CARTESIAN_POINT ( 'NONE',  ( 37.97459685856477307, 1.637169565754164058, -6.109999999999996767 ) ) ;
#140063 = VERTEX_POINT ( 'NONE', #95405 ) ;
#140064 = EDGE_CURVE ( 'NONE', #86178, #56732, #97542, .T. ) ;
#140065 = CARTESIAN_POINT ( 'NONE',  ( 30.29974487139158867, -27.71228299555227537, 4.000000000000000000 ) ) ;
#140066 = ORIENTED_EDGE ( 'NONE', *, *, #133199, .T. ) ;
#140067 = EDGE_LOOP ( 'NONE', ( #88327, #35820, #25303, #22793 ) ) ;
#140068 = EDGE_LOOP ( 'NONE', ( #99094, #141717, #69771, #48046 ) ) ;
#140069 = VECTOR ( 'NONE', #100521, 1000.000000000000227 ) ;
#140070 = EDGE_CURVE ( 'NONE', #52608, #9115, #86697, .T. ) ;
#140071 = CARTESIAN_POINT ( 'NONE',  ( -15.68879807097514956, -1.757674993583058898, 4.000000000000000000 ) ) ;
#140072 = CARTESIAN_POINT ( 'NONE',  ( 34.42500000000002558, -22.26999999999999247, -0.5000000000000000000 ) ) ;
#140073 = PRODUCT_DEFINITION_CONTEXT ( 'detailed design', #104973, 'design' ) ;
#140074 = ORIENTED_EDGE ( 'NONE', *, *, #68724, .T. ) ;
#140075 =( NAMED_UNIT ( * ) SI_UNIT ( $, .STERADIAN. ) SOLID_ANGLE_UNIT ( ) );
#140076 = CARTESIAN_POINT ( 'NONE',  ( 52.28752705046288440, 0.000000000000000000, -7.949999999999998401 ) ) ;
#140077 = ADVANCED_FACE ( 'NONE', ( #75817 ), #40347, .F. ) ;
#140078 = CARTESIAN_POINT ( 'NONE',  ( 0.000000000000000000, 9.735942053221458872E-16, -7.950000000000000178 ) ) ;
#140079 = FACE_BOUND ( 'NONE', #82416, .T. ) ;
#140080 = VERTEX_POINT ( 'NONE', #9822 ) ;
#140081 = LINE ( 'NONE', #64641, #138307 ) ;
#140082 = CARTESIAN_POINT ( 'NONE',  ( 3.000000000000000000, -47.62213595499959951, 36.92500000000000426 ) ) ;
#140083 = ORIENTED_EDGE ( 'NONE', *, *, #71725, .T. ) ;
#140084 = LINE ( 'NONE', #42199, #38890 ) ;
#140085 = ORIENTED_EDGE ( 'NONE', *, *, #133868, .F. ) ;
#140087 = VERTEX_POINT ( 'NONE', #355 ) ;
#140086 = EDGE_CURVE ( 'NONE', #114619, #74261, #142504, .T. ) ;
#140088 = PLANE ( 'NONE',  #128186 ) ;
#140089 = ORIENTED_EDGE ( 'NONE', *, *, #53996, .T. ) ;
#140090 = VECTOR ( 'NONE', #16418, 1000.000000000000227 ) ;
#140091 = CARTESIAN_POINT ( 'NONE',  ( 60.43293019189810877, 1.637169565754156508, 6.110000000000000320 ) ) ;
#140092 = VERTEX_POINT ( 'NONE', #110541 ) ;
#140093 = CARTESIAN_POINT ( 'NONE',  ( 26.12840764549667583, 3.061616997868380183E-16, -2.500000000000001332 ) ) ;
#140094 = AXIS2_PLACEMENT_3D ( 'NONE', #64398, #116094, #61751 ) ;
#140095 = FACE_OUTER_BOUND ( 'NONE', #56102, .T. ) ;
#140096 = ADVANCED_FACE ( 'NONE', ( #134481 ), #67078, .F. ) ;
#140097 = ORIENTED_EDGE ( 'NONE', *, *, #79583, .T. ) ;
#140098 = FILL_AREA_STYLE ('',( #139400 ) ) ;
#140099 = EDGE_CURVE ( 'NONE', #64709, #4325, #120718, .T. ) ;
#140100 = CARTESIAN_POINT ( 'NONE',  ( -17.20710678118642178, -11.24070752338416312, 5.000000000000000000 ) ) ;
#140101 = VECTOR ( 'NONE', #65290, 1000.000000000000000 ) ;
#140102 = FILL_AREA_STYLE_COLOUR ( '', #38958 ) ;
#140103 = DIRECTION ( 'NONE',  ( 0.7071067811865487940, 0.7071067811865463515, 0.000000000000000000 ) ) ;
#140104 = EDGE_CURVE ( 'NONE', #125864, #41067, #77267, .T. ) ;
#140105 = CARTESIAN_POINT ( 'NONE',  ( -22.77325839282152131, -11.24070752338416845, 18.24660765846977384 ) ) ;
#140106 = ORIENTED_EDGE ( 'NONE', *, *, #104091, .F. ) ;
#140107 = ORIENTED_EDGE ( 'NONE', *, *, #33962, .F. ) ;
#140108 = LINE ( 'NONE', #84990, #137594 ) ;
#140109 = DIRECTION ( 'NONE',  ( 0.7071067811865487940, -0.7071067811865463515, 0.000000000000000000 ) ) ;
#140110 = VERTEX_POINT ( 'NONE', #67827 ) ;
#140111 = ADVANCED_FACE ( 'NONE', ( #88114 ), #99679, .F. ) ;
#140112 = VERTEX_POINT ( 'NONE', #122872 ) ;
#140113 = EDGE_LOOP ( 'NONE', ( #106700, #13883, #64991, #31845 ) ) ;
#140114 = CARTESIAN_POINT ( 'NONE',  ( -1.641757024588595737, 15.75929247661555799, 19.34181609438699923 ) ) ;
#140115 = DIRECTION ( 'NONE',  ( 0.6830127018922180770, -0.6830127018922204085, -0.2588190451025213501 ) ) ;
#140116 = ORIENTED_EDGE ( 'NONE', *, *, #101254, .F. ) ;
#140117 = CARTESIAN_POINT ( 'NONE',  ( -2.241399257802041856, 21.72499999999999432, 5.000000000000000000 ) ) ;
#140118 = PRESENTATION_LAYER_ASSIGNMENT (  '', '', ( #10518 ) ) ;
#140119 = CARTESIAN_POINT ( 'NONE',  ( 39.18398860626899705, 28.73617430169814568, 5.000000000000000000 ) ) ;
#140120 = AXIS2_PLACEMENT_3D ( 'NONE', #83616, #4522, #127826 ) ;
#140121 = CARTESIAN_POINT ( 'NONE',  ( 16.83790314143521982, -6.871911579029513106, -3.967499999999993587 ) ) ;
#140122 = VECTOR ( 'NONE', #142607, 1000.000000000000000 ) ;
#140123 = DIRECTION ( 'NONE',  ( 0.7071067811865487940, 0.7071067811865463515, 0.000000000000000000 ) ) ;
#140124 = VERTEX_POINT ( 'NONE', #133070 ) ;
#140125 = CARTESIAN_POINT ( 'NONE',  ( 122.1204301918981230, 3.055000000000002380, -5.291415217122917625 ) ) ;
#140126 = VECTOR ( 'NONE', #11485, 1000.000000000000000 ) ;
#140127 = EDGE_CURVE ( 'NONE', #121270, #47360, #11955, .T. ) ;
#140128 = LINE ( 'NONE', #118335, #72127 ) ;
#140129 = CARTESIAN_POINT ( 'NONE',  ( 54.48921356237310221, -27.52281430457093236, 5.000000000000000000 ) ) ;
#140131 = ORIENTED_EDGE ( 'NONE', *, *, #71045, .F. ) ;
#140130 = CARTESIAN_POINT ( 'NONE',  ( -14.81601139373099585, 28.73617430169776910, 5.000000000000000000 ) ) ;
#140132 = DIRECTION ( 'NONE',  ( 0.3543493200069162685, -0.000000000000000000, -0.9351131265310288487 ) ) ;
#140133 = EDGE_LOOP ( 'NONE', ( #86467, #69289, #137042, #105348 ) ) ;
#140134 = CARTESIAN_POINT ( 'NONE',  ( 76.64169371712954160, -2.130196079827424871, -7.949999999999998401 ) ) ;
#140135 = ADVANCED_FACE ( 'NONE', ( #13370 ), #24276, .F. ) ;
#140136 = LINE ( 'NONE', #17597, #638 ) ;
#140137 = LINE ( 'NONE', #40811, #102744 ) ;
#140138 = ORIENTED_EDGE ( 'NONE', *, *, #86153, .T. ) ;
#140139 = DIRECTION ( 'NONE',  ( -0.6830127018922180770, -0.6830127018922204085, -0.2588190451025213501 ) ) ;
#140140 = CARTESIAN_POINT ( 'NONE',  ( 26.67183060077628554, 8.259292476615632594, 4.000000000000000000 ) ) ;
#140141 = CARTESIAN_POINT ( 'NONE',  ( 14.27159235450332098, 9.902892378096218942E-16, 0.000000000000000000 ) ) ;
#140142 = ORIENTED_EDGE ( 'NONE', *, *, #54990, .T. ) ;
#140143 = DIRECTION ( 'NONE',  ( 0.000000000000000000, -1.000000000000000000, 0.000000000000000000 ) ) ;
#140144 = CARTESIAN_POINT ( 'NONE',  ( 6.299744871391586898, -27.71228299555210484, 4.000000000000000000 ) ) ;
#140145 = CARTESIAN_POINT ( 'NONE',  ( -25.17183060077629619, -2.240707523384257716, 4.000000000000000000 ) ) ;
#140146 = LINE ( 'NONE', #16170, #14776 ) ;
#140147 = CARTESIAN_POINT ( 'NONE',  ( -9.183988606268997046, 28.73617430169793607, 5.000000000000000000 ) ) ;
#140148 = ORIENTED_EDGE ( 'NONE', *, *, #137503, .F. ) ;
#140149 = VERTEX_POINT ( 'NONE', #79426 ) ;
#140150 = DIRECTION ( 'NONE',  ( -0.7071067811865486830, -0.7071067811865464625, 0.000000000000000000 ) ) ;
#140151 = LINE ( 'NONE', #42983, #62190 ) ;
#140152 = CARTESIAN_POINT ( 'NONE',  ( 9.749569808101886892, 3.967499999999998916, 6.871911579029510442 ) ) ;
#140153 = DIRECTION ( 'NONE',  ( 0.7071067811865487940, 0.7071067811865463515, 0.000000000000000000 ) ) ;
#140154 = EDGE_CURVE ( 'NONE', #111064, #70001, #132363, .T. ) ;
#140155 = DIRECTION ( 'NONE',  ( -0.7071067811865487940, 0.7071067811865463515, -0.000000000000000000 ) ) ;
#140156 = FACE_OUTER_BOUND ( 'NONE', #98801, .T. ) ;
#140157 = ORIENTED_EDGE ( 'NONE', *, *, #27944, .T. ) ;
#140158 = LINE ( 'NONE', #38695, #120510 ) ;
#140159 = DIRECTION ( 'NONE',  ( 0.7071067811865487940, 0.7071067811865463515, 0.000000000000000000 ) ) ;
#140160 = CARTESIAN_POINT ( 'NONE',  ( 4.712472949537106715, 0.000000000000000000, 6.094999999999989981 ) ) ;
#140161 = CARTESIAN_POINT ( 'NONE',  ( 38.84959685856477307, 6.109999999999997655, 1.637169565754163836 ) ) ;
#140162 = CARTESIAN_POINT ( 'NONE',  ( -19.05000000000000071, 3.174999999999997158, 4.000000000000000000 ) ) ;
#140163 = ORIENTED_EDGE ( 'NONE', *, *, #20901, .F. ) ;
#140164 = DIRECTION ( 'NONE',  ( 0.000000000000000000, -1.000000000000000000, 0.000000000000000000 ) ) ;
#140165 = EDGE_LOOP ( 'NONE', ( #77184, #112519, #9614, #112931 ) ) ;
#140166 = VERTEX_POINT ( 'NONE', #1757 ) ;
#140167 = CARTESIAN_POINT ( 'NONE',  ( -8.163471288734461595, 15.75929247661555976, 9.299976744542901130 ) ) ;
#140168 = DIRECTION ( 'NONE',  ( -0.7071067811865486830, -0.7071067811865464625, 0.000000000000000000 ) ) ;
#140169 = DIRECTION ( 'NONE',  ( 0.7071067811865487940, -0.7071067811865463515, 0.000000000000000000 ) ) ;
#140170 = PLANE ( 'NONE',  #129925 ) ;
#140171 = CARTESIAN_POINT ( 'NONE',  ( -30.79289321881324426, -8.240707523384196875, 5.000000000000000000 ) ) ;
#140172 = DIRECTION ( 'NONE',  ( -1.000000000000000000, -1.224606353822377258E-16, -0.000000000000000000 ) ) ;
#140173 = LINE ( 'NONE', #63358, #70880 ) ;
#140174 = ORIENTED_EDGE ( 'NONE', *, *, #68057, .T. ) ;
#140175 = DIRECTION ( 'NONE',  ( -0.7071067811865486830, 0.7071067811865464625, 0.000000000000000000 ) ) ;
#140176 = CARTESIAN_POINT ( 'NONE',  ( 21.15294044719737698, 3.821174125832445049E-16, 0.000000000000000000 ) ) ;
#140177 = LINE ( 'NONE', #107530, #93507 ) ;
#140178 = DIRECTION ( 'NONE',  ( -0.000000000000000000, 0.3543493200069153248, 0.9351131265310292928 ) ) ;
#140179 = PLANE ( 'NONE',  #68213 ) ;
#140180 = CARTESIAN_POINT ( 'NONE',  ( 104.3500270504628844, -5.819803920172573086, -5.819803920172573086 ) ) ;
#140181 = CARTESIAN_POINT ( 'NONE',  ( 70.37086038379622721, 6.884901960086289741, -3.974999999999993427 ) ) ;
#140182 = AXIS2_PLACEMENT_3D ( 'NONE', #70694, #135233, #59802 ) ;
#140183 = LINE ( 'NONE', #85074, #34557 ) ;
#140184 = ORIENTED_EDGE ( 'NONE', *, *, #78750, .T. ) ;
#140185 = ORIENTED_EDGE ( 'NONE', *, *, #9092, .T. ) ;
#140186 = CARTESIAN_POINT ( 'NONE',  ( 56.56250000000000711, -5.819803920172572198, -5.819803920172573086 ) ) ;
#140187 = CARTESIAN_POINT ( 'NONE',  ( -2.207106781186525701, 3.759292476615680112, 5.000000000000000000 ) ) ;
#140188 = CARTESIAN_POINT ( 'NONE',  ( -2.999999999999968026, -16.44781430457066662, 5.000000000000000000 ) ) ;
#140189 = CARTESIAN_POINT ( 'NONE',  ( 14.51078643762690490, -27.52281430457045275, 5.000000000000000000 ) ) ;
#140190 = ORIENTED_EDGE ( 'NONE', *, *, #47815, .T. ) ;
#140191 =( BOUNDED_CURVE ( )  B_SPLINE_CURVE ( 3, ( #104098, #28734, #4760, #138920 ),
 .UNSPECIFIED., .F., .F. ) 
 B_SPLINE_CURVE_WITH_KNOTS ( ( 4, 4 ),
 ( 4.350170835173033268, 4.500739107949262241 ),
 .UNSPECIFIED. ) 
 CURVE ( )  GEOMETRIC_REPRESENTATION_ITEM ( )  RATIONAL_B_SPLINE_CURVE ( ( 1.000000000000000000, 0.9981116584018946414, 0.9981116584018946414, 1.000000000000000000 ) ) 
 REPRESENTATION_ITEM ( '' )  );
#140192 = CARTESIAN_POINT ( 'NONE',  ( 66.18398860626901126, 28.73617430169833753, 5.000000000000000000 ) ) ;
#140193 = VECTOR ( 'NONE', #64939, 1000.000000000000000 ) ;
#140194 = CARTESIAN_POINT ( 'NONE',  ( 46.08376352523143993, -6.110000000000001208, -3.741295971395164515E-16 ) ) ;
#140195 = EDGE_LOOP ( 'NONE', ( #99983, #84866, #108695, #49362 ) ) ;
#140196 = ADVANCED_FACE ( 'NONE', ( #66370 ), #90984, .F. ) ;
#140197 = DIRECTION ( 'NONE',  ( -1.000000000000000000, -1.224606353822377258E-16, -0.000000000000000000 ) ) ;
#140198 = ORIENTED_EDGE ( 'NONE', *, *, #15923, .T. ) ;
#140199 = EDGE_CURVE ( 'NONE', #14841, #78241, #88843, .T. ) ;
#140200 = ORIENTED_EDGE ( 'NONE', *, *, #93924, .F. ) ;
#140201 = DIRECTION ( 'NONE',  ( -0.7071067811865486830, -0.7071067811865464625, 0.000000000000000000 ) ) ;
#140202 = CARTESIAN_POINT ( 'NONE',  ( -9.183988606268997046, 28.73617430169793607, 5.000000000000000000 ) ) ;
#140203 = VERTEX_POINT ( 'NONE', #57647 ) ;
#140204 = LINE ( 'NONE', #87958, #2541 ) ;
#140205 = ADVANCED_FACE ( 'NONE', ( #77956 ), #122140, .F. ) ;
#140206 = ADVANCED_FACE ( 'NONE', ( #101834 ), #56241, .F. ) ;
#140208 = ORIENTED_EDGE ( 'NONE', *, *, #106808, .T. ) ;
#140207 = CARTESIAN_POINT ( 'NONE',  ( -30.18398860626900060, 28.73617430169808173, 5.000000000000000000 ) ) ;
#140209 = LINE ( 'NONE', #117695, #121851 ) ;
#140210 = DIRECTION ( 'NONE',  ( 0.7071067811865486830, -0.7071067811865464625, -0.000000000000000000 ) ) ;
#140211 = LINE ( 'NONE', #118438, #36885 ) ;
#140212 = VECTOR ( 'NONE', #97569, 1000.000000000000000 ) ;
#140214 = ORIENTED_EDGE ( 'NONE', *, *, #107279, .T. ) ;
#140213 = EDGE_CURVE ( 'NONE', #106288, #68187, #14428, .T. ) ;
#140215 = EDGE_CURVE ( 'NONE', #37549, #101265, #98959, .T. ) ;
#140216 = ORIENTED_EDGE ( 'NONE', *, *, #26786, .F. ) ;
#140217 = EDGE_CURVE ( 'NONE', #90401, #72522, #143200, .T. ) ;
#140218 = VECTOR ( 'NONE', #43791, 1000.000000000000000 ) ;
#140219 = DIRECTION ( 'NONE',  ( -1.000000000000000000, -1.224606353822377258E-16, -0.000000000000000000 ) ) ;
#140220 = CARTESIAN_POINT ( 'NONE',  ( 77.93293019189812298, 1.637169565754156508, 6.110000000000000320 ) ) ;
#140221 = PLANE ( 'NONE',  #37197 ) ;
#140222 = EDGE_CURVE ( 'NONE', #82210, #43404, #108798, .T. ) ;
#140223 = DIRECTION ( 'NONE',  ( 1.000000000000000000, -0.000000000000000000, 0.000000000000000000 ) ) ;
#140224 = DIRECTION ( 'NONE',  ( -0.000000000000000000, -0.3543493200069152693, 0.9351131265310292928 ) ) ;
#140225 = EDGE_LOOP ( 'NONE', ( #70612, #56399, #15434, #94431 ) ) ;
#140226 = VERTEX_POINT ( 'NONE', #95768 ) ;
#140228 = EDGE_CURVE ( 'NONE', #69799, #1792, #76460, .T. ) ;
#140227 = AXIS2_PLACEMENT_3D ( 'NONE', #7078, #51360, #95552 ) ;
#140229 = DIRECTION ( 'NONE',  ( -0.6830127018922180770, -0.6830127018922204085, -0.2588190451025213501 ) ) ;
#140230 = DIRECTION ( 'NONE',  ( -0.7071067811865486830, -0.7071067811865464625, -0.000000000000000000 ) ) ;
#140231 = VERTEX_POINT ( 'NONE', #7311 ) ;
#140232 = EDGE_CURVE ( 'NONE', #93195, #58856, #80116, .T. ) ;
#140233 = ORIENTED_EDGE ( 'NONE', *, *, #110454, .T. ) ;
#140234 = CARTESIAN_POINT ( 'NONE',  ( 34.45011844616451668, 13.51628081163735828, 5.000000000000000888 ) ) ;
#140235 = ORIENTED_EDGE ( 'NONE', *, *, #117157, .F. ) ;
#140236 = CARTESIAN_POINT ( 'NONE',  ( 34.92499999999998295, 0.5846064065779636998, -3.200354092940492112 ) ) ;
#140237 = EDGE_CURVE ( 'NONE', #17447, #125425, #107358, .T. ) ;
#140238 = CARTESIAN_POINT ( 'NONE',  ( -34.47516574401891631, -14.97193265888402181, 4.998110765256835286 ) ) ;
#140239 = FACE_BOUND ( 'NONE', #35300, .T. ) ;
#140240 = DIRECTION ( 'NONE',  ( 1.000000000000000000, 0.000000000000000000, 0.000000000000000000 ) ) ;
#140241 = CARTESIAN_POINT ( 'NONE',  ( 40.47502705046289151, -5.819803920172573086, 5.819803920172573086 ) ) ;
#140242 = LINE ( 'NONE', #9702, #41062 ) ;
#140244 = EDGE_LOOP ( 'NONE', ( #59335, #67905, #141887, #10513 ) ) ;
#140243 = DIRECTION ( 'NONE',  ( -0.000000000000000000, 0.000000000000000000, 1.000000000000000000 ) ) ;
#140245 = EDGE_CURVE ( 'NONE', #118125, #18521, #51577, .T. ) ;
#140246 = LINE ( 'NONE', #61989, #90335 ) ;
#140247 = CONTEXT_DEPENDENT_SHAPE_REPRESENTATION ( #37469, #63245 ) ;
#140248 = ORIENTED_EDGE ( 'NONE', *, *, #1693, .F. ) ;
#140249 = ORIENTED_EDGE ( 'NONE', *, *, #45704, .T. ) ;
#140250 = CARTESIAN_POINT ( 'NONE',  ( 85.80793019189810877, -6.109999999999998543, 1.637169565754158507 ) ) ;
#140251 = ORIENTED_EDGE ( 'NONE', *, *, #110411, .T. ) ;
#140252 = DIRECTION ( 'NONE',  ( -0.6830127018922180770, -0.6830127018922204085, -0.2588190451025213501 ) ) ;
#140253 = DIRECTION ( 'NONE',  ( -0.6830127018922180770, -0.6830127018922204085, -0.2588190451025213501 ) ) ;
#140254 = PLANE ( 'NONE',  #51334 ) ;
#140255 = DIRECTION ( 'NONE',  ( -0.7071067811865486830, -0.7071067811865464625, -0.000000000000000000 ) ) ;
#140256 = ADVANCED_FACE ( 'NONE', ( #96446 ), #18920, .T. ) ;
#140257 = CARTESIAN_POINT ( 'NONE',  ( 4.600000000000001421, -2.055000000000000160, 2.789133085058098087E-16 ) ) ;
#140258 = DIRECTION ( 'NONE',  ( -0.7071067811865486830, -0.7071067811865464625, 0.000000000000000000 ) ) ;
#140259 = CARTESIAN_POINT ( 'NONE',  ( 5.671830600776438303, 5.259292476615662792, 4.000000000000000000 ) ) ;
#140260 = EDGE_CURVE ( 'NONE', #39036, #83246, #52264, .T. ) ;
#140261 = DIRECTION ( 'NONE',  ( -1.000000000000000000, -1.224606353822377258E-16, -0.000000000000000000 ) ) ;
#140262 = CARTESIAN_POINT ( 'NONE',  ( 45.29974487139158867, -27.71228299555237840, 4.000000000000000000 ) ) ;
#140263 = PLANE ( 'NONE',  #86296 ) ;
#140264 = ORIENTED_EDGE ( 'NONE', *, *, #130789, .T. ) ;
#140265 = LINE ( 'NONE', #8971, #28743 ) ;
#140266 = EDGE_CURVE ( 'NONE', #34599, #79126, #50141, .T. ) ;
#140267 = PLANE ( 'NONE',  #35157 ) ;
#140268 = ORIENTED_EDGE ( 'NONE', *, *, #116414, .F. ) ;
#140269 = VERTEX_POINT ( 'NONE', #113409 ) ;
#140270 = ORIENTED_EDGE ( 'NONE', *, *, #99267, .F. ) ;
#140271 = CARTESIAN_POINT ( 'NONE',  ( 31.93793019189809712, -6.110000000000001208, 1.637169565754158951 ) ) ;
#140272 = VERTEX_POINT ( 'NONE', #58389 ) ;
#140273 = DIRECTION ( 'NONE',  ( 0.7071067811865487940, 0.7071067811865463515, -0.000000000000000000 ) ) ;
#140274 = VECTOR ( 'NONE', #130419, 1000.000000000000227 ) ;
#140275 = CARTESIAN_POINT ( 'NONE',  ( 18.12913961620377279, 5.278424836066147208, 3.047499999999990550 ) ) ;
#140276 = CARTESIAN_POINT ( 'NONE',  ( 3.894756034733422911, 12.18018086707143866, -25.55842831757935940 ) ) ;
#140277 = ORIENTED_EDGE ( 'NONE', *, *, #124732, .T. ) ;
#140278 = AXIS2_PLACEMENT_3D ( 'NONE', #71395, #115556, #135925 ) ;
#140279 = ADVANCED_FACE ( 'NONE', ( #102572 ), #3216, .F. ) ;
#140280 = CARTESIAN_POINT ( 'NONE',  ( 7.139999999999985469, -39.92999999999999972, 18.93259187797431764 ) ) ;
#140281 = ORIENTED_EDGE ( 'NONE', *, *, #52191, .F. ) ;
#140282 = PLANE ( 'NONE',  #132126 ) ;
#140283 = PLANE ( 'NONE',  #47542 ) ;
#140285 = ORIENTED_EDGE ( 'NONE', *, *, #23516, .T. ) ;
#140284 = LINE ( 'NONE', #107638, #23980 ) ;
#140286 = ORIENTED_EDGE ( 'NONE', *, *, #122325, .T. ) ;
#140287 = DIRECTION ( 'NONE',  ( -0.7071067811865486830, -0.7071067811865464625, -0.000000000000000000 ) ) ;
#140288 = ORIENTED_EDGE ( 'NONE', *, *, #80164, .T. ) ;
#140289 = LINE ( 'NONE', #87343, #43533 ) ;
#140290 = ORIENTED_EDGE ( 'NONE', *, *, #104590, .T. ) ;
#140291 = ORIENTED_EDGE ( 'NONE', *, *, #114260, .F. ) ;
#140292 = VERTEX_POINT ( 'NONE', #140691 ) ;
#140293 = COLOUR_RGB ( '', 0.40784314, 0.44705882, 0.49803922) ;
#140294 = PLANE ( 'NONE',  #102789 ) ;
#140295 = PLANE ( 'NONE',  #141876 ) ;
#140296 = CARTESIAN_POINT ( 'NONE',  ( 34.49999999999976552, 0.05432934483094861711, 4.994342998332161443 ) ) ;
#140297 = DIRECTION ( 'NONE',  ( 0.7071067811865487940, 0.7071067811865463515, -0.000000000000000000 ) ) ;
#140298 = EDGE_CURVE ( 'NONE', #16022, #8423, #126958, .T. ) ;
#140299 = PLANE ( 'NONE',  #50621 ) ;
#140300 = EDGE_LOOP ( 'NONE', ( #45647, #94715, #111722, #24788 ) ) ;
#140301 = CARTESIAN_POINT ( 'NONE',  ( -60.18398860626900415, 28.73617430169829490, 5.000000000000000000 ) ) ;
#140302 = ORIENTED_EDGE ( 'NONE', *, *, #23752, .T. ) ;
#140303 = FACE_OUTER_BOUND ( 'NONE', #52360, .T. ) ;
#140304 = VECTOR ( 'NONE', #85992, 1000.000000000000000 ) ;
#140305 = CARTESIAN_POINT ( 'NONE',  ( 27.54123647476855652, 0.000000000000000000, 7.934999999999990727 ) ) ;
#140306 = CARTESIAN_POINT ( 'NONE',  ( 12.81349135397630867, -15.74070752338412404, 8.904080028138910308 ) ) ;
#140307 = EDGE_LOOP ( 'NONE', ( #110998, #113141, #102209, #88588 ) ) ;
#140308 = PLANE ( 'NONE',  #131699 ) ;
#140309 = CARTESIAN_POINT ( 'NONE',  ( 29.20710678118634718, 12.75929247661558996, 5.000000000000000000 ) ) ;
#140310 = ADVANCED_FACE ( 'NONE', ( #61063 ), #71917, .F. ) ;
#140311 = EDGE_LOOP ( 'NONE', ( #12199, #67496, #9330, #74406 ) ) ;
#140312 = EDGE_LOOP ( 'NONE', ( #128527, #36058, #119582, #132135 ) ) ;
#140313 = CARTESIAN_POINT ( 'NONE',  ( 20.97999999999999687, -2.055000000000000160, 2.789133085058098087E-16 ) ) ;
#140314 = PLANE ( 'NONE',  #88233 ) ;
#140315 = UNCERTAINTY_MEASURE_WITH_UNIT (LENGTH_MEASURE( 1.000000000000000082E-05 ), #121660, 'distance_accuracy_value', 'NONE');
#140316 = CARTESIAN_POINT ( 'NONE',  ( 69.29974487139159578, -27.71228299555254537, 4.000000000000000000 ) ) ;
#140317 = VECTOR ( 'NONE', #105888, 1000.000000000000000 ) ;
#140318 = LINE ( 'NONE', #41004, #68315 ) ;
#140319 = CARTESIAN_POINT ( 'NONE',  ( 69.62043019189812298, 3.055000000000002380, -5.291415217122917625 ) ) ;
#140320 = ADVANCED_FACE ( 'NONE', ( #105217 ), #5874, .F. ) ;
#140321 = CARTESIAN_POINT ( 'NONE',  ( -0.2997448713915885632, -27.71228299555206220, 4.000000000000000000 ) ) ;
#140322 = CARTESIAN_POINT ( 'NONE',  ( 34.92499999999998295, -21.72500000000000142, 5.000000000000000000 ) ) ;
#140323 = EDGE_CURVE ( 'NONE', #14903, #99523, #84895, .T. ) ;
#140324 = LINE ( 'NONE', #41009, #104285 ) ;
#140325 = DIRECTION ( 'NONE',  ( 0.7071067811865487940, 0.7071067811865463515, 0.000000000000000000 ) ) ;
#140326 = ORIENTED_EDGE ( 'NONE', *, *, #13984, .T. ) ;
#140327 = PLANE ( 'NONE',  #69650 ) ;
#140328 = ORIENTED_EDGE ( 'NONE', *, *, #133809, .T. ) ;
#140329 = LINE ( 'NONE', #121419, #36270 ) ;
#140330 = FACE_OUTER_BOUND ( 'NONE', #11192, .T. ) ;
#140331 = ORIENTED_EDGE ( 'NONE', *, *, #121138, .T. ) ;
#140332 = DIRECTION ( 'NONE',  ( 0.3543493200069163240, 0.000000000000000000, 0.9351131265310288487 ) ) ;
#140334 = ORIENTED_EDGE ( 'NONE', *, *, #140730, .T. ) ;
#140333 = CARTESIAN_POINT ( 'NONE',  ( -34.92500000000001137, -18.28150956279557704, 4.759050581649344025 ) ) ;
#140335 = EDGE_CURVE ( 'NONE', #11920, #22872, #81224, .T. ) ;
#140336 = FACE_OUTER_BOUND ( 'NONE', #40594, .T. ) ;
#140337 = DIRECTION ( 'NONE',  ( -0.7071067811865486830, -0.7071067811865464625, -0.000000000000000000 ) ) ;
#140338 = ORIENTED_EDGE ( 'NONE', *, *, #98465, .F. ) ;
#140339 = EDGE_LOOP ( 'NONE', ( #52945, #24930, #136386, #23592 ) ) ;
#140340 = SURFACE_STYLE_FILL_AREA ( #94670 ) ;
#140341 = UNCERTAINTY_MEASURE_WITH_UNIT (LENGTH_MEASURE( 1.000000000000000082E-05 ), #94244, 'distance_accuracy_value', 'NONE');
#140342 = LINE ( 'NONE', #96793, #119352 ) ;
#140343 = CARTESIAN_POINT ( 'NONE',  ( 92.68336038379624142, -2.130196079827426203, 7.949999999999997513 ) ) ;
#140344 = CARTESIAN_POINT ( 'NONE',  ( -51.48921356237309510, -27.52281430457091460, 5.000000000000000000 ) ) ;
#140345 = CARTESIAN_POINT ( 'NONE',  ( 0.7928932188134528714, 9.759292476615627265, 5.000000000000000000 ) ) ;
#140346 = ORIENTED_EDGE ( 'NONE', *, *, #6647, .F. ) ;
#140347 = DIRECTION ( 'NONE',  ( 0.6830127018922180770, -0.6830127018922204085, -0.2588190451025213501 ) ) ;
#140348 = PLANE ( 'NONE',  #80939 ) ;
#140349 = CARTESIAN_POINT ( 'NONE',  ( 31.50000000000000000, 0.000000000000000000, 6.094999999999989981 ) ) ;
#140350 = VECTOR ( 'NONE', #45535, 1000.000000000000000 ) ;
#140351 = DIRECTION ( 'NONE',  ( 0.000000000000000000, -1.000000000000000000, 0.000000000000000000 ) ) ;
#140352 = EDGE_LOOP ( 'NONE', ( #76268, #8055, #27591, #52893 ) ) ;
#140353 = DIRECTION ( 'NONE',  ( 0.7071067811865487940, 0.7071067811865463515, 0.000000000000000000 ) ) ;
#140354 = EDGE_LOOP ( 'NONE', ( #36374, #78267, #86262, #65917 ) ) ;
#140355 = CARTESIAN_POINT ( 'NONE',  ( 79.91709685856476142, 3.054999999999998828, 5.291415217122922066 ) ) ;
#140356 = CARTESIAN_POINT ( 'NONE',  ( 60.48921356237309510, -27.52281430457097500, 5.000000000000000000 ) ) ;
#140357 = VECTOR ( 'NONE', #117650, 999.9999999999998863 ) ;
#140358 = CARTESIAN_POINT ( 'NONE',  ( -28.49999999999980460, 11.52377502935400955, -1.522421517564018112 ) ) ;
#140359 = ORIENTED_EDGE ( 'NONE', *, *, #19563, .T. ) ;
#140360 = DIRECTION ( 'NONE',  ( 1.000000000000000000, 0.000000000000000000, 0.000000000000000000 ) ) ;
#140361 = FACE_OUTER_BOUND ( 'NONE', #49497, .T. ) ;
#140362 = PLANE ( 'NONE',  #43971 ) ;
#140363 = EDGE_CURVE ( 'NONE', #71971, #13935, #129107, .T. ) ;
#140365 = ORIENTED_EDGE ( 'NONE', *, *, #44603, .F. ) ;
#140364 = CARTESIAN_POINT ( 'NONE',  ( -34.92500000000001137, 22.22500000000000142, 4.500000000000000888 ) ) ;
#140366 = CARTESIAN_POINT ( 'NONE',  ( 3.198522738312878477, 22.22500000000000142, -9.446427897663703277 ) ) ;
#140367 = CARTESIAN_POINT ( 'NONE',  ( 38.28752705046288440, 0.000000000000000000, -7.949999999999998401 ) ) ;
#140368 =( BOUNDED_CURVE ( )  B_SPLINE_CURVE ( 3, ( #117280, #73808, #29570, #140478 ),
 .UNSPECIFIED., .F., .F. ) 
 B_SPLINE_CURVE_WITH_KNOTS ( ( 4, 4 ),
 ( 5.043186909253408956, 5.074607125596339863 ),
 .UNSPECIFIED. ) 
 CURVE ( )  GEOMETRIC_REPRESENTATION_ITEM ( )  RATIONAL_B_SPLINE_CURVE ( ( 1.000000000000000000, 0.9999177325257868620, 0.9999177325257868620, 1.000000000000000000 ) ) 
 REPRESENTATION_ITEM ( '' )  );
#140369 = LINE ( 'NONE', #61437, #21511 ) ;
#140370 = ORIENTED_EDGE ( 'NONE', *, *, #118277, .T. ) ;
#140371 = VECTOR ( 'NONE', #119199, 1000.000000000000000 ) ;
#140372 = EDGE_LOOP ( 'NONE', ( #65359, #105518, #46177, #124027, #48081 ) ) ;
#140373 = EDGE_CURVE ( 'NONE', #26996, #99025, #40003, .T. ) ;
#140374 = CARTESIAN_POINT ( 'NONE',  ( 78.02126352523146124, -4.472830434245839371, -4.472830434245840259 ) ) ;
#140375 = VERTEX_POINT ( 'NONE', #128415 ) ;
#140376 = EDGE_CURVE ( 'NONE', #124257, #135110, #23222, .T. ) ;
#140377 = CARTESIAN_POINT ( 'NONE',  ( -12.69999999999998153, 0.000000000000000000, 2.500000000000000444 ) ) ;
#140378 = CARTESIAN_POINT ( 'NONE',  ( -18.98911971346038285, -22.02621442084247860, 4.990779571109222879 ) ) ;
#140379 = EDGE_CURVE ( 'NONE', #73261, #89868, #21785, .T. ) ;
#140380 = CARTESIAN_POINT ( 'NONE',  ( 22.49999999999985434, -10.91253812416064228, 4.000000000000000000 ) ) ;
#140381 = LINE ( 'NONE', #138251, #135756 ) ;
#140382 = ORIENTED_EDGE ( 'NONE', *, *, #67677, .F. ) ;
#140383 = ADVANCED_FACE ( 'NONE', ( #99317 ), #10180, .F. ) ;
#140384 = CARTESIAN_POINT ( 'NONE',  ( 42.18398860626899705, 28.73617430169816700, 5.000000000000000000 ) ) ;
#140385 = SURFACE_STYLE_FILL_AREA ( #96146 ) ;
#140386 = ORIENTED_EDGE ( 'NONE', *, *, #16156, .T. ) ;
#140388 = EDGE_CURVE ( 'NONE', #91909, #68198, #59756, .T. ) ;
#140387 = VECTOR ( 'NONE', #6276, 1000.000000000000000 ) ;
#140389 = CARTESIAN_POINT ( 'NONE',  ( 29.99999999999979039, -11.35517001088069300, -1.126524801160039724 ) ) ;
#140390 = DIRECTION ( 'NONE',  ( 0.000000000000000000, 1.000000000000000000, -0.000000000000000000 ) ) ;
#140391 = DIRECTION ( 'NONE',  ( -0.7071067811865486830, -0.7071067811865464625, -0.000000000000000000 ) ) ;
#140392 = ORIENTED_EDGE ( 'NONE', *, *, #102968, .F. ) ;
#140393 = ORIENTED_EDGE ( 'NONE', *, *, #110687, .F. ) ;
#140394 = ADVANCED_FACE ( 'NONE', ( #120336 ), #97923, .T. ) ;
#140395 = VECTOR ( 'NONE', #102778, 999.9999999999998863 ) ;
#140396 = EDGE_CURVE ( 'NONE', #2401, #25054, #67237, .T. ) ;
#140397 = DIRECTION ( 'NONE',  ( 0.6830127018922181881, 0.6830127018922202975, -0.2588190451025214056 ) ) ;
#140398 = CARTESIAN_POINT ( 'NONE',  ( 8.816011393731004731, 28.73617430169781173, 5.000000000000000000 ) ) ;
#140399 = CARTESIAN_POINT ( 'NONE',  ( -20.99999999999985789, 19.55218569542897100, 5.000000000000000000 ) ) ;
#140400 = CARTESIAN_POINT ( 'NONE',  ( 27.00000000000000355, 0.000000000000000000, 0.000000000000000000 ) ) ;
#140401 =( NAMED_UNIT ( * ) SI_UNIT ( $, .STERADIAN. ) SOLID_ANGLE_UNIT ( ) );
#140402 = ADVANCED_FACE ( 'NONE', ( #52961 ), #120476, .T. ) ;
#140403 = COLOUR_RGB ( '', 0.72549020, 0.75294118, 0.79215686) ;
#140404 = AXIS2_PLACEMENT_3D ( 'NONE', #124342, #93142, #25010 ) ;
#140405 = CARTESIAN_POINT ( 'NONE',  ( 8.999999999999943157, -1.447814304570811617, 5.000000000000000000 ) ) ;
#140406 = SURFACE_STYLE_FILL_AREA ( #126657 ) ;
#140407 = EDGE_LOOP ( 'NONE', ( #125939, #91272, #129070, #81273 ) ) ;
#140408 = VECTOR ( 'NONE', #108785, 1000.000000000000000 ) ;
#140409 = ORIENTED_EDGE ( 'NONE', *, *, #13989, .T. ) ;
#140410 = VERTEX_POINT ( 'NONE', #33417 ) ;
#140411 = VERTEX_POINT ( 'NONE', #142160 ) ;
#140412 = VECTOR ( 'NONE', #11387, 1000.000000000000000 ) ;
#140413 = LINE ( 'NONE', #87475, #116515 ) ;
#140414 = ORIENTED_EDGE ( 'NONE', *, *, #131427, .F. ) ;
#140415 = CARTESIAN_POINT ( 'NONE',  ( 68.91252705046288440, -7.949999999999998401, -4.867971026610728450E-16 ) ) ;
#140416 = CARTESIAN_POINT ( 'NONE',  ( 83.99451991528748351, 28.92564299267996830, 4.000000000000000000 ) ) ;
#140417 = CARTESIAN_POINT ( 'NONE',  ( 42.18398860626899705, 28.73617430169816700, 5.000000000000000000 ) ) ;
#140418 = EDGE_CURVE ( 'NONE', #30830, #63481, #100070, .T. ) ;
#140419 = CARTESIAN_POINT ( 'NONE',  ( -72.29974487139158157, -27.71228299555256669, 4.000000000000000000 ) ) ;
#140420 = DIRECTION ( 'NONE',  ( 0.7071067811865486830, -0.7071067811865464625, -0.000000000000000000 ) ) ;
#140421 = EDGE_LOOP ( 'NONE', ( #34030, #27488, #101028 ) ) ;
#140422 = PLANE ( 'NONE',  #93505 ) ;
#140423 = CARTESIAN_POINT ( 'NONE',  ( 0.000000000000000000, 0.000000000000000000, 10.00000000000000000 ) ) ;
#140424 = ORIENTED_EDGE ( 'NONE', *, *, #79908, .F. ) ;
#140425 = CARTESIAN_POINT ( 'NONE',  ( -25.00051279177633390, 3.647752439586037454, 4.157751055492734160 ) ) ;
#140426 = EDGE_LOOP ( 'NONE', ( #82713, #123853, #123183, #22763 ) ) ;
#140427 = CARTESIAN_POINT ( 'NONE',  ( 12.29580628287044242, -5.278424836066144543, 3.047499999999995879 ) ) ;
#140428 = ORIENTED_EDGE ( 'NONE', *, *, #50861, .F. ) ;
#140429 = CARTESIAN_POINT ( 'NONE',  ( 62.56293019189811133, 1.637169565754157174, 6.110000000000002984 ) ) ;
#140430 = VERTEX_POINT ( 'NONE', #20331 ) ;
#140431 = ORIENTED_EDGE ( 'NONE', *, *, #120997, .T. ) ;
#140432 = EDGE_CURVE ( 'NONE', #87956, #105448, #85593, .T. ) ;
#140433 = DIRECTION ( 'NONE',  ( 1.000000000000000000, 0.000000000000000000, 0.000000000000000000 ) ) ;
#140434 = VECTOR ( 'NONE', #130493, 1000.000000000000000 ) ;
#140435 = CARTESIAN_POINT ( 'NONE',  ( 27.18398860626900060, 28.73617430169806042, 5.000000000000000000 ) ) ;
#140436 = CARTESIAN_POINT ( 'NONE',  ( 95.81293019189809002, -1.637169565754159617, -6.110000000000001208 ) ) ;
#140437 = DIRECTION ( 'NONE',  ( 0.7071067811865486830, -0.7071067811865464625, -0.000000000000000000 ) ) ;
#140438 = EDGE_CURVE ( 'NONE', #108363, #50134, #64575, .T. ) ;
#140439 = DIRECTION ( 'NONE',  ( -0.7071067811865486830, -0.7071067811865464625, 0.000000000000000000 ) ) ;
#140440 = PLANE ( 'NONE',  #92655 ) ;
#140441 = DIRECTION ( 'NONE',  ( 0.000000000000000000, -1.000000000000000000, 0.000000000000000000 ) ) ;
#140442 = VECTOR ( 'NONE', #124683, 1000.000000000000000 ) ;
#140443 = DIRECTION ( 'NONE',  ( 0.7071067811865486830, -0.7071067811865464625, -0.000000000000000000 ) ) ;
#140444 = PLANE ( 'NONE',  #38195 ) ;
#140445 = VERTEX_POINT ( 'NONE', #108753 ) ;
#140446 = CARTESIAN_POINT ( 'NONE',  ( -26.99451991528749417, 28.92564299267956685, 4.000000000000000000 ) ) ;
#140447 = EDGE_CURVE ( 'NONE', #36187, #135322, #88487, .T. ) ;
#140448 = ORIENTED_EDGE ( 'NONE', *, *, #48182, .F. ) ;
#140449 = ORIENTED_EDGE ( 'NONE', *, *, #45766, .T. ) ;
#140450 = ORIENTED_EDGE ( 'NONE', *, *, #83139, .F. ) ;
#140451 = AXIS2_PLACEMENT_3D ( 'NONE', #31243, #51570, #95763 ) ;
#140452 = ORIENTED_EDGE ( 'NONE', *, *, #18633, .T. ) ;
#140453 = CARTESIAN_POINT ( 'NONE',  ( 160.0000000000000000, 0.000000000000000000, 0.000000000000000000 ) ) ;
#140454 = DIRECTION ( 'NONE',  ( 1.369518533665900312E-16, -1.000000000000000000, 0.000000000000000000 ) ) ;
#140455 = VECTOR ( 'NONE', #105788, 1000.000000000000000 ) ;
#140456 = EDGE_CURVE ( 'NONE', #30730, #99209, #19637, .T. ) ;
#140457 = DIRECTION ( 'NONE',  ( -0.6830127018922180770, -0.6830127018922204085, -0.2588190451025213501 ) ) ;
#140458 = EDGE_LOOP ( 'NONE', ( #4513, #31819, #71424, #123715 ) ) ;
#140459 = CARTESIAN_POINT ( 'NONE',  ( 2.999999999999999556, -47.62213595499959951, 36.92500000000000426 ) ) ;
#140460 = ORIENTED_EDGE ( 'NONE', *, *, #69458, .F. ) ;
#140461 = CARTESIAN_POINT ( 'NONE',  ( 2.749569808101886004, 3.967499999999998916, 6.871911579029510442 ) ) ;
#140462 = LINE ( 'NONE', #6334, #104873 ) ;
#140463 = DIRECTION ( 'NONE',  ( 0.7071067811865487940, 0.7071067811865463515, 0.000000000000000000 ) ) ;
#140464 = ORIENTED_EDGE ( 'NONE', *, *, #127417, .T. ) ;
#140465 = ORIENTED_EDGE ( 'NONE', *, *, #75911, .F. ) ;
#140466 = VECTOR ( 'NONE', #138033, 1000.000000000000000 ) ;
#140467 = ORIENTED_EDGE ( 'NONE', *, *, #108227, .F. ) ;
#140468 = DIRECTION ( 'NONE',  ( -0.7071067811865487940, 0.7071067811865463515, 0.000000000000000000 ) ) ;
#140469 = LINE ( 'NONE', #85368, #106610 ) ;
#140470 = DIRECTION ( 'NONE',  ( -0.6830127018922181881, 0.6830127018922202975, -0.2588190451025214056 ) ) ;
#140471 = CARTESIAN_POINT ( 'NONE',  ( -14.58838509405158135, 22.22500000000000142, 4.777194822843813249 ) ) ;
#140473 = ADVANCED_FACE ( 'NONE', ( #53721 ), #42846, .T. ) ;
#140472 = LINE ( 'NONE', #61536, #6531 ) ;
#140474 = CARTESIAN_POINT ( 'NONE',  ( 34.49999999999975842, -13.53574439159937093, 4.994342998332162331 ) ) ;
#140475 = DIRECTION ( 'NONE',  ( 0.6830127018922180770, -0.6830127018922204085, -0.2588190451025213501 ) ) ;
#140476 = EDGE_CURVE ( 'NONE', #23492, #128513, #65323, .T. ) ;
#140477 = CARTESIAN_POINT ( 'NONE',  ( 31.35459685856476497, -1.637169565754161615, 6.110000000000000320 ) ) ;
#140478 = CARTESIAN_POINT ( 'NONE',  ( -12.72281430457050710, -21.72500000000000142, 5.000000000000000000 ) ) ;
#140479 = ORIENTED_EDGE ( 'NONE', *, *, #21487, .T. ) ;
#140480 = FACE_OUTER_BOUND ( 'NONE', #37413, .T. ) ;
#140481 = CARTESIAN_POINT ( 'NONE',  ( 39.18398860626899705, 28.73617430169814568, 5.000000000000000000 ) ) ;
#140482 = EDGE_LOOP ( 'NONE', ( #86947, #90246, #122703, #91020 ) ) ;
#140483 = DIRECTION ( 'NONE',  ( -1.000000000000000000, 0.000000000000000000, 0.000000000000000000 ) ) ;
#140485 = ORIENTED_EDGE ( 'NONE', *, *, #113401, .T. ) ;
#140484 = CARTESIAN_POINT ( 'NONE',  ( 55.62203754808112421, -51.91654526991841578, -39.52330221398148069 ) ) ;
#140486 = ADVANCED_FACE ( 'NONE', ( #121086 ), #109506, .F. ) ;
#140487 = LINE ( 'NONE', #54245, #76960 ) ;
#140488 = DIRECTION ( 'NONE',  ( 1.734723475976806848E-16, -1.000000000000000000, 0.000000000000000000 ) ) ;
#140489 = EDGE_LOOP ( 'NONE', ( #48990, #121380, #55026, #16628 ) ) ;
#140490 = LINE ( 'NONE', #62974, #132344 ) ;
#140491 = ORIENTED_EDGE ( 'NONE', *, *, #132746, .F. ) ;
#140492 = VECTOR ( 'NONE', #140390, 1000.000000000000000 ) ;
#140494 = VECTOR ( 'NONE', #76218, 1000.000000000000000 ) ;
#140493 = PRODUCT_RELATED_PRODUCT_CATEGORY ( 'part', '', ( #96739 ) ) ;
#140495 = CARTESIAN_POINT ( 'NONE',  ( 93.41252705046289861, -7.949999999999998401, -4.867971026610728450E-16 ) ) ;
#140497 = CARTESIAN_POINT ( 'NONE',  ( 124.7666937171295558, -7.949999999999999289, 2.130196079827424427 ) ) ;
#140496 = AXIS2_PLACEMENT_3D ( 'NONE', #14296, #91849, #111465 ) ;
#140498 = DIRECTION ( 'NONE',  ( -0.000000000000000000, -0.3543493200069152693, 0.9351131265310292928 ) ) ;
#140499 = CARTESIAN_POINT ( 'NONE',  ( 34.49999999999976552, 18.05432934483075513, 4.994342998332162331 ) ) ;
#140500 = CARTESIAN_POINT ( 'NONE',  ( -15.18398860626900237, 28.73617430169797871, 5.000000000000000000 ) ) ;
#140501 = DIRECTION ( 'NONE',  ( 0.7071067811865487940, 0.7071067811865463515, 0.000000000000000000 ) ) ;
#140502 = AXIS2_PLACEMENT_3D ( 'NONE', #75306, #76744, #97752 ) ;
#140503 = CARTESIAN_POINT ( 'NONE',  ( 17.99451991528748351, 28.92564299267950645, 4.000000000000000000 ) ) ;
#140504 = CARTESIAN_POINT ( 'NONE',  ( 8.020833333333333925, -6.094999999999989981, -1.633150327867689100 ) ) ;
#140505 = CARTESIAN_POINT ( 'NONE',  ( 17.04123647476855652, 0.000000000000000000, 7.934999999999990727 ) ) ;
#140506 = VECTOR ( 'NONE', #121983, 999.9999999999998863 ) ;
#140507 = CARTESIAN_POINT ( 'NONE',  ( -72.48921356237309510, -27.52281430457106026, 5.000000000000000000 ) ) ;
#140508 = LINE ( 'NONE', #137687, #131209 ) ;
#140509 = ORIENTED_EDGE ( 'NONE', *, *, #91494, .T. ) ;
#140510 = EDGE_CURVE ( 'NONE', #126872, #117172, #10869, .T. ) ;
#140511 = EDGE_LOOP ( 'NONE', ( #175, #134798, #53975 ) ) ;
#140512 =( NAMED_UNIT ( * ) PLANE_ANGLE_UNIT ( ) SI_UNIT ( $, .RADIAN. ) );
#140513 = EDGE_LOOP ( 'NONE', ( #92213, #13905, #137336, #18913 ) ) ;
#140514 = DIRECTION ( 'NONE',  ( -0.7071067811865486830, -0.7071067811865464625, -0.000000000000000000 ) ) ;
#140515 = DIRECTION ( 'NONE',  ( 1.000000000000000000, 0.000000000000000000, 0.000000000000000000 ) ) ;
#140516 = CARTESIAN_POINT ( 'NONE',  ( 35.91508676806215306, -12.74070752338415957, 18.74364270924362685 ) ) ;
#140517 = ORIENTED_EDGE ( 'NONE', *, *, #80806, .T. ) ;
#140518 = CARTESIAN_POINT ( 'NONE',  ( -28.49999999999979750, -4.533600742197692490, 5.000000000000000000 ) ) ;
#140519 = LINE ( 'NONE', #41210, #39629 ) ;
#140520 = LINE ( 'NONE', #41212, #122973 ) ;
#140521 =( NAMED_UNIT ( * ) SI_UNIT ( $, .STERADIAN. ) SOLID_ANGLE_UNIT ( ) );
#140523 = ORIENTED_EDGE ( 'NONE', *, *, #66274, .F. ) ;
#140522 = LINE ( 'NONE', #18002, #84516 ) ;
#140524 = CARTESIAN_POINT ( 'NONE',  ( -60.18398860626900415, 28.73617430169829490, 5.000000000000000000 ) ) ;
#140525 = AXIS2_PLACEMENT_3D ( 'NONE', #38472, #83410, #115261 ) ;
#140526 = CARTESIAN_POINT ( 'NONE',  ( 0.000000000000000000, 15.45873954670184780, -0.03131636524294264395 ) ) ;
#140527 = DIRECTION ( 'NONE',  ( -0.7071067811865487940, 0.7071067811865463515, -0.000000000000000000 ) ) ;
#140528 = FACE_OUTER_BOUND ( 'NONE', #86659, .T. ) ;
#140529 = PLANE ( 'NONE',  #93843 ) ;
#140530 = LINE ( 'NONE', #129655, #30634 ) ;
#140531 = ORIENTED_EDGE ( 'NONE', *, *, #31623, .F. ) ;
#140532 = ORIENTED_EDGE ( 'NONE', *, *, #48078, .T. ) ;
#140533 = EDGE_LOOP ( 'NONE', ( #122001, #68117, #34979, #7918 ) ) ;
#140534 = ADVANCED_FACE ( 'NONE', ( #132728 ), #113059, .F. ) ;
#140535 = CARTESIAN_POINT ( 'NONE',  ( 105.0004301918981184, -3.055000000000002380, 5.291415217122920289 ) ) ;
#140536 = VECTOR ( 'NONE', #95113, 1000.000000000000000 ) ;
#140537 = ORIENTED_EDGE ( 'NONE', *, *, #34063, .T. ) ;
#140538 = ADVANCED_FACE ( 'NONE', ( #68196 ), #111656, .F. ) ;
#140539 = CARTESIAN_POINT ( 'NONE',  ( 128.5279624519181141, -51.91654526992253693, 39.52330221397851062 ) ) ;
#140540 = AXIS2_PLACEMENT_3D ( 'NONE', #54294, #32518, #120933 ) ;
#140541 = DIRECTION ( 'NONE',  ( 0.7071067811865487940, 0.7071067811865463515, -0.000000000000000000 ) ) ;
#140542 = ORIENTED_EDGE ( 'NONE', *, *, #104357, .T. ) ;
#140543 = EDGE_CURVE ( 'NONE', #7434, #70301, #35560, .T. ) ;
#140544 = EDGE_CURVE ( 'NONE', #786, #41180, #141314, .T. ) ;
#140545 = DIRECTION ( 'NONE',  ( 0.7071067811865487940, 0.7071067811865463515, -0.000000000000000000 ) ) ;
#140546 = LINE ( 'NONE', #128963, #72125 ) ;
#140547 = CARTESIAN_POINT ( 'NONE',  ( 93.09959685856479439, -6.109999999999997655, -1.637169565754160283 ) ) ;
#140548 = EDGE_LOOP ( 'NONE', ( #109423, #6257, #112080, #29366 ) ) ;
#140549 = CARTESIAN_POINT ( 'NONE',  ( 22.22840764549667725, 9.139736423841732040E-16, 0.000000000000000000 ) ) ;
#140550 = FACE_OUTER_BOUND ( 'NONE', #64494, .T. ) ;
#140551 = AXIS2_PLACEMENT_3D ( 'NONE', #71016, #72465, #61576 ) ;
#140552 = CARTESIAN_POINT ( 'NONE',  ( -24.00548008471250938, 28.92564299267921513, 4.000000000000000000 ) ) ;
#140553 = DIRECTION ( 'NONE',  ( -0.6830127018922181881, 0.6830127018922202975, -0.2588190451025214056 ) ) ;
#140554 = EDGE_LOOP ( 'NONE', ( #37756, #77794, #4698, #44348 ) ) ;
#140555 = ORIENTED_EDGE ( 'NONE', *, *, #80027, .F. ) ;
#140556 = ADVANCED_FACE ( 'NONE', ( #3565 ), #14478, .T. ) ;
#140557 = VECTOR ( 'NONE', #113663, 1000.000000000000227 ) ;
#140558 = ORIENTED_EDGE ( 'NONE', *, *, #136296, .F. ) ;
#140559 = DIRECTION ( 'NONE',  ( -0.3543493200069162685, -0.000000000000000000, -0.9351131265310288487 ) ) ;
#140560 = ADVANCED_FACE ( 'NONE', ( #13026 ), #57303, .F. ) ;
#140561 = DIRECTION ( 'NONE',  ( -0.7071067811865486830, 0.7071067811865464625, 0.000000000000000000 ) ) ;
#140562 = CARTESIAN_POINT ( 'NONE',  ( 5.171236474768553748, 0.000000000000000000, 7.934999999999990727 ) ) ;
#140563 = DIRECTION ( 'NONE',  ( -1.000000000000000000, -1.224606353822377258E-16, -0.000000000000000000 ) ) ;
#140564 = EDGE_CURVE ( 'NONE', #89344, #137750, #143135, .T. ) ;
#140565 = EDGE_LOOP ( 'NONE', ( #135621, #110772, #18522, #75632 ) ) ;
#140566 = AXIS2_PLACEMENT_3D ( 'NONE', #118285, #76238, #42196 ) ;
#140567 = ORIENTED_EDGE ( 'NONE', *, *, #74786, .F. ) ;
#140568 = DIRECTION ( 'NONE',  ( -0.3543493200069163240, 0.000000000000000000, -0.9351131265310288487 ) ) ;
#140569 = ORIENTED_EDGE ( 'NONE', *, *, #26988, .F. ) ;
#140570 = ORIENTED_EDGE ( 'NONE', *, *, #82971, .F. ) ;
#140571 = EDGE_CURVE ( 'NONE', #12215, #31122, #59444, .T. ) ;
#140572 = CARTESIAN_POINT ( 'NONE',  ( 1.516262732464673579, -0.4000000000000004108, 2.467792535850613866 ) ) ;
#140573 = ORIENTED_EDGE ( 'NONE', *, *, #85879, .T. ) ;
#140574 = CARTESIAN_POINT ( 'NONE',  ( 2.999999999999981792, 4.931123077392134846, 4.000000000000000000 ) ) ;
#140575 = DIRECTION ( 'NONE',  ( 0.7071067811865487940, 0.7071067811865463515, -0.000000000000000000 ) ) ;
#140576 = EDGE_CURVE ( 'NONE', #33542, #36959, #114483, .T. ) ;
#140577 = CARTESIAN_POINT ( 'NONE',  ( -12.20000000000000284, -25.33999999999998565, -1.334633813784589971E-30 ) ) ;
#140578 = PLANE ( 'NONE',  #141555 ) ;
#140579 = VERTEX_POINT ( 'NONE', #91351 ) ;
#140580 = DIRECTION ( 'NONE',  ( 0.7071067811865486830, -0.7071067811865464625, -0.000000000000000000 ) ) ;
#140582 = CARTESIAN_POINT ( 'NONE',  ( 8.510786437626906675, -27.52281430457049183, 5.000000000000000000 ) ) ;
#140581 = VECTOR ( 'NONE', #96314, 1000.000000000000000 ) ;
#140583 = VERTEX_POINT ( 'NONE', #125392 ) ;
#140584 = CARTESIAN_POINT ( 'NONE',  ( 25.39999999999999858, -1.505985334814471388, -7.801307722062915673 ) ) ;
#140585 = CARTESIAN_POINT ( 'NONE',  ( -25.49999999999982236, 21.43112307739196254, 4.000000000000000000 ) ) ;
#140586 = CARTESIAN_POINT ( 'NONE',  ( 18.79653912142945060, -2.499999999999996447, 0.000000000000000000 ) ) ;
#140587 = VERTEX_POINT ( 'NONE', #720 ) ;
#140588 = FACE_OUTER_BOUND ( 'NONE', #56504, .T. ) ;
#140589 = ORIENTED_EDGE ( 'NONE', *, *, #1908, .F. ) ;
#140590 = ORIENTED_EDGE ( 'NONE', *, *, #100954, .F. ) ;
#140591 = VECTOR ( 'NONE', #56987, 999.9999999999998863 ) ;
#140592 = VERTEX_POINT ( 'NONE', #45015 ) ;
#140593 = AXIS2_PLACEMENT_3D ( 'NONE', #18413, #117728, #108272 ) ;
#140594 = EDGE_CURVE ( 'NONE', #70558, #16196, #79063, .T. ) ;
#140595 = VECTOR ( 'NONE', #40027, 1000.000000000000000 ) ;
#140596 = CARTESIAN_POINT ( 'NONE',  ( 30.24543019189811233, -5.291415217122918513, -3.055000000000000160 ) ) ;
#140597 = FILL_AREA_STYLE ('',( #96353 ) ) ;
#140598 = CARTESIAN_POINT ( 'NONE',  ( -13.41009064519824179, 9.759292476615621936, 11.28811694763775542 ) ) ;
#140599 = CARTESIAN_POINT ( 'NONE',  ( 12.51280225271498736, 3.061616997868383634E-16, -2.500000000000000444 ) ) ;
#140600 = CARTESIAN_POINT ( 'NONE',  ( 7.499999999999947597, 19.39370406404968605, 1.459788787078186489 ) ) ;
#140602 = DIRECTION ( 'NONE',  ( 0.6830127018922181881, 0.6830127018922202975, -0.2588190451025214056 ) ) ;
#140601 = CARTESIAN_POINT ( 'NONE',  ( -4.786780966966382778, 12.75929247661558996, 10.29404684609034071 ) ) ;
#140603 = AXIS2_PLACEMENT_3D ( 'NONE', #50524, #38228, #58605 ) ;
#140604 = CARTESIAN_POINT ( 'NONE',  ( -2.708222910169498565, -15.74070752338411694, 19.73771281079097051 ) ) ;
#140605 = FACE_OUTER_BOUND ( 'NONE', #68958, .T. ) ;
#140606 = CARTESIAN_POINT ( 'NONE',  ( -34.49999999999975842, -11.94567065516892690, 4.994342998332167660 ) ) ;
#140607 = CARTESIAN_POINT ( 'NONE',  ( 26.99999999999981881, -6.412538124160691133, 4.000000000000000000 ) ) ;
#140608 = EDGE_CURVE ( 'NONE', #97802, #130638, #23178, .T. ) ;
#140609 = ORIENTED_EDGE ( 'NONE', *, *, #64287, .T. ) ;
#140610 = ORIENTED_EDGE ( 'NONE', *, *, #90905, .T. ) ;
#140611 = ORIENTED_EDGE ( 'NONE', *, *, #51443, .F. ) ;
#140612 = EDGE_LOOP ( 'NONE', ( #128499, #27184, #113627, #50839 ) ) ;
#140613 = FACE_OUTER_BOUND ( 'NONE', #15980, .T. ) ;
#140614 = ORIENTED_EDGE ( 'NONE', *, *, #80357, .T. ) ;
#140615 =( BOUNDED_CURVE ( )  B_SPLINE_CURVE ( 2, ( #119540, #129725, #22370, #20237, #9337, #120990, #631, #65948, #76075, #30432, #74666, #118855, #120242, #65224, #66635, #110805, #107945, #109408, #76818, #110106, #20960, #8617, #10090, #52862, #98531, #142757, #87661, #32582, #99217, #143456, #44173, #47764, #100690, #4145, #123881, #35460, #91933, #2033, #46340, #124573, #23078, #89792, #90526, #102120, #1337, #80383, #57927, #134770, #15076, #69503, #79698, #2780, #78229, #89107, #136157, #12225, #133327, #78958, #24539, #14382, #67356, #59349, #47080, #102835, #68794, #112975, #91260, #103506, #34010, #101387, #36839, #122412, #13644, #70244, #45620, #58665, #111548, #56515, #68101, #25248, #81086, #135471, #36151, #113689, #134033, #114403, #125289, #34718, #3476, #123164, #25979, #23837, #112284, #12933, #57210, #29520, #62913, #84641, #117935, #94069, #81819, #16497, #82501, #18631, #73758, #126015, #139760, #28117, #116550, #93370, #38284, #107089, #139025, #73078, #40441, #106348, #128160, #126691, #15750, #92633, #117230, #27372, #7023, #60047, #72381, #17908, #60789, #51307, #48438, #128844, #49891, #138308, #95495, #49176, #26685, #17234, #136871, #61496, #37578, #70928, #71631, #104950, #115079, #105644, #104212, #6300, #115789, #4879, #137602, #5618, #127415, #38990, #83956, #83214, #94773, #50581, #39729, #28836, #62184, #75904, #142597, #119376, #10616, #7765, #96895, #54189, #141898, #9917, #76642, #118685, #20067, #41850, #121531, #132467, #85328, #99051, #131008, #120076, #52705, #141141, #22208, #96197, #19376, #86791, #54883, #43996, #109947, #31686, #98376, #43287, #86069, #65789, #63630, #20792, #120818, #64316, #143293, #66471, #88217, #9163, #97643, #33156, #107790, #52014, #130302, #42592, #21525, #8452, #75215, #30992, #108483, #77368, #65045, #53430, #109236, #87496, #41127, #140436, #129552, #131715, #32409, #30246, #74498, #46905, #56342, #1164, #112801, #67928, #122977, #91084, #133852, #34542, #123713, #458, #33844, #14198, #135305, #68618, #22908, #134588, #100520, #25065, #13461, #78768, #1851, #55595, #110636, #35986, #78060, #11313, #45446, #12762, #101932, #133162, #69321, #67172, #89626, #23659, #88943, #2595, #112115, #80215, #46158, #57743, #124399, #57037, #99783, #111364, #101210, #90337, #35285, #113506, #79526, #44751, #24371, #122237, #12054, #64074, #121993, #44497, #97377, #111110, #85809, #11801, #55350, #19833, #96650, #86551, #43049, #21978, #30749, #33610, #108241, #130783, #20536, #130047, #66227, #42341, #53938, #99525, #21281, #41592, #76387, #77810, #53178, #110400, #74977, #22662, #75669, #132204, #194, #121296, #10381, #9668, #64794, #141642, #31447, #32902, #109711, #140895, #119841, #87962, #108973, #98133, #131476, #66932, #119149, #132932, #8908, #142359, #87252, #11077, #32155, #120550, #65538, #54634, #98821, #77122, #143053, #88696, #43744, #28112, #4138, #70922, #138303, #106343, #95491, #17901, #38982, #6294, #50575, #93366, #117225, #26678, #83208, #28830, #27366, #62178, #73749, #139753, #60785, #115074, #7014, #15744, #117928, #104205, #49882, #128154, #60040, #126684, #4874, #71625, #51303, #72376, #49170, #116544, #38276, #92628, #40433, #84634, #127409, #128838, #59345, #29514, #103501, #82497, #137593, #48431, #136866, #94765, #37573, #115781, #17228, #81812, #126006, #16491, #104946, #5612, #61490, #94064, #139020, #105635, #39726, #83951, #73073, #98371, #77363, #88211, #64310, #52006, #43281, #8445, #18625, #54874, #52698, #63623, #9911, #132462, #65038, #20061, #130298, #109232, #87491, #10610, #76636, #142590, #96888, #129543, #62905, #131708, #33150, #107084, #21520, #141135, #7758, #41841, #109941, #43990, #99046, #32403, #54183, #120813, #19370, #96189, #42586, #140429, #86784, #41121, #143288, #86063, #65782, #30984, #85321, #75209, #30239, #119369, #108475, #74492, #118678, #97636, #107782, #9156, #53424, #141892, #131004, #31682, #75898, #120069, #20786, #67921, #124393, #34535, #78760, #13458, #55589, #88939, #36658, #69317, #2591, #122232, #123708, #23655, #47594, #101927, #122972, #134581, #110629, #121524, #80208, #44745, #22201, #111359, #112110, #46900, #99777, #58488, #133157, #12049, #45440, #11308, #91079, #91754, #66465, #133846, #25061, #453, #101204, #102661, #78053, #135302, #33836, #135982, #100514, #57737, #113500, #35981, #35281, #12756, #89618, #22902, #56335, #67166, #14192, #1158, #46151, #112795, #57031, #1844, #90332, #3305, #79520, #24364, #68610, #125102, #104779, #70064, #117066, #70757, #83777, #93191, #106175, #92451, #138132, #59861, #114227, #127991, #17741, #16313, #38116, #116375, #137424, #127233, #4692, #27207, #6849, #115608, #60607, #71452, #28672, #82335, #126517, #14905, #48258, #139590, #72920, #105473, #81635, #83038, #15582, #49721, #5439, #27935, #17065, #80903, #62016, #25785, #51132, #93896, #95327, #59179, #72205, #103330, #3977, #136687, #114904, #48991, #37391, #50415, #26513, #38818, #125838, #61331, #6136, #104035, #94601, #138856, #39551, #74313, #118501, #8285, #119904, #43112, #64863, #97455, #96717, #107624, #85158, #19202, #20609, #53239, #54702, #63459, #109045, #131534, #52534, #87319, #40274, #129373, #86621, #30815, #42412, #73590, #9734, #30061, #98882, #76458, #140962, #41663, #31510, #10445, #130848, #85878, #130117, #8979, #128677, #51845, #119213, #32224, #120627, #142425, #19894, #54004, #109775, #84483, #21345, #75043, #29346, #64142, #65606, #117759, #18446, #98198, #75732, #96034, #62729, #140271, #40956, #106909, #7589, #108308, #141707, #35823, #101753, #122795, #90158, #134404, #33673, #57567, #110462, #23478, #112633, #111182, #2412, #14009, #80049, #992, #89447, #46727, #269, #77185, #67742, #133681, #68455, #55412, #66998, #99590, #11868, #90906, #12594, #11135, #56872, #122061, #32968, #135136, #124223, #78586, #100340, #35103, #56156, #45977, #45276, #44566, #24899 ),
 .UNSPECIFIED., .F., .T. ) 
 B_SPLINE_CURVE_WITH_KNOTS ( ( 3, 2, 2, 2, 2, 2, 2, 2, 2, 2, 2, 2, 2, 2, 2, 2, 2, 2, 2, 2, 2, 2, 2, 2, 2, 2, 2, 2, 2, 2, 2, 2, 2, 2, 2, 2, 2, 2, 2, 2, 2, 2, 2, 2, 2, 2, 2, 2, 2, 2, 2, 2, 2, 2, 2, 2, 2, 2, 2, 2, 2, 2, 2, 2, 2, 2, 2, 2, 2, 2, 2, 2, 2, 2, 2, 2, 2, 2, 2, 2, 2, 2, 2, 2, 2, 2, 2, 2, 2, 2, 2, 2, 2, 2, 2, 2, 2, 2, 2, 2, 2, 2, 2, 2, 2, 2, 2, 2, 2, 2, 2, 2, 2, 2, 2, 2, 2, 2, 2, 2, 2, 2, 2, 2, 2, 2, 2, 2, 2, 2, 2, 2, 2, 2, 2, 2, 2, 2, 2, 2, 2, 2, 2, 2, 2, 2, 2, 2, 2, 2, 2, 2, 2, 2, 2, 2, 2, 2, 2, 2, 2, 2, 2, 2, 2, 2, 2, 2, 2, 2, 2, 2, 2, 2, 2, 2, 2, 2, 2, 2, 2, 2, 2, 2, 2, 2, 2, 2, 2, 2, 2, 2, 2, 2, 2, 2, 2, 2, 2, 2, 2, 2, 2, 2, 2, 2, 2, 2, 2, 2, 2, 2, 2, 2, 2, 2, 2, 2, 2, 2, 2, 2, 2, 2, 2, 2, 2, 2, 2, 2, 2, 2, 2, 2, 2, 2, 2, 2, 2, 2, 2, 2, 2, 2, 2, 2, 2, 2, 2, 2, 2, 2, 2, 2, 2, 2, 2, 2, 2, 2, 2, 2, 2, 2, 2, 2, 2, 2, 2, 2, 2, 2, 2, 2, 2, 2, 2, 2, 2, 2, 2, 2, 2, 2, 2, 2, 2, 2, 2, 2, 2, 2, 2, 2, 2, 2, 2, 2, 2, 2, 2, 2, 2, 2, 2, 2, 2, 2, 2, 2, 2, 2, 2, 2, 2, 2, 2, 2, 2, 2, 2, 2, 2, 2, 2, 2, 2, 2, 2, 2, 2, 2, 2, 2, 2, 2, 2, 2, 2, 2, 2, 2, 2, 2, 2, 2, 2, 2, 2, 2, 2, 3 ),
 ( 0.000000000000000000, 0.002777777777777777884, 0.005555555555555555768, 0.008333333333333333218, 0.01111111111111111154, 0.01388888888888888812, 0.01666666666666666644, 0.01944444444444444475, 0.02222222222222222307, 0.02500000000000000139, 0.02777777777777777624, 0.03055555555555555455, 0.03333333333333333287, 0.03611111111111110772, 0.03888888888888888951, 0.04166666666666666435, 0.04444444444444444614, 0.04722222222222222099, 0.05000000000000000278, 0.05277777777777777762, 0.05555555555555555247, 0.05833333333333333426, 0.06111111111111110911, 0.06388888888888888395, 0.06666666666666666574, 0.06944444444444444753, 0.07222222222222221544, 0.07499999999999999722, 0.07777777777777777901, 0.08055555555555556080, 0.08333333333333332871, 0.08611111111111111049, 0.08888888888888889228, 0.09166666666666666019, 0.09444444444444444198, 0.09722222222222222376, 0.1000000000000000056, 0.1027777777777777735, 0.1055555555555555552, 0.1083333333333333370, 0.1111111111111111049, 0.1138888888888888867, 0.1166666666666666685, 0.1194444444444444503, 0.1222222222222222182, 0.1250000000000000000, 0.1277777777777777679, 0.1305555555555555636, 0.1333333333333333315, 0.1361111111111110994, 0.1388888888888888951, 0.1416666666666666630, 0.1444444444444444309, 0.1472222222222222265, 0.1499999999999999944, 0.1527777777777777901, 0.1555555555555555580, 0.1583333333333333259, 0.1611111111111111216, 0.1638888888888888895, 0.1666666666666666574, 0.1694444444444444531, 0.1722222222222222210, 0.1750000000000000167, 0.1777777777777777846, 0.1805555555555555525, 0.1833333333333333204, 0.1861111111111111160, 0.1888888888888888840, 0.1916666666666666796, 0.1944444444444444475, 0.1972222222222222154, 0.2000000000000000111, 0.2027777777777777790, 0.2055555555555555469, 0.2083333333333333426, 0.2111111111111111105, 0.2138888888888888784, 0.2166666666666666741, 0.2194444444444444420, 0.2222222222222222099, 0.2249999999999999778, 0.2277777777777777735, 0.2305555555555555691, 0.2333333333333333370, 0.2361111111111111049, 0.2388888888888889006, 0.2416666666666666685, 0.2444444444444444364, 0.2472222222222222321, 0.2500000000000000000, 0.2527777777777777679, 0.2555555555555555358, 0.2583333333333333592, 0.2611111111111111271, 0.2638888888888888951, 0.2666666666666666630, 0.2694444444444444309, 0.2722222222222221988, 0.2750000000000000222, 0.2777777777777777901, 0.2805555555555555580, 0.2833333333333333259, 0.2861111111111110938, 0.2888888888888888618, 0.2916666666666666852, 0.2944444444444444531, 0.2972222222222222210, 0.2999999999999999889, 0.3027777777777777568, 0.3055555555555555802, 0.3083333333333333481, 0.3111111111111111160, 0.3138888888888888840, 0.3166666666666666519, 0.3194444444444444198, 0.3222222222222222432, 0.3250000000000000111, 0.3277777777777777790, 0.3305555555555555469, 0.3333333333333333148, 0.3361111111111111382, 0.3388888888888889062, 0.3416666666666666741, 0.3444444444444444420, 0.3472222222222222099, 0.3500000000000000333, 0.3527777777777778012, 0.3555555555555555691, 0.3583333333333333370, 0.3611111111111111049, 0.3638888888888888729, 0.3666666666666666408, 0.3694444444444444642, 0.3722222222222222321, 0.3750000000000000000, 0.3777777777777777679, 0.3805555555555555358, 0.3833333333333333592, 0.3861111111111111271, 0.3888888888888888951, 0.3916666666666666630, 0.3944444444444444309, 0.3972222222222221988, 0.4000000000000000222, 0.4027777777777777901, 0.4055555555555555580, 0.4083333333333333259, 0.4111111111111110938, 0.4138888888888888618, 0.4166666666666666852, 0.4194444444444444531, 0.4222222222222222210, 0.4249999999999999889, 0.4277777777777777568, 0.4305555555555555802, 0.4333333333333333481, 0.4361111111111111160, 0.4388888888888888840, 0.4416666666666666519, 0.4444444444444444198, 0.4472222222222222432, 0.4499999999999999556, 0.4527777777777777790, 0.4555555555555555469, 0.4583333333333333148, 0.4611111111111111382, 0.4638888888888889062, 0.4666666666666666741, 0.4694444444444444420, 0.4722222222222222099, 0.4749999999999999778, 0.4777777777777778012, 0.4805555555555555691, 0.4833333333333333370, 0.4861111111111111049, 0.4888888888888888729, 0.4916666666666666408, 0.4944444444444444642, 0.4972222222222222321, 0.5000000000000000000, 0.5027777777777777679, 0.5055555555555555358, 0.5083333333333333037, 0.5111111111111110716, 0.5138888888888888395, 0.5166666666666667185, 0.5194444444444444864, 0.5222222222222222543, 0.5250000000000000222, 0.5277777777777777901, 0.5305555555555555580, 0.5333333333333333259, 0.5361111111111110938, 0.5388888888888888618, 0.5416666666666666297, 0.5444444444444443976, 0.5472222222222222765, 0.5500000000000000444, 0.5527777777777778123, 0.5555555555555555802, 0.5583333333333333481, 0.5611111111111111160, 0.5638888888888888840, 0.5666666666666666519, 0.5694444444444444198, 0.5722222222222221877, 0.5749999999999999556, 0.5777777777777777235, 0.5805555555555556024, 0.5833333333333333703, 0.5861111111111112493, 0.5888888888888889062, 0.5916666666666666741, 0.5944444444444444420, 0.5972222222222222099, 0.5999999999999999778, 0.6027777777777777457, 0.6055555555555555136, 0.6083333333333332815, 0.6111111111111111605, 0.6138888888888889284, 0.6166666666666666963, 0.6194444444444444642, 0.6222222222222222321, 0.6250000000000000000, 0.6277777777777777679, 0.6305555555555555358, 0.6333333333333333037, 0.6361111111111110716, 0.6388888888888888395, 0.6416666666666667185, 0.6444444444444444864, 0.6472222222222222543, 0.6500000000000000222, 0.6527777777777777901, 0.6555555555555555580, 0.6583333333333333259, 0.6611111111111110938, 0.6638888888888888618, 0.6666666666666666297, 0.6694444444444443976, 0.6722222222222222765, 0.6750000000000000444, 0.6777777777777778123, 0.6805555555555555802, 0.6833333333333333481, 0.6861111111111111160, 0.6888888888888888840, 0.6916666666666666519, 0.6944444444444444198, 0.6972222222222221877, 0.7000000000000000666, 0.7027777777777777235, 0.7055555555555556024, 0.7083333333333333703, 0.7111111111111111382, 0.7138888888888889062, 0.7166666666666666741, 0.7194444444444444420, 0.7222222222222222099, 0.7249999999999999778, 0.7277777777777777457, 0.7305555555555555136, 0.7333333333333332815, 0.7361111111111111605, 0.7388888888888889284, 0.7416666666666666963, 0.7444444444444444642, 0.7472222222222222321, 0.7500000000000000000, 0.7527777777777777679, 0.7555555555555555358, 0.7583333333333333037, 0.7611111111111110716, 0.7638888888888888395, 0.7666666666666667185, 0.7694444444444444864, 0.7722222222222222543, 0.7750000000000000222, 0.7777777777777777901, 0.7805555555555555580, 0.7833333333333333259, 0.7861111111111110938, 0.7888888888888888618, 0.7916666666666666297, 0.7944444444444443976, 0.7972222222222222765, 0.8000000000000000444, 0.8027777777777778123, 0.8055555555555555802, 0.8083333333333333481, 0.8111111111111111160, 0.8138888888888888840, 0.8166666666666666519, 0.8194444444444444198, 0.8222222222222221877, 0.8249999999999999556, 0.8277777777777777235, 0.8305555555555556024, 0.8333333333333333703, 0.8361111111111111382, 0.8388888888888889062, 0.8416666666666666741, 0.8444444444444444420, 0.8472222222222222099, 0.8499999999999999778, 0.8527777777777777457, 0.8555555555555555136, 0.8583333333333332815, 0.8611111111111111605, 0.8638888888888889284, 0.8666666666666666963, 0.8694444444444444642, 0.8722222222222222321, 0.8750000000000000000, 0.8777777777777777679, 0.8805555555555555358, 0.8833333333333333037, 0.8861111111111110716, 0.8888888888888888395, 0.8916666666666667185, 0.8944444444444444864, 0.8972222222222222543, 0.8999999999999999112, 0.9027777777777777901, 0.9055555555555555580, 0.9083333333333333259, 0.9111111111111110938, 0.9138888888888888618, 0.9166666666666666297, 0.9194444444444443976, 0.9222222222222222765, 0.9250000000000000444, 0.9277777777777778123, 0.9305555555555555802, 0.9333333333333333481, 0.9361111111111111160, 0.9388888888888888840, 0.9416666666666666519, 0.9444444444444444198, 0.9472222222222221877, 0.9499999999999999556, 0.9527777777777777235, 0.9555555555555556024, 0.9583333333333333703, 0.9611111111111111382, 0.9638888888888889062, 0.9666666666666666741, 0.9694444444444444420, 0.9722222222222222099, 0.9749999999999999778 ),
 .UNSPECIFIED. ) 
 CURVE ( )  GEOMETRIC_REPRESENTATION_ITEM ( )  RATIONAL_B_SPLINE_CURVE ( ( 1.000000000000000000, 0.9659258262890683122, 1.000000000000000000, 0.9659258262890683122, 1.000000000000000000, 0.9659258262890683122, 1.000000000000000000, 0.9659258262890683122, 1.000000000000000000, 0.9659258262890683122, 1.000000000000000000, 0.9659258262890683122, 1.000000000000000000, 0.9659258262890683122, 1.000000000000000000, 0.9659258262890683122, 1.000000000000000000, 0.9659258262890683122, 1.000000000000000000, 0.9659258262890683122, 1.000000000000000000, 0.9659258262890683122, 1.000000000000000000, 0.9659258262890683122, 1.000000000000000000, 0.9659258262890683122, 1.000000000000000000, 0.9659258262890683122, 1.000000000000000000, 0.9659258262890683122, 1.000000000000000000, 0.9659258262890683122, 1.000000000000000000, 0.9659258262890683122, 1.000000000000000000, 0.9659258262890683122, 1.000000000000000000, 0.9659258262890683122, 1.000000000000000000, 0.9659258262890683122, 1.000000000000000000, 0.9659258262890683122, 1.000000000000000000, 0.9659258262890683122, 1.000000000000000000, 0.9659258262890683122, 1.000000000000000000, 0.9659258262890683122, 1.000000000000000000, 0.9659258262890683122, 1.000000000000000000, 0.9659258262890683122, 1.000000000000000000, 0.9659258262890683122, 1.000000000000000000, 0.9659258262890683122, 1.000000000000000000, 0.9659258262890683122, 1.000000000000000000, 0.9659258262890683122, 1.000000000000000000, 0.9659258262890683122, 1.000000000000000000, 0.9659258262890683122, 1.000000000000000000, 0.9659258262890683122, 1.000000000000000000, 0.9659258262890683122, 1.000000000000000000, 0.9659258262890683122, 1.000000000000000000, 0.9659258262890683122, 1.000000000000000000, 0.9659258262890683122, 1.000000000000000000, 0.9659258262890683122, 1.000000000000000000, 0.9659258262890683122, 1.000000000000000000, 0.9659258262890683122, 1.000000000000000000, 0.9659258262890683122, 1.000000000000000000, 0.9659258262890683122, 1.000000000000000000, 0.9659258262890683122, 1.000000000000000000, 0.9659258262890683122, 1.000000000000000000, 0.9659258262890683122, 1.000000000000000000, 0.9659258262890683122, 1.000000000000000000, 0.9659258262890683122, 1.000000000000000000, 0.9659258262890683122, 1.000000000000000000, 0.9659258262890683122, 1.000000000000000000, 0.9659258262890683122, 1.000000000000000000, 0.9659258262890683122, 1.000000000000000000, 0.9659258262890683122, 1.000000000000000000, 0.9659258262890683122, 1.000000000000000000, 0.9659258262890683122, 1.000000000000000000, 0.9659258262890683122, 1.000000000000000000, 0.9659258262890683122, 1.000000000000000000, 0.9659258262890683122, 1.000000000000000000, 0.9659258262890683122, 1.000000000000000000, 0.9659258262890683122, 1.000000000000000000, 0.9659258262890683122, 1.000000000000000000, 0.9659258262890683122, 1.000000000000000000, 0.9659258262890683122, 1.000000000000000000, 0.9659258262890683122, 1.000000000000000000, 0.9659258262890683122, 1.000000000000000000, 0.9659258262890683122, 1.000000000000000000, 0.9659258262890683122, 1.000000000000000000, 0.9659258262890683122, 1.000000000000000000, 0.9659258262890683122, 1.000000000000000000, 0.9659258262890683122, 1.000000000000000000, 0.9659258262890683122, 1.000000000000000000, 0.9659258262890683122, 1.000000000000000000, 0.9659258262890683122, 1.000000000000000000, 0.9659258262890683122, 1.000000000000000000, 0.9659258262890683122, 1.000000000000000000, 0.9659258262890683122, 1.000000000000000000, 0.9659258262890683122, 1.000000000000000000, 0.9659258262890683122, 1.000000000000000000, 0.9659258262890683122, 1.000000000000000000, 0.9659258262890683122, 1.000000000000000000, 0.9659258262890683122, 1.000000000000000000, 0.9659258262890683122, 1.000000000000000000, 0.9659258262890683122, 1.000000000000000000, 0.9659258262890683122, 1.000000000000000000, 0.9659258262890683122, 1.000000000000000000, 0.9659258262890683122, 1.000000000000000000, 0.9659258262890683122, 1.000000000000000000, 0.9659258262890683122, 1.000000000000000000, 0.9659258262890683122, 1.000000000000000000, 0.9659258262890683122, 1.000000000000000000, 0.9659258262890683122, 1.000000000000000000, 0.9659258262890683122, 1.000000000000000000, 0.9659258262890683122, 1.000000000000000000, 0.9659258262890683122, 1.000000000000000000, 0.9659258262890683122, 1.000000000000000000, 0.9659258262890683122, 1.000000000000000000, 0.9659258262890683122, 1.000000000000000000, 0.9659258262890683122, 1.000000000000000000, 0.9659258262890683122, 1.000000000000000000, 0.9659258262890683122, 1.000000000000000000, 0.9659258262890683122, 1.000000000000000000, 0.9659258262890683122, 1.000000000000000000, 0.9659258262890683122, 1.000000000000000000, 0.9659258262890683122, 1.000000000000000000, 0.9659258262890683122, 1.000000000000000000, 0.9659258262890683122, 1.000000000000000000, 0.9659258262890683122, 1.000000000000000000, 0.9659258262890683122, 1.000000000000000000, 0.9659258262890683122, 1.000000000000000000, 0.9659258262890683122, 1.000000000000000000, 0.9659258262890683122, 1.000000000000000000, 0.9659258262890683122, 1.000000000000000000, 0.9659258262890683122, 1.000000000000000000, 0.9659258262890683122, 1.000000000000000000, 0.9659258262890683122, 1.000000000000000000, 0.9659258262890683122, 1.000000000000000000, 0.9659258262890683122, 1.000000000000000000, 0.9659258262890683122, 1.000000000000000000, 0.9659258262890683122, 1.000000000000000000, 0.9659258262890683122, 1.000000000000000000, 0.9659258262890683122, 1.000000000000000000, 0.9659258262890683122, 1.000000000000000000, 0.9659258262890683122, 1.000000000000000000, 0.9659258262890683122, 1.000000000000000000, 0.9659258262890683122, 1.000000000000000000, 0.9659258262890683122, 1.000000000000000000, 0.9659258262890683122, 1.000000000000000000, 0.9659258262890683122, 1.000000000000000000, 0.9659258262890683122, 1.000000000000000000, 0.9659258262890683122, 1.000000000000000000, 0.9659258262890683122, 1.000000000000000000, 0.9659258262890683122, 1.000000000000000000, 0.9659258262890683122, 1.000000000000000000, 0.9659258262890683122, 1.000000000000000000, 0.9659258262890683122, 1.000000000000000000, 0.9659258262890683122, 1.000000000000000000, 0.9659258262890683122, 1.000000000000000000, 0.9659258262890683122, 1.000000000000000000, 0.9659258262890683122, 1.000000000000000000, 0.9659258262890683122, 1.000000000000000000, 0.9659258262890683122, 1.000000000000000000, 0.9659258262890683122, 1.000000000000000000, 0.9659258262890683122, 1.000000000000000000, 0.9659258262890683122, 1.000000000000000000, 0.9659258262890683122, 1.000000000000000000, 0.9659258262890683122, 1.000000000000000000, 0.9659258262890683122, 1.000000000000000000, 0.9659258262890683122, 1.000000000000000000, 0.9659258262890683122, 1.000000000000000000, 0.9659258262890683122, 1.000000000000000000, 0.9659258262890683122, 1.000000000000000000, 0.9659258262890683122, 1.000000000000000000, 0.9659258262890683122, 1.000000000000000000, 0.9659258262890683122, 1.000000000000000000, 0.9659258262890683122, 1.000000000000000000, 0.9659258262890683122, 1.000000000000000000, 0.9659258262890683122, 1.000000000000000000, 0.9659258262890683122, 1.000000000000000000, 0.9659258262890683122, 1.000000000000000000, 0.9659258262890683122, 1.000000000000000000, 0.9659258262890683122, 1.000000000000000000, 0.9659258262890683122, 1.000000000000000000, 0.9659258262890683122, 1.000000000000000000, 0.9659258262890683122, 1.000000000000000000, 0.9659258262890683122, 1.000000000000000000, 0.9659258262890683122, 1.000000000000000000, 0.9659258262890683122, 1.000000000000000000, 0.9659258262890683122, 1.000000000000000000, 0.9659258262890683122, 1.000000000000000000, 0.9659258262890683122, 1.000000000000000000, 0.9659258262890683122, 1.000000000000000000, 0.9659258262890683122, 1.000000000000000000, 0.9659258262890683122, 1.000000000000000000, 0.9659258262890683122, 1.000000000000000000, 0.9659258262890683122, 1.000000000000000000, 0.9659258262890683122, 1.000000000000000000, 0.9659258262890683122, 1.000000000000000000, 0.9659258262890683122, 1.000000000000000000, 0.9659258262890683122, 1.000000000000000000, 0.9659258262890683122, 1.000000000000000000, 0.9659258262890683122, 1.000000000000000000, 0.9659258262890683122, 1.000000000000000000, 0.9659258262890683122, 1.000000000000000000, 0.9659258262890683122, 1.000000000000000000, 0.9659258262890683122, 1.000000000000000000, 0.9659258262890683122, 1.000000000000000000, 0.9659258262890683122, 1.000000000000000000, 0.9659258262890683122, 1.000000000000000000, 0.9659258262890683122, 1.000000000000000000, 0.9659258262890683122, 1.000000000000000000, 0.9659258262890683122, 1.000000000000000000, 0.9659258262890683122, 1.000000000000000000, 0.9659258262890683122, 1.000000000000000000, 0.9659258262890683122, 1.000000000000000000, 0.9659258262890683122, 1.000000000000000000, 0.9659258262890683122, 1.000000000000000000, 0.9659258262890683122, 1.000000000000000000, 0.9659258262890683122, 1.000000000000000000, 0.9659258262890683122, 1.000000000000000000, 0.9659258262890683122, 1.000000000000000000, 0.9659258262890683122, 1.000000000000000000, 0.9659258262890683122, 1.000000000000000000, 0.9659258262890683122, 1.000000000000000000, 0.9659258262890683122, 1.000000000000000000, 0.9659258262890683122, 1.000000000000000000, 0.9659258262890683122, 1.000000000000000000, 0.9659258262890683122, 1.000000000000000000, 0.9659258262890683122, 1.000000000000000000, 0.9659258262890683122, 1.000000000000000000, 0.9659258262890683122, 1.000000000000000000, 0.9659258262890683122, 1.000000000000000000, 0.9659258262890683122, 1.000000000000000000, 0.9659258262890683122, 1.000000000000000000, 0.9659258262890683122, 1.000000000000000000, 0.9659258262890683122, 1.000000000000000000, 0.9659258262890683122, 1.000000000000000000, 0.9659258262890683122, 1.000000000000000000, 0.9659258262890683122, 1.000000000000000000, 0.9659258262890683122, 1.000000000000000000, 0.9659258262890683122, 1.000000000000000000, 0.9659258262890683122, 1.000000000000000000, 0.9659258262890683122, 1.000000000000000000, 0.9659258262890683122, 1.000000000000000000, 0.9659258262890683122, 1.000000000000000000, 0.9659258262890683122, 1.000000000000000000, 0.9659258262890683122, 1.000000000000000000, 0.9659258262890683122, 1.000000000000000000, 0.9659258262890683122, 1.000000000000000000, 0.9659258262890683122, 1.000000000000000000, 0.9659258262890683122, 1.000000000000000000, 0.9659258262890683122, 1.000000000000000000, 0.9659258262890683122, 1.000000000000000000, 0.9659258262890683122, 1.000000000000000000, 0.9659258262890683122, 1.000000000000000000, 0.9659258262890683122, 1.000000000000000000, 0.9659258262890683122, 1.000000000000000000, 0.9659258262890683122, 1.000000000000000000, 0.9659258262890683122, 1.000000000000000000, 0.9659258262890683122, 1.000000000000000000, 0.9659258262890683122, 1.000000000000000000, 0.9659258262890683122, 1.000000000000000000, 0.9659258262890683122, 1.000000000000000000, 0.9659258262890683122, 1.000000000000000000, 0.9659258262890683122, 1.000000000000000000, 0.9659258262890683122, 1.000000000000000000, 0.9659258262890683122, 1.000000000000000000, 0.9659258262890683122, 1.000000000000000000, 0.9659258262890683122, 1.000000000000000000, 0.9659258262890683122, 1.000000000000000000, 0.9659258262890683122, 1.000000000000000000, 0.9659258262890683122, 1.000000000000000000, 0.9659258262890683122, 1.000000000000000000, 0.9659258262890683122, 1.000000000000000000, 0.9659258262890683122, 1.000000000000000000, 0.9659258262890683122, 1.000000000000000000, 0.9659258262890683122, 1.000000000000000000, 0.9659258262890683122, 1.000000000000000000, 0.9659258262890683122, 1.000000000000000000, 0.9659258262890683122, 1.000000000000000000, 0.9659258262890683122, 1.000000000000000000, 0.9659258262890683122, 1.000000000000000000, 0.9659258262890683122, 1.000000000000000000, 0.9659258262890683122, 1.000000000000000000, 0.9659258262890683122, 1.000000000000000000, 0.9659258262890683122, 1.000000000000000000, 0.9659258262890683122, 1.000000000000000000, 0.9659258262890683122, 1.000000000000000000, 0.9659258262890683122, 1.000000000000000000, 0.9659258262890683122, 1.000000000000000000, 0.9659258262890683122, 1.000000000000000000, 0.9659258262890683122, 1.000000000000000000, 0.9659258262890683122, 1.000000000000000000, 0.9659258262890683122, 1.000000000000000000, 0.9659258262890683122, 1.000000000000000000, 0.9659258262890683122, 1.000000000000000000, 0.9659258262890683122, 1.000000000000000000, 0.9659258262890683122, 1.000000000000000000, 0.9659258262890683122, 1.000000000000000000, 0.9659258262890683122, 1.000000000000000000, 0.9659258262890683122, 1.000000000000000000, 0.9659258262890683122, 1.000000000000000000, 0.9659258262890683122, 1.000000000000000000, 0.9659258262890683122, 1.000000000000000000, 0.9659258262890683122, 1.000000000000000000, 0.9659258262890683122, 1.000000000000000000, 0.9659258262890683122, 1.000000000000000000, 0.9659258262890683122, 1.000000000000000000, 0.9659258262890683122, 1.000000000000000000, 0.9659258262890683122, 1.000000000000000000, 0.9659258262890683122, 1.000000000000000000, 0.9659258262890683122, 1.000000000000000000, 0.9659258262890683122, 1.000000000000000000, 0.9659258262890683122, 1.000000000000000000, 0.9659258262890683122, 1.000000000000000000, 0.9659258262890683122, 1.000000000000000000, 0.9659258262890683122, 1.000000000000000000, 0.9659258262890683122, 1.000000000000000000, 0.9659258262890683122, 1.000000000000000000, 0.9659258262890683122, 1.000000000000000000, 0.9659258262890683122, 1.000000000000000000, 0.9659258262890683122, 1.000000000000000000, 0.9659258262890683122, 1.000000000000000000, 0.9659258262890683122, 1.000000000000000000, 0.9659258262890683122, 1.000000000000000000, 0.9659258262890683122, 1.000000000000000000, 0.9659258262890683122, 1.000000000000000000, 0.9659258262890683122, 1.000000000000000000, 0.9659258262890683122, 1.000000000000000000, 0.9659258262890683122, 1.000000000000000000, 0.9659258262890683122, 1.000000000000000000, 0.9659258262890683122, 1.000000000000000000, 0.9659258262890683122, 1.000000000000000000, 0.9659258262890683122, 1.000000000000000000, 0.9659258262890683122, 1.000000000000000000, 0.9659258262890683122, 1.000000000000000000, 0.9659258262890683122, 1.000000000000000000, 0.9659258262890683122, 1.000000000000000000, 0.9659258262890683122, 1.000000000000000000, 0.9659258262890683122, 1.000000000000000000, 0.9659258262890683122, 1.000000000000000000, 0.9659258262890683122, 1.000000000000000000, 0.9659258262890683122, 1.000000000000000000, 0.9659258262890683122, 1.000000000000000000, 0.9659258262890683122, 1.000000000000000000, 0.9659258262890683122, 1.000000000000000000, 0.9659258262890683122, 1.000000000000000000, 0.9659258262890683122, 1.000000000000000000, 0.9659258262890683122, 1.000000000000000000, 0.9659258262890683122, 1.000000000000000000, 0.9659258262890683122, 1.000000000000000000, 0.9659258262890683122, 1.000000000000000000, 0.9659258262890683122, 1.000000000000000000, 0.9659258262890683122, 1.000000000000000000, 0.9659258262890683122, 1.000000000000000000, 0.9659258262890683122, 1.000000000000000000, 0.9659258262890683122, 1.000000000000000000, 0.9659258262890683122, 1.000000000000000000, 0.9659258262890683122, 1.000000000000000000, 0.9659258262890683122, 1.000000000000000000, 0.9659258262890683122, 1.000000000000000000, 0.9659258262890683122, 1.000000000000000000, 0.9659258262890683122, 1.000000000000000000, 0.9659258262890683122, 1.000000000000000000, 0.9659258262890683122, 1.000000000000000000, 0.9659258262890683122, 1.000000000000000000, 0.9659258262890683122, 1.000000000000000000, 0.9659258262890683122, 1.000000000000000000, 0.9659258262890683122, 1.000000000000000000, 0.9659258262890683122, 1.000000000000000000, 0.9659258262890683122, 1.000000000000000000, 0.9659258262890683122, 1.000000000000000000, 0.9659258262890683122, 1.000000000000000000 ) ) 
 REPRESENTATION_ITEM ( '' )  );
#140616 = ORIENTED_EDGE ( 'NONE', *, *, #29406, .F. ) ;
#140617 = DIRECTION ( 'NONE',  ( 1.000000000000000000, 0.000000000000000000, 0.000000000000000000 ) ) ;
#140618 = DIRECTION ( 'NONE',  ( -1.000000000000000000, -0.000000000000000000, -0.000000000000000000 ) ) ;
#140619 = ADVANCED_FACE ( 'NONE', ( #135560 ), #69604, .F. ) ;
#140620 = PLANE ( 'NONE',  #113353 ) ;
#140621 = ORIENTED_EDGE ( 'NONE', *, *, #73593, .F. ) ;
#140622 = VECTOR ( 'NONE', #69302, 999.9999999999998863 ) ;
#140623 = CARTESIAN_POINT ( 'NONE',  ( 8.811592354503320124, -2.500000000000000444, 3.061616997868384620E-16 ) ) ;
#140624 = ORIENTED_EDGE ( 'NONE', *, *, #88206, .T. ) ;
#140625 = CARTESIAN_POINT ( 'NONE',  ( -11.51078643762690490, -27.52281430457047406, 5.000000000000000000 ) ) ;
#140626 = CARTESIAN_POINT ( 'NONE',  ( -10.99806943317894437, -22.22500000000000142, 4.500000000000000888 ) ) ;
#140627 = VECTOR ( 'NONE', #116590, 1000.000000000000000 ) ;
#140628 = CARTESIAN_POINT ( 'NONE',  ( 12.75456980810188767, -6.871911579029512218, 3.967499999999996252 ) ) ;
#140629 = VERTEX_POINT ( 'NONE', #13732 ) ;
#140630 = CARTESIAN_POINT ( 'NONE',  ( 89.45376352523146579, -6.109999999999999432, -3.741295971395163529E-16 ) ) ;
#140631 = LINE ( 'NONE', #3841, #66815 ) ;
#140632 = DIRECTION ( 'NONE',  ( 1.000000000000000000, 0.000000000000000000, 0.000000000000000000 ) ) ;
#140633 = CARTESIAN_POINT ( 'NONE',  ( 10.32500000000000107, 8.432637487761466488, -4.375000000000001776 ) ) ;
#140634 = ORIENTED_EDGE ( 'NONE', *, *, #43812, .F. ) ;
#140635 = ORIENTED_EDGE ( 'NONE', *, *, #18951, .T. ) ;
#140636 = CARTESIAN_POINT ( 'NONE',  ( 0.000000000000000000, 0.000000000000000000, 5.000000000000000000 ) ) ;
#140637 = ORIENTED_EDGE ( 'NONE', *, *, #15161, .T. ) ;
#140638 = VECTOR ( 'NONE', #43935, 1000.000000000000000 ) ;
#140639 = CARTESIAN_POINT ( 'NONE',  ( 33.71230993966005229, -21.73547319004781286, 4.999917730833663754 ) ) ;
#140640 = CARTESIAN_POINT ( 'NONE',  ( 53.99451991528749062, 28.92564299267975869, 4.000000000000000000 ) ) ;
#140641 = LINE ( 'NONE', #85539, #14526 ) ;
#140642 = LINE ( 'NONE', #129056, #873 ) ;
#140643 = ORIENTED_EDGE ( 'NONE', *, *, #128680, .T. ) ;
#140644 = CARTESIAN_POINT ( 'NONE',  ( 9.459838389497344124, 18.75929247661553489, 8.305906642995505962 ) ) ;
#140645 = EDGE_CURVE ( 'NONE', #65778, #72974, #136245, .T. ) ;
#140646 = DIRECTION ( 'NONE',  ( 0.7071067811865486830, -0.7071067811865464625, -0.000000000000000000 ) ) ;
#140647 = CARTESIAN_POINT ( 'NONE',  ( 18.18398860626898994, 28.73617430169800002, 5.000000000000000000 ) ) ;
#140648 = ORIENTED_EDGE ( 'NONE', *, *, #133188, .T. ) ;
#140649 = DIRECTION ( 'NONE',  ( 0.7071067811865487940, -0.7071067811865463515, 0.000000000000000000 ) ) ;
#140650 = CARTESIAN_POINT ( 'NONE',  ( 9.279999999999999361, -2.055000000000000160, 2.789133085058098087E-16 ) ) ;
#140651 = ORIENTED_EDGE ( 'NONE', *, *, #78441, .F. ) ;
#140652 = ADVANCED_FACE ( 'NONE', ( #58021 ), #68886, .T. ) ;
#140654 = EDGE_LOOP ( 'NONE', ( #10714, #19088, #104323, #90734 ) ) ;
#140653 = CARTESIAN_POINT ( 'NONE',  ( -34.92500000000001137, -2.993876922608041724, 4.000000000000000000 ) ) ;
#140655 = EDGE_LOOP ( 'NONE', ( #140611, #9048, #112677, #57406, #43682, #64207 ) ) ;
#140656 = EDGE_CURVE ( 'NONE', #54563, #116840, #25340, .T. ) ;
#140657 = DIRECTION ( 'NONE',  ( -1.000000000000000000, -0.000000000000000000, -0.000000000000000000 ) ) ;
#140658 = DIRECTION ( 'NONE',  ( 1.000000000000000000, 0.000000000000000000, 0.000000000000000000 ) ) ;
#140659 = VERTEX_POINT ( 'NONE', #34106 ) ;
#140660 = DIRECTION ( 'NONE',  ( -0.000000000000000000, -1.000000000000000000, -0.000000000000000000 ) ) ;
#140661 = CARTESIAN_POINT ( 'NONE',  ( 12.69999999999999574, -59.76999999999998892, 24.34531699603382293 ) ) ;
#140662 = EDGE_CURVE ( 'NONE', #47408, #87797, #125180, .T. ) ;
#140663 = PRESENTATION_STYLE_ASSIGNMENT (( #44246 ) ) ;
#140664 = VECTOR ( 'NONE', #80890, 1000.000000000000000 ) ;
#140665 = EDGE_CURVE ( 'NONE', #100474, #31073, #118024, .T. ) ;
#140666 = FACE_OUTER_BOUND ( 'NONE', #143002, .T. ) ;
#140667 = CARTESIAN_POINT ( 'NONE',  ( 0.1600000000000021405, -7.631040150288877832, 2.276131627664947921 ) ) ;
#140668 = DIRECTION ( 'NONE',  ( 0.6830127018922181881, 0.6830127018922202975, -0.2588190451025214056 ) ) ;
#140669 = DIRECTION ( 'NONE',  ( -0.3543493200069163240, -0.000000000000000000, -0.9351131265310288487 ) ) ;
#140670 = DIRECTION ( 'NONE',  ( 0.7071067811865487940, 0.7071067811865463515, 0.000000000000000000 ) ) ;
#140671 = DIRECTION ( 'NONE',  ( 0.7071067811865487940, 0.7071067811865463515, 0.000000000000000000 ) ) ;
#140672 = CARTESIAN_POINT ( 'NONE',  ( -2.816011393730999401, 28.73617430169785436, 5.000000000000000000 ) ) ;
#140673 = CARTESIAN_POINT ( 'NONE',  ( 8.700255128608413102, -27.71228299555199825, 4.000000000000000000 ) ) ;
#140674 = CARTESIAN_POINT ( 'NONE',  ( -25.49999999999982592, -14.56887692260765377, 4.000000000000000000 ) ) ;
#140675 = DIRECTION ( 'NONE',  ( -0.7071067811865487940, 0.7071067811865463515, -0.000000000000000000 ) ) ;
#140676 = ORIENTED_EDGE ( 'NONE', *, *, #115020, .F. ) ;
#140677 = EDGE_CURVE ( 'NONE', #121970, #21922, #72473, .T. ) ;
#140678 = ORIENTED_EDGE ( 'NONE', *, *, #58177, .F. ) ;
#140679 = ORIENTED_EDGE ( 'NONE', *, *, #122335, .T. ) ;
#140680 = CARTESIAN_POINT ( 'NONE',  ( 111.8333333333333428, -6.884901960086287964, 3.974999999999998312 ) ) ;
#140681 = AXIS2_PLACEMENT_3D ( 'NONE', #39454, #72829, #73501 ) ;
#140682 = EDGE_LOOP ( 'NONE', ( #54896, #52506, #141037, #63359 ) ) ;
#140683 = ORIENTED_EDGE ( 'NONE', *, *, #134660, .F. ) ;
#140684 = ORIENTED_EDGE ( 'NONE', *, *, #103262, .T. ) ;
#140685 = DIRECTION ( 'NONE',  ( -1.000000000000000000, -1.224606353822377258E-16, -0.000000000000000000 ) ) ;
#140686 = DIRECTION ( 'NONE',  ( 0.000000000000000000, 1.000000000000000000, 0.000000000000000000 ) ) ;
#140687 = ORIENTED_EDGE ( 'NONE', *, *, #87283, .F. ) ;
#140688 = AXIS2_PLACEMENT_3D ( 'NONE', #1704, #99615, #111957 ) ;
#140689 = DIRECTION ( 'NONE',  ( 1.734723475976806848E-16, -1.000000000000000000, 0.000000000000000000 ) ) ;
#140690 = CARTESIAN_POINT ( 'NONE',  ( 37.03163515922168614, 2.259292476615694323, 13.77329220150646094 ) ) ;
#140691 = CARTESIAN_POINT ( 'NONE',  ( 10.82816939922345156, -20.24070752338408141, 4.000000000000000000 ) ) ;
#140692 = CARTESIAN_POINT ( 'NONE',  ( 20.67183060077632462, -21.74070752338406365, 4.000000000000000000 ) ) ;
#140693 = CARTESIAN_POINT ( 'NONE',  ( 107.3337635252314470, 6.110000000000001208, 1.122388791418549305E-15 ) ) ;
#140694 = ORIENTED_EDGE ( 'NONE', *, *, #15290, .T. ) ;
#140695 = CARTESIAN_POINT ( 'NONE',  ( -28.49999999999979750, 6.052185695429105117, 5.000000000000000000 ) ) ;
#140696 = FACE_OUTER_BOUND ( 'NONE', #80040, .T. ) ;
#140698 = CARTESIAN_POINT ( 'NONE',  ( 22.53999999999999915, 2.055000000000001492, 2.516649172247811554E-16 ) ) ;
#140697 = AXIS2_PLACEMENT_3D ( 'NONE', #68779, #24525, #69490 ) ;
#140699 = DIRECTION ( 'NONE',  ( -0.7071067811865487940, 0.7071067811865463515, 0.000000000000000000 ) ) ;
#140700 = FILL_AREA_STYLE ('',( #40703 ) ) ;
#140701 = VECTOR ( 'NONE', #105972, 1000.000000000000227 ) ;
#140702 = CARTESIAN_POINT ( 'NONE',  ( 27.49586038379622721, -3.974999999999998312, -6.884901960086286188 ) ) ;
#140703 = PLANE ( 'NONE',  #19020 ) ;
#140704 = EDGE_CURVE ( 'NONE', #40296, #68778, #39086, .T. ) ;
#140705 = ORIENTED_EDGE ( 'NONE', *, *, #6457, .T. ) ;
#140706 = EDGE_LOOP ( 'NONE', ( #51386, #121523, #7798, #95512 ) ) ;
#140707 = EDGE_CURVE ( 'NONE', #41256, #103418, #117327, .T. ) ;
#140708 = CARTESIAN_POINT ( 'NONE',  ( 24.91666666666665719, -6.884901960086287076, -3.975000000000000977 ) ) ;
#140709 = VERTEX_POINT ( 'NONE', #29611 ) ;
#140710 = FACE_OUTER_BOUND ( 'NONE', #38367, .T. ) ;
#140711 = EDGE_CURVE ( 'NONE', #69227, #111174, #23743, .T. ) ;
#140712 = DIRECTION ( 'NONE',  ( 0.3543493200069162685, -0.000000000000000000, -0.9351131265310288487 ) ) ;
#140713 = DIRECTION ( 'NONE',  ( -0.7071067811865487940, -0.7071067811865463515, -0.000000000000000000 ) ) ;
#140715 = ADVANCED_FACE ( 'NONE', ( #49976 ), #127517, .F. ) ;
#140714 = LINE ( 'NONE', #10200, #49231 ) ;
#140716 = EDGE_CURVE ( 'NONE', #8328, #95030, #46479, .T. ) ;
#140717 = DIRECTION ( 'NONE',  ( 0.000000000000000000, 1.286409696682840916E-16, -1.000000000000000000 ) ) ;
#140718 = CARTESIAN_POINT ( 'NONE',  ( 120.6620968585647802, -5.291415217122919401, 3.054999999999997939 ) ) ;
#140719 = VERTEX_POINT ( 'NONE', #50670 ) ;
#140720 = LINE ( 'NONE', #94365, #103544 ) ;
#140721 = VERTEX_POINT ( 'NONE', #17322 ) ;
#140722 = CARTESIAN_POINT ( 'NONE',  ( 71.53752705046289861, -9.735942053221456900E-16, 7.949999999999998401 ) ) ;
#140723 = DIRECTION ( 'NONE',  ( 0.7071067811865487940, 0.7071067811865463515, 0.000000000000000000 ) ) ;
#140724 = DIRECTION ( 'NONE',  ( 0.7071067811865487940, 0.7071067811865463515, 0.000000000000000000 ) ) ;
#140725 = EDGE_LOOP ( 'NONE', ( #22350, #137619, #72938, #76855 ) ) ;
#140727 = EDGE_CURVE ( 'NONE', #47662, #17057, #105732, .T. ) ;
#140726 = CARTESIAN_POINT ( 'NONE',  ( 42.72959685856476142, -6.110000000000000320, -1.637169565754161393 ) ) ;
#140728 = VERTEX_POINT ( 'NONE', #138397 ) ;
#140729 = DIRECTION ( 'NONE',  ( -0.7071067811865487940, 0.7071067811865463515, -0.000000000000000000 ) ) ;
#140730 = EDGE_CURVE ( 'NONE', #14203, #138480, #115173, .T. ) ;
#140731 = PLANE ( 'NONE',  #20677 ) ;
#140732 = PLANE ( 'NONE',  #52431 ) ;
#140733 = CIRCLE ( 'NONE', #136086, 28.00000000000002487 ) ;
#140734 = DIRECTION ( 'NONE',  ( -0.7071067811865487940, 0.7071067811865463515, -0.000000000000000000 ) ) ;
#140735 = EDGE_CURVE ( 'NONE', #44234, #132762, #93467, .T. ) ;
#140736 = CARTESIAN_POINT ( 'NONE',  ( 42.34959685856478018, 6.109999999999996767, 1.637169565754163836 ) ) ;
#140737 = EDGE_LOOP ( 'NONE', ( #109059, #12266, #103626, #40572 ) ) ;
#140738 = FACE_OUTER_BOUND ( 'NONE', #102248, .T. ) ;
#140739 = VERTEX_POINT ( 'NONE', #48534 ) ;
#140740 = ORIENTED_EDGE ( 'NONE', *, *, #97366, .F. ) ;
#140741 = ADVANCED_FACE ( 'NONE', ( #92732 ), #139124, .F. ) ;
#140742 = VERTEX_POINT ( 'NONE', #128247 ) ;
#140743 = PRODUCT ( '1.6 Slide Key', '1.6 Slide Key', '', ( #49691 ) ) ;
#140744 = CARTESIAN_POINT ( 'NONE',  ( -12.70000000000000462, -28.33999999999998565, 13.17925390838734323 ) ) ;
#140745 = VERTEX_POINT ( 'NONE', #115893 ) ;
#140746 = LINE ( 'NONE', #71249, #136341 ) ;
#140747 = EDGE_CURVE ( 'NONE', #35520, #77121, #136973, .T. ) ;
#140748 = CARTESIAN_POINT ( 'NONE',  ( 0.000000000000000000, -21.72500000000000142, 4.500000000000000888 ) ) ;
#140749 = CARTESIAN_POINT ( 'NONE',  ( -34.36246187583878253, 22.22500000000000142, 4.000000000000000000 ) ) ;
#140750 = FACE_BOUND ( 'NONE', #109470, .T. ) ;
#140751 = ORIENTED_EDGE ( 'NONE', *, *, #30202, .T. ) ;
#140752 = DIRECTION ( 'NONE',  ( -0.7071067811865487940, 0.7071067811865463515, -0.000000000000000000 ) ) ;
#140753 = CARTESIAN_POINT ( 'NONE',  ( -4.499999999999962697, -5.947814304570770538, 5.000000000000000000 ) ) ;
#140754 = DIRECTION ( 'NONE',  ( -0.7071067811865486830, -0.7071067811865464625, 0.000000000000000000 ) ) ;
#140755 = ORIENTED_EDGE ( 'NONE', *, *, #102135, .T. ) ;
#140756 = DIRECTION ( 'NONE',  ( -0.7071067811865486830, -0.7071067811865464625, 0.000000000000000000 ) ) ;
#140757 = ORIENTED_EDGE ( 'NONE', *, *, #52666, .F. ) ;
#140758 = VERTEX_POINT ( 'NONE', #104310 ) ;
#140759 = DIRECTION ( 'NONE',  ( -0.000000000000000000, 0.3543493200069153248, 0.9351131265310292928 ) ) ;
#140760 = ORIENTED_EDGE ( 'NONE', *, *, #43363, .F. ) ;
#140761 = EDGE_CURVE ( 'NONE', #46517, #73841, #64979, .T. ) ;
#140762 = CARTESIAN_POINT ( 'NONE',  ( 60.87043019189810877, -3.055000000000001492, 5.291415217122917625 ) ) ;
#140763 = EDGE_LOOP ( 'NONE', ( #79316, #24751, #76748, #30368, #53718 ) ) ;
#140764 = VECTOR ( 'NONE', #40782, 1000.000000000000114 ) ;
#140765 = DIRECTION ( 'NONE',  ( -0.7071067811865486830, 0.7071067811865464625, 0.000000000000000000 ) ) ;
#140766 = DIRECTION ( 'NONE',  ( 0.5735764363510444941, 0.8191520442889929088, 0.000000000000000000 ) ) ;
#140767 = ORIENTED_EDGE ( 'NONE', *, *, #136100, .T. ) ;
#140768 = PLANE ( 'NONE',  #134872 ) ;
#140769 = EDGE_CURVE ( 'NONE', #109323, #84890, #83497, .T. ) ;
#140770 = DIRECTION ( 'NONE',  ( 0.7071067811865487940, -0.7071067811865463515, 0.000000000000000000 ) ) ;
#140771 = LINE ( 'NONE', #119720, #73629 ) ;
#140772 = CARTESIAN_POINT ( 'NONE',  ( 13.49999999999991473, -1.592773361805351673, -6.492772025301255745 ) ) ;
#140773 = CARTESIAN_POINT ( 'NONE',  ( 6.183988606268994381, 28.73617430169791476, 5.000000000000000000 ) ) ;
#140774 = DIRECTION ( 'NONE',  ( -0.7071067811865486830, -0.7071067811865464625, 0.000000000000000000 ) ) ;
#140775 = ORIENTED_EDGE ( 'NONE', *, *, #22081, .F. ) ;
#140776 = EDGE_LOOP ( 'NONE', ( #54247, #55098, #7760, #101586 ) ) ;
#140777 = DIRECTION ( 'NONE',  ( -0.3543493200069162685, -0.000000000000000000, -0.9351131265310288487 ) ) ;
#140779 = PLANE ( 'NONE',  #49009 ) ;
#140778 = VECTOR ( 'NONE', #142788, 1000.000000000000000 ) ;
#140780 = ORIENTED_EDGE ( 'NONE', *, *, #6260, .F. ) ;
#140781 = ORIENTED_EDGE ( 'NONE', *, *, #119618, .F. ) ;
#140783 = ORIENTED_EDGE ( 'NONE', *, *, #133305, .T. ) ;
#140782 = CIRCLE ( 'NONE', #115297, 9.500000000000001776 ) ;
#140784 = DIRECTION ( 'NONE',  ( 1.000000000000000000, 0.000000000000000000, 0.000000000000000000 ) ) ;
#140785 = LINE ( 'NONE', #118273, #70706 ) ;
#140786 = FACE_OUTER_BOUND ( 'NONE', #36900, .T. ) ;
#140787 = VERTEX_POINT ( 'NONE', #16600 ) ;
#140788 = DIRECTION ( 'NONE',  ( 0.3543493200069162685, -0.000000000000000000, -0.9351131265310288487 ) ) ;
#140789 = VECTOR ( 'NONE', #12581, 1000.000000000000000 ) ;
#140790 = AXIS2_PLACEMENT_3D ( 'NONE', #622, #22359, #98523 ) ;
#140791 =( BOUNDED_CURVE ( )  B_SPLINE_CURVE ( 3, ( #79572, #44797, #11356, #91132 ),
 .UNSPECIFIED., .F., .T. ) 
 B_SPLINE_CURVE_WITH_KNOTS ( ( 4, 4 ),
 ( 4.350170835173026163, 4.500739107949268458 ),
 .UNSPECIFIED. ) 
 CURVE ( )  GEOMETRIC_REPRESENTATION_ITEM ( )  RATIONAL_B_SPLINE_CURVE ( ( 1.000000000000000000, 0.9981116584018941973, 0.9981116584018941973, 1.000000000000000000 ) ) 
 REPRESENTATION_ITEM ( '' )  );
#140792 = CARTESIAN_POINT ( 'NONE',  ( 5.999999999999977796, -16.44781430457066662, 5.000000000000000000 ) ) ;
#140793 = CARTESIAN_POINT ( 'NONE',  ( 21.79623647476855552, 7.934999999999990727, -1.457635852685135314E-15 ) ) ;
#140794 = DIRECTION ( 'NONE',  ( -1.000000000000000000, -0.000000000000000000, -0.000000000000000000 ) ) ;
#140795 = VERTEX_POINT ( 'NONE', #105047 ) ;
#140796 = CARTESIAN_POINT ( 'NONE',  ( 115.7037635252314516, 6.109999999999999432, 1.122388791418549108E-15 ) ) ;
#140798 = EDGE_CURVE ( 'NONE', #22078, #139771, #5710, .T. ) ;
#140797 = LINE ( 'NONE', #106016, #23433 ) ;
#140799 = DIRECTION ( 'NONE',  ( -0.000000000000000000, 0.000000000000000000, 1.000000000000000000 ) ) ;
#140801 = ORIENTED_EDGE ( 'NONE', *, *, #24136, .T. ) ;
#140800 = CARTESIAN_POINT ( 'NONE',  ( 7.251592354503322291, 9.902892378096218942E-16, 0.000000000000000000 ) ) ;
#140802 = DIRECTION ( 'NONE',  ( 0.6830127018922180770, -0.6830127018922204085, -0.2588190451025213501 ) ) ;
#140803 = VERTEX_POINT ( 'NONE', #33249 ) ;
#140804 = FACE_OUTER_BOUND ( 'NONE', #6162, .T. ) ;
#140805 = DIRECTION ( 'NONE',  ( 0.000000000000000000, 0.000000000000000000, 1.000000000000000000 ) ) ;
#140806 = PLANE ( 'NONE',  #88893 ) ;
#140807 = ORIENTED_EDGE ( 'NONE', *, *, #54619, .F. ) ;
#140808 = ADVANCED_FACE ( 'NONE', ( #121618 ), #44092, .F. ) ;
#140809 = LINE ( 'NONE', #23878, #47368 ) ;
#140810 = DIRECTION ( 'NONE',  ( -1.000000000000000000, -0.000000000000000000, -0.000000000000000000 ) ) ;
#140811 = CARTESIAN_POINT ( 'NONE',  ( 20.99999999999985079, -4.068876922607768343, 4.000000000000000000 ) ) ;
#140812 = EDGE_LOOP ( 'NONE', ( #6932, #87555, #68142, #111484 ) ) ;
#140813 = VECTOR ( 'NONE', #79771, 1000.000000000000227 ) ;
#140814 = CARTESIAN_POINT ( 'NONE',  ( 26.20710678118635784, -5.240707523384230626, 5.000000000000000000 ) ) ;
#140816 = AXIS2_PLACEMENT_3D ( 'NONE', #32268, #88073, #42455 ) ;
#140815 = LINE ( 'NONE', #53091, #28409 ) ;
#140817 = DIRECTION ( 'NONE',  ( 0.000000000000000000, 0.000000000000000000, -1.000000000000000000 ) ) ;
#140818 = LINE ( 'NONE', #43670, #120217 ) ;
#140819 = ADVANCED_FACE ( 'NONE', ( #110030 ), #76736, .F. ) ;
#140820 = ORIENTED_EDGE ( 'NONE', *, *, #124514, .F. ) ;
#140822 = ORIENTED_EDGE ( 'NONE', *, *, #100281, .F. ) ;
#140821 = EDGE_CURVE ( 'NONE', #88773, #68120, #7052, .T. ) ;
#140823 = DIRECTION ( 'NONE',  ( -0.7071067811865486830, -0.7071067811865464625, -0.000000000000000000 ) ) ;
#140824 = LINE ( 'NONE', #21204, #117709 ) ;
#140825 = EDGE_CURVE ( 'NONE', #35675, #87648, #107180, .T. ) ;
#140826 = CARTESIAN_POINT ( 'NONE',  ( 12.08290314143522082, 3.967499999999992699, -6.871911579029513994 ) ) ;
#140827 =( NAMED_UNIT ( * ) PLANE_ANGLE_UNIT ( ) SI_UNIT ( $, .RADIAN. ) );
#140828 = CARTESIAN_POINT ( 'NONE',  ( -16.49999999999988276, -16.91253812416058722, 4.000000000000000000 ) ) ;
#140829 = CARTESIAN_POINT ( 'NONE',  ( -45.48921356237309510, -27.52281430457087197, 5.000000000000000000 ) ) ;
#140830 = ORIENTED_EDGE ( 'NONE', *, *, #95824, .F. ) ;
#140831 = EDGE_CURVE ( 'NONE', #43903, #69745, #65873, .T. ) ;
#140832 = DIRECTION ( 'NONE',  ( -0.7071067811865486830, 0.7071067811865464625, 0.000000000000000000 ) ) ;
#140833 = CARTESIAN_POINT ( 'NONE',  ( 6.024972949537104938, -4.461849672132299993, -4.461849672132299105 ) ) ;
#140834 = VECTOR ( 'NONE', #110108, 1000.000000000000000 ) ;
#140835 = DIRECTION ( 'NONE',  ( -1.000000000000000000, -1.224606353822377258E-16, -0.000000000000000000 ) ) ;
#140836 = CARTESIAN_POINT ( 'NONE',  ( 38.41209685856478018, 5.291415217122922066, -3.054999999999995275 ) ) ;
#140837 = FACE_OUTER_BOUND ( 'NONE', #109765, .T. ) ;
#140838 = AXIS2_PLACEMENT_3D ( 'NONE', #97506, #100395, #108353 ) ;
#140839 = EDGE_CURVE ( 'NONE', #91297, #83273, #7857, .T. ) ;
#140840 = EDGE_LOOP ( 'NONE', ( #27033, #2333, #66590, #109286 ) ) ;
#140841 = SURFACE_STYLE_FILL_AREA ( #96599 ) ;
#140842 = ORIENTED_EDGE ( 'NONE', *, *, #17501, .T. ) ;
#140843 = VERTEX_POINT ( 'NONE', #54972 ) ;
#140844 = DIRECTION ( 'NONE',  ( -0.000000000000000000, 0.000000000000000000, 1.000000000000000000 ) ) ;
#140845 = CARTESIAN_POINT ( 'NONE',  ( 30.48921356237309510, -27.52281430457076894, 5.000000000000000000 ) ) ;
#140846 = ADVANCED_FACE ( 'NONE', ( #120167 ), #20156, .F. ) ;
#140847 = VERTEX_POINT ( 'NONE', #99139 ) ;
#140848 = CARTESIAN_POINT ( 'NONE',  ( 18.08314806772920136, 21.75929247661550292, 7.311836541448091253 ) ) ;
#140849 = LINE ( 'NONE', #75628, #139159 ) ;
#140850 = CARTESIAN_POINT ( 'NONE',  ( 23.29289321881329755, 8.259292476615637923, 5.000000000000000000 ) ) ;
#140851 = CARTESIAN_POINT ( 'NONE',  ( -24.97566027651206610, 3.896288752498341168, 4.156157854036512944 ) ) ;
#140852 = CARTESIAN_POINT ( 'NONE',  ( 131.8806778009765708, -49.14999999999999147, 40.92499999999999005 ) ) ;
#140853 = ORIENTED_EDGE ( 'NONE', *, *, #87896, .T. ) ;
#140854 = CARTESIAN_POINT ( 'NONE',  ( 1.802887254483181323, 1.153283441868768300, -6.189908599751838381 ) ) ;
#140855 = CARTESIAN_POINT ( 'NONE',  ( 34.03163515922170035, 2.259292476615690770, 13.77329220150645384 ) ) ;
#140856 = EDGE_CURVE ( 'NONE', #140742, #107457, #52096, .T. ) ;
#140857 = CARTESIAN_POINT ( 'NONE',  ( 39.48921356237310221, -27.52281430457082934, 5.000000000000000000 ) ) ;
#140858 = LINE ( 'NONE', #55315, #31631 ) ;
#140859 = DIRECTION ( 'NONE',  ( 1.301042606982605074E-16, -1.000000000000000000, 0.000000000000000000 ) ) ;
#140860 = PLANE ( 'NONE',  #130118 ) ;
#140861 = DIRECTION ( 'NONE',  ( 0.7071067811865487940, 0.7071067811865463515, -0.000000000000000000 ) ) ;
#140862 = CARTESIAN_POINT ( 'NONE',  ( 59.87086038379622721, 6.884901960086289741, -3.974999999999993427 ) ) ;
#140863 = CARTESIAN_POINT ( 'NONE',  ( -26.99999999999980815, -6.033600742197676503, 5.000000000000000000 ) ) ;
#140864 = ORIENTED_EDGE ( 'NONE', *, *, #98467, .F. ) ;
#140865 = ORIENTED_EDGE ( 'NONE', *, *, #73686, .F. ) ;
#140866 = CARTESIAN_POINT ( 'NONE',  ( 55.39583333333331439, -2.130196079827427091, 7.949999999999999289 ) ) ;
#140867 = DIRECTION ( 'NONE',  ( 0.7071067811865487940, -0.7071067811865463515, 0.000000000000000000 ) ) ;
#140868 = LINE ( 'NONE', #118408, #106344 ) ;
#140869 = EDGE_CURVE ( 'NONE', #87975, #41180, #140519, .T. ) ;
#140870 = FACE_OUTER_BOUND ( 'NONE', #10797, .T. ) ;
#140871 = ORIENTED_EDGE ( 'NONE', *, *, #32491, .F. ) ;
#140873 = EDGE_CURVE ( 'NONE', #90362, #5701, #85417, .T. ) ;
#140872 = FACE_OUTER_BOUND ( 'NONE', #124886, .T. ) ;
#140874 = EDGE_CURVE ( 'NONE', #53423, #139751, #33918, .T. ) ;
#140875 = CARTESIAN_POINT ( 'NONE',  ( 45.35459685856476852, -1.637169565754161615, 6.110000000000000320 ) ) ;
#140876 = ORIENTED_EDGE ( 'NONE', *, *, #41255, .T. ) ;
#140877 = DIRECTION ( 'NONE',  ( 0.7071067811865487940, -0.7071067811865463515, 0.000000000000000000 ) ) ;
#140878 = ORIENTED_EDGE ( 'NONE', *, *, #93391, .F. ) ;
#140879 = ORIENTED_EDGE ( 'NONE', *, *, #121765, .T. ) ;
#140880 = DIRECTION ( 'NONE',  ( 0.000000000000000000, -1.000000000000000000, 0.000000000000000000 ) ) ;
#140881 = VECTOR ( 'NONE', #23058, 1000.000000000000000 ) ;
#140882 = VECTOR ( 'NONE', #11343, 1000.000000000000000 ) ;
#140883 = VECTOR ( 'NONE', #53018, 1000.000000000000000 ) ;
#140884 = EDGE_CURVE ( 'NONE', #33598, #103751, #53534, .T. ) ;
#140885 = CARTESIAN_POINT ( 'NONE',  ( 82.03752705046288440, -9.735942053221456900E-16, 7.949999999999998401 ) ) ;
#140886 = DIRECTION ( 'NONE',  ( 0.3543493200069162685, -0.000000000000000000, -0.9351131265310288487 ) ) ;
#140887 = VECTOR ( 'NONE', #65383, 1000.000000000000227 ) ;
#140888 = CARTESIAN_POINT ( 'NONE',  ( -2.292893218813436995, 20.25929247661551358, 5.000000000000000000 ) ) ;
#140889 = VERTEX_POINT ( 'NONE', #86879 ) ;
#140890 = EDGE_CURVE ( 'NONE', #66246, #92499, #109334, .T. ) ;
#140892 = AXIS2_PLACEMENT_3D ( 'NONE', #57076, #100560, #45489 ) ;
#140891 = CARTESIAN_POINT ( 'NONE',  ( -5.700255128608413102, -27.71228299555201957, 4.000000000000000000 ) ) ;
#140894 = ORIENTED_EDGE ( 'NONE', *, *, #6575, .T. ) ;
#140893 = CARTESIAN_POINT ( 'NONE',  ( -31.49999999999977973, -12.08601207473292405, -10.46905243149087106 ) ) ;
#140895 = CARTESIAN_POINT ( 'NONE',  ( 80.93793019189809002, -6.110000000000001208, 1.637169565754158951 ) ) ;
#140896 = CARTESIAN_POINT ( 'NONE',  ( 15.45833333333333393, -3.047499999999997211, -5.278424836066143655 ) ) ;
#140897 = CARTESIAN_POINT ( 'NONE',  ( 20.99451991528748707, 28.92564299267952777, 4.000000000000000000 ) ) ;
#140898 = CARTESIAN_POINT ( 'NONE',  ( -36.18398860626899705, 28.73617430169812437, 5.000000000000000000 ) ) ;
#140900 = CARTESIAN_POINT ( 'NONE',  ( -32.99451991528749062, 28.92564299267960948, 4.000000000000000000 ) ) ;
#140899 = VECTOR ( 'NONE', #71824, 1000.000000000000000 ) ;
#140901 = CARTESIAN_POINT ( 'NONE',  ( 36.18398860626899705, 28.73617430169812437, 5.000000000000000000 ) ) ;
#140902 = CIRCLE ( 'NONE', #13603, 2.055000000000001048 ) ;
#140903 = VERTEX_POINT ( 'NONE', #98454 ) ;
#140904 = EDGE_CURVE ( 'NONE', #141462, #132753, #142680, .T. ) ;
#140905 = FACE_OUTER_BOUND ( 'NONE', #93828, .T. ) ;
#140906 = CARTESIAN_POINT ( 'NONE',  ( 66.12043019189812298, 3.055000000000001936, -5.291415217122916737 ) ) ;
#140907 = CARTESIAN_POINT ( 'NONE',  ( 15.48921356237309510, -27.52281430457066236, 5.000000000000000000 ) ) ;
#140908 = CARTESIAN_POINT ( 'NONE',  ( -17.51078643762690845, -27.52281430457043143, 5.000000000000000000 ) ) ;
#140909 = SURFACE_STYLE_USAGE ( .BOTH. , #107573 ) ;
#140910 = ORIENTED_EDGE ( 'NONE', *, *, #129911, .F. ) ;
#140911 = ORIENTED_EDGE ( 'NONE', *, *, #141858, .T. ) ;
#140912 = AXIS2_PLACEMENT_3D ( 'NONE', #127100, #16931, #43676 ) ;
#140913 = PLANE ( 'NONE',  #56133 ) ;
#140915 = EDGE_CURVE ( 'NONE', #51846, #72705, #47691, .T. ) ;
#140914 = DIRECTION ( 'NONE',  ( -1.000000000000000000, -1.224606353822377258E-16, -0.000000000000000000 ) ) ;
#140916 = ORIENTED_EDGE ( 'NONE', *, *, #22469, .F. ) ;
#140917 = EDGE_LOOP ( 'NONE', ( #95964, #20365, #114911, #142020 ) ) ;
#140918 = VECTOR ( 'NONE', #33057, 1000.000000000000227 ) ;
#140919 = LINE ( 'NONE', #65561, #134744 ) ;
#140920 = ORIENTED_EDGE ( 'NONE', *, *, #8361, .T. ) ;
#140921 = LINE ( 'NONE', #138263, #53877 ) ;
#140922 = CARTESIAN_POINT ( 'NONE',  ( -0.4892135623730947680, -27.52281430457055578, 5.000000000000000000 ) ) ;
#140923 = VECTOR ( 'NONE', #126937, 1000.000000000000227 ) ;
#140924 = AXIS2_PLACEMENT_3D ( 'NONE', #125588, #61764, #114672 ) ;
#140925 = VECTOR ( 'NONE', #23330, 1000.000000000000000 ) ;
#140927 = CIRCLE ( 'NONE', #78450, 5.968999999999998529 ) ;
#140926 = CARTESIAN_POINT ( 'NONE',  ( -11.67183060077638856, -18.74070752338409207, 4.000000000000000000 ) ) ;
#140928 = FACE_BOUND ( 'NONE', #23757, .T. ) ;
#140929 = CYLINDRICAL_SURFACE ( 'NONE', #126592, 0.5000000000000004441 ) ;
#140930 = DIRECTION ( 'NONE',  ( 0.7071067811865486830, -0.7071067811865464625, -0.000000000000000000 ) ) ;
#140931 = CARTESIAN_POINT ( 'NONE',  ( 17.81601139373099940, 28.73617430169775133, 5.000000000000000000 ) ) ;
#140933 = ORIENTED_EDGE ( 'NONE', *, *, #64358, .T. ) ;
#140932 = CARTESIAN_POINT ( 'NONE',  ( 0.4892135623730947680, -27.52281430457055578, 5.000000000000000000 ) ) ;
#140934 = STYLED_ITEM ( 'NONE', ( #76151 ), #49850 ) ;
#140935 = VECTOR ( 'NONE', #15598, 999.9999999999998863 ) ;
#140936 = LINE ( 'NONE', #141677, #81153 ) ;
#140937 = CONTEXT_DEPENDENT_SHAPE_REPRESENTATION ( #131878, #107171 ) ;
#140938 = EDGE_LOOP ( 'NONE', ( #32015, #31402, #35174, #143505 ) ) ;
#140939 = EDGE_CURVE ( 'NONE', #3772, #8318, #18660, .T. ) ;
#140940 = ORIENTED_EDGE ( 'NONE', *, *, #49108, .F. ) ;
#140941 = CARTESIAN_POINT ( 'NONE',  ( 82.16209685856479439, -5.291415217122919401, 3.054999999999997939 ) ) ;
#140942 = ORIENTED_EDGE ( 'NONE', *, *, #60602, .T. ) ;
#140943 = CARTESIAN_POINT ( 'NONE',  ( 23.99999999999983302, -19.06887692260762179, 4.000000000000000000 ) ) ;
#140944 = ORIENTED_EDGE ( 'NONE', *, *, #15382, .T. ) ;
#140945 = DIRECTION ( 'NONE',  ( 0.7071067811865487940, 0.7071067811865463515, -0.000000000000000000 ) ) ;
#140946 = VECTOR ( 'NONE', #85913, 999.9999999999998863 ) ;
#140947 = CARTESIAN_POINT ( 'NONE',  ( -34.92500000000001137, 16.32446447596929318, 2.764066516344052094 ) ) ;
#140948 = CARTESIAN_POINT ( 'NONE',  ( 1.828169399223519953, -5.240707523384232402, 4.000000000000000000 ) ) ;
#140949 = CARTESIAN_POINT ( 'NONE',  ( -35.99451991528749772, 28.92564299267963079, 4.000000000000000000 ) ) ;
#140950 = CARTESIAN_POINT ( 'NONE',  ( -33.18398860626899705, 28.73617430169810305, 5.000000000000000000 ) ) ;
#140951 = CARTESIAN_POINT ( 'NONE',  ( 8.500000000000000000, 9.521314400968980422E-16, 0.000000000000000000 ) ) ;
#140952 = DIRECTION ( 'NONE',  ( -0.6830127018922181881, 0.6830127018922202975, -0.2588190451025214056 ) ) ;
#140953 = DIRECTION ( 'NONE',  ( 0.7071067811865486830, -0.7071067811865464625, -0.000000000000000000 ) ) ;
#140954 = ORIENTED_EDGE ( 'NONE', *, *, #1413, .F. ) ;
#140955 = ORIENTED_EDGE ( 'NONE', *, *, #37812, .T. ) ;
#140956 = LINE ( 'NONE', #51125, #72758 ) ;
#140957 = PLANE ( 'NONE',  #129916 ) ;
#140958 = ORIENTED_EDGE ( 'NONE', *, *, #110163, .T. ) ;
#140959 = ORIENTED_EDGE ( 'NONE', *, *, #78902, .T. ) ;
#140960 = CARTESIAN_POINT ( 'NONE',  ( 57.29974487139158157, -27.71228299555246011, 4.000000000000000000 ) ) ;
#140961 = EDGE_LOOP ( 'NONE', ( #86930, #75014, #124309, #51276 ) ) ;
#140962 = CARTESIAN_POINT ( 'NONE',  ( 36.16709685856476852, -3.055000000000000160, -5.291415217122921177 ) ) ;
#140963 = VERTEX_POINT ( 'NONE', #11406 ) ;
#140964 = DIRECTION ( 'NONE',  ( -1.000000000000000000, 0.000000000000000000, 0.000000000000000000 ) ) ;
#140965 = CARTESIAN_POINT ( 'NONE',  ( 23.67080628287044064, -3.047499999999997211, -5.278424836066143655 ) ) ;
#140966 = CARTESIAN_POINT ( 'NONE',  ( 6.275962415994857047, 11.42931026327849686, -27.74749330399082226 ) ) ;
#140967 = ORIENTED_EDGE ( 'NONE', *, *, #59820, .T. ) ;
#140968 = DIRECTION ( 'NONE',  ( 0.7071067811865487940, 0.7071067811865463515, 0.000000000000000000 ) ) ;
#140969 = ORIENTED_EDGE ( 'NONE', *, *, #43639, .T. ) ;
#140971 = EDGE_CURVE ( 'NONE', #136929, #103105, #44076, .T. ) ;
#140970 = DIRECTION ( 'NONE',  ( 0.000000000000000000, 0.000000000000000000, 1.000000000000000000 ) ) ;
#140972 = CARTESIAN_POINT ( 'NONE',  ( 0.000000000000000000, -21.72500000000000142, 4.500000000000000888 ) ) ;
#140974 = ORIENTED_EDGE ( 'NONE', *, *, #95781, .F. ) ;
#140973 = CARTESIAN_POINT ( 'NONE',  ( 31.49999999999977973, 6.277155672890302185, -3.510561720659014728 ) ) ;
#140975 = ORIENTED_EDGE ( 'NONE', *, *, #22081, .T. ) ;
#140976 = LINE ( 'NONE', #64880, #139477 ) ;
#140977 = PLANE ( 'NONE',  #26274 ) ;
#140978 = ORIENTED_EDGE ( 'NONE', *, *, #75179, .F. ) ;
#140979 = DIRECTION ( 'NONE',  ( -0.6830127018922181881, 0.6830127018922202975, -0.2588190451025214056 ) ) ;
#140980 = ORIENTED_EDGE ( 'NONE', *, *, #5497, .F. ) ;
#140981 = VERTEX_POINT ( 'NONE', #68026 ) ;
#140982 = ORIENTED_EDGE ( 'NONE', *, *, #90905, .F. ) ;
#140983 = LINE ( 'NONE', #76486, #65770 ) ;
#140984 = VECTOR ( 'NONE', #105455, 1000.000000000000000 ) ;
#140985 = VECTOR ( 'NONE', #133034, 1000.000000000000000 ) ;
#140986 = VECTOR ( 'NONE', #23587, 1000.000000000000000 ) ;
#140987 = LINE ( 'NONE', #75765, #9028 ) ;
#140988 = DIRECTION ( 'NONE',  ( -0.7071067811865486830, -0.7071067811865464625, -0.000000000000000000 ) ) ;
#140989 = DIRECTION ( 'NONE',  ( 0.000000000000000000, 0.000000000000000000, -1.000000000000000000 ) ) ;
#140990 = EDGE_CURVE ( 'NONE', #105277, #110666, #1259, .T. ) ;
#140991 = DIRECTION ( 'NONE',  ( 1.000000000000000000, -0.000000000000000000, 0.000000000000000000 ) ) ;
#140992 = DIRECTION ( 'NONE',  ( -0.7071067811865487940, 0.7071067811865463515, -0.000000000000000000 ) ) ;
#140993 = EDGE_CURVE ( 'NONE', #139777, #74065, #66554, .T. ) ;
#140995 = ORIENTED_EDGE ( 'NONE', *, *, #59686, .T. ) ;
#140994 = ADVANCED_FACE ( 'NONE', ( #23000 ), #99885, .F. ) ;
#140996 = CARTESIAN_POINT ( 'NONE',  ( 67.35416666666664298, -2.130196079827425759, -7.950000000000000178 ) ) ;
#140997 = ORIENTED_EDGE ( 'NONE', *, *, #42424, .F. ) ;
#140998 = AXIS2_PLACEMENT_3D ( 'NONE', #61033, #72620, #137845 ) ;
#140999 = LINE ( 'NONE', #41706, #51756 ) ;
#141000 = ADVANCED_FACE ( 'NONE', ( #2695 ), #78149, .F. ) ;
#141001 = EDGE_CURVE ( 'NONE', #77315, #86117, #111295, .T. ) ;
#141002 = CARTESIAN_POINT ( 'NONE',  ( 31.33290314143522082, -3.967499999999994476, 6.871911579029513106 ) ) ;
#141003 = VERTEX_POINT ( 'NONE', #36758 ) ;
#141004 = DIRECTION ( 'NONE',  ( 0.7071067811865487940, -0.7071067811865463515, 0.000000000000000000 ) ) ;
#141005 = LINE ( 'NONE', #41711, #90711 ) ;
#141006 = VERTEX_POINT ( 'NONE', #552 ) ;
#141007 = ORIENTED_EDGE ( 'NONE', *, *, #62147, .F. ) ;
#141008 = EDGE_CURVE ( 'NONE', #20953, #130029, #91182, .T. ) ;
#141009 = LINE ( 'NONE', #54058, #51130 ) ;
#141010 = LINE ( 'NONE', #75089, #65068 ) ;
#141011 = DIRECTION ( 'NONE',  ( 1.000000000000000000, 0.000000000000000000, 0.000000000000000000 ) ) ;
#141012 = STYLED_ITEM ( 'NONE', ( #17454 ), #47140 ) ;
#141013 = FACE_OUTER_BOUND ( 'NONE', #45169, .T. ) ;
#141014 = DIRECTION ( 'NONE',  ( -1.000000000000000000, -0.000000000000000000, -0.000000000000000000 ) ) ;
#141015 = CARTESIAN_POINT ( 'NONE',  ( 61.30793019189810877, -6.109999999999999432, 1.637169565754158507 ) ) ;
#141016 =( BOUNDED_CURVE ( )  B_SPLINE_CURVE ( 3, ( #106764, #51709, #129970, #85730 ),
 .UNSPECIFIED., .F., .F. ) 
 B_SPLINE_CURVE_WITH_KNOTS ( ( 4, 4 ),
 ( 1.901594255663618060, 1.933014472006549633 ),
 .UNSPECIFIED. ) 
 CURVE ( )  GEOMETRIC_REPRESENTATION_ITEM ( )  RATIONAL_B_SPLINE_CURVE ( ( 1.000000000000000000, 0.9999177325257868620, 0.9999177325257868620, 1.000000000000000000 ) ) 
 REPRESENTATION_ITEM ( '' )  );
#141017 = LINE ( 'NONE', #142476, #99624 ) ;
#141018 = ADVANCED_FACE ( 'NONE', ( #12152 ), #33931, .F. ) ;
#141020 = CARTESIAN_POINT ( 'NONE',  ( 20.99451991528748707, 28.92564299267952777, 4.000000000000000000 ) ) ;
#141019 = VECTOR ( 'NONE', #53144, 999.9999999999998863 ) ;
#141021 = CARTESIAN_POINT ( 'NONE',  ( -18.18398860626898994, 28.73617430169800002, 5.000000000000000000 ) ) ;
#141022 = LINE ( 'NONE', #85211, #37417 ) ;
#141023 = VERTEX_POINT ( 'NONE', #135399 ) ;
#141024 = CARTESIAN_POINT ( 'NONE',  ( -34.82816939922327748, 3.759292476615692102, 4.000000000000000000 ) ) ;
#141025 = ORIENTED_EDGE ( 'NONE', *, *, #7723, .T. ) ;
#141026 = LINE ( 'NONE', #130182, #24658 ) ;
#141027 = DIRECTION ( 'NONE',  ( -0.000000000000000000, 1.000000000000000000, -0.000000000000000000 ) ) ;
#141028 = EDGE_LOOP ( 'NONE', ( #50512, #74819, #14779, #94973 ) ) ;
#141029 = VECTOR ( 'NONE', #101096, 1000.000000000000000 ) ;
#141030 =( GEOMETRIC_REPRESENTATION_CONTEXT ( 3 ) GLOBAL_UNCERTAINTY_ASSIGNED_CONTEXT ( ( #114130 ) ) GLOBAL_UNIT_ASSIGNED_CONTEXT ( ( #53299, #73642, #98255 ) ) REPRESENTATION_CONTEXT ( 'NONE', 'WORKASPACE' ) );
#141031 = DIRECTION ( 'NONE',  ( 0.7071067811865486830, -0.7071067811865464625, -0.000000000000000000 ) ) ;
#141033 = ORIENTED_EDGE ( 'NONE', *, *, #11053, .F. ) ;
#141032 = CARTESIAN_POINT ( 'NONE',  ( -24.32816939922335919, -3.740707523384244837, 4.000000000000000000 ) ) ;
#141034 = DIRECTION ( 'NONE',  ( 0.7071067811865487940, 0.7071067811865463515, 0.000000000000000000 ) ) ;
#141035 = PLANE ( 'NONE',  #78793 ) ;
#141036 = FACE_OUTER_BOUND ( 'NONE', #60781, .T. ) ;
#141037 = ORIENTED_EDGE ( 'NONE', *, *, #60056, .T. ) ;
#141038 = ORIENTED_EDGE ( 'NONE', *, *, #54819, .T. ) ;
#141039 = CARTESIAN_POINT ( 'NONE',  ( 127.0000000000000568, -4.172191364199829167, -4.786994800550450790 ) ) ;
#141040 = LINE ( 'NONE', #85960, #58374 ) ;
#141041 = CIRCLE ( 'NONE', #64685, 2.500000000000000444 ) ;
#141042 = EDGE_CURVE ( 'NONE', #109446, #114222, #122323, .T. ) ;
#141043 = VECTOR ( 'NONE', #98034, 1000.000000000000000 ) ;
#141044 = DIRECTION ( 'NONE',  ( 0.3543493200069162685, -0.000000000000000000, -0.9351131265310288487 ) ) ;
#141045 = CARTESIAN_POINT ( 'NONE',  ( 81.16252705046289861, 7.949999999999998401, 1.460391307983218338E-15 ) ) ;
#141046 = CARTESIAN_POINT ( 'NONE',  ( -13.49999999999989697, -17.56887692260763245, 4.000000000000000000 ) ) ;
#141047 = DIRECTION ( 'NONE',  ( 1.000000000000000000, -0.000000000000000000, 0.000000000000000000 ) ) ;
#141048 = ORIENTED_EDGE ( 'NONE', *, *, #109193, .F. ) ;
#141049 = DIRECTION ( 'NONE',  ( -0.7071067811865486830, 0.7071067811865464625, 0.000000000000000000 ) ) ;
#141050 = DIRECTION ( 'NONE',  ( 0.6830127018922180770, -0.6830127018922204085, -0.2588190451025213501 ) ) ;
#141051 = CARTESIAN_POINT ( 'NONE',  ( 31.35416666666666785, 1.633150327867695095, 6.094999999999988205 ) ) ;
#141052 = EDGE_CURVE ( 'NONE', #12164, #81524, #67351, .T. ) ;
#141053 = VECTOR ( 'NONE', #101608, 1000.000000000000000 ) ;
#141054 = VERTEX_POINT ( 'NONE', #80302 ) ;
#141055 = PLANE ( 'NONE',  #95351 ) ;
#141056 = EDGE_CURVE ( 'NONE', #4889, #58332, #124491, .T. ) ;
#141057 = ORIENTED_EDGE ( 'NONE', *, *, #99069, .T. ) ;
#141058 = CARTESIAN_POINT ( 'NONE',  ( 79.47959685856477563, 6.109999999999999432, 1.637169565754164280 ) ) ;
#141059 = EDGE_CURVE ( 'NONE', #11920, #56350, #102754, .T. ) ;
#141060 = LINE ( 'NONE', #139682, #117150 ) ;
#141061 = CARTESIAN_POINT ( 'NONE',  ( 24.99033360189226016, 3.759292476615681888, 4.478963035907999490 ) ) ;
#141062 = ORIENTED_EDGE ( 'NONE', *, *, #66746, .F. ) ;
#141063 = CARTESIAN_POINT ( 'NONE',  ( 4.499999999999972466, 3.431123077392145948, 4.000000000000000000 ) ) ;
#141064 = EDGE_CURVE ( 'NONE', #128234, #78195, #133945, .T. ) ;
#141065 = CARTESIAN_POINT ( 'NONE',  ( 25.39999999999999858, -7.600000000000055600, -33.92499999999998295 ) ) ;
#141066 = LINE ( 'NONE', #109161, #101809 ) ;
#141067 = DIRECTION ( 'NONE',  ( -1.000000000000000000, -1.224606353822377258E-16, -0.000000000000000000 ) ) ;
#141069 = ORIENTED_EDGE ( 'NONE', *, *, #54736, .T. ) ;
#141068 = CARTESIAN_POINT ( 'NONE',  ( 45.29974487139158867, -27.71228299555237840, 4.000000000000000000 ) ) ;
#141070 = CARTESIAN_POINT ( 'NONE',  ( -29.99451991528749417, 28.92564299267958816, 4.000000000000000000 ) ) ;
#141071 = CARTESIAN_POINT ( 'NONE',  ( 77.70833333333332860, -3.974999999999999201, -6.884901960086287964 ) ) ;
#141072 = ADVANCED_FACE ( 'NONE', ( #34637 ), #123081, .F. ) ;
#141073 = DIRECTION ( 'NONE',  ( 0.6830127018922180770, -0.6830127018922204085, -0.2588190451025213501 ) ) ;
#141074 = VERTEX_POINT ( 'NONE', #136793 ) ;
#141075 = ORIENTED_EDGE ( 'NONE', *, *, #47305, .F. ) ;
#141076 = CARTESIAN_POINT ( 'NONE',  ( 71.31293019189810423, -1.637169565754159617, -6.110000000000001208 ) ) ;
#141077 = ORIENTED_EDGE ( 'NONE', *, *, #46899, .T. ) ;
#141078 = ADVANCED_FACE ( 'NONE', ( #25895 ), #6946, .F. ) ;
#141079 = CARTESIAN_POINT ( 'NONE',  ( 0.4892135623730947680, -27.52281430457055578, 5.000000000000000000 ) ) ;
#141080 = CARTESIAN_POINT ( 'NONE',  ( 6.471592354503322042, 9.902892378096218942E-16, 0.000000000000000000 ) ) ;
#141081 = DIRECTION ( 'NONE',  ( -0.000000000000000000, 0.3543493200069153248, 0.9351131265310292928 ) ) ;
#141082 = ORIENTED_EDGE ( 'NONE', *, *, #27628, .F. ) ;
#141083 = CARTESIAN_POINT ( 'NONE',  ( -6.888376381052371933, 9.759292476615621936, 17.35367589129214494 ) ) ;
#141084 = PLANE ( 'NONE',  #44377 ) ;
#141085 = VERTEX_POINT ( 'NONE', #95426 ) ;
#141086 = CARTESIAN_POINT ( 'NONE',  ( 125.5000000000000568, -3.922572014496796822, -6.914906274931464480 ) ) ;
#141087 = FACE_OUTER_BOUND ( 'NONE', #119391, .T. ) ;
#141088 = DIRECTION ( 'NONE',  ( -0.6830127018922181881, 0.6830127018922202975, -0.2588190451025214056 ) ) ;
#141089 = CIRCLE ( 'NONE', #78610, 5.968999999999998529 ) ;
#141090 = VECTOR ( 'NONE', #16935, 999.9999999999998863 ) ;
#141091 = VECTOR ( 'NONE', #65439, 1000.000000000000000 ) ;
#141092 = VERTEX_POINT ( 'NONE', #4796 ) ;
#141093 = ORIENTED_EDGE ( 'NONE', *, *, #119759, .T. ) ;
#141094 = VECTOR ( 'NONE', #46137, 1000.000000000000000 ) ;
#141095 = FACE_BOUND ( 'NONE', #96898, .T. ) ;
#141096 = DIRECTION ( 'NONE',  ( 0.6830127018922181881, 0.6830127018922202975, -0.2588190451025214056 ) ) ;
#141097 = LINE ( 'NONE', #109194, #99910 ) ;
#141098 = CARTESIAN_POINT ( 'NONE',  ( -24.18398860626899705, 28.73617430169804265, 5.000000000000000000 ) ) ;
#141099 =( GEOMETRIC_REPRESENTATION_CONTEXT ( 3 ) GLOBAL_UNCERTAINTY_ASSIGNED_CONTEXT ( ( #79564 ) ) GLOBAL_UNIT_ASSIGNED_CONTEXT ( ( #33390, #18891, #65292 ) ) REPRESENTATION_CONTEXT ( 'NONE', 'WORKASPACE' ) );
#141100 = CARTESIAN_POINT ( 'NONE',  ( -39.18398860626899705, 28.73617430169814568, 5.000000000000000000 ) ) ;
#141101 = DIRECTION ( 'NONE',  ( -0.000000000000000000, 0.3543493200069153248, 0.9351131265310292928 ) ) ;
#141102 = ORIENTED_EDGE ( 'NONE', *, *, #133199, .F. ) ;
#141103 = EDGE_CURVE ( 'NONE', #135001, #33848, #2520, .T. ) ;
#141104 = VECTOR ( 'NONE', #58342, 999.9999999999998863 ) ;
#141105 = ORIENTED_EDGE ( 'NONE', *, *, #8996, .T. ) ;
#141106 = ORIENTED_EDGE ( 'NONE', *, *, #35562, .T. ) ;
#141107 = ORIENTED_EDGE ( 'NONE', *, *, #106042, .F. ) ;
#141108 = CONICAL_SURFACE ( 'NONE', #6756, 2.055000000000000604, 0.9599310885968764806 ) ;
#141109 = VECTOR ( 'NONE', #55931, 1000.000000000000000 ) ;
#141110 = CARTESIAN_POINT ( 'NONE',  ( 183.8247562798506749, -48.93522302958620429, 39.28544916627627970 ) ) ;
#141111 = EDGE_CURVE ( 'NONE', #47430, #80191, #138227, .T. ) ;
#141112 = CARTESIAN_POINT ( 'NONE',  ( 1.500000000000000000, 0.000000000000000000, 9.500000000000001776 ) ) ;
#141113 = VECTOR ( 'NONE', #112901, 1000.000000000000000 ) ;
#141115 = EDGE_CURVE ( 'NONE', #78905, #44742, #28765, .T. ) ;
#141114 = FACE_OUTER_BOUND ( 'NONE', #41540, .T. ) ;
#141116 = ORIENTED_EDGE ( 'NONE', *, *, #138269, .F. ) ;
#141117 = LINE ( 'NONE', #84621, #143181 ) ;
#141118 = LINE ( 'NONE', #31668, #132841 ) ;
#141119 = PLANE ( 'NONE',  #138398 ) ;
#141120 = LINE ( 'NONE', #140419, #67027 ) ;
#141121 = VECTOR ( 'NONE', #71959, 1000.000000000000000 ) ;
#141122 = CARTESIAN_POINT ( 'NONE',  ( -12.79289321881336328, -14.24070752338414358, 5.000000000000000000 ) ) ;
#141123 = ORIENTED_EDGE ( 'NONE', *, *, #90476, .T. ) ;
#141124 = AXIS2_PLACEMENT_3D ( 'NONE', #33571, #121948, #55305 ) ;
#141125 = CARTESIAN_POINT ( 'NONE',  ( 66.18398860626901126, 28.73617430169833753, 5.000000000000000000 ) ) ;
#141126 = DIRECTION ( 'NONE',  ( -1.000000000000000000, -1.224606353822377258E-16, -0.000000000000000000 ) ) ;
#141127 = VECTOR ( 'NONE', #121762, 1000.000000000000000 ) ;
#141128 = ORIENTED_EDGE ( 'NONE', *, *, #80069, .T. ) ;
#141129 = CARTESIAN_POINT ( 'NONE',  ( -69.48921356237309510, -27.52281430457103895, 5.000000000000000000 ) ) ;
#141130 = ORIENTED_EDGE ( 'NONE', *, *, #123139, .T. ) ;
#141132 = ORIENTED_EDGE ( 'NONE', *, *, #66429, .T. ) ;
#141131 = ADVANCED_FACE ( 'NONE', ( #93293 ), #23326, .T. ) ;
#141133 = VECTOR ( 'NONE', #126294, 1000.000000000000000 ) ;
#141134 = ORIENTED_EDGE ( 'NONE', *, *, #635, .F. ) ;
#141136 = VECTOR ( 'NONE', #69975, 1000.000000000000000 ) ;
#141135 = CARTESIAN_POINT ( 'NONE',  ( 64.31293019189810423, -1.637169565754159617, -6.110000000000001208 ) ) ;
#141137 = ORIENTED_EDGE ( 'NONE', *, *, #129155, .F. ) ;
#141138 = ORIENTED_EDGE ( 'NONE', *, *, #103001, .F. ) ;
#141139 = CARTESIAN_POINT ( 'NONE',  ( 7.499999999999951150, -10.91253812416064584, 4.000000000000000000 ) ) ;
#141140 = SURFACE_SIDE_STYLE ('',( #54882 ) ) ;
#141141 = CARTESIAN_POINT ( 'NONE',  ( 101.3545968585647614, -1.637169565754161615, 6.110000000000000320 ) ) ;
#141142 = LINE ( 'NONE', #109237, #107330 ) ;
#141143 = DIRECTION ( 'NONE',  ( 0.7071067811865486830, -0.7071067811865464625, -0.000000000000000000 ) ) ;
#141144 = EDGE_LOOP ( 'NONE', ( #125349, #40791, #61935, #56126 ) ) ;
#141145 = DIRECTION ( 'NONE',  ( 0.7071067811865487940, 0.7071067811865463515, 0.000000000000000000 ) ) ;
#141146 = AXIS2_PLACEMENT_3D ( 'NONE', #134466, #35170, #56228 ) ;
#141147 = DIRECTION ( 'NONE',  ( 0.000000000000000000, 0.000000000000000000, 1.000000000000000000 ) ) ;
#141148 = PLANE ( 'NONE',  #120793 ) ;
#141149 = CARTESIAN_POINT ( 'NONE',  ( -8.510786437626906675, -27.52281430457049183, 5.000000000000000000 ) ) ;
#141150 = VERTEX_POINT ( 'NONE', #114325 ) ;
#141152 = EDGE_CURVE ( 'NONE', #42879, #110325, #92552, .T. ) ;
#141151 = CARTESIAN_POINT ( 'NONE',  ( 34.49999999999975842, 1.464255608400477415, 4.994342998332161443 ) ) ;
#141153 = ORIENTED_EDGE ( 'NONE', *, *, #28641, .F. ) ;
#141154 = ORIENTED_EDGE ( 'NONE', *, *, #66104, .T. ) ;
#141155 = ORIENTED_EDGE ( 'NONE', *, *, #22856, .T. ) ;
#141156 = CARTESIAN_POINT ( 'NONE',  ( 119.2037635252314658, 6.109999999999998543, 1.122388791418548911E-15 ) ) ;
#141157 = ORIENTED_EDGE ( 'NONE', *, *, #101167, .F. ) ;
#141158 = EDGE_CURVE ( 'NONE', #80458, #110318, #38212, .T. ) ;
#141159 = DIRECTION ( 'NONE',  ( -1.000000000000000000, -0.000000000000000000, -0.000000000000000000 ) ) ;
#141160 = DIRECTION ( 'NONE',  ( 0.000000000000000000, 0.000000000000000000, 1.000000000000000000 ) ) ;
#141161 = PLANE ( 'NONE',  #50975 ) ;
#141162 = EDGE_CURVE ( 'NONE', #41309, #106729, #90521, .T. ) ;
#141163 = EDGE_LOOP ( 'NONE', ( #22551, #20999, #73612, #31868 ) ) ;
#141164 = CARTESIAN_POINT ( 'NONE',  ( 0.8183591370940052068, -49.14999999999998437, 41.64499999999997470 ) ) ;
#141165 = ORIENTED_EDGE ( 'NONE', *, *, #95006, .T. ) ;
#141166 = EDGE_CURVE ( 'NONE', #119486, #125242, #139690, .T. ) ;
#141167 = ADVANCED_FACE ( 'NONE', ( #94694 ), #49099, .F. ) ;
#141168 = CARTESIAN_POINT ( 'NONE',  ( 2.166236474768552966, 7.934999999999990727, -1.457635852685135314E-15 ) ) ;
#141169 = FACE_OUTER_BOUND ( 'NONE', #123916, .T. ) ;
#141170 = EDGE_CURVE ( 'NONE', #84015, #95610, #27300, .T. ) ;
#141171 = FACE_OUTER_BOUND ( 'NONE', #75187, .T. ) ;
#141172 = CARTESIAN_POINT ( 'NONE',  ( 39.20833333333332860, -3.974999999999999201, -6.884901960086287964 ) ) ;
#141173 = ORIENTED_EDGE ( 'NONE', *, *, #101928, .F. ) ;
#141174 = VERTEX_POINT ( 'NONE', #17839 ) ;
#141175 = ADVANCED_FACE ( 'NONE', ( #105569 ), #39656, .F. ) ;
#141176 = ORIENTED_EDGE ( 'NONE', *, *, #18592, .T. ) ;
#141177 = CARTESIAN_POINT ( 'NONE',  ( 26.99999999999980105, -13.39766691384881092, -10.96608748226472052 ) ) ;
#141178 = DIRECTION ( 'NONE',  ( -0.7071067811865486830, -0.7071067811865464625, 0.000000000000000000 ) ) ;
#141179 = EDGE_CURVE ( 'NONE', #50236, #139610, #6231, .T. ) ;
#141180 = CARTESIAN_POINT ( 'NONE',  ( -14.47599861414540356, 22.03583458319439004, 4.979811245910085837 ) ) ;
#141181 = DIRECTION ( 'NONE',  ( 0.7071067811865487940, 0.7071067811865463515, -0.000000000000000000 ) ) ;
#141182 = EDGE_CURVE ( 'NONE', #93303, #132555, #141429, .T. ) ;
#141183 = VECTOR ( 'NONE', #3493, 1000.000000000000000 ) ;
#141184 = CARTESIAN_POINT ( 'NONE',  ( 9.489213562373095101, -27.52281430457062328, 5.000000000000000000 ) ) ;
#141185 = CARTESIAN_POINT ( 'NONE',  ( 30.18793019189809357, 6.110000000000002984, -1.637169565754156730 ) ) ;
#141186 = DIRECTION ( 'NONE',  ( 0.7071067811865487940, 0.7071067811865463515, 0.000000000000000000 ) ) ;
#141187 = ORIENTED_EDGE ( 'NONE', *, *, #41118, .T. ) ;
#141188 = PLANE ( 'NONE',  #64874 ) ;
#141189 = AXIS2_PLACEMENT_3D ( 'NONE', #136345, #25433, #37036 ) ;
#141190 = VECTOR ( 'NONE', #46194, 1000.000000000000000 ) ;
#141191 = CIRCLE ( 'NONE', #46360, 2.500000000000000888 ) ;
#141192 = LINE ( 'NONE', #44805, #24512 ) ;
#141193 = ORIENTED_EDGE ( 'NONE', *, *, #80106, .T. ) ;
#141194 = PRESENTATION_LAYER_ASSIGNMENT (  '', '', ( #134295 ) ) ;
#141195 = EDGE_CURVE ( 'NONE', #114640, #7978, #5546, .T. ) ;
#141197 = ORIENTED_EDGE ( 'NONE', *, *, #134682, .T. ) ;
#141196 = CARTESIAN_POINT ( 'NONE',  ( 41.97916666666665719, -7.950000000000000178, 2.130196079827424427 ) ) ;
#141198 = CARTESIAN_POINT ( 'NONE',  ( 57.18398860626899705, 28.73617430169827358, 5.000000000000000000 ) ) ;
#141199 = ORIENTED_EDGE ( 'NONE', *, *, #35749, .T. ) ;
#141200 = DIRECTION ( 'NONE',  ( -0.7071067811865486830, -0.7071067811865464625, 0.000000000000000000 ) ) ;
#141201 = VERTEX_POINT ( 'NONE', #50508 ) ;
#141202 = PLANE ( 'NONE',  #95249 ) ;
#141203 = VECTOR ( 'NONE', #47508, 1000.000000000000227 ) ;
#141204 = EDGE_LOOP ( 'NONE', ( #140491, #81286, #104751 ) ) ;
#141206 = EDGE_CURVE ( 'NONE', #126973, #95699, #128086, .T. ) ;
#141205 =( BOUNDED_CURVE ( )  B_SPLINE_CURVE ( 3, ( #40500, #7828, #8511, #20130 ),
 .UNSPECIFIED., .F., .T. ) 
 B_SPLINE_CURVE_WITH_KNOTS ( ( 4, 4 ),
 ( 2.280733380739273120, 2.329266631601943693 ),
 .UNSPECIFIED. ) 
 CURVE ( )  GEOMETRIC_REPRESENTATION_ITEM ( )  RATIONAL_B_SPLINE_CURVE ( ( 1.000000000000000000, 0.9998037199289477872, 0.9998037199289477872, 1.000000000000000000 ) ) 
 REPRESENTATION_ITEM ( '' )  );
#141207 = FACE_OUTER_BOUND ( 'NONE', #126233, .T. ) ;
#141208 = CARTESIAN_POINT ( 'NONE',  ( 119.0791937171295700, 3.975000000000002753, -6.884901960086283523 ) ) ;
#141209 = DIRECTION ( 'NONE',  ( 0.7071067811865487940, -0.7071067811865463515, 0.000000000000000000 ) ) ;
#141210 = DIRECTION ( 'NONE',  ( -0.000000000000000000, -0.3543493200069152138, 0.9351131265310292928 ) ) ;
#141211 = DIRECTION ( 'NONE',  ( -0.7071067811865486830, 0.7071067811865464625, 0.000000000000000000 ) ) ;
#141212 = LINE ( 'NONE', #71706, #3148 ) ;
#141213 = DIRECTION ( 'NONE',  ( 0.7071067811865487940, 0.7071067811865463515, -0.000000000000000000 ) ) ;
#141214 = CARTESIAN_POINT ( 'NONE',  ( 9.187500000000001776, 4.461849672132297329, -4.461849672132302658 ) ) ;
#141216 = VECTOR ( 'NONE', #138570, 1000.000000000000000 ) ;
#141215 = CARTESIAN_POINT ( 'NONE',  ( 16.31206980810188867, 7.934999999999992504, 2.126176841940951689 ) ) ;
#141217 = VECTOR ( 'NONE', #78143, 999.9999999999998863 ) ;
#141218 = FACE_OUTER_BOUND ( 'NONE', #19201, .T. ) ;
#141219 = CARTESIAN_POINT ( 'NONE',  ( -42.48921356237308800, -27.52281430457085065, 5.000000000000000000 ) ) ;
#141220 = ORIENTED_EDGE ( 'NONE', *, *, #89778, .F. ) ;
#141221 = EDGE_LOOP ( 'NONE', ( #76968, #74106, #111810, #81349 ) ) ;
#141222 = VECTOR ( 'NONE', #16233, 1000.000000000000000 ) ;
#141223 = DIRECTION ( 'NONE',  ( -0.7071067811865486830, -0.7071067811865464625, -0.000000000000000000 ) ) ;
#141224 = VERTEX_POINT ( 'NONE', #83881 ) ;
#141225 = EDGE_CURVE ( 'NONE', #115259, #138298, #73013, .T. ) ;
#141226 = VECTOR ( 'NONE', #143193, 1000.000000000000000 ) ;
#141227 = DIRECTION ( 'NONE',  ( -1.000000000000000000, -1.224606353822377258E-16, -0.000000000000000000 ) ) ;
#141228 = CARTESIAN_POINT ( 'NONE',  ( 20.65000000000000213, 0.000000000000000000, 6.350000000000008527 ) ) ;
#141229 = PLANE ( 'NONE',  #25527 ) ;
#141230 = CARTESIAN_POINT ( 'NONE',  ( 130.7303687233793994, -48.51451318982863370, -38.21513923099880117 ) ) ;
#141231 = ORIENTED_EDGE ( 'NONE', *, *, #133427, .F. ) ;
#141232 = CONICAL_SURFACE ( 'NONE', #39439, 2.500000000000000888, 0.9599310885968822538 ) ;
#141233 = CARTESIAN_POINT ( 'NONE',  ( -2.510786437626908008, -27.52281430457053446, 5.000000000000000000 ) ) ;
#141234 = EDGE_CURVE ( 'NONE', #6614, #110607, #85985, .T. ) ;
#141235 = CARTESIAN_POINT ( 'NONE',  ( 92.00000000000000000, 0.000000000000000000, -7.950000000000000178 ) ) ;
#141236 = VECTOR ( 'NONE', #80554, 1000.000000000000227 ) ;
#141237 = FACE_OUTER_BOUND ( 'NONE', #119345, .T. ) ;
#141239 = VERTEX_POINT ( 'NONE', #141065 ) ;
#141238 = DIRECTION ( 'NONE',  ( -0.000000000000000000, -0.000000000000000000, 1.000000000000000000 ) ) ;
#141240 = LINE ( 'NONE', #53538, #11895 ) ;
#141241 = VECTOR ( 'NONE', #140036, 1000.000000000000000 ) ;
#141242 = DIRECTION ( 'NONE',  ( -0.000000000000000000, 1.000000000000000000, -0.000000000000000000 ) ) ;
#141243 = CARTESIAN_POINT ( 'NONE',  ( -21.79289321881330110, -20.24070752338407075, 5.000000000000000000 ) ) ;
#141244 = EDGE_CURVE ( 'NONE', #140847, #78830, #128772, .T. ) ;
#141245 = CARTESIAN_POINT ( 'NONE',  ( 56.62524208091845423, -47.99115898043764616, 37.22402166429048975 ) ) ;
#141246 = VERTEX_POINT ( 'NONE', #19993 ) ;
#141247 = ORIENTED_EDGE ( 'NONE', *, *, #107335, .T. ) ;
#141248 = ORIENTED_EDGE ( 'NONE', *, *, #131201, .T. ) ;
#141249 = CARTESIAN_POINT ( 'NONE',  ( 102.3754301918981184, -5.291415217122920289, -3.055000000000001492 ) ) ;
#141250 = VECTOR ( 'NONE', #59675, 999.9999999999998863 ) ;
#141251 = ORIENTED_EDGE ( 'NONE', *, *, #41405, .F. ) ;
#141252 = EDGE_CURVE ( 'NONE', #52888, #108664, #130942, .T. ) ;
#141253 = CARTESIAN_POINT ( 'NONE',  ( 126.8009042512159539, -49.32595796886460704, 36.54674188582824002 ) ) ;
#141254 = VECTOR ( 'NONE', #118945, 1000.000000000000000 ) ;
#141255 = CARTESIAN_POINT ( 'NONE',  ( 6.160000000000001030, -2.055000000000000160, 2.789133085058098087E-16 ) ) ;
#141256 = ORIENTED_EDGE ( 'NONE', *, *, #60189, .F. ) ;
#141257 = CARTESIAN_POINT ( 'NONE',  ( 12.19999999999999574, -22.33999999999998565, 0.000000000000000000 ) ) ;
#141258 = CARTESIAN_POINT ( 'NONE',  ( -8.187538124160473885, -22.22500000000000142, 4.000000000000000000 ) ) ;
#141259 = CARTESIAN_POINT ( 'NONE',  ( 94.55793019189810877, 6.110000000000000320, -1.637169565754156064 ) ) ;
#141260 = EDGE_LOOP ( 'NONE', ( #90899, #45419, #39420, #140755, #94667, #71931, #101398, #15415, #106174, #98289 ) ) ;
#141261 = ADVANCED_FACE ( 'NONE', ( #140361 ), #41053, .F. ) ;
#141262 = CARTESIAN_POINT ( 'NONE',  ( 11.99451991528749417, 28.92564299267946382, 4.000000000000000000 ) ) ;
#141263 = DIRECTION ( 'NONE',  ( -0.7071067811865486830, -0.7071067811865464625, 0.000000000000000000 ) ) ;
#141264 = CARTESIAN_POINT ( 'NONE',  ( 7.940000000000001279, -33.26999999999999602, -10.00000000000000178 ) ) ;
#141265 = VECTOR ( 'NONE', #122063, 1000.000000000000000 ) ;
#141266 = CARTESIAN_POINT ( 'NONE',  ( 7.499999999999954703, 6.277155672890280869, -3.510561720658957441 ) ) ;
#141267 = ORIENTED_EDGE ( 'NONE', *, *, #8647, .T. ) ;
#141268 = ORIENTED_EDGE ( 'NONE', *, *, #123938, .T. ) ;
#141269 = EDGE_CURVE ( 'NONE', #5220, #48400, #109875, .T. ) ;
#141270 = ORIENTED_EDGE ( 'NONE', *, *, #131889, .T. ) ;
#141271 = CARTESIAN_POINT ( 'NONE',  ( 10.49999999999993605, -5.947814304570766986, 5.000000000000000000 ) ) ;
#141272 = EDGE_CURVE ( 'NONE', #139596, #115334, #96127, .T. ) ;
#141273 = CARTESIAN_POINT ( 'NONE',  ( -18.18398860626898994, 28.73617430169800002, 5.000000000000000000 ) ) ;
#141274 = CARTESIAN_POINT ( 'NONE',  ( 17.12956980810188767, -3.967499999999998028, -6.871911579029511330 ) ) ;
#141275 = VECTOR ( 'NONE', #88829, 1000.000000000000000 ) ;
#141276 = DIRECTION ( 'NONE',  ( -0.6830127018922180770, -0.6830127018922204085, -0.2588190451025213501 ) ) ;
#141277 = CARTESIAN_POINT ( 'NONE',  ( 6.932893218813447334, -34.94289321881344534, -40.00000000000000000 ) ) ;
#141278 = EDGE_CURVE ( 'NONE', #13019, #93595, #10539, .T. ) ;
#141279 = ORIENTED_EDGE ( 'NONE', *, *, #51057, .T. ) ;
#141280 = ORIENTED_EDGE ( 'NONE', *, *, #51503, .F. ) ;
#141281 = DIRECTION ( 'NONE',  ( -1.000000000000000000, -0.000000000000000000, -0.000000000000000000 ) ) ;
#141282 = ORIENTED_EDGE ( 'NONE', *, *, #66607, .T. ) ;
#141283 = EDGE_LOOP ( 'NONE', ( #83195, #14468, #115072, #76507 ) ) ;
#141284 = AXIS2_PLACEMENT_3D ( 'NONE', #49050, #124445, #25846 ) ;
#141285 = ADVANCED_FACE ( 'NONE', ( #29447 ), #54802, .F. ) ;
#141286 = CIRCLE ( 'NONE', #78810, 2.999999999999999556 ) ;
#141287 = AXIS2_PLACEMENT_3D ( 'NONE', #58254, #938, #143064 ) ;
#141288 = FILL_AREA_STYLE_COLOUR ( '', #9561 ) ;
#141290 = EDGE_CURVE ( 'NONE', #134483, #93602, #86717, .T. ) ;
#141289 = DIRECTION ( 'NONE',  ( 0.000000000000000000, -1.000000000000000000, 0.000000000000000000 ) ) ;
#141291 = ORIENTED_EDGE ( 'NONE', *, *, #51792, .T. ) ;
#141292 = DIRECTION ( 'NONE',  ( -0.7071067811865487940, 0.7071067811865463515, -0.000000000000000000 ) ) ;
#141293 = CARTESIAN_POINT ( 'NONE',  ( 15.83159235450332147, 2.500000000000001776, 0.000000000000000000 ) ) ;
#141294 = VECTOR ( 'NONE', #116854, 999.9999999999998863 ) ;
#141295 = CARTESIAN_POINT ( 'NONE',  ( 17.54840764549667398, 0.000000000000000000, 2.500000000000001332 ) ) ;
#141296 = PLANE ( 'NONE',  #34529 ) ;
#141297 = CIRCLE ( 'NONE', #32558, 4.000000000000000000 ) ;
#141298 = AXIS2_PLACEMENT_3D ( 'NONE', #58890, #126912, #114616 ) ;
#141299 = VECTOR ( 'NONE', #141178, 1000.000000000000000 ) ;
#141300 = MECHANICAL_DESIGN_GEOMETRIC_PRESENTATION_REPRESENTATION (  '', ( #4984 ), #55975 ) ;
#141301 = LINE ( 'NONE', #42014, #116072 ) ;
#141302 = VERTEX_POINT ( 'NONE', #9085 ) ;
#141303 = AXIS2_PLACEMENT_3D ( 'NONE', #67934, #54195, #88220 ) ;
#141304 = CARTESIAN_POINT ( 'NONE',  ( 12.35051985313232237, 0.000000000000000000, 2.500000000000000444 ) ) ;
#141305 = ORIENTED_EDGE ( 'NONE', *, *, #25145, .F. ) ;
#141306 = CARTESIAN_POINT ( 'NONE',  ( 25.40000000000000924, 6.150563586872422661, -5.029781026407817990 ) ) ;
#141307 = DIRECTION ( 'NONE',  ( -0.6830127018922180770, -0.6830127018922204085, -0.2588190451025213501 ) ) ;
#141308 = EDGE_LOOP ( 'NONE', ( #22309, #53260, #43964, #18092 ) ) ;
#141309 = EDGE_CURVE ( 'NONE', #97669, #22290, #120743, .T. ) ;
#141310 = ORIENTED_EDGE ( 'NONE', *, *, #3667, .T. ) ;
#141311 = PLANE ( 'NONE',  #113071 ) ;
#141312 = ORIENTED_EDGE ( 'NONE', *, *, #120521, .T. ) ;
#141313 = ORIENTED_EDGE ( 'NONE', *, *, #63054, .F. ) ;
#141314 = CIRCLE ( 'NONE', #44167, 2.500000000000000888 ) ;
#141315 = VERTEX_POINT ( 'NONE', #21449 ) ;
#141316 = CARTESIAN_POINT ( 'NONE',  ( 31.26626352523144448, 4.472830434245838482, -4.472830434245837594 ) ) ;
#141317 = PLANE ( 'NONE',  #83111 ) ;
#141318 = DIRECTION ( 'NONE',  ( 0.000000000000000000, 0.000000000000000000, 1.000000000000000000 ) ) ;
#141319 = SURFACE_SIDE_STYLE ('',( #99968 ) ) ;
#141320 = CARTESIAN_POINT ( 'NONE',  ( -7.499999999999958256, 19.08746187583906462, 4.000000000000000000 ) ) ;
#141321 = CARTESIAN_POINT ( 'NONE',  ( -18.48921356237309510, -27.52281430457068367, 5.000000000000000000 ) ) ;
#141323 = DIRECTION ( 'NONE',  ( -0.000000000000000000, -0.3543493200069152693, 0.9351131265310292928 ) ) ;
#141322 = DIRECTION ( 'NONE',  ( 0.7071067811865486830, -0.7071067811865464625, -0.000000000000000000 ) ) ;
#141324 = VECTOR ( 'NONE', #96976, 1000.000000000000227 ) ;
#141325 = CARTESIAN_POINT ( 'NONE',  ( 4.734933297179464873, 12.75929247661558286, 18.34774599283955254 ) ) ;
#141326 = AXIS2_PLACEMENT_3D ( 'NONE', #23047, #135437, #57888 ) ;
#141327 = DIRECTION ( 'NONE',  ( 0.7071067811865486830, -0.7071067811865464625, -0.000000000000000000 ) ) ;
#141328 = VECTOR ( 'NONE', #79860, 1000.000000000000000 ) ;
#141329 = CARTESIAN_POINT ( 'NONE',  ( -5.999999999999952927, -7.447814304570758104, 5.000000000000000000 ) ) ;
#141330 = LINE ( 'NONE', #51488, #116556 ) ;
#141331 = ORIENTED_EDGE ( 'NONE', *, *, #124396, .F. ) ;
#141332 = VECTOR ( 'NONE', #75633, 1000.000000000000227 ) ;
#141333 = ORIENTED_EDGE ( 'NONE', *, *, #121336, .T. ) ;
#141334 = ORIENTED_EDGE ( 'NONE', *, *, #7060, .F. ) ;
#141335 = EDGE_LOOP ( 'NONE', ( #113574, #33177, #139050, #77844 ) ) ;
#141336 = FACE_OUTER_BOUND ( 'NONE', #50864, .T. ) ;
#141337 = ORIENTED_EDGE ( 'NONE', *, *, #95993, .F. ) ;
#141338 = AXIS2_PLACEMENT_3D ( 'NONE', #87195, #41527, #51008 ) ;
#141339 = EDGE_LOOP ( 'NONE', ( #7780, #18157, #49327, #114235 ) ) ;
#141340 = CARTESIAN_POINT ( 'NONE',  ( 0.000000000000000000, 0.000000000000000000, 5.000000000000000000 ) ) ;
#141341 = CARTESIAN_POINT ( 'NONE',  ( -34.92500000000001137, -22.22500000000000142, 4.500000000000000888 ) ) ;
#141342 =( GEOMETRIC_REPRESENTATION_CONTEXT ( 3 ) GLOBAL_UNCERTAINTY_ASSIGNED_CONTEXT ( ( #2482 ) ) GLOBAL_UNIT_ASSIGNED_CONTEXT ( ( #112838, #134625, #24408 ) ) REPRESENTATION_CONTEXT ( 'NONE', 'WORKASPACE' ) );
#141343 = CARTESIAN_POINT ( 'NONE',  ( 7.828169399223476432, -14.24070752338413293, 4.000000000000000000 ) ) ;
#141344 = VERTEX_POINT ( 'NONE', #8379 ) ;
#141345 = DIRECTION ( 'NONE',  ( -0.000000000000000000, -0.3543493200069152693, 0.9351131265310292928 ) ) ;
#141346 = ORIENTED_EDGE ( 'NONE', *, *, #7603, .F. ) ;
#141347 = LINE ( 'NONE', #128357, #7928 ) ;
#141348 = ADVANCED_FACE ( 'NONE', ( #117857 ), #142526, .F. ) ;
#141349 =( GEOMETRIC_REPRESENTATION_CONTEXT ( 3 ) GLOBAL_UNCERTAINTY_ASSIGNED_CONTEXT ( ( #56579 ) ) GLOBAL_UNIT_ASSIGNED_CONTEXT ( ( #38703, #4571, #127117 ) ) REPRESENTATION_CONTEXT ( 'NONE', 'WORKASPACE' ) );
#141350 = CARTESIAN_POINT ( 'NONE',  ( 10.42123647476855375, -9.717572351234235426E-16, -7.934999999999990727 ) ) ;
#141351 = VERTEX_POINT ( 'NONE', #63557 ) ;
#141352 = CARTESIAN_POINT ( 'NONE',  ( 95.87043019189810877, -3.055000000000001936, 5.291415217122918513 ) ) ;
#141353 = EDGE_CURVE ( 'NONE', #94963, #108745, #129476, .T. ) ;
#141354 = DIRECTION ( 'NONE',  ( -0.000000000000000000, 0.3543493200069153248, 0.9351131265310292928 ) ) ;
#141355 = ADVANCED_FACE ( 'NONE', ( #107011 ), #120001, .T. ) ;
#141356 = CARTESIAN_POINT ( 'NONE',  ( 55.28643332384059761, -49.19207878845114834, -41.22112633375382984 ) ) ;
#141357 = CARTESIAN_POINT ( 'NONE',  ( 31.92500000000001492, 0.4299755680430057958, -27.68972139052992532 ) ) ;
#141358 = ORIENTED_EDGE ( 'NONE', *, *, #110186, .F. ) ;
#141359 = ORIENTED_EDGE ( 'NONE', *, *, #45064, .T. ) ;
#141360 = ADVANCED_FACE ( 'NONE', ( #84574 ), #141815, .F. ) ;
#141361 = DIRECTION ( 'NONE',  ( -0.7071067811865486830, -0.7071067811865464625, 0.000000000000000000 ) ) ;
#141362 = AXIS2_PLACEMENT_3D ( 'NONE', #65142, #141987, #65872 ) ;
#141363 = VERTEX_POINT ( 'NONE', #64971 ) ;
#141364 = CARTESIAN_POINT ( 'NONE',  ( 9.005480084712511157, 28.92564299267931816, 4.000000000000000000 ) ) ;
#141365 = LINE ( 'NONE', #140640, #65041 ) ;
#141366 = DIRECTION ( 'NONE',  ( 0.000000000000000000, 0.000000000000000000, -1.000000000000000000 ) ) ;
#141367 = EDGE_CURVE ( 'NONE', #90068, #61512, #109160, .T. ) ;
#141368 = LINE ( 'NONE', #76121, #105100 ) ;
#141369 = VERTEX_POINT ( 'NONE', #65712 ) ;
#141370 = CARTESIAN_POINT ( 'NONE',  ( 6.792893218813411238, -20.24070752338407431, 5.000000000000000000 ) ) ;
#141371 = EDGE_CURVE ( 'NONE', #37438, #72185, #91006, .T. ) ;
#141372 = DIRECTION ( 'NONE',  ( 0.7071067811865487940, 0.7071067811865463515, 0.000000000000000000 ) ) ;
#141373 = CARTESIAN_POINT ( 'NONE',  ( -33.18398860626899705, 28.73617430169810305, 5.000000000000000000 ) ) ;
#141374 = ORIENTED_EDGE ( 'NONE', *, *, #25016, .F. ) ;
#141375 = DIRECTION ( 'NONE',  ( -1.000000000000000000, -1.224606353822377258E-16, -0.000000000000000000 ) ) ;
#141376 = VECTOR ( 'NONE', #141345, 1000.000000000000000 ) ;
#141377 = CARTESIAN_POINT ( 'NONE',  ( -32.20710678118631876, 18.75929247661553489, 5.000000000000000000 ) ) ;
#141378 = VERTEX_POINT ( 'NONE', #55515 ) ;
#141379 = EDGE_CURVE ( 'NONE', #138104, #104458, #101853, .T. ) ;
#141381 = ORIENTED_EDGE ( 'NONE', *, *, #80668, .T. ) ;
#141380 = CARTESIAN_POINT ( 'NONE',  ( 0.1164707300447627020, -51.38852430739338217, -37.54101415799215857 ) ) ;
#141382 = ORIENTED_EDGE ( 'NONE', *, *, #70576, .F. ) ;
#141383 = ADVANCED_FACE ( 'NONE', ( #35202 ), #12686, .F. ) ;
#141384 = CARTESIAN_POINT ( 'NONE',  ( 27.29974487139158512, -27.71228299555225405, 4.000000000000000000 ) ) ;
#141385 = DIRECTION ( 'NONE',  ( -0.000000000000000000, 0.000000000000000000, 1.000000000000000000 ) ) ;
#141387 = ORIENTED_EDGE ( 'NONE', *, *, #15035, .T. ) ;
#141386 = AXIS2_PLACEMENT_3D ( 'NONE', #14648, #92184, #92916 ) ;
#141388 = DIRECTION ( 'NONE',  ( -0.000000000000000000, 0.3543493200069153248, 0.9351131265310292928 ) ) ;
#141389 = EDGE_CURVE ( 'NONE', #115605, #125405, #133092, .T. ) ;
#141390 = CARTESIAN_POINT ( 'NONE',  ( 0.2997448713915885632, -27.71228299555206220, 4.000000000000000000 ) ) ;
#141391 = DIRECTION ( 'NONE',  ( -0.7071067811865486830, -0.7071067811865464625, 0.000000000000000000 ) ) ;
#141392 = CARTESIAN_POINT ( 'NONE',  ( 31.62500000000000000, -7.950000000000000178, -4.867971026610729436E-16 ) ) ;
#141393 = CARTESIAN_POINT ( 'NONE',  ( 3.500000000000000444, 0.000000000000000000, 6.094999999999989981 ) ) ;
#141394 = CARTESIAN_POINT ( 'NONE',  ( 45.48921356237309510, -27.52281430457087197, 5.000000000000000000 ) ) ;
#141395 = DIRECTION ( 'NONE',  ( -0.6830127018922181881, 0.6830127018922202975, -0.2588190451025214056 ) ) ;
#141396 = EDGE_CURVE ( 'NONE', #110142, #121003, #35918, .T. ) ;
#141397 = LINE ( 'NONE', #42113, #8716 ) ;
#141398 = CARTESIAN_POINT ( 'NONE',  ( 25.49999999999982947, -1.912538124160735542, 4.000000000000000000 ) ) ;
#141399 = DIRECTION ( 'NONE',  ( -0.7071067811865486830, -0.7071067811865464625, 0.000000000000000000 ) ) ;
#141400 = VECTOR ( 'NONE', #39608, 1000.000000000000000 ) ;
#141401 = DIRECTION ( 'NONE',  ( 1.000000000000000000, 0.000000000000000000, 0.000000000000000000 ) ) ;
#141402 = FACE_OUTER_BOUND ( 'NONE', #37025, .T. ) ;
#141403 = EDGE_LOOP ( 'NONE', ( #33186, #83056, #12043, #48257, #96188, #123381 ) ) ;
#141404 = ORIENTED_EDGE ( 'NONE', *, *, #51338, .F. ) ;
#141405 = VERTEX_POINT ( 'NONE', #14117 ) ;
#141406 = VECTOR ( 'NONE', #115226, 999.9999999999998863 ) ;
#141407 = CARTESIAN_POINT ( 'NONE',  ( 115.0416666666666714, -3.975000000000002753, 6.884901960086286188 ) ) ;
#141408 = CIRCLE ( 'NONE', #81206, 2.500000000000000888 ) ;
#141409 = EDGE_LOOP ( 'NONE', ( #55017, #128146, #36477, #69810, #20038, #80101 ) ) ;
#141410 = EDGE_LOOP ( 'NONE', ( #82394, #81062, #130356, #120491 ) ) ;
#141411 = VERTEX_POINT ( 'NONE', #22134 ) ;
#141412 = ADVANCED_FACE ( 'NONE', ( #124319 ), #56263, .F. ) ;
#141413 = LINE ( 'NONE', #85588, #124313 ) ;
#141414 = CARTESIAN_POINT ( 'NONE',  ( -9.524999999999991473, -4.870000000000014317, -10.00000000000000178 ) ) ;
#141415 = VECTOR ( 'NONE', #98738, 999.9999999999998863 ) ;
#141416 = VECTOR ( 'NONE', #128895, 1000.000000000000227 ) ;
#141417 = VECTOR ( 'NONE', #81327, 1000.000000000000000 ) ;
#141418 = AXIS2_PLACEMENT_3D ( 'NONE', #132749, #33439, #99341 ) ;
#141419 = ORIENTED_EDGE ( 'NONE', *, *, #73941, .F. ) ;
#141420 = CARTESIAN_POINT ( 'NONE',  ( 153.4000000000000057, -16.48000000000005016, -34.92499999999998295 ) ) ;
#141421 = AXIS2_PLACEMENT_3D ( 'NONE', #46165, #14204, #102671 ) ;
#141422 = LINE ( 'NONE', #126956, #32624 ) ;
#141423 = DIRECTION ( 'NONE',  ( -0.3543493200069162685, -0.000000000000000000, -0.9351131265310288487 ) ) ;
#141424 = DIRECTION ( 'NONE',  ( 0.7071067811865487940, -0.7071067811865463515, 0.000000000000000000 ) ) ;
#141425 = CARTESIAN_POINT ( 'NONE',  ( 100.6254301918981042, 5.291415217122919401, 3.055000000000002824 ) ) ;
#141426 = VERTEX_POINT ( 'NONE', #34461 ) ;
#141427 = CARTESIAN_POINT ( 'NONE',  ( 16.45742106731621135, 0.9613713492673626737, -33.49048331797055766 ) ) ;
#141428 = CARTESIAN_POINT ( 'NONE',  ( -15.63964197871511885, 8.074661077379714058, 4.334728602384618767 ) ) ;
#141429 = CIRCLE ( 'NONE', #95154, 2.500000000000000444 ) ;
#141430 = CARTESIAN_POINT ( 'NONE',  ( -8.999999999999941380, -13.06887692260767686, 4.000000000000000000 ) ) ;
#141431 = CARTESIAN_POINT ( 'NONE',  ( 34.42499999999998295, 22.22500000000000142, 4.165035510187007795 ) ) ;
#141432 = DIRECTION ( 'NONE',  ( -0.000000000000000000, 0.000000000000000000, 1.000000000000000000 ) ) ;
#141433 = CARTESIAN_POINT ( 'NONE',  ( 0.5724039806122919183, -0.5999999999999993117, -4.262472862582124655 ) ) ;
#141434 = CARTESIAN_POINT ( 'NONE',  ( -74.99451991528749772, 28.92564299267990435, 4.000000000000000000 ) ) ;
#141435 = EDGE_CURVE ( 'NONE', #74099, #136109, #56958, .T. ) ;
#141436 = CARTESIAN_POINT ( 'NONE',  ( -25.39999999999996305, 0.000000000000000000, 2.500000000000000000 ) ) ;
#141437 = EDGE_LOOP ( 'NONE', ( #104469, #134012, #92170, #23710, #28686 ) ) ;
#141438 = ORIENTED_EDGE ( 'NONE', *, *, #112131, .T. ) ;
#141439 = CARTESIAN_POINT ( 'NONE',  ( 28.41666666666666075, -6.884901960086287076, -3.975000000000000977 ) ) ;
#141440 = ORIENTED_EDGE ( 'NONE', *, *, #128754, .T. ) ;
#141441 = VECTOR ( 'NONE', #77663, 1000.000000000000000 ) ;
#141442 = LINE ( 'NONE', #96468, #66855 ) ;
#141443 = ADVANCED_FACE ( 'NONE', ( #101131 ), #123007, .T. ) ;
#141444 = VECTOR ( 'NONE', #57082, 1000.000000000000000 ) ;
#141445 = CARTESIAN_POINT ( 'NONE',  ( -34.92500000000001137, 21.72500000000000142, 5.000000000000000000 ) ) ;
#141446 = LINE ( 'NONE', #118235, #59621 ) ;
#141447 = DIRECTION ( 'NONE',  ( -1.000000000000000000, -1.224606353822377258E-16, -0.000000000000000000 ) ) ;
#141448 = CARTESIAN_POINT ( 'NONE',  ( 45.18398860626900415, 28.73617430169818832, 5.000000000000000000 ) ) ;
#141449 = AXIS2_PLACEMENT_3D ( 'NONE', #105279, #53025, #86406 ) ;
#141450 = AXIS2_PLACEMENT_3D ( 'NONE', #37327, #59801, #27145 ) ;
#141451 = CARTESIAN_POINT ( 'NONE',  ( 119.4954301918981230, 5.291415217122916737, 3.055000000000001936 ) ) ;
#141452 = ORIENTED_EDGE ( 'NONE', *, *, #75018, .T. ) ;
#141453 = EDGE_CURVE ( 'NONE', #124154, #31469, #11239, .T. ) ;
#141454 = VECTOR ( 'NONE', #68096, 1000.000000000000227 ) ;
#141455 = DIRECTION ( 'NONE',  ( -1.000000000000000000, -1.224606353822377258E-16, -0.000000000000000000 ) ) ;
#141456 = ORIENTED_EDGE ( 'NONE', *, *, #142187, .F. ) ;
#141457 = DIRECTION ( 'NONE',  ( 0.7071067811865487940, -0.7071067811865463515, 0.000000000000000000 ) ) ;
#141458 = AXIS2_PLACEMENT_3D ( 'NONE', #48691, #92895, #62436 ) ;
#141459 = DIRECTION ( 'NONE',  ( -0.000000000000000000, -0.000000000000000000, 1.000000000000000000 ) ) ;
#141460 = LINE ( 'NONE', #130603, #71912 ) ;
#141461 = DIRECTION ( 'NONE',  ( -0.5735764363510499342, -0.8191520442889891340, 0.000000000000000000 ) ) ;
#141462 = VERTEX_POINT ( 'NONE', #102591 ) ;
#141463 = CARTESIAN_POINT ( 'NONE',  ( 46.52126352523142572, -4.472830434245839371, -4.472830434245840259 ) ) ;
#141464 = EDGE_CURVE ( 'NONE', #21453, #127775, #2625, .T. ) ;
#141465 = VERTEX_POINT ( 'NONE', #89547 ) ;
#141466 = CARTESIAN_POINT ( 'NONE',  ( -18.79289321881331887, -5.240707523384230626, 5.000000000000000000 ) ) ;
#141467 = CARTESIAN_POINT ( 'NONE',  ( 13.17183060077638324, -17.24070752338410628, 4.000000000000000000 ) ) ;
#141468 = DIRECTION ( 'NONE',  ( 0.000000000000000000, 0.000000000000000000, -1.000000000000000000 ) ) ;
#141469 = DIRECTION ( 'NONE',  ( -0.000000000000000000, -0.3543493200069152693, 0.9351131265310292928 ) ) ;
#141470 = VECTOR ( 'NONE', #90296, 999.9999999999998863 ) ;
#141471 = CARTESIAN_POINT ( 'NONE',  ( 40.74543019189810877, -5.291415217122918513, -3.055000000000000160 ) ) ;
#141472 = ORIENTED_EDGE ( 'NONE', *, *, #130521, .T. ) ;
#141473 = DIRECTION ( 'NONE',  ( -0.7071067811865486830, -0.7071067811865464625, -0.000000000000000000 ) ) ;
#141474 = ORIENTED_EDGE ( 'NONE', *, *, #37313, .T. ) ;
#141475 = VERTEX_POINT ( 'NONE', #1776 ) ;
#141476 = VECTOR ( 'NONE', #97743, 1000.000000000000227 ) ;
#141477 = ORIENTED_EDGE ( 'NONE', *, *, #1841, .F. ) ;
#141478 = VECTOR ( 'NONE', #84006, 999.9999999999998863 ) ;
#141479 = DIRECTION ( 'NONE',  ( -1.000000000000000000, -1.369518533665900312E-16, 0.000000000000000000 ) ) ;
#141480 = ADVANCED_FACE ( 'NONE', ( #122897 ), #118436, .T. ) ;
#141481 = ORIENTED_EDGE ( 'NONE', *, *, #23700, .F. ) ;
#141482 = DIRECTION ( 'NONE',  ( -1.000000000000000000, -1.224606353822377258E-16, -0.000000000000000000 ) ) ;
#141483 = AXIS2_PLACEMENT_3D ( 'NONE', #110655, #53459, #133877 ) ;
#141484 = DIRECTION ( 'NONE',  ( -0.3543493200069162685, -0.000000000000000000, -0.9351131265310288487 ) ) ;
#141485 =( BOUNDED_CURVE ( )  B_SPLINE_CURVE ( 2, ( #85123, #60002, #49849, #58624, #60750, #4834, #15711, #115747, #25937, #85832, #8244, #103466, #30019 ),
 .UNSPECIFIED., .F., .T. ) 
 B_SPLINE_CURVE_WITH_KNOTS ( ( 3, 2, 2, 2, 2, 2, 3 ),
 ( 0.5833333333333333703, 0.5861111111111111382, 0.5888888888888889062, 0.5916666666666666741, 0.5944444444444444420, 0.5972222222222222099, 0.5999999999999999778 ),
 .UNSPECIFIED. ) 
 CURVE ( )  GEOMETRIC_REPRESENTATION_ITEM ( )  RATIONAL_B_SPLINE_CURVE ( ( 1.000000000000000000, 0.9659258262890683122, 1.000000000000000000, 0.9659258262890683122, 1.000000000000000000, 0.9659258262890683122, 1.000000000000000000, 0.9659258262890683122, 1.000000000000000000, 0.9659258262890683122, 1.000000000000000000, 0.9659258262890683122, 1.000000000000000000 ) ) 
 REPRESENTATION_ITEM ( '' )  );
#141486 = DIRECTION ( 'NONE',  ( -0.7071067811865486830, 0.7071067811865464625, 0.000000000000000000 ) ) ;
#141487 = EDGE_CURVE ( 'NONE', #142366, #63264, #28595, .T. ) ;
#141488 = FACE_BOUND ( 'NONE', #28564, .T. ) ;
#141489 = VERTEX_POINT ( 'NONE', #93126 ) ;
#141490 = CARTESIAN_POINT ( 'NONE',  ( 48.48921356237309510, -27.52281430457089328, 5.000000000000000000 ) ) ;
#141491 = LINE ( 'NONE', #129169, #21263 ) ;
#141493 = EDGE_CURVE ( 'NONE', #56410, #28809, #74570, .T. ) ;
#141492 = DIRECTION ( 'NONE',  ( -1.000000000000000000, 0.000000000000000000, -0.000000000000000000 ) ) ;
#141494 = EDGE_LOOP ( 'NONE', ( #1377, #59595, #66911, #75225 ) ) ;
#141495 = EDGE_CURVE ( 'NONE', #135742, #128359, #69990, .T. ) ;
#141496 = CARTESIAN_POINT ( 'NONE',  ( -22.62823445044371340, -8.240707523384196875, 11.38925528200757853 ) ) ;
#141497 = ORIENTED_EDGE ( 'NONE', *, *, #116409, .F. ) ;
#141498 = ORIENTED_EDGE ( 'NONE', *, *, #103325, .T. ) ;
#141499 = VECTOR ( 'NONE', #74585, 1000.000000000000000 ) ;
#141500 = LINE ( 'NONE', #138656, #95776 ) ;
#141501 = ORIENTED_EDGE ( 'NONE', *, *, #13305, .F. ) ;
#141502 = CARTESIAN_POINT ( 'NONE',  ( 56.05793019189811588, 6.110000000000000320, -1.637169565754156064 ) ) ;
#141503 = EDGE_LOOP ( 'NONE', ( #26581, #59175, #33587, #26971 ) ) ;
#141504 = PLANE ( 'NONE',  #136670 ) ;
#141505 = DIRECTION ( 'NONE',  ( 0.6830127018922181881, 0.6830127018922202975, -0.2588190451025214056 ) ) ;
#141506 = ORIENTED_EDGE ( 'NONE', *, *, #5818, .F. ) ;
#141507 = LINE ( 'NONE', #19008, #60786 ) ;
#141508 = DIRECTION ( 'NONE',  ( -0.7071067811865486830, -0.7071067811865464625, 0.000000000000000000 ) ) ;
#141509 = AXIS2_PLACEMENT_3D ( 'NONE', #50088, #127641, #18111 ) ;
#141510 = ADVANCED_FACE ( 'NONE', ( #72852 ), #14837, .F. ) ;
#141511 = VECTOR ( 'NONE', #85874, 1000.000000000000000 ) ;
#141512 = VECTOR ( 'NONE', #70207, 999.9999999999998863 ) ;
#141513 = DIRECTION ( 'NONE',  ( 0.7071067811865487940, 0.7071067811865463515, 0.000000000000000000 ) ) ;
#141514 = DIRECTION ( 'NONE',  ( -0.5735764363510507113, 0.8191520442889885789, 1.003171929053520926E-16 ) ) ;
#141515 = CARTESIAN_POINT ( 'NONE',  ( 12.47336096364207236, -5.240707523384232402, 16.25846745537498705 ) ) ;
#141516 = CARTESIAN_POINT ( 'NONE',  ( -28.17183060077627843, 21.75929247661548871, 4.000000000000000000 ) ) ;
#141517 = ORIENTED_EDGE ( 'NONE', *, *, #85912, .T. ) ;
#141518 = STYLED_ITEM ( 'NONE', ( #32633 ), #72264 ) ;
#141519 = VECTOR ( 'NONE', #53895, 1000.000000000000000 ) ;
#141520 = ORIENTED_EDGE ( 'NONE', *, *, #83733, .T. ) ;
#141521 = VECTOR ( 'NONE', #47826, 1000.000000000000000 ) ;
#141522 = EDGE_LOOP ( 'NONE', ( #104717, #16333, #92919, #105274 ) ) ;
#141523 = CARTESIAN_POINT ( 'NONE',  ( 21.29159235450332233, 9.902892378096218942E-16, 0.000000000000000000 ) ) ;
#141524 = DIRECTION ( 'NONE',  ( 1.000000000000000000, 0.000000000000000000, 0.000000000000000000 ) ) ;
#141525 = ORIENTED_EDGE ( 'NONE', *, *, #13037, .T. ) ;
#141526 = VECTOR ( 'NONE', #63301, 999.9999999999998863 ) ;
#141527 = ORIENTED_EDGE ( 'NONE', *, *, #96017, .T. ) ;
#141528 = VERTEX_POINT ( 'NONE', #15517 ) ;
#141529 = CARTESIAN_POINT ( 'NONE',  ( -26.20666063542134339, 21.75929247661549226, 4.998822639870711626 ) ) ;
#141530 = DIRECTION ( 'NONE',  ( -1.000000000000000000, -1.224606353822377258E-16, -0.000000000000000000 ) ) ;
#141531 = CARTESIAN_POINT ( 'NONE',  ( -28.82816939922333432, -5.240707523384228850, 4.000000000000000000 ) ) ;
#141532 = ORIENTED_EDGE ( 'NONE', *, *, #67925, .F. ) ;
#141533 = VECTOR ( 'NONE', #13391, 999.9999999999998863 ) ;
#141534 = CARTESIAN_POINT ( 'NONE',  ( 34.92499999999998295, -21.72500000000000142, 5.000000000000000000 ) ) ;
#141535 = CARTESIAN_POINT ( 'NONE',  ( 30.18398860626900060, 28.73617430169808173, 5.000000000000000000 ) ) ;
#141536 = CARTESIAN_POINT ( 'NONE',  ( 17.42123647476855908, -9.717572351234235426E-16, -7.934999999999990727 ) ) ;
#141537 = EDGE_CURVE ( 'NONE', #11432, #77500, #117006, .T. ) ;
#141538 = CARTESIAN_POINT ( 'NONE',  ( -68.99451991528748351, 28.92564299267986172, 4.000000000000000000 ) ) ;
#141539 = ORIENTED_EDGE ( 'NONE', *, *, #59651, .T. ) ;
#141540 = CARTESIAN_POINT ( 'NONE',  ( 122.2662635252314374, 4.472830434245839371, -4.472830434245839371 ) ) ;
#141541 = AXIS2_PLACEMENT_3D ( 'NONE', #18789, #12021, #56309 ) ;
#141542 = EDGE_CURVE ( 'NONE', #83949, #72597, #116297, .T. ) ;
#141543 = DIRECTION ( 'NONE',  ( 0.7071067811865487940, 0.7071067811865463515, 0.000000000000000000 ) ) ;
#141544 = DIRECTION ( 'NONE',  ( -0.6830127018922180770, -0.6830127018922204085, -0.2588190451025213501 ) ) ;
#141546 = VERTEX_POINT ( 'NONE', #3916 ) ;
#141545 = CARTESIAN_POINT ( 'NONE',  ( -4.190466188707369533, -22.22500000000000142, -6.646463778304954495 ) ) ;
#141547 = DIRECTION ( 'NONE',  ( -0.7071067811865487940, 0.7071067811865463515, -0.000000000000000000 ) ) ;
#141548 = ORIENTED_EDGE ( 'NONE', *, *, #52920, .T. ) ;
#141549 = CARTESIAN_POINT ( 'NONE',  ( -23.24240614354803824, -1.100504885936601784, 4.183743008713593170 ) ) ;
#141550 = FACE_OUTER_BOUND ( 'NONE', #79474, .T. ) ;
#141551 = ADVANCED_FACE ( 'NONE', ( #6066 ), #39475, .F. ) ;
#141552 = ADVANCED_FACE ( 'NONE', ( #103965 ), #61947, .F. ) ;
#141553 = DIRECTION ( 'NONE',  ( 0.7071067811865487940, 0.7071067811865463515, -0.000000000000000000 ) ) ;
#141554 = VERTEX_POINT ( 'NONE', #83710 ) ;
#141555 = AXIS2_PLACEMENT_3D ( 'NONE', #44909, #23062, #32562 ) ;
#141556 = VECTOR ( 'NONE', #110752, 1000.000000000000227 ) ;
#141557 = CIRCLE ( 'NONE', #79091, 5.968999999999998529 ) ;
#141558 = CARTESIAN_POINT ( 'NONE',  ( 34.92499999999998295, -21.72500000000000142, 5.000000000000000000 ) ) ;
#141559 = CARTESIAN_POINT ( 'NONE',  ( -19.92399413215983728, -3.162306507096367625, -35.07835588745236066 ) ) ;
#141560 = EDGE_LOOP ( 'NONE', ( #20816, #98235, #54078, #87483 ) ) ;
#141561 = DIRECTION ( 'NONE',  ( 0.7071067811865486830, -0.7071067811865464625, -0.000000000000000000 ) ) ;
#141562 = VECTOR ( 'NONE', #78135, 1000.000000000000227 ) ;
#141563 = DIRECTION ( 'NONE',  ( 0.3543493200069162685, -0.000000000000000000, -0.9351131265310288487 ) ) ;
#141564 = VERTEX_POINT ( 'NONE', #48193 ) ;
#141565 = CARTESIAN_POINT ( 'NONE',  ( 4.958333333333333925, -3.047499999999997211, -5.278424836066143655 ) ) ;
#141566 = EDGE_CURVE ( 'NONE', #95511, #5654, #135912, .T. ) ;
#141567 = CARTESIAN_POINT ( 'NONE',  ( 20.50183651486031522, -17.24070752338409918, 8.407044977365179861 ) ) ;
#141568 = ORIENTED_EDGE ( 'NONE', *, *, #25026, .T. ) ;
#141569 = AXIS2_PLACEMENT_3D ( 'NONE', #39979, #4385, #28366 ) ;
#141570 = ADVANCED_FACE ( 'NONE', ( #104705 ), #80839, .F. ) ;
#141571 = ORIENTED_EDGE ( 'NONE', *, *, #115107, .T. ) ;
#141572 = DIRECTION ( 'NONE',  ( 0.7071067811865487940, 0.7071067811865463515, -0.000000000000000000 ) ) ;
#141573 = FACE_OUTER_BOUND ( 'NONE', #72501, .T. ) ;
#141574 = EDGE_CURVE ( 'NONE', #37037, #16100, #26441, .T. ) ;
#141575 = CARTESIAN_POINT ( 'NONE',  ( 11.35373647476855119, -5.808823158059035485, -5.808823158059033709 ) ) ;
#141576 =( NAMED_UNIT ( * ) SI_UNIT ( $, .STERADIAN. ) SOLID_ANGLE_UNIT ( ) );
#141577 = DIRECTION ( 'NONE',  ( -0.7071067811865486830, 0.7071067811865464625, 0.000000000000000000 ) ) ;
#141578 = CARTESIAN_POINT ( 'NONE',  ( 19.10813147593277250, 4.202752102959690472E-16, 0.000000000000000000 ) ) ;
#141579 = ORIENTED_EDGE ( 'NONE', *, *, #124012, .T. ) ;
#141580 = LINE ( 'NONE', #120484, #58328 ) ;
#141581 = CARTESIAN_POINT ( 'NONE',  ( -12.70710678118645376, 20.25929247661551713, 5.000000000000000000 ) ) ;
#141582 = ADVANCED_FACE ( 'NONE', ( #127164 ), #61264, .T. ) ;
#141583 = VECTOR ( 'NONE', #50121, 1000.000000000000227 ) ;
#141584 = CARTESIAN_POINT ( 'NONE',  ( 126.5615712523421053, -6.570126589092502911, -2.091773665023263451 ) ) ;
#141585 = CARTESIAN_POINT ( 'NONE',  ( 36.22459685856478728, -1.637169565754161171, 6.109999999999998543 ) ) ;
#141586 = CARTESIAN_POINT ( 'NONE',  ( 14.99451991528749595, 28.92564299267948513, 4.000000000000000000 ) ) ;
#141587 = ORIENTED_EDGE ( 'NONE', *, *, #132508, .T. ) ;
#141588 = LINE ( 'NONE', #72811, #65014 ) ;
#141589 = ORIENTED_EDGE ( 'NONE', *, *, #58693, .T. ) ;
#141590 = ORIENTED_EDGE ( 'NONE', *, *, #81334, .F. ) ;
#141591 = EDGE_CURVE ( 'NONE', #16744, #48450, #137355, .T. ) ;
#141592 = LINE ( 'NONE', #146, #47977 ) ;
#141593 = DIRECTION ( 'NONE',  ( 0.6830127018922181881, 0.6830127018922202975, -0.2588190451025214056 ) ) ;
#141594 = ORIENTED_EDGE ( 'NONE', *, *, #115932, .T. ) ;
#141595 = LINE ( 'NONE', #130736, #122606 ) ;
#141596 = FACE_OUTER_BOUND ( 'NONE', #54017, .T. ) ;
#141597 = CARTESIAN_POINT ( 'NONE',  ( -51.29974487139158867, -27.71228299555242103, 4.000000000000000000 ) ) ;
#141598 = CARTESIAN_POINT ( 'NONE',  ( 13.18000000000000149, 2.055000000000001492, 0.000000000000000000 ) ) ;
#141599 = DIRECTION ( 'NONE',  ( 0.7071067811865487940, 0.7071067811865463515, 0.000000000000000000 ) ) ;
#141600 = ORIENTED_EDGE ( 'NONE', *, *, #112289, .F. ) ;
#141601 = ADVANCED_FACE ( 'NONE', ( #38046 ), #138784, .T. ) ;
#141602 = DIRECTION ( 'NONE',  ( -0.000000000000000000, 0.000000000000000000, 1.000000000000000000 ) ) ;
#141603 = CARTESIAN_POINT ( 'NONE',  ( 2.000000000000000000, -2.375000000000000000, 4.319999999999998508 ) ) ;
#141604 = ADVANCED_FACE ( 'NONE', ( #27141 ), #49653, .F. ) ;
#141606 = VECTOR ( 'NONE', #27133, 999.9999999999998863 ) ;
#141605 = CARTESIAN_POINT ( 'NONE',  ( 60.29974487139158867, -27.71228299555248142, 4.000000000000000000 ) ) ;
#141607 = CARTESIAN_POINT ( 'NONE',  ( -25.39999999999996305, 0.000000000000000000, 2.500000000000000000 ) ) ;
#141608 = PLANE ( 'NONE',  #137041 ) ;
#141609 = DIRECTION ( 'NONE',  ( -0.7071067811865487940, 0.7071067811865463515, 0.000000000000000000 ) ) ;
#141610 = CARTESIAN_POINT ( 'NONE',  ( 57.82919371712954870, -3.975000000000001865, 6.884901960086284411 ) ) ;
#141611 = ADVANCED_FACE ( 'NONE', ( #40205 ), #128608, .F. ) ;
#141612 = DIRECTION ( 'NONE',  ( -0.000000000000000000, 0.000000000000000000, 1.000000000000000000 ) ) ;
#141613 = VERTEX_POINT ( 'NONE', #119834 ) ;
#141614 = VERTEX_POINT ( 'NONE', #52455 ) ;
#141615 = CARTESIAN_POINT ( 'NONE',  ( 57.87499999999999289, 7.950000000000000178, 1.460391307983218535E-15 ) ) ;
#141616 = CARTESIAN_POINT ( 'NONE',  ( 9.489213562373095101, -27.52281430457062328, 5.000000000000000000 ) ) ;
#141617 = LINE ( 'NONE', #98110, #25347 ) ;
#141618 = LINE ( 'NONE', #77098, #53047 ) ;
#141619 = ORIENTED_EDGE ( 'NONE', *, *, #118743, .T. ) ;
#141620 = VECTOR ( 'NONE', #73793, 1000.000000000000000 ) ;
#141621 = AXIS2_PLACEMENT_3D ( 'NONE', #140625, #137805, #84834 ) ;
#141622 = DIRECTION ( 'NONE',  ( 0.7071067811865486830, -0.7071067811865464625, -0.000000000000000000 ) ) ;
#141623 = VECTOR ( 'NONE', #105309, 999.9999999999998863 ) ;
#141624 = CARTESIAN_POINT ( 'NONE',  ( 48.12543019189810423, 5.291415217122919401, 3.055000000000002824 ) ) ;
#141625 = ORIENTED_EDGE ( 'NONE', *, *, #104869, .F. ) ;
#141626 = CARTESIAN_POINT ( 'NONE',  ( 5.999999999999960032, -11.35517001088072142, -1.126524801160094347 ) ) ;
#141627 = VERTEX_POINT ( 'NONE', #108233 ) ;
#141629 = EDGE_LOOP ( 'NONE', ( #71321, #60823, #1575 ) ) ;
#141628 = VECTOR ( 'NONE', #62958, 1000.000000000000000 ) ;
#141630 = AXIS2_PLACEMENT_3D ( 'NONE', #129633, #41940, #75290 ) ;
#141631 = VECTOR ( 'NONE', #125179, 1000.000000000000000 ) ;
#141632 = VECTOR ( 'NONE', #38232, 1000.000000000000114 ) ;
#141633 = CARTESIAN_POINT ( 'NONE',  ( 5.510786437626906675, -27.52281430457051314, 5.000000000000000000 ) ) ;
#141635 = LINE ( 'NONE', #74968, #80118 ) ;
#141634 = VECTOR ( 'NONE', #126653, 1000.000000000000000 ) ;
#141636 = DIRECTION ( 'NONE',  ( -0.000000000000000000, -0.3543493200069152693, 0.9351131265310292928 ) ) ;
#141637 = DIRECTION ( 'NONE',  ( -0.000000000000000000, 0.000000000000000000, 1.000000000000000000 ) ) ;
#141638 = EDGE_LOOP ( 'NONE', ( #59792, #80016, #94522, #75108, #140386 ) ) ;
#141639 = DIRECTION ( 'NONE',  ( 0.6830127018922181881, 0.6830127018922202975, -0.2588190451025214056 ) ) ;
#141641 = ORIENTED_EDGE ( 'NONE', *, *, #53404, .T. ) ;
#141640 = FACE_OUTER_BOUND ( 'NONE', #55193, .T. ) ;
#141642 = CARTESIAN_POINT ( 'NONE',  ( 81.52126352523141861, -4.472830434245838482, -4.472830434245840259 ) ) ;
#141643 = CARTESIAN_POINT ( 'NONE',  ( 15.02083333333333393, -6.094999999999989981, -1.633150327867689322 ) ) ;
#141644 = CARTESIAN_POINT ( 'NONE',  ( 14.51078643762690490, -27.52281430457045275, 5.000000000000000000 ) ) ;
#141645 = LINE ( 'NONE', #85812, #42261 ) ;
#141646 = COLOUR_RGB ( '', 0.09019608, 0.27058824, 0.51372549) ;
#141647 = CARTESIAN_POINT ( 'NONE',  ( -4.446650576632151797, 2.259292476615694323, 14.86850063742355488 ) ) ;
#141648 = PLANE ( 'NONE',  #92442 ) ;
#141649 = EDGE_LOOP ( 'NONE', ( #131341, #76409, #108837, #109665 ) ) ;
#141650 = FILL_AREA_STYLE_COLOUR ( '', #22178 ) ;
#141651 = CARTESIAN_POINT ( 'NONE',  ( 69.32876352523145158, 0.000000000000000000, -6.109999999999998543 ) ) ;
#141652 = CARTESIAN_POINT ( 'NONE',  ( -21.00548008471250938, 28.92564299267923644, 4.000000000000000000 ) ) ;
#141653 = DIRECTION ( 'NONE',  ( -0.7071067811865486830, -0.7071067811865464625, 0.000000000000000000 ) ) ;
#141654 = DIRECTION ( 'NONE',  ( -0.7071067811865487940, 0.7071067811865463515, -0.000000000000000000 ) ) ;
#141655 = VERTEX_POINT ( 'NONE', #118428 ) ;
#141656 = EDGE_LOOP ( 'NONE', ( #90298, #64281, #142348, #5246 ) ) ;
#141657 = CARTESIAN_POINT ( 'NONE',  ( -18.85181644961843972, 17.25929247661554555, 8.802941693769158249 ) ) ;
#141658 = DIRECTION ( 'NONE',  ( 0.000000000000000000, 0.000000000000000000, 1.000000000000000000 ) ) ;
#141659 = ORIENTED_EDGE ( 'NONE', *, *, #39277, .F. ) ;
#141660 = VECTOR ( 'NONE', #37561, 1000.000000000000000 ) ;
#141661 = ORIENTED_EDGE ( 'NONE', *, *, #100711, .F. ) ;
#141662 = VECTOR ( 'NONE', #85830, 1000.000000000000000 ) ;
#141663 = CARTESIAN_POINT ( 'NONE',  ( 3.000000000000000000, -7.600000000000055600, -31.92499999999998650 ) ) ;
#141664 = EDGE_LOOP ( 'NONE', ( #96466, #20925, #21266, #86943 ) ) ;
#141665 = VECTOR ( 'NONE', #43463, 999.9999999999998863 ) ;
#141666 = LINE ( 'NONE', #216, #111701 ) ;
#141667 = DIRECTION ( 'NONE',  ( -0.6830127018922181881, 0.6830127018922202975, -0.2588190451025214056 ) ) ;
#141668 = EDGE_CURVE ( 'NONE', #80500, #33114, #131469, .T. ) ;
#141669 = FACE_BOUND ( 'NONE', #56563, .T. ) ;
#141670 = DIRECTION ( 'NONE',  ( -0.3543493200069162685, -0.000000000000000000, -0.9351131265310288487 ) ) ;
#141671 = CARTESIAN_POINT ( 'NONE',  ( -17.81601139373099940, 28.73617430169775133, 5.000000000000000000 ) ) ;
#141672 = EDGE_CURVE ( 'NONE', #68801, #69641, #95963, .T. ) ;
#141673 = FACE_OUTER_BOUND ( 'NONE', #125608, .T. ) ;
#141675 = ORIENTED_EDGE ( 'NONE', *, *, #30775, .F. ) ;
#141674 = CARTESIAN_POINT ( 'NONE',  ( -12.20000000000000284, -34.64999999999999147, 17.49210858042621908 ) ) ;
#141676 = AXIS2_PLACEMENT_3D ( 'NONE', #43093, #85857, #119886 ) ;
#141677 = CARTESIAN_POINT ( 'NONE',  ( 6.183988606268994381, 28.73617430169791476, 5.000000000000000000 ) ) ;
#141678 = ORIENTED_EDGE ( 'NONE', *, *, #4143, .F. ) ;
#141679 = ORIENTED_EDGE ( 'NONE', *, *, #108266, .T. ) ;
#141680 = CARTESIAN_POINT ( 'NONE',  ( 85.07876352523143737, -7.482591942790325086E-16, 6.109999999999998543 ) ) ;
#141681 = VERTEX_POINT ( 'NONE', #64787 ) ;
#141682 = DIRECTION ( 'NONE',  ( -0.7071067811865486830, 0.7071067811865463515, 0.000000000000000000 ) ) ;
#141683 = ADVANCED_FACE ( 'NONE', ( #129300 ), #63388, .T. ) ;
#141684 = DIRECTION ( 'NONE',  ( -0.6830127018922180770, -0.6830127018922204085, -0.2588190451025213501 ) ) ;
#141685 = AXIS2_PLACEMENT_3D ( 'NONE', #20902, #44873, #54995 ) ;
#141686 = VERTEX_POINT ( 'NONE', #9662 ) ;
#141687 = CARTESIAN_POINT ( 'NONE',  ( -14.81601139373099585, 28.73617430169776910, 5.000000000000000000 ) ) ;
#141688 = PRESENTATION_LAYER_ASSIGNMENT (  '', '', ( #2786 ) ) ;
#141689 = EDGE_CURVE ( 'NONE', #59344, #57055, #20527, .T. ) ;
#141690 = FACE_OUTER_BOUND ( 'NONE', #49744, .T. ) ;
#141691 = CARTESIAN_POINT ( 'NONE',  ( -4.499999999999962697, -7.420205493532904484, -2.617629953481263261 ) ) ;
#141692 = LINE ( 'NONE', #42395, #131160 ) ;
#141693 = FACE_OUTER_BOUND ( 'NONE', #139814, .T. ) ;
#141694 = CARTESIAN_POINT ( 'NONE',  ( 20.12514619309222041, -14.24070752338413470, 9.401115078912612333 ) ) ;
#141695 = DIRECTION ( 'NONE',  ( -0.7071067811865487940, 0.7071067811865463515, 0.000000000000000000 ) ) ;
#141696 = PLANE ( 'NONE',  #25391 ) ;
#141697 = ORIENTED_EDGE ( 'NONE', *, *, #25696, .T. ) ;
#141698 = VECTOR ( 'NONE', #8828, 1000.000000000000227 ) ;
#141699 = EDGE_CURVE ( 'NONE', #121031, #55582, #86545, .T. ) ;
#141700 = CARTESIAN_POINT ( 'NONE',  ( -19.82816939922339117, -5.240707523384228850, 4.000000000000000000 ) ) ;
#141701 = ORIENTED_EDGE ( 'NONE', *, *, #120189, .F. ) ;
#141702 = LINE ( 'NONE', #1675, #102828 ) ;
#141703 = DIRECTION ( 'NONE',  ( -0.6830127018922180770, -0.6830127018922204085, -0.2588190451025213501 ) ) ;
#141704 = VERTEX_POINT ( 'NONE', #41584 ) ;
#141705 = ORIENTED_EDGE ( 'NONE', *, *, #87527, .T. ) ;
#141706 = ORIENTED_EDGE ( 'NONE', *, *, #72711, .T. ) ;
#141707 = CARTESIAN_POINT ( 'NONE',  ( 31.20876352523144348, -7.482591942790329030E-16, 6.110000000000001208 ) ) ;
#141708 = VECTOR ( 'NONE', #113585, 1000.000000000000227 ) ;
#141709 = ORIENTED_EDGE ( 'NONE', *, *, #92270, .T. ) ;
#141710 = CARTESIAN_POINT ( 'NONE',  ( -4.499999999999976019, 22.22500000000000142, 4.362957392718799454 ) ) ;
#141711 = CARTESIAN_POINT ( 'NONE',  ( -14.29289321881335262, -15.74070752338412760, 5.000000000000000000 ) ) ;
#141712 = CARTESIAN_POINT ( 'NONE',  ( 29.35830628287044064, -1.633150327867689988, 6.094999999999989981 ) ) ;
#141713 = CARTESIAN_POINT ( 'NONE',  ( 6.851678761571759146, 12.66444798601647470, -25.17854338220229593 ) ) ;
#141714 = ORIENTED_EDGE ( 'NONE', *, *, #71373, .F. ) ;
#141715 = CARTESIAN_POINT ( 'NONE',  ( 10.15640092694706453, 3.821174125832445049E-16, 0.000000000000000000 ) ) ;
#141716 = EDGE_CURVE ( 'NONE', #137834, #74547, #18376, .T. ) ;
#141717 = ORIENTED_EDGE ( 'NONE', *, *, #134166, .F. ) ;
#141718 = CARTESIAN_POINT ( 'NONE',  ( -3.489213562373097322, -27.52281430457057709, 5.000000000000000000 ) ) ;
#141719 = CARTESIAN_POINT ( 'NONE',  ( -34.92500000000001137, -16.29806943317882073, 4.500000000000000888 ) ) ;
#141720 = AXIS2_PLACEMENT_3D ( 'NONE', #29932, #106777, #53869 ) ;
#141721 = AXIS2_PLACEMENT_3D ( 'NONE', #43140, #300, #100372 ) ;
#141723 = ORIENTED_EDGE ( 'NONE', *, *, #36295, .F. ) ;
#141722 = LINE ( 'NONE', #54717, #56419 ) ;
#141724 = VECTOR ( 'NONE', #31114, 1000.000000000000000 ) ;
#141725 = VERTEX_POINT ( 'NONE', #85803 ) ;
#141726 = CARTESIAN_POINT ( 'NONE',  ( -23.20710678118637915, -20.24070752338406720, 5.000000000000000000 ) ) ;
#141727 = LINE ( 'NONE', #32240, #107038 ) ;
#141728 = EDGE_CURVE ( 'NONE', #94372, #131124, #107554, .T. ) ;
#141730 = EDGE_CURVE ( 'NONE', #102027, #67530, #139521, .T. ) ;
#141729 = AXIS2_PLACEMENT_3D ( 'NONE', #43292, #10626, #21532 ) ;
#141731 = FACE_OUTER_BOUND ( 'NONE', #88772, .T. ) ;
#141733 = ORIENTED_EDGE ( 'NONE', *, *, #66273, .T. ) ;
#141732 = CIRCLE ( 'NONE', #67663, 2.500000000000000444 ) ;
#141734 = CARTESIAN_POINT ( 'NONE',  ( -3.489213562373097322, -27.52281430457057709, 5.000000000000000000 ) ) ;
#141735 = ORIENTED_EDGE ( 'NONE', *, *, #39157, .F. ) ;
#141736 = ORIENTED_EDGE ( 'NONE', *, *, #99361, .F. ) ;
#141737 = VERTEX_POINT ( 'NONE', #119143 ) ;
#141738 = DIRECTION ( 'NONE',  ( -0.6830127018922181881, 0.6830127018922202975, -0.2588190451025214056 ) ) ;
#141739 = VECTOR ( 'NONE', #94685, 1000.000000000000000 ) ;
#141740 = AXIS2_PLACEMENT_3D ( 'NONE', #131440, #143020, #79242 ) ;
#141741 =( GEOMETRIC_REPRESENTATION_CONTEXT ( 3 ) GLOBAL_UNCERTAINTY_ASSIGNED_CONTEXT ( ( #133202 ) ) GLOBAL_UNIT_ASSIGNED_CONTEXT ( ( #108989, #108257, #64089 ) ) REPRESENTATION_CONTEXT ( 'NONE', 'WORKASPACE' ) );
#141742 = DIRECTION ( 'NONE',  ( -0.7071067811865486830, 0.7071067811865464625, 0.000000000000000000 ) ) ;
#141743 = EDGE_CURVE ( 'NONE', #114577, #107625, #51054, .T. ) ;
#141744 = LINE ( 'NONE', #77902, #28453 ) ;
#141745 = CARTESIAN_POINT ( 'NONE',  ( 66.48921356237309510, -27.52281430457101763, 5.000000000000000000 ) ) ;
#141746 = DIRECTION ( 'NONE',  ( 0.000000000000000000, -1.301042606982605074E-16, 1.000000000000000000 ) ) ;
#141747 = EDGE_CURVE ( 'NONE', #98173, #8470, #7517, .T. ) ;
#141748 = CARTESIAN_POINT ( 'NONE',  ( -31.49999999999977263, 13.08746187583910370, 4.000000000000000000 ) ) ;
#141749 = EDGE_LOOP ( 'NONE', ( #39949, #38298, #82358, #112614 ) ) ;
#141750 = ADVANCED_FACE ( 'NONE', ( #76375 ), #42334, .F. ) ;
#141751 = DIRECTION ( 'NONE',  ( 0.7071067811865486830, -0.7071067811865464625, -0.000000000000000000 ) ) ;
#141752 = ORIENTED_EDGE ( 'NONE', *, *, #131029, .F. ) ;
#141753 = DIRECTION ( 'NONE',  ( 0.3543493200069162685, -0.000000000000000000, -0.9351131265310288487 ) ) ;
#141754 = DIRECTION ( 'NONE',  ( -1.000000000000000000, -1.224606353822377258E-16, -0.000000000000000000 ) ) ;
#141755 = ORIENTED_EDGE ( 'NONE', *, *, #113630, .F. ) ;
#141756 = CARTESIAN_POINT ( 'NONE',  ( 0.000000000000000000, 0.000000000000000000, 5.000000000000000000 ) ) ;
#141757 = EDGE_CURVE ( 'NONE', #17670, #91794, #130774, .T. ) ;
#141758 = FACE_OUTER_BOUND ( 'NONE', #52165, .T. ) ;
#141759 = ORIENTED_EDGE ( 'NONE', *, *, #105818, .T. ) ;
#141760 = ORIENTED_EDGE ( 'NONE', *, *, #98301, .T. ) ;
#141761 = CARTESIAN_POINT ( 'NONE',  ( 55.56056557994607914, -52.00875322212550600, 39.86617647058822911 ) ) ;
#141762 = CARTESIAN_POINT ( 'NONE',  ( -29.21837311707484730, 21.74787736706806740, 4.999607392498049308 ) ) ;
#141763 = LINE ( 'NONE', #51898, #30722 ) ;
#141764 = DIRECTION ( 'NONE',  ( -1.000000000000000000, -1.224606353822377258E-16, -0.000000000000000000 ) ) ;
#141765 = EDGE_CURVE ( 'NONE', #14410, #45511, #106099, .T. ) ;
#141766 = LINE ( 'NONE', #55464, #106057 ) ;
#141767 = CARTESIAN_POINT ( 'NONE',  ( 65.82876352523145158, 0.000000000000000000, -6.109999999999999432 ) ) ;
#141768 = VECTOR ( 'NONE', #58840, 1000.000000000000000 ) ;
#141769 = DIRECTION ( 'NONE',  ( -0.3543493200069162685, -0.000000000000000000, -0.9351131265310288487 ) ) ;
#141770 = AXIS2_PLACEMENT_3D ( 'NONE', #50203, #138635, #105962 ) ;
#141771 = CARTESIAN_POINT ( 'NONE',  ( 45.48921356237309510, -27.52281430457087197, 5.000000000000000000 ) ) ;
#141772 = CARTESIAN_POINT ( 'NONE',  ( -30.29974487139158867, -27.71228299555227537, 4.000000000000000000 ) ) ;
#141773 = CARTESIAN_POINT ( 'NONE',  ( 12.48921356237309155, -27.52281430457064104, 5.000000000000000000 ) ) ;
#141774 = ORIENTED_EDGE ( 'NONE', *, *, #427, .T. ) ;
#141775 = LINE ( 'NONE', #65673, #72035 ) ;
#141776 = ORIENTED_EDGE ( 'NONE', *, *, #24175, .F. ) ;
#141777 = CARTESIAN_POINT ( 'NONE',  ( 128.5894344200537489, -52.00875322212550600, 39.86617647058822911 ) ) ;
#141778 = VECTOR ( 'NONE', #73343, 1000.000000000000000 ) ;
#141779 = VERTEX_POINT ( 'NONE', #43041 ) ;
#141780 = DIRECTION ( 'NONE',  ( -0.7071067811865487940, 0.7071067811865463515, 0.000000000000000000 ) ) ;
#141782 = VERTEX_POINT ( 'NONE', #29282 ) ;
#141781 = DIRECTION ( 'NONE',  ( 0.000000000000000000, 1.000000000000000000, 0.000000000000000000 ) ) ;
#141783 = CARTESIAN_POINT ( 'NONE',  ( 106.8750000000000000, 7.950000000000000178, 1.460391307983218535E-15 ) ) ;
#141784 = LINE ( 'NONE', #109843, #18525 ) ;
#141785 = CARTESIAN_POINT ( 'NONE',  ( 17.99999999999988276, 11.58746187583911968, 4.000000000000000000 ) ) ;
#141786 = ORIENTED_EDGE ( 'NONE', *, *, #47022, .T. ) ;
#141787 = EDGE_LOOP ( 'NONE', ( #39843, #3483, #67732 ) ) ;
#141788 = DIRECTION ( 'NONE',  ( 0.7071067811865487940, -0.7071067811865463515, 0.000000000000000000 ) ) ;
#141789 = CARTESIAN_POINT ( 'NONE',  ( -19.93618820137057668, -3.270000000000008011, -40.00000000002046363 ) ) ;
#141790 = VECTOR ( 'NONE', #44359, 1000.000000000000000 ) ;
#141791 = DIRECTION ( 'NONE',  ( 0.000000000000000000, -1.000000000000000000, 0.000000000000000000 ) ) ;
#141793 = EDGE_CURVE ( 'NONE', #143369, #59118, #73524, .T. ) ;
#141792 = CARTESIAN_POINT ( 'NONE',  ( 30.85005128541006059, -8.240707523384196875, 17.25253755692246571 ) ) ;
#141794 = CARTESIAN_POINT ( 'NONE',  ( 83.93336038379621300, 2.130196079827431532, -7.949999999999997513 ) ) ;
#141796 = EDGE_CURVE ( 'NONE', #62769, #119974, #33605, .T. ) ;
#141795 = LINE ( 'NONE', #51926, #48607 ) ;
#141797 = CARTESIAN_POINT ( 'NONE',  ( 30.48921356237309510, -27.52281430457076894, 5.000000000000000000 ) ) ;
#141798 = ORIENTED_EDGE ( 'NONE', *, *, #48064, .T. ) ;
#141799 = ADVANCED_FACE ( 'NONE', ( #34291 ), #54628, .F. ) ;
#141800 = CARTESIAN_POINT ( 'NONE',  ( 30.18398860626900060, 28.73617430169808173, 5.000000000000000000 ) ) ;
#141801 = PLANE ( 'NONE',  #27616 ) ;
#141803 = AXIS2_PLACEMENT_3D ( 'NONE', #34487, #69270, #68567 ) ;
#141802 = CARTESIAN_POINT ( 'NONE',  ( 13.75179860200718984, 5.925774409307370760, 4.669108085256723939 ) ) ;
#141804 = VECTOR ( 'NONE', #63542, 999.9999999999998863 ) ;
#141805 = VERTEX_POINT ( 'NONE', #101679 ) ;
#141806 = DIRECTION ( 'NONE',  ( 0.7071067811865487940, 0.7071067811865463515, 0.000000000000000000 ) ) ;
#141807 = VERTEX_POINT ( 'NONE', #66220 ) ;
#141808 = CARTESIAN_POINT ( 'NONE',  ( 73.93793019189809002, -6.110000000000001208, 1.637169565754158951 ) ) ;
#141809 = FILL_AREA_STYLE ('',( #97557 ) ) ;
#141811 = CIRCLE ( 'NONE', #25995, 2.500000000000000444 ) ;
#141810 = DIRECTION ( 'NONE',  ( 0.6830127018922181881, 0.6830127018922202975, -0.2588190451025214056 ) ) ;
#141812 = EDGE_LOOP ( 'NONE', ( #112673, #39009, #79160, #7682 ) ) ;
#141813 = VECTOR ( 'NONE', #97012, 1000.000000000000000 ) ;
#141814 = PLANE ( 'NONE',  #7103 ) ;
#141815 = PLANE ( 'NONE',  #7165 ) ;
#141816 = DIRECTION ( 'NONE',  ( -0.7071067811865487940, 0.7071067811865463515, -0.000000000000000000 ) ) ;
#141817 = DIRECTION ( 'NONE',  ( -0.5735764363510499342, -0.8191520442889891340, 0.000000000000000000 ) ) ;
#141819 = ORIENTED_EDGE ( 'NONE', *, *, #124443, .F. ) ;
#141818 = DIRECTION ( 'NONE',  ( -0.6830127018922181881, 0.6830127018922202975, -0.2588190451025214056 ) ) ;
#141820 = CARTESIAN_POINT ( 'NONE',  ( -30.18398860626900060, 28.73617430169808173, 5.000000000000000000 ) ) ;
#141821 = DIRECTION ( 'NONE',  ( -1.000000000000000000, -1.224606353822377258E-16, -0.000000000000000000 ) ) ;
#141822 = VECTOR ( 'NONE', #15330, 999.9999999999998863 ) ;
#141823 = CARTESIAN_POINT ( 'NONE',  ( 77.56250000000000000, -5.819803920172573086, -5.819803920172573974 ) ) ;
#141824 = FILL_AREA_STYLE ('',( #97571 ) ) ;
#141825 = ORIENTED_EDGE ( 'NONE', *, *, #92398, .F. ) ;
#141826 = ORIENTED_EDGE ( 'NONE', *, *, #77626, .F. ) ;
#141827 = CARTESIAN_POINT ( 'NONE',  ( 63.29209685856476852, -5.291415217122921177, 3.054999999999999272 ) ) ;
#141828 = EDGE_LOOP ( 'NONE', ( #88946, #183, #28883, #124545 ) ) ;
#141829 = DIRECTION ( 'NONE',  ( -0.000000000000000000, -0.3543493200069152693, 0.9351131265310292928 ) ) ;
#141830 = LINE ( 'NONE', #97578, #85081 ) ;
#141831 = EDGE_CURVE ( 'NONE', #106541, #2749, #35762, .T. ) ;
#141832 = CYLINDRICAL_SURFACE ( 'NONE', #8622, 2.500000000000000444 ) ;
#141833 = CARTESIAN_POINT ( 'NONE',  ( 22.49999999999985079, -8.947814304570739452, 5.000000000000000000 ) ) ;
#141834 = ORIENTED_EDGE ( 'NONE', *, *, #41560, .T. ) ;
#141835 = VECTOR ( 'NONE', #118738, 1000.000000000000000 ) ;
#141836 = AXIS2_PLACEMENT_3D ( 'NONE', #69176, #137996, #49585 ) ;
#141837 = VECTOR ( 'NONE', #100992, 1000.000000000000000 ) ;
#141838 = LINE ( 'NONE', #42534, #74633 ) ;
#141839 =( NAMED_UNIT ( * ) PLANE_ANGLE_UNIT ( ) SI_UNIT ( $, .RADIAN. ) );
#141840 = VECTOR ( 'NONE', #23666, 1000.000000000000000 ) ;
#141841 = VERTEX_POINT ( 'NONE', #77115 ) ;
#141842 = CARTESIAN_POINT ( 'NONE',  ( -38.99451991528749062, 28.92564299267965211, 4.000000000000000000 ) ) ;
#141844 = LINE ( 'NONE', #131672, #8413 ) ;
#141843 = VECTOR ( 'NONE', #5185, 1000.000000000000000 ) ;
#141845 = PLANE ( 'NONE',  #123399 ) ;
#141846 = CIRCLE ( 'NONE', #113993, 2.500000000000000888 ) ;
#141847 = PRESENTATION_LAYER_ASSIGNMENT (  '', '', ( #7580 ) ) ;
#141848 = ORIENTED_EDGE ( 'NONE', *, *, #30080, .T. ) ;
#141849 = VERTEX_POINT ( 'NONE', #134331 ) ;
#141850 = EDGE_CURVE ( 'NONE', #138592, #60071, #78515, .T. ) ;
#141851 = EDGE_CURVE ( 'NONE', #62501, #130662, #111104, .T. ) ;
#141852 = EDGE_CURVE ( 'NONE', #103011, #61774, #99518, .T. ) ;
#141853 = DIRECTION ( 'NONE',  ( 0.6830127018922180770, -0.6830127018922204085, -0.2588190451025213501 ) ) ;
#141854 = CARTESIAN_POINT ( 'NONE',  ( 181.1499999999997783, -47.87246431468552998, 37.20487561447688307 ) ) ;
#141855 = CARTESIAN_POINT ( 'NONE',  ( 25.49999999999982236, 22.01701374228157349, 2.453858888625571666 ) ) ;
#141856 = PLANE ( 'NONE',  #133978 ) ;
#141857 = DIRECTION ( 'NONE',  ( -0.7071067811865486830, -0.7071067811865464625, 0.000000000000000000 ) ) ;
#141858 = EDGE_CURVE ( 'NONE', #114427, #54563, #100964, .T. ) ;
#141859 = EDGE_CURVE ( 'NONE', #122401, #85531, #111392, .T. ) ;
#141860 = CARTESIAN_POINT ( 'NONE',  ( 0.02904021785397910282, -0.6000000000000001998, 3.399959840769902097 ) ) ;
#141861 = ORIENTED_EDGE ( 'NONE', *, *, #136469, .T. ) ;
#141862 = AXIS2_PLACEMENT_3D ( 'NONE', #64192, #43160, #84529 ) ;
#141863 = ORIENTED_EDGE ( 'NONE', *, *, #95752, .T. ) ;
#141864 = CARTESIAN_POINT ( 'NONE',  ( 112.7870968585647802, 3.054999999999997495, 5.291415217122919401 ) ) ;
#141865 = EDGE_LOOP ( 'NONE', ( #33432, #19854, #34442, #1915 ) ) ;
#141866 = ADVANCED_FACE ( 'NONE', ( #46652 ), #132195, .T. ) ;
#141867 = EDGE_LOOP ( 'NONE', ( #89032, #111973, #15063, #87540, #16715, #113849 ) ) ;
#141868 = CARTESIAN_POINT ( 'NONE',  ( 183.7102003651226596, -49.08473565290510265, 39.91868829876759861 ) ) ;
#141869 = VECTOR ( 'NONE', #53626, 1000.000000000000000 ) ;
#141870 = FACE_OUTER_BOUND ( 'NONE', #31611, .T. ) ;
#141871 = EDGE_CURVE ( 'NONE', #57727, #55777, #923, .T. ) ;
#141872 = LINE ( 'NONE', #131691, #54151 ) ;
#141873 = ORIENTED_EDGE ( 'NONE', *, *, #80983, .T. ) ;
#141874 = PLANE ( 'NONE',  #115398 ) ;
#141875 = LINE ( 'NONE', #73730, #95756 ) ;
#141876 = AXIS2_PLACEMENT_3D ( 'NONE', #118532, #107651, #8311 ) ;
#141878 = CARTESIAN_POINT ( 'NONE',  ( 57.97502705046289151, -5.819803920172573086, 5.819803920172573086 ) ) ;
#141877 = DIRECTION ( 'NONE',  ( 0.7071067811865487940, 0.7071067811865463515, 0.000000000000000000 ) ) ;
#141879 = CARTESIAN_POINT ( 'NONE',  ( 5.848407645496676466, -3.851859888774471706E-31, 2.500000000000001332 ) ) ;
#141880 = VECTOR ( 'NONE', #139519, 999.9999999999998863 ) ;
#141881 = PRESENTATION_LAYER_ASSIGNMENT (  '', '', ( #93215 ) ) ;
#141882 = EDGE_CURVE ( 'NONE', #23510, #17946, #2337, .T. ) ;
#141883 = CARTESIAN_POINT ( 'NONE',  ( 24.48921356237309510, -27.52281430457072631, 5.000000000000000000 ) ) ;
#141884 = ORIENTED_EDGE ( 'NONE', *, *, #9594, .F. ) ;
#141885 = FACE_OUTER_BOUND ( 'NONE', #129582, .T. ) ;
#141886 = CARTESIAN_POINT ( 'NONE',  ( 20.99999999999984723, -16.44781430457065241, 5.000000000000000000 ) ) ;
#141887 = ORIENTED_EDGE ( 'NONE', *, *, #8810, .F. ) ;
#141888 = DIRECTION ( 'NONE',  ( 0.7071067811865487940, -0.7071067811865463515, 0.000000000000000000 ) ) ;
#141889 = VERTEX_POINT ( 'NONE', #112564 ) ;
#141890 = ORIENTED_EDGE ( 'NONE', *, *, #26823, .T. ) ;
#141891 = VERTEX_POINT ( 'NONE', #87954 ) ;
#141892 = CARTESIAN_POINT ( 'NONE',  ( 59.93793019189810423, -6.110000000000001208, 1.637169565754158951 ) ) ;
#141893 = ADVANCED_FACE ( 'NONE', ( #132926 ), #45206, .T. ) ;
#141894 = VERTEX_POINT ( 'NONE', #138614 ) ;
#141895 = VERTEX_POINT ( 'NONE', #50178 ) ;
#141896 = CARTESIAN_POINT ( 'NONE',  ( -36.18398860626899705, 28.73617430169812437, 5.000000000000000000 ) ) ;
#141897 = PLANE ( 'NONE',  #93654 ) ;
#141898 = CARTESIAN_POINT ( 'NONE',  ( 103.2504301918981184, 3.055000000000002824, -5.291415217122919401 ) ) ;
#141899 = CARTESIAN_POINT ( 'NONE',  ( -8.999999999999934275, -6.412538124160692909, 4.000000000000000000 ) ) ;
#141901 = DIRECTION ( 'NONE',  ( -0.3543493200069162685, -0.000000000000000000, -0.9351131265310288487 ) ) ;
#141900 = AXIS2_PLACEMENT_3D ( 'NONE', #112779, #89597, #54855 ) ;
#141902 = ADVANCED_FACE ( 'NONE', ( #94368 ), #13939, .F. ) ;
#141903 = EDGE_LOOP ( 'NONE', ( #47069, #84798, #83169, #45164 ) ) ;
#141904 = DIRECTION ( 'NONE',  ( 0.6830127018922181881, 0.6830127018922202975, -0.2588190451025214056 ) ) ;
#141905 = VECTOR ( 'NONE', #64949, 1000.000000000000000 ) ;
#141906 = CARTESIAN_POINT ( 'NONE',  ( 12.18398860626900060, 28.73617430169795739, 5.000000000000000000 ) ) ;
#141907 =( BOUNDED_CURVE ( )  B_SPLINE_CURVE ( 3, ( #108758, #33424, #77622, #88495 ),
 .UNSPECIFIED., .F., .F. ) 
 B_SPLINE_CURVE_WITH_KNOTS ( ( 4, 4 ),
 ( 5.920967161967926273, 7.341195215986648037 ),
 .UNSPECIFIED. ) 
 CURVE ( )  GEOMETRIC_REPRESENTATION_ITEM ( )  RATIONAL_B_SPLINE_CURVE ( ( 1.000000000000000000, 0.8388583629366588301, 0.8388583629366588301, 1.000000000000000000 ) ) 
 REPRESENTATION_ITEM ( '' )  );
#141908 = DIRECTION ( 'NONE',  ( 0.000000000000000000, -1.000000000000000000, 0.000000000000000000 ) ) ;
#141910 = ADVANCED_FACE ( 'NONE', ( #105255 ), #108887, .T. ) ;
#141909 = CARTESIAN_POINT ( 'NONE',  ( 78.10002705046289861, 5.819803920172570422, 5.819803920172575751 ) ) ;
#141911 = VERTEX_POINT ( 'NONE', #5905 ) ;
#141912 = LINE ( 'NONE', #65800, #113158 ) ;
#141913 = ORIENTED_EDGE ( 'NONE', *, *, #43055, .F. ) ;
#141914 = EDGE_CURVE ( 'NONE', #91102, #64204, #60316, .T. ) ;
#141915 = VERTEX_POINT ( 'NONE', #83529 ) ;
#141916 = ORIENTED_EDGE ( 'NONE', *, *, #23764, .T. ) ;
#141917 = CARTESIAN_POINT ( 'NONE',  ( 124.8912635252314516, -4.472830434245838482, -4.472830434245838482 ) ) ;
#141919 = EDGE_LOOP ( 'NONE', ( #70237, #26355, #119530, #74730 ) ) ;
#141918 = AXIS2_PLACEMENT_3D ( 'NONE', #77480, #75327, #121648 ) ;
#141920 =( BOUNDED_CURVE ( )  B_SPLINE_CURVE ( 2, ( #97800, #10762, #133311, #42738, #99198, #20942, #65206, #54337, #143438, #99951, #44154, #88377, #132616 ),
 .UNSPECIFIED., .F., .T. ) 
 B_SPLINE_CURVE_WITH_KNOTS ( ( 3, 2, 2, 2, 2, 2, 3 ),
 ( 0.06666666666666672125, 0.06944444444444450304, 0.07222222222222228483, 0.07500000000000006661, 0.07777777777777784840, 0.08055555555555564407, 0.08333333333333341197 ),
 .UNSPECIFIED. ) 
 CURVE ( )  GEOMETRIC_REPRESENTATION_ITEM ( )  RATIONAL_B_SPLINE_CURVE ( ( 0.9999999999999993339, 0.9659258262890689783, 1.000000000000000000, 0.9659258262890683122, 1.000000000000000000, 0.9659258262890683122, 1.000000000000000000, 0.9659258262890683122, 1.000000000000000000, 0.9659258262890683122, 1.000000000000000000, 0.9659258262890673130, 1.000000000000001110 ) ) 
 REPRESENTATION_ITEM ( '' )  );
#141921 = ADVANCED_FACE ( 'NONE', ( #16825 ), #25545, .F. ) ;
#141922 = DIRECTION ( 'NONE',  ( -0.7071067811865487940, 0.7071067811865463515, -0.000000000000000000 ) ) ;
#141923 = DIRECTION ( 'NONE',  ( 0.5735764363510444941, 0.8191520442889929088, 0.000000000000000000 ) ) ;
#141924 = ORIENTED_EDGE ( 'NONE', *, *, #75387, .T. ) ;
#141925 = LINE ( 'NONE', #56362, #62753 ) ;
#141926 = AXIS2_PLACEMENT_3D ( 'NONE', #102039, #36766, #46265 ) ;
#141927 = ORIENTED_EDGE ( 'NONE', *, *, #133989, .F. ) ;
#141928 = CARTESIAN_POINT ( 'NONE',  ( 11.35373647476855119, -5.808823158059035485, -5.808823158059033709 ) ) ;
#141929 = DIRECTION ( 'NONE',  ( -0.7071067811865486830, -0.7071067811865464625, 0.000000000000000000 ) ) ;
#141930 = DIRECTION ( 'NONE',  ( 0.5735764363510444941, 0.8191520442889929088, 0.000000000000000000 ) ) ;
#141931 = ADVANCED_FACE ( 'NONE', ( #58240 ), #69817, .F. ) ;
#141932 = DIRECTION ( 'NONE',  ( -0.000000000000000000, 0.3543493200069153248, 0.9351131265310292928 ) ) ;
#141933 = ORIENTED_EDGE ( 'NONE', *, *, #98117, .F. ) ;
#141934 = ORIENTED_EDGE ( 'NONE', *, *, #40080, .T. ) ;
#141935 = ORIENTED_EDGE ( 'NONE', *, *, #135180, .T. ) ;
#141936 = CYLINDRICAL_SURFACE ( 'NONE', #92696, 7.950000000000000178 ) ;
#141937 = DIRECTION ( 'NONE',  ( 0.7071067811865487940, 0.7071067811865463515, 0.000000000000000000 ) ) ;
#141938 = VECTOR ( 'NONE', #33379, 999.9999999999998863 ) ;
#141939 = DIRECTION ( 'NONE',  ( 0.000000000000000000, 0.000000000000000000, -1.000000000000000000 ) ) ;
#141940 = ADVANCED_FACE ( 'NONE', ( #81400 ), #92218, .F. ) ;
#141941 = CARTESIAN_POINT ( 'NONE',  ( -3.707106781186519928, 5.259292476615663681, 5.000000000000000000 ) ) ;
#141942 = AXIS2_PLACEMENT_3D ( 'NONE', #105334, #114075, #3159 ) ;
#141943 = CARTESIAN_POINT ( 'NONE',  ( 29.99451991528749417, 28.92564299267958816, 4.000000000000000000 ) ) ;
#141944 = CARTESIAN_POINT ( 'NONE',  ( -19.05000000000000071, 3.174999999999997158, 1.444000000000000394 ) ) ;
#141945 = CARTESIAN_POINT ( 'NONE',  ( 32.37543019189810423, -5.291415217122920289, -3.055000000000001492 ) ) ;
#141946 = DIRECTION ( 'NONE',  ( 0.000000000000000000, 0.000000000000000000, -1.000000000000000000 ) ) ;
#141947 = LINE ( 'NONE', #17278, #16435 ) ;
#141948 = ORIENTED_EDGE ( 'NONE', *, *, #72655, .T. ) ;
#141949 = DIRECTION ( 'NONE',  ( -0.3543493200069162685, -0.000000000000000000, -0.9351131265310288487 ) ) ;
#141950 = VECTOR ( 'NONE', #94441, 1000.000000000000000 ) ;
#141951 = VECTOR ( 'NONE', #126963, 1000.000000000000000 ) ;
#141952 = ORIENTED_EDGE ( 'NONE', *, *, #119890, .T. ) ;
#141953 = FACE_OUTER_BOUND ( 'NONE', #104777, .T. ) ;
#141954 = ORIENTED_EDGE ( 'NONE', *, *, #58435, .T. ) ;
#141955 = LINE ( 'NONE', #86842, #71515 ) ;
#141957 = ORIENTED_EDGE ( 'NONE', *, *, #136766, .F. ) ;
#141956 = DIRECTION ( 'NONE',  ( -0.6830127018922180770, -0.6830127018922204085, -0.2588190451025213501 ) ) ;
#141958 = LINE ( 'NONE', #21584, #60826 ) ;
#141959 = EDGE_CURVE ( 'NONE', #1859, #3259, #92953, .T. ) ;
#141960 = ORIENTED_EDGE ( 'NONE', *, *, #1260, .T. ) ;
#141961 = FILL_AREA_STYLE_COLOUR ( '', #46166 ) ;
#141962 = ORIENTED_EDGE ( 'NONE', *, *, #38949, .T. ) ;
#141963 = CARTESIAN_POINT ( 'NONE',  ( -12.29974487139158512, -27.71228299555214747, 4.000000000000000000 ) ) ;
#141964 = ORIENTED_EDGE ( 'NONE', *, *, #81664, .T. ) ;
#141965 = CARTESIAN_POINT ( 'NONE',  ( -26.29289321881326913, 20.25929247661551003, 5.000000000000000000 ) ) ;
#141966 = EDGE_CURVE ( 'NONE', #50223, #129671, #26977, .T. ) ;
#141967 = CARTESIAN_POINT ( 'NONE',  ( 108.5791937171295700, 3.975000000000002753, -6.884901960086283523 ) ) ;
#141968 = LINE ( 'NONE', #86858, #20456 ) ;
#141969 = DIRECTION ( 'NONE',  ( -0.6830127018922180770, -0.6830127018922204085, -0.2588190451025213501 ) ) ;
#141970 = FACE_OUTER_BOUND ( 'NONE', #140421, .T. ) ;
#141971 = DIRECTION ( 'NONE',  ( -0.7071067811865487940, 0.7071067811865463515, -0.000000000000000000 ) ) ;
#141972 = CARTESIAN_POINT ( 'NONE',  ( 9.041666666666666075, 3.047499999999993214, -5.278424836066146320 ) ) ;
#141973 = CARTESIAN_POINT ( 'NONE',  ( 15.43706980810188512, 2.126176841940952134, -7.934999999999992504 ) ) ;
#141974 = CARTESIAN_POINT ( 'NONE',  ( 0.2569208697893815008, -0.3999999999999998002, -2.015694669338588429 ) ) ;
#141975 = DIRECTION ( 'NONE',  ( -0.000000000000000000, -0.3543493200069152693, 0.9351131265310292928 ) ) ;
#141976 = VERTEX_POINT ( 'NONE', #137903 ) ;
#141977 = VECTOR ( 'NONE', #96728, 1000.000000000000000 ) ;
#141978 = ORIENTED_EDGE ( 'NONE', *, *, #126649, .T. ) ;
#141979 = EDGE_CURVE ( 'NONE', #115599, #69745, #82812, .T. ) ;
#141980 = CARTESIAN_POINT ( 'NONE',  ( 0.000000000000000000, 0.000000000000000000, 5.000000000000000000 ) ) ;
#141981 = VERTEX_POINT ( 'NONE', #71952 ) ;
#141982 = VECTOR ( 'NONE', #115472, 1000.000000000000000 ) ;
#141983 = CARTESIAN_POINT ( 'NONE',  ( -63.18398860626900415, 28.73617430169831621, 5.000000000000000000 ) ) ;
#141984 = CARTESIAN_POINT ( 'NONE',  ( 128.2885478629881959, -48.75494892434343797, -38.51155878621305106 ) ) ;
#141985 = ORIENTED_EDGE ( 'NONE', *, *, #86685, .F. ) ;
#141986 = CARTESIAN_POINT ( 'NONE',  ( -1.499999999999985789, -7.533600742197660516, 5.000000000000000000 ) ) ;
#141987 = DIRECTION ( 'NONE',  ( 0.6830127018922181881, 0.6830127018922202975, -0.2588190451025214056 ) ) ;
#141988 = VECTOR ( 'NONE', #1023, 1000.000000000000000 ) ;
#141989 = CARTESIAN_POINT ( 'NONE',  ( -1.214984197241888220, -3.740707523384244837, 15.76143240460123707 ) ) ;
#141990 = EDGE_CURVE ( 'NONE', #116759, #75714, #116122, .T. ) ;
#141991 =( NAMED_UNIT ( * ) PLANE_ANGLE_UNIT ( ) SI_UNIT ( $, .RADIAN. ) );
#141993 = VERTEX_POINT ( 'NONE', #107391 ) ;
#141992 = CARTESIAN_POINT ( 'NONE',  ( 42.48921356237308800, -27.52281430457085065, 5.000000000000000000 ) ) ;
#141994 = LINE ( 'NONE', #142684, #23499 ) ;
#141995 = CARTESIAN_POINT ( 'NONE',  ( 84.29974487139159578, -27.71228299555264840, 4.000000000000000000 ) ) ;
#141996 = FACE_OUTER_BOUND ( 'NONE', #18354, .T. ) ;
#141997 = DIRECTION ( 'NONE',  ( 0.6830127018922181881, 0.6830127018922202975, -0.2588190451025214056 ) ) ;
#141998 = DIRECTION ( 'NONE',  ( 0.7071067811865487940, 0.7071067811865463515, 0.000000000000000000 ) ) ;
#141999 = VECTOR ( 'NONE', #123229, 1000.000000000000114 ) ;
#142000 = ORIENTED_EDGE ( 'NONE', *, *, #8448, .F. ) ;
#142001 = ORIENTED_EDGE ( 'NONE', *, *, #33492, .T. ) ;
#142002 = VERTEX_POINT ( 'NONE', #106658 ) ;
#142003 = CARTESIAN_POINT ( 'NONE',  ( 95.37543019189810423, -5.291415217122920289, -3.055000000000001492 ) ) ;
#142004 = CIRCLE ( 'NONE', #130406, 2.500000000000000444 ) ;
#142005 = EDGE_LOOP ( 'NONE', ( #24177, #7, #103528, #93188 ) ) ;
#142006 = MANIFOLD_SOLID_BREP ( 'Cut-Extrude1', #138928 ) ;
#142007 = CARTESIAN_POINT ( 'NONE',  ( 126.9785101690858085, -47.44491123045132497, 36.62621018406386497 ) ) ;
#142008 = AXIS2_PLACEMENT_3D ( 'NONE', #108220, #94512, #140867 ) ;
#142009 = LINE ( 'NONE', #42698, #57028 ) ;
#142010 = VERTEX_POINT ( 'NONE', #84253 ) ;
#142011 = DIRECTION ( 'NONE',  ( 1.000000000000000000, 0.000000000000000000, 0.000000000000000000 ) ) ;
#142012 = CARTESIAN_POINT ( 'NONE',  ( 48.68749999999998579, -5.819803920172573974, 5.819803920172573086 ) ) ;
#142013 = CARTESIAN_POINT ( 'NONE',  ( 98.93293019189812298, 1.637169565754156508, 6.110000000000000320 ) ) ;
#142014 = ORIENTED_EDGE ( 'NONE', *, *, #55889, .F. ) ;
#142015 = DIRECTION ( 'NONE',  ( -0.7071067811865487940, 0.7071067811865463515, 0.000000000000000000 ) ) ;
#142016 = EDGE_CURVE ( 'NONE', #111064, #108173, #79262, .T. ) ;
#142017 = VECTOR ( 'NONE', #116331, 1000.000000000000000 ) ;
#142018 = CARTESIAN_POINT ( 'NONE',  ( 115.3333333333333286, -6.884901960086287964, 3.974999999999998312 ) ) ;
#142019 = ORIENTED_EDGE ( 'NONE', *, *, #72922, .F. ) ;
#142020 = ORIENTED_EDGE ( 'NONE', *, *, #72189, .T. ) ;
#142021 = ORIENTED_EDGE ( 'NONE', *, *, #102084, .F. ) ;
#142022 = LINE ( 'NONE', #64434, #104653 ) ;
#142024 = EDGE_CURVE ( 'NONE', #109497, #139229, #19669, .T. ) ;
#142023 = EDGE_CURVE ( 'NONE', #21869, #2836, #28424, .T. ) ;
#142025 = EDGE_CURVE ( 'NONE', #20582, #95024, #108071, .T. ) ;
#142026 = CARTESIAN_POINT ( 'NONE',  ( 2.999999999999983569, -9.412538124160661823, 4.000000000000000000 ) ) ;
#142027 = STYLED_ITEM ( 'NONE', ( #59973 ), #79080 ) ;
#142028 = CARTESIAN_POINT ( 'NONE',  ( 0.000000000000000000, 0.000000000000000000, 0.000000000000000000 ) ) ;
#142029 = LINE ( 'NONE', #143424, #110460 ) ;
#142030 = FACE_OUTER_BOUND ( 'NONE', #54025, .T. ) ;
#142031 = ADVANCED_FACE ( 'NONE', ( #129866 ), #53346, .T. ) ;
#142032 = EDGE_CURVE ( 'NONE', #73728, #81832, #42165, .T. ) ;
#142033 = EDGE_CURVE ( 'NONE', #64109, #99607, #101988, .T. ) ;
#142034 = ORIENTED_EDGE ( 'NONE', *, *, #98719, .T. ) ;
#142035 = ORIENTED_EDGE ( 'NONE', *, *, #22113, .T. ) ;
#142037 = EDGE_CURVE ( 'NONE', #84513, #114295, #8741, .T. ) ;
#142036 = CARTESIAN_POINT ( 'NONE',  ( 34.42499999999998295, 0.000000000000000000, 4.500000000000000888 ) ) ;
#142038 = ORIENTED_EDGE ( 'NONE', *, *, #74006, .F. ) ;
#142039 = ORIENTED_EDGE ( 'NONE', *, *, #57796, .T. ) ;
#142040 = ADVANCED_FACE ( 'NONE', ( #6602 ), #50884, .F. ) ;
#142041 = VECTOR ( 'NONE', #98012, 999.9999999999998863 ) ;
#142042 = ADVANCED_FACE ( 'NONE', ( #8058 ), #27894, .T. ) ;
#142043 = CARTESIAN_POINT ( 'NONE',  ( 69.48921356237309510, -27.52281430457103895, 5.000000000000000000 ) ) ;
#142044 = VERTEX_POINT ( 'NONE', #31281 ) ;
#142045 = LINE ( 'NONE', #77507, #131603 ) ;
#142046 =( NAMED_UNIT ( * ) PLANE_ANGLE_UNIT ( ) SI_UNIT ( $, .RADIAN. ) );
#142047 = LINE ( 'NONE', #76798, #6201 ) ;
#142048 = VECTOR ( 'NONE', #84937, 1000.000000000000000 ) ;
#142049 = DIRECTION ( 'NONE',  ( 0.7071067811865486830, -0.7071067811865464625, -0.000000000000000000 ) ) ;
#142050 = FACE_OUTER_BOUND ( 'NONE', #4179, .T. ) ;
#142051 = ORIENTED_EDGE ( 'NONE', *, *, #7958, .F. ) ;
#142052 = EDGE_CURVE ( 'NONE', #88480, #130600, #141460, .T. ) ;
#142053 = CARTESIAN_POINT ( 'NONE',  ( 21.46453280170069888, 4.202752102959690472E-16, 0.000000000000000000 ) ) ;
#142054 = ORIENTED_EDGE ( 'NONE', *, *, #13422, .T. ) ;
#142055 = DIRECTION ( 'NONE',  ( 0.7071067811865486830, -0.7071067811865464625, -0.000000000000000000 ) ) ;
#142056 = ORIENTED_EDGE ( 'NONE', *, *, #664, .F. ) ;
#142057 = CARTESIAN_POINT ( 'NONE',  ( -42.29974487139158157, -27.71228299555235708, 4.000000000000000000 ) ) ;
#142058 = ORIENTED_EDGE ( 'NONE', *, *, #88400, .T. ) ;
#142059 = CARTESIAN_POINT ( 'NONE',  ( 22.04263059361153410, -22.22500000000000142, -16.58716479377923392 ) ) ;
#142060 = ORIENTED_EDGE ( 'NONE', *, *, #113230, .T. ) ;
#142061 = ORIENTED_EDGE ( 'NONE', *, *, #75095, .F. ) ;
#142063 = EDGE_CURVE ( 'NONE', #38177, #3445, #119663, .T. ) ;
#142062 = VECTOR ( 'NONE', #32753, 1000.000000000000000 ) ;
#142064 = ORIENTED_EDGE ( 'NONE', *, *, #124808, .T. ) ;
#142065 = DIRECTION ( 'NONE',  ( 1.000000000000000000, 0.000000000000000000, 0.000000000000000000 ) ) ;
#142066 = AXIS2_PLACEMENT_3D ( 'NONE', #128916, #116618, #139835 ) ;
#142067 = LINE ( 'NONE', #129013, #25244 ) ;
#142068 = CARTESIAN_POINT ( 'NONE',  ( -12.18398860626900060, 28.73617430169795739, 5.000000000000000000 ) ) ;
#142069 = CARTESIAN_POINT ( 'NONE',  ( -51.48921356237309510, -27.52281430457091460, 5.000000000000000000 ) ) ;
#142070 = CARTESIAN_POINT ( 'NONE',  ( 13.73493329717941158, 12.75929247661558996, 18.34774599283953123 ) ) ;
#142071 = CARTESIAN_POINT ( 'NONE',  ( 18.32816939922340183, -3.740707523384248390, 4.000000000000000000 ) ) ;
#142073 = CARTESIAN_POINT ( 'NONE',  ( 26.75159235450331963, 9.902892378096218942E-16, 0.000000000000000000 ) ) ;
#142072 = AXIS2_PLACEMENT_3D ( 'NONE', #33684, #77885, #43124 ) ;
#142075 = EDGE_CURVE ( 'NONE', #57315, #5353, #102055, .T. ) ;
#142074 = LINE ( 'NONE', #39916, #27394 ) ;
#142076 = PLANE ( 'NONE',  #138543 ) ;
#142077 = AXIS2_PLACEMENT_3D ( 'NONE', #88048, #75060, #85899 ) ;
#142078 = CARTESIAN_POINT ( 'NONE',  ( -32.20710678118632586, -20.24070752338406720, 5.000000000000000000 ) ) ;
#142079 = VERTEX_POINT ( 'NONE', #56464 ) ;
#142080 = EDGE_CURVE ( 'NONE', #68374, #35947, #47718, .T. ) ;
#142081 = EDGE_LOOP ( 'NONE', ( #134728, #65275, #2379, #55089 ) ) ;
#142082 = ORIENTED_EDGE ( 'NONE', *, *, #67098, .F. ) ;
#142083 = LINE ( 'NONE', #652, #33356 ) ;
#142084 = VERTEX_POINT ( 'NONE', #25190 ) ;
#142085 = EDGE_CURVE ( 'NONE', #132991, #7168, #12882, .T. ) ;
#142086 = VECTOR ( 'NONE', #60465, 1000.000000000000000 ) ;
#142087 = ORIENTED_EDGE ( 'NONE', *, *, #128694, .T. ) ;
#142088 = LINE ( 'NONE', #17415, #9694 ) ;
#142089 = CARTESIAN_POINT ( 'NONE',  ( -32.99999999999976552, -12.03360074219761522, 5.000000000000000000 ) ) ;
#142090 = LINE ( 'NONE', #75389, #90284 ) ;
#142091 = ORIENTED_EDGE ( 'NONE', *, *, #122211, .F. ) ;
#142092 = DIRECTION ( 'NONE',  ( -0.000000000000000000, -0.3543493200069152693, 0.9351131265310292928 ) ) ;
#142093 = ORIENTED_EDGE ( 'NONE', *, *, #63682, .T. ) ;
#142094 = VECTOR ( 'NONE', #137403, 1000.000000000000000 ) ;
#142095 = CARTESIAN_POINT ( 'NONE',  ( 17.07999999999999829, 9.521314400968980422E-16, 0.000000000000000000 ) ) ;
#142096 = VECTOR ( 'NONE', #76835, 1000.000000000000227 ) ;
#142097 = CARTESIAN_POINT ( 'NONE',  ( 7.650403141435218934, 7.934999999999989839, -2.126176841940961904 ) ) ;
#142098 = ORIENTED_EDGE ( 'NONE', *, *, #65335, .T. ) ;
#142099 = CARTESIAN_POINT ( 'NONE',  ( 89.89126352523143737, -4.472830434245839371, -4.472830434245839371 ) ) ;
#142100 = LINE ( 'NONE', #55803, #106097 ) ;
#142102 = EDGE_CURVE ( 'NONE', #120930, #123203, #23029, .T. ) ;
#142101 = CARTESIAN_POINT ( 'NONE',  ( 25.39999999999999858, -7.600000000000055600, -28.92499999999998650 ) ) ;
#142103 = CARTESIAN_POINT ( 'NONE',  ( -29.99999999999978328, -16.02097659208072855, -11.96015758381201444 ) ) ;
#142104 = VERTEX_POINT ( 'NONE', #123830 ) ;
#142105 = ORIENTED_EDGE ( 'NONE', *, *, #31375, .F. ) ;
#142106 = DIRECTION ( 'NONE',  ( 0.000000000000000000, 1.000000000000000000, 0.000000000000000000 ) ) ;
#142107 = EDGE_LOOP ( 'NONE', ( #44819, #117513, #109082, #3625 ) ) ;
#142109 = VECTOR ( 'NONE', #67020, 1000.000000000000000 ) ;
#142108 = LINE ( 'NONE', #20280, #85625 ) ;
#142110 = DIRECTION ( 'NONE',  ( 0.7071067811865487940, 0.7071067811865463515, 0.000000000000000000 ) ) ;
#142111 = DIRECTION ( 'NONE',  ( 0.7071067811865487940, 0.7071067811865463515, -0.000000000000000000 ) ) ;
#142112 = CARTESIAN_POINT ( 'NONE',  ( -30.48921356237309510, -27.52281430457076894, 5.000000000000000000 ) ) ;
#142113 = ORIENTED_EDGE ( 'NONE', *, *, #49438, .T. ) ;
#142114 = CARTESIAN_POINT ( 'NONE',  ( 34.92499999999998295, 18.20450307870172324, 3.476483422452878447 ) ) ;
#142115 = LINE ( 'NONE', #18124, #90618 ) ;
#142116 = CARTESIAN_POINT ( 'NONE',  ( -29.99451991528749417, 28.92564299267958816, 4.000000000000000000 ) ) ;
#142117 = VERTEX_POINT ( 'NONE', #68053 ) ;
#142118 = DIRECTION ( 'NONE',  ( -0.6830127018922180770, -0.6830127018922204085, -0.2588190451025213501 ) ) ;
#142119 = AXIS2_PLACEMENT_3D ( 'NONE', #50268, #126377, #106027 ) ;
#142120 = CARTESIAN_POINT ( 'NONE',  ( -36.18398860626899705, 28.73617430169812437, 5.000000000000000000 ) ) ;
#142121 = VERTEX_POINT ( 'NONE', #101335 ) ;
#142124 = EDGE_CURVE ( 'NONE', #121849, #62751, #120468, .T. ) ;
#142123 = VERTEX_POINT ( 'NONE', #123111 ) ;
#142122 = LINE ( 'NONE', #110858, #108783 ) ;
#142125 = VERTEX_POINT ( 'NONE', #34667 ) ;
#142126 =( GEOMETRIC_REPRESENTATION_CONTEXT ( 3 ) GLOBAL_UNCERTAINTY_ASSIGNED_CONTEXT ( ( #72099 ) ) GLOBAL_UNIT_ASSIGNED_CONTEXT ( ( #18386, #10385, #96653 ) ) REPRESENTATION_CONTEXT ( 'NONE', 'WORKASPACE' ) );
#142127 = LINE ( 'NONE', #85560, #26181 ) ;
#142128 = LINE ( 'NONE', #85562, #87738 ) ;
#142129 = VERTEX_POINT ( 'NONE', #1971 ) ;
#142130 = LINE ( 'NONE', #129075, #125269 ) ;
#142131 = CARTESIAN_POINT ( 'NONE',  ( -17.99999999999987210, -21.03360074219752462, 5.000000000000000000 ) ) ;
#142132 = ADVANCED_FACE ( 'NONE', ( #135425 ), #90469, .T. ) ;
#142134 = VECTOR ( 'NONE', #16141, 999.9999999999998863 ) ;
#142133 = DIRECTION ( 'NONE',  ( 1.000000000000000000, 3.115803279706880257E-16, 0.000000000000000000 ) ) ;
#142135 = CARTESIAN_POINT ( 'NONE',  ( 7.139999999999985469, -39.92999999999999972, -39.50000000000000000 ) ) ;
#142136 = LINE ( 'NONE', #130540, #23475 ) ;
#142137 = CARTESIAN_POINT ( 'NONE',  ( 27.79289321881326558, 0.7592924766157104211, 5.000000000000000000 ) ) ;
#142138 = DIRECTION ( 'NONE',  ( -1.000000000000000000, -1.224606353822377258E-16, -0.000000000000000000 ) ) ;
#142139 = LINE ( 'NONE', #53698, #87655 ) ;
#142140 = PLANE ( 'NONE',  #92060 ) ;
#142141 = LINE ( 'NONE', #97904, #65250 ) ;
#142142 = PLANE ( 'NONE',  #134009 ) ;
#142143 = DIRECTION ( 'NONE',  ( -0.7071067811865487940, 0.7071067811865463515, 0.000000000000000000 ) ) ;
#142144 = CARTESIAN_POINT ( 'NONE',  ( 76.78752705046289861, 0.000000000000000000, -7.949999999999998401 ) ) ;
#142145 = ORIENTED_EDGE ( 'NONE', *, *, #30398, .T. ) ;
#142147 = EDGE_CURVE ( 'NONE', #81437, #21537, #57869, .T. ) ;
#142146 = AXIS2_PLACEMENT_3D ( 'NONE', #125265, #59332, #25954 ) ;
#142148 = ORIENTED_EDGE ( 'NONE', *, *, #19160, .F. ) ;
#142149 = ORIENTED_EDGE ( 'NONE', *, *, #133181, .T. ) ;
#142150 = CARTESIAN_POINT ( 'NONE',  ( 98.70833333333332860, -3.974999999999999201, -6.884901960086287964 ) ) ;
#142151 = EDGE_CURVE ( 'NONE', #22356, #6977, #67300, .T. ) ;
#142152 = ORIENTED_EDGE ( 'NONE', *, *, #39946, .F. ) ;
#142153 = ORIENTED_EDGE ( 'NONE', *, *, #134682, .F. ) ;
#142154 = ORIENTED_EDGE ( 'NONE', *, *, #79847, .T. ) ;
#142155 = CARTESIAN_POINT ( 'NONE',  ( 15.18079593298623564, 4.202752102959690472E-16, 0.000000000000000000 ) ) ;
#142156 = PLANE ( 'NONE',  #4563 ) ;
#142157 = ORIENTED_EDGE ( 'NONE', *, *, #10569, .F. ) ;
#142158 = DIRECTION ( 'NONE',  ( 1.734723475976806848E-16, -1.000000000000000000, 0.000000000000000000 ) ) ;
#142159 = FACE_OUTER_BOUND ( 'NONE', #18089, .T. ) ;
#142160 = CARTESIAN_POINT ( 'NONE',  ( -23.99999999999983302, -16.06887692260764666, 4.000000000000000000 ) ) ;
#142161 = LINE ( 'NONE', #19638, #37293 ) ;
#142162 = ORIENTED_EDGE ( 'NONE', *, *, #954, .F. ) ;
#142163 = EDGE_CURVE ( 'NONE', #68937, #16896, #35410, .T. ) ;
#142164 = LINE ( 'NONE', #64580, #92792 ) ;
#142165 = SURFACE_STYLE_USAGE ( .BOTH. , #30539 ) ;
#142166 = CIRCLE ( 'NONE', #7894, 5.968999999999998529 ) ;
#142167 = CARTESIAN_POINT ( 'NONE',  ( 23.99451991528749062, 28.92564299267954908, 4.000000000000000000 ) ) ;
#142168 = CARTESIAN_POINT ( 'NONE',  ( 24.35416666666666785, 1.633150327867675555, 6.094999999999998863 ) ) ;
#142169 = LINE ( 'NONE', #19645, #47737 ) ;
#142170 = CARTESIAN_POINT ( 'NONE',  ( 31.87086038379621655, 6.884901960086289741, -3.974999999999993427 ) ) ;
#142171 = DIRECTION ( 'NONE',  ( -1.000000000000000000, -0.000000000000000000, -0.000000000000000000 ) ) ;
#142172 = VECTOR ( 'NONE', #82776, 1000.000000000000000 ) ;
#142173 = VERTEX_POINT ( 'NONE', #33960 ) ;
#142174 = ORIENTED_EDGE ( 'NONE', *, *, #21725, .T. ) ;
#142175 = CARTESIAN_POINT ( 'NONE',  ( 26.22916666666666075, 7.950000000000001954, -2.130196079827421762 ) ) ;
#142176 = ORIENTED_EDGE ( 'NONE', *, *, #8206, .F. ) ;
#142177 = DIRECTION ( 'NONE',  ( -0.6830127018922181881, 0.6830127018922202975, -0.2588190451025214056 ) ) ;
#142178 = DIRECTION ( 'NONE',  ( -1.000000000000000000, -1.224606353822377258E-16, -0.000000000000000000 ) ) ;
#142179 = CARTESIAN_POINT ( 'NONE',  ( -29.67183060077626422, -3.740707523384238176, 4.000000000000000000 ) ) ;
#142180 = CONICAL_SURFACE ( 'NONE', #61184, 2.055000000000000604, 0.9599310885968764806 ) ;
#142181 = DIRECTION ( 'NONE',  ( 0.7071067811865487940, 0.7071067811865463515, 0.000000000000000000 ) ) ;
#142182 = LINE ( 'NONE', #89905, #113830 ) ;
#142183 = CARTESIAN_POINT ( 'NONE',  ( -15.48921356237309510, -27.52281430457066236, 5.000000000000000000 ) ) ;
#142184 = CARTESIAN_POINT ( 'NONE',  ( 127.6620968585647802, -5.291415217122919401, 3.054999999999997939 ) ) ;
#142185 = VECTOR ( 'NONE', #141553, 1000.000000000000000 ) ;
#142186 = EDGE_LOOP ( 'NONE', ( #21045, #122469, #45610, #98056 ) ) ;
#142187 = EDGE_CURVE ( 'NONE', #121941, #111265, #133966, .T. ) ;
#142188 = VERTEX_POINT ( 'NONE', #2728 ) ;
#142189 = CARTESIAN_POINT ( 'NONE',  ( 33.70710678118631165, -3.740707523384253719, 5.000000000000000000 ) ) ;
#142190 = DIRECTION ( 'NONE',  ( 0.000000000000000000, -1.000000000000000000, 0.000000000000000000 ) ) ;
#142191 = AXIS2_PLACEMENT_3D ( 'NONE', #123408, #34964, #3013 ) ;
#142192 = LINE ( 'NONE', #8059, #30294 ) ;
#142193 = ORIENTED_EDGE ( 'NONE', *, *, #82591, .F. ) ;
#142194 = CARTESIAN_POINT ( 'NONE',  ( 44.04209685856477563, 5.291415217122923842, -3.054999999999996163 ) ) ;
#142195 = AXIS2_PLACEMENT_3D ( 'NONE', #833, #13133, #132106 ) ;
#142196 = ORIENTED_EDGE ( 'NONE', *, *, #127006, .F. ) ;
#142197 = DIRECTION ( 'NONE',  ( -0.6830127018922180770, 0.6830127018922202975, -0.2588190451025213501 ) ) ;
#142198 = FACE_OUTER_BOUND ( 'NONE', #134205, .T. ) ;
#142199 = CARTESIAN_POINT ( 'NONE',  ( 27.18398860626900060, 28.73617430169806042, 5.000000000000000000 ) ) ;
#142200 = PLANE ( 'NONE',  #108566 ) ;
#142201 = AXIS2_PLACEMENT_3D ( 'NONE', #15075, #25247, #59348 ) ;
#142202 = EDGE_CURVE ( 'NONE', #5968, #40900, #19913, .T. ) ;
#142203 = CARTESIAN_POINT ( 'NONE',  ( 40.45376352523144448, -6.109999999999998543, -3.741295971395162543E-16 ) ) ;
#142204 = EDGE_CURVE ( 'NONE', #1190, #130461, #36104, .T. ) ;
#142205 = ORIENTED_EDGE ( 'NONE', *, *, #72172, .T. ) ;
#142207 = EDGE_CURVE ( 'NONE', #134120, #126282, #131291, .T. ) ;
#142206 = CARTESIAN_POINT ( 'NONE',  ( 7.171830600776424092, -14.24070752338414003, 4.000000000000000000 ) ) ;
#142208 = ORIENTED_EDGE ( 'NONE', *, *, #62036, .F. ) ;
#142209 = ORIENTED_EDGE ( 'NONE', *, *, #60574, .T. ) ;
#142210 = ORIENTED_EDGE ( 'NONE', *, *, #84284, .T. ) ;
#142211 = EDGE_CURVE ( 'NONE', #131756, #121582, #131582, .T. ) ;
#142212 = CARTESIAN_POINT ( 'NONE',  ( -54.48921356237310221, -27.52281430457093236, 5.000000000000000000 ) ) ;
#142213 = DIRECTION ( 'NONE',  ( 0.000000000000000000, -1.000000000000000000, 0.000000000000000000 ) ) ;
#142214 = ORIENTED_EDGE ( 'NONE', *, *, #54220, .T. ) ;
#142215 = FACE_OUTER_BOUND ( 'NONE', #143411, .T. ) ;
#142216 = ADVANCED_FACE ( 'NONE', ( #18678 ), #100388, .F. ) ;
#142217 = LINE ( 'NONE', #66081, #10766 ) ;
#142218 = VECTOR ( 'NONE', #83630, 999.9999999999998863 ) ;
#142219 = CARTESIAN_POINT ( 'NONE',  ( 14.00000000000000178, 0.000000000000000000, 6.094999999999989981 ) ) ;
#142220 = DIRECTION ( 'NONE',  ( 0.3543493200069162685, -0.000000000000000000, -0.9351131265310288487 ) ) ;
#142221 = ADVANCED_FACE ( 'NONE', ( #1032 ), #21393, .F. ) ;
#142222 = FACE_BOUND ( 'NONE', #72288, .T. ) ;
#142223 = ORIENTED_EDGE ( 'NONE', *, *, #112601, .F. ) ;
#142224 = ADVANCED_FACE ( 'NONE', ( #132322 ), #89493, .T. ) ;
#142225 = FACE_OUTER_BOUND ( 'NONE', #47051, .T. ) ;
#142226 = FACE_OUTER_BOUND ( 'NONE', #17600, .T. ) ;
#142227 = LINE ( 'NONE', #9510, #9131 ) ;
#142228 = VERTEX_POINT ( 'NONE', #67043 ) ;
#142229 = CARTESIAN_POINT ( 'NONE',  ( -1.499999999999984013, 0.05218569542916363935, 5.000000000000000000 ) ) ;
#142230 = VERTEX_POINT ( 'NONE', #133728 ) ;
#142231 = EDGE_LOOP ( 'NONE', ( #21689, #74125, #27796, #119127 ) ) ;
#142232 = FACE_OUTER_BOUND ( 'NONE', #16892, .T. ) ;
#142233 = EDGE_CURVE ( 'NONE', #81784, #75896, #11918, .T. ) ;
#142234 = VERTEX_POINT ( 'NONE', #98242 ) ;
#142235 = CARTESIAN_POINT ( 'NONE',  ( 58.09959685856477307, -6.109999999999997655, -1.637169565754160283 ) ) ;
#142236 = ORIENTED_EDGE ( 'NONE', *, *, #81757, .T. ) ;
#142237 = CARTESIAN_POINT ( 'NONE',  ( 45.48921356237309510, -27.52281430457087197, 5.000000000000000000 ) ) ;
#142238 = ORIENTED_EDGE ( 'NONE', *, *, #83088, .T. ) ;
#142239 = DIRECTION ( 'NONE',  ( 0.7071067811865487940, -0.7071067811865463515, 0.000000000000000000 ) ) ;
#142240 = CARTESIAN_POINT ( 'NONE',  ( -11.51078643762690490, -27.52281430457047406, 5.000000000000000000 ) ) ;
#142241 = ORIENTED_EDGE ( 'NONE', *, *, #67809, .T. ) ;
#142242 = DIRECTION ( 'NONE',  ( -0.6830127018922180770, -0.6830127018922204085, -0.2588190451025213501 ) ) ;
#142243 = LINE ( 'NONE', #126503, #62017 ) ;
#142244 = VECTOR ( 'NONE', #43270, 999.9999999999998863 ) ;
#142245 = DIRECTION ( 'NONE',  ( 0.7071067811865486830, -0.7071067811865464625, -0.000000000000000000 ) ) ;
#142246 = FACE_OUTER_BOUND ( 'NONE', #71097, .T. ) ;
#142247 = CARTESIAN_POINT ( 'NONE',  ( 34.42499999999998295, -10.45860074219784330, 5.000000000000000000 ) ) ;
#142248 = DIRECTION ( 'NONE',  ( 0.7071067811865487940, 0.7071067811865463515, -0.000000000000000000 ) ) ;
#142249 = DIRECTION ( 'NONE',  ( -0.3543493200069162685, -0.000000000000000000, -0.9351131265310288487 ) ) ;
#142250 = VERTEX_POINT ( 'NONE', #62955 ) ;
#142251 = EDGE_CURVE ( 'NONE', #61103, #34098, #120672, .T. ) ;
#142252 = VERTEX_POINT ( 'NONE', #143159 ) ;
#142253 = EDGE_LOOP ( 'NONE', ( #118614, #102154, #89286, #63201 ) ) ;
#142254 = DIRECTION ( 'NONE',  ( -0.3543493200069163240, 4.681814790819596721E-17, -0.9351131265310288487 ) ) ;
#142255 = DIRECTION ( 'NONE',  ( -0.000000000000000000, -0.3543493200069152693, 0.9351131265310292928 ) ) ;
#142256 = ORIENTED_EDGE ( 'NONE', *, *, #98802, .F. ) ;
#142257 = EDGE_LOOP ( 'NONE', ( #50490, #99660, #61940, #27641 ) ) ;
#142258 = CARTESIAN_POINT ( 'NONE',  ( -33.48921356237309510, -27.52281430457078670, 5.000000000000000000 ) ) ;
#142259 = LINE ( 'NONE', #99412, #22433 ) ;
#142260 = PLANE ( 'NONE',  #115708 ) ;
#142261 = VERTEX_POINT ( 'NONE', #142466 ) ;
#142262 = PLANE ( 'NONE',  #32426 ) ;
#142263 = VECTOR ( 'NONE', #96543, 1000.000000000000000 ) ;
#142264 = CARTESIAN_POINT ( 'NONE',  ( -60.18398860626900415, 28.73617430169829490, 5.000000000000000000 ) ) ;
#142265 = AXIS2_PLACEMENT_3D ( 'NONE', #60150, #38379, #68890 ) ;
#142266 = CARTESIAN_POINT ( 'NONE',  ( 18.00456980810188767, 6.871911579029510442, -3.967499999999998916 ) ) ;
#142267 = CARTESIAN_POINT ( 'NONE',  ( -15.18398860626900237, 28.73617430169797871, 5.000000000000000000 ) ) ;
#142268 = EDGE_LOOP ( 'NONE', ( #47948, #1171, #65413, #140933 ) ) ;
#142269 = CARTESIAN_POINT ( 'NONE',  ( 118.7662635252314516, 4.472830434245839371, -4.472830434245839371 ) ) ;
#142270 = VECTOR ( 'NONE', #68363, 1000.000000000000000 ) ;
#142272 = EDGE_CURVE ( 'NONE', #88886, #103321, #73115, .T. ) ;
#142271 = CARTESIAN_POINT ( 'NONE',  ( -11.70025512860841133, -27.71228299555198049, 4.000000000000000000 ) ) ;
#142273 = DIRECTION ( 'NONE',  ( -0.000000000000000000, -0.3543493200069152693, 0.9351131265310292928 ) ) ;
#142275 = ORIENTED_EDGE ( 'NONE', *, *, #95288, .F. ) ;
#142274 = LINE ( 'NONE', #95, #5530 ) ;
#142276 = DIRECTION ( 'NONE',  ( -0.7071067811865487940, 0.7071067811865463515, -0.000000000000000000 ) ) ;
#142277 = ORIENTED_EDGE ( 'NONE', *, *, #1478, .F. ) ;
#142278 = CARTESIAN_POINT ( 'NONE',  ( 76.78752705046289861, 0.000000000000000000, -7.949999999999998401 ) ) ;
#142279 = FACE_OUTER_BOUND ( 'NONE', #59552, .T. ) ;
#142280 = DIRECTION ( 'NONE',  ( -0.7071067811865487940, 0.7071067811865463515, -0.000000000000000000 ) ) ;
#142281 = VERTEX_POINT ( 'NONE', #54747 ) ;
#142282 = VECTOR ( 'NONE', #111407, 1000.000000000000000 ) ;
#142283 = ADVANCED_FACE ( 'NONE', ( #11176 ), #17953, .F. ) ;
#142284 = CARTESIAN_POINT ( 'NONE',  ( 0.000000000000000000, 0.000000000000000000, 7.950000000000000178 ) ) ;
#142285 = CARTESIAN_POINT ( 'NONE',  ( -19.83455468016618184, -2.420908269918533140, -33.24323018688586018 ) ) ;
#142286 = VERTEX_POINT ( 'NONE', #95543 ) ;
#142287 = CYLINDRICAL_SURFACE ( 'NONE', #32047, 2.500000000000000000 ) ;
#142288 = LINE ( 'NONE', #98055, #88635 ) ;
#142289 = ORIENTED_EDGE ( 'NONE', *, *, #105646, .T. ) ;
#142290 = CYLINDRICAL_SURFACE ( 'NONE', #80860, 0.5000000000000004441 ) ;
#142292 = EDGE_CURVE ( 'NONE', #111382, #143133, #139804, .T. ) ;
#142291 = ORIENTED_EDGE ( 'NONE', *, *, #141103, .T. ) ;
#142293 = EDGE_LOOP ( 'NONE', ( #13387, #68222, #94613, #23298 ) ) ;
#142294 = FACE_OUTER_BOUND ( 'NONE', #66628, .T. ) ;
#142295 = FACE_OUTER_BOUND ( 'NONE', #81583, .T. ) ;
#142296 = ORIENTED_EDGE ( 'NONE', *, *, #43953, .F. ) ;
#142297 = AXIS2_PLACEMENT_3D ( 'NONE', #4878, #84640, #95494 ) ;
#142298 = CARTESIAN_POINT ( 'NONE',  ( 184.1500000000000057, -30.18000000000009564, -12.70000000000045404 ) ) ;
#142299 = AXIS2_PLACEMENT_3D ( 'NONE', #58145, #48660, #126216 ) ;
#142300 = VECTOR ( 'NONE', #113734, 1000.000000000000227 ) ;
#142301 = CARTESIAN_POINT ( 'NONE',  ( 156.1499999999997783, -57.14999999999999147, -62.92499999999978400 ) ) ;
#142302 = DIRECTION ( 'NONE',  ( -0.7071067811865486830, -0.7071067811865464625, 0.000000000000000000 ) ) ;
#142303 = ORIENTED_EDGE ( 'NONE', *, *, #36665, .T. ) ;
#142304 = COLOUR_RGB ( '', 0.09019608, 0.27058824, 0.51372549) ;
#142305 = CARTESIAN_POINT ( 'NONE',  ( 0.000000000000000000, 8.616843969807042924, 0.000000000000000000 ) ) ;
#142306 = FACE_OUTER_BOUND ( 'NONE', #111622, .T. ) ;
#142307 = FACE_OUTER_BOUND ( 'NONE', #60495, .T. ) ;
#142308 = CARTESIAN_POINT ( 'NONE',  ( 3.707106781186514599, 14.25929247661557575, 5.000000000000000000 ) ) ;
#142309 = CARTESIAN_POINT ( 'NONE',  ( 33.16209685856478018, -5.291415217122919401, 3.054999999999998384 ) ) ;
#142310 = CARTESIAN_POINT ( 'NONE',  ( -7.140000000000000568, -39.92999999999998550, -39.79289321881344677 ) ) ;
#142311 = AXIS2_PLACEMENT_3D ( 'NONE', #133836, #35972, #123698 ) ;
#142312 = ORIENTED_EDGE ( 'NONE', *, *, #50756, .T. ) ;
#142313 = VERTEX_POINT ( 'NONE', #22080 ) ;
#142314 = DIRECTION ( 'NONE',  ( 0.6830127018922180770, -0.6830127018922204085, -0.2588190451025213501 ) ) ;
#142315 = EDGE_CURVE ( 'NONE', #103344, #41451, #33716, .T. ) ;
#142316 = ORIENTED_EDGE ( 'NONE', *, *, #103664, .F. ) ;
#142317 = ORIENTED_EDGE ( 'NONE', *, *, #101446, .T. ) ;
#142318 = DIRECTION ( 'NONE',  ( -0.000000000000000000, 0.3543493200069153248, 0.9351131265310292928 ) ) ;
#142319 = CARTESIAN_POINT ( 'NONE',  ( -72.29974487139158157, -27.71228299555256669, 4.000000000000000000 ) ) ;
#142320 = VERTEX_POINT ( 'NONE', #84681 ) ;
#142321 = DIRECTION ( 'NONE',  ( 0.6830127018922181881, 0.6830127018922202975, -0.2588190451025214056 ) ) ;
#142322 = LINE ( 'NONE', #64033, #104566 ) ;
#142323 = CARTESIAN_POINT ( 'NONE',  ( 34.92499999999998295, 22.22500000000000142, 4.000000000000000000 ) ) ;
#142324 = EDGE_CURVE ( 'NONE', #50292, #131000, #76504, .T. ) ;
#142325 = PLANE ( 'NONE',  #46546 ) ;
#142326 = DIRECTION ( 'NONE',  ( 0.7071067811865487940, 0.7071067811865463515, 0.000000000000000000 ) ) ;
#142327 = ORIENTED_EDGE ( 'NONE', *, *, #31824, .T. ) ;
#142328 = EDGE_CURVE ( 'NONE', #5368, #127658, #29566, .T. ) ;
#142329 = CARTESIAN_POINT ( 'NONE',  ( 0.000000000000000000, -49.14999999999999147, 34.92500000000001847 ) ) ;
#142330 = CARTESIAN_POINT ( 'NONE',  ( -21.32816939922338406, 20.25929247661551358, 4.000000000000000000 ) ) ;
#142331 = DIRECTION ( 'NONE',  ( -0.7071067811865486830, -0.7071067811865464625, 0.000000000000000000 ) ) ;
#142332 = CARTESIAN_POINT ( 'NONE',  ( -15.18398860626900237, 28.73617430169797871, 5.000000000000000000 ) ) ;
#142333 = CARTESIAN_POINT ( 'NONE',  ( -48.18398860626899705, 28.73617430169820608, 5.000000000000000000 ) ) ;
#142334 = CARTESIAN_POINT ( 'NONE',  ( 55.05836038379620589, -7.949999999999997513, -2.130196079827425759 ) ) ;
#142335 = DIRECTION ( 'NONE',  ( 0.7071067811865487940, 0.7071067811865463515, 0.000000000000000000 ) ) ;
#142336 = VERTEX_POINT ( 'NONE', #33015 ) ;
#142337 = ORIENTED_EDGE ( 'NONE', *, *, #27179, .F. ) ;
#142338 = CARTESIAN_POINT ( 'NONE',  ( 50.72916666666665719, 7.950000000000001954, -2.130196079827421762 ) ) ;
#142339 = DIRECTION ( 'NONE',  ( -0.000000000000000000, 0.3543493200069153248, 0.9351131265310292928 ) ) ;
#142340 = CARTESIAN_POINT ( 'NONE',  ( 13.92145407031093818, 3.061616997868383634E-16, -2.500000000000000444 ) ) ;
#142341 = DIRECTION ( 'NONE',  ( -0.7071067811865486830, 0.7071067811865464625, 0.000000000000000000 ) ) ;
#142342 = VERTEX_POINT ( 'NONE', #77231 ) ;
#142343 = PLANE ( 'NONE',  #71095 ) ;
#142344 = EDGE_CURVE ( 'NONE', #12589, #43910, #99642, .T. ) ;
#142345 = AXIS2_PLACEMENT_3D ( 'NONE', #68102, #12934, #112976 ) ;
#142346 = DIRECTION ( 'NONE',  ( -0.3543493200069162685, -0.000000000000000000, -0.9351131265310288487 ) ) ;
#142347 = CARTESIAN_POINT ( 'NONE',  ( 49.87543019189810423, -5.291415217122920289, -3.055000000000001492 ) ) ;
#142348 = ORIENTED_EDGE ( 'NONE', *, *, #13438, .T. ) ;
#142349 = LINE ( 'NONE', #122712, #75748 ) ;
#142350 = ORIENTED_EDGE ( 'NONE', *, *, #41856, .T. ) ;
#142351 = VERTEX_POINT ( 'NONE', #77922 ) ;
#142352 = CARTESIAN_POINT ( 'NONE',  ( 24.41159235450331977, 2.500000000000001332, 0.000000000000000000 ) ) ;
#142353 = DIRECTION ( 'NONE',  ( 0.7071067811865487940, 0.7071067811865463515, -0.000000000000000000 ) ) ;
#142354 = DIRECTION ( 'NONE',  ( -0.000000000000000000, -0.3543493200069152138, 0.9351131265310292928 ) ) ;
#142355 = EDGE_LOOP ( 'NONE', ( #66905, #53707, #31951, #132785 ) ) ;
#142356 = PLANE ( 'NONE',  #11747 ) ;
#142358 = EDGE_LOOP ( 'NONE', ( #121675, #102860, #61571, #90704 ) ) ;
#142357 = CARTESIAN_POINT ( 'NONE',  ( 0.000000000000000000, 0.000000000000000000, 0.000000000000000000 ) ) ;
#142359 = CARTESIAN_POINT ( 'NONE',  ( 79.47959685856477563, 6.109999999999999432, 1.637169565754164280 ) ) ;
#142360 = CARTESIAN_POINT ( 'NONE',  ( 4.828169399223499525, 21.75929247661549581, 4.000000000000000000 ) ) ;
#142361 = LINE ( 'NONE', #107563, #54740 ) ;
#142362 = CARTESIAN_POINT ( 'NONE',  ( 12.69999999999999574, -35.28159979880237529, 17.66442088362879659 ) ) ;
#142363 = DIRECTION ( 'NONE',  ( -0.000000000000000000, 0.000000000000000000, 1.000000000000000000 ) ) ;
#142364 = VECTOR ( 'NONE', #25900, 1000.000000000000000 ) ;
#142365 = ADVANCED_FACE ( 'NONE', ( #122110 ), #22765, .F. ) ;
#142366 = VERTEX_POINT ( 'NONE', #39292 ) ;
#142367 = LINE ( 'NONE', #43060, #26847 ) ;
#142368 = CARTESIAN_POINT ( 'NONE',  ( 62.76626352523144448, 4.472830434245839371, -4.472830434245838482 ) ) ;
#142369 = EDGE_CURVE ( 'NONE', #43657, #41375, #38569, .T. ) ;
#142370 = CIRCLE ( 'NONE', #8099, 5.968999999999998529 ) ;
#142371 = PLANE ( 'NONE',  #71903 ) ;
#142372 = CARTESIAN_POINT ( 'NONE',  ( 32.99999999999976552, -4.068876922607775448, 4.000000000000000000 ) ) ;
#142373 =( NAMED_UNIT ( * ) SI_UNIT ( $, .STERADIAN. ) SOLID_ANGLE_UNIT ( ) );
#142374 = ORIENTED_EDGE ( 'NONE', *, *, #3479, .T. ) ;
#142375 = ORIENTED_EDGE ( 'NONE', *, *, #19027, .T. ) ;
#142376 = FACE_OUTER_BOUND ( 'NONE', #140840, .T. ) ;
#142377 = DIRECTION ( 'NONE',  ( 1.734723475976806848E-16, -1.000000000000000000, 0.000000000000000000 ) ) ;
#142378 = ORIENTED_EDGE ( 'NONE', *, *, #61238, .F. ) ;
#142379 = EDGE_CURVE ( 'NONE', #125764, #83371, #73356, .T. ) ;
#142380 = EDGE_CURVE ( 'NONE', #100225, #43483, #82803, .T. ) ;
#142381 = ORIENTED_EDGE ( 'NONE', *, *, #34263, .T. ) ;
#142382 = VECTOR ( 'NONE', #126925, 1000.000000000000000 ) ;
#142383 = CARTESIAN_POINT ( 'NONE',  ( 1.500000000000001332, -5.947814304570766986, 5.000000000000000000 ) ) ;
#142384 = VERTEX_POINT ( 'NONE', #137895 ) ;
#142385 = DIRECTION ( 'NONE',  ( -0.7071067811865487940, 0.7071067811865463515, -0.000000000000000000 ) ) ;
#142386 = CARTESIAN_POINT ( 'NONE',  ( 22.85159235450332105, -2.500000000000000444, 3.061616997868384620E-16 ) ) ;
#142387 = LINE ( 'NONE', #11830, #11848 ) ;
#142388 = EDGE_CURVE ( 'NONE', #90074, #85291, #49483, .T. ) ;
#142389 = FACE_BOUND ( 'NONE', #32513, .T. ) ;
#142390 = EDGE_CURVE ( 'NONE', #137465, #97116, #61090, .T. ) ;
#142391 = CARTESIAN_POINT ( 'NONE',  ( -36.18398860626899705, 28.73617430169812437, 5.000000000000000000 ) ) ;
#142392 = LINE ( 'NONE', #109010, #108178 ) ;
#142394 = ORIENTED_EDGE ( 'NONE', *, *, #122530, .T. ) ;
#142393 = CARTESIAN_POINT ( 'NONE',  ( -69.18398860626899705, 28.73617430169835529, 5.000000000000000000 ) ) ;
#142395 = DIRECTION ( 'NONE',  ( -0.000000000000000000, 0.3543493200069153248, 0.9351131265310292928 ) ) ;
#142397 = EDGE_CURVE ( 'NONE', #48401, #127256, #84245, .T. ) ;
#142396 = ITEM_DEFINED_TRANSFORMATION ( 'NONE', 'NONE', #77178,  #127880 ) ;
#142398 = AXIS2_PLACEMENT_3D ( 'NONE', #48180, #4597, #118222 ) ;
#142399 = ORIENTED_EDGE ( 'NONE', *, *, #56835, .T. ) ;
#142400 = VECTOR ( 'NONE', #56882, 999.9999999999998863 ) ;
#142402 = EDGE_LOOP ( 'NONE', ( #93661, #118653, #102290, #120329 ) ) ;
#142401 = VECTOR ( 'NONE', #132476, 1000.000000000000227 ) ;
#142403 = CARTESIAN_POINT ( 'NONE',  ( 80.26626352523145158, 4.472830434245838482, -4.472830434245837594 ) ) ;
#142404 = VERTEX_POINT ( 'NONE', #72678 ) ;
#142405 = CIRCLE ( 'NONE', #82283, 2.247899999999996901 ) ;
#142406 = CARTESIAN_POINT ( 'NONE',  ( -18.29974487139159223, -27.71228299555219010, 4.000000000000000000 ) ) ;
#142407 = EDGE_LOOP ( 'NONE', ( #12994, #128048, #12970, #66292 ) ) ;
#142408 = LINE ( 'NONE', #129356, #32825 ) ;
#142409 = EDGE_CURVE ( 'NONE', #95511, #61485, #93670, .T. ) ;
#142410 = LINE ( 'NONE', #62709, #68038 ) ;
#142411 = FACE_OUTER_BOUND ( 'NONE', #38222, .T. ) ;
#142412 = DIRECTION ( 'NONE',  ( 0.7071067811865487940, 0.7071067811865463515, -0.000000000000000000 ) ) ;
#142413 = CARTESIAN_POINT ( 'NONE',  ( -20.99999999999984368, 8.816494571476647835, 4.604407763760409722 ) ) ;
#142414 = LINE ( 'NONE', #119202, #97947 ) ;
#142415 = PLANE ( 'NONE',  #113360 ) ;
#142416 = ORIENTED_EDGE ( 'NONE', *, *, #17897, .T. ) ;
#142417 = EDGE_CURVE ( 'NONE', #50406, #120761, #27674, .T. ) ;
#142418 = CARTESIAN_POINT ( 'NONE',  ( -16.49999999999988276, 16.46639925780209168, 5.000000000000000000 ) ) ;
#142419 = ORIENTED_EDGE ( 'NONE', *, *, #127720, .T. ) ;
#142420 = PLANE ( 'NONE',  #12459 ) ;
#142421 = DIRECTION ( 'NONE',  ( 0.000000000000000000, 0.000000000000000000, 1.000000000000000000 ) ) ;
#142422 = ORIENTED_EDGE ( 'NONE', *, *, #16620, .T. ) ;
#142423 = ORIENTED_EDGE ( 'NONE', *, *, #28806, .T. ) ;
#142424 = EDGE_CURVE ( 'NONE', #49858, #119902, #40718, .T. ) ;
#142425 = CARTESIAN_POINT ( 'NONE',  ( 34.27126352523143993, 4.472830434245838482, 4.472830434245842035 ) ) ;
#142426 = EDGE_CURVE ( 'NONE', #30783, #49766, #67339, .T. ) ;
#142427 = ORIENTED_EDGE ( 'NONE', *, *, #107580, .T. ) ;
#142428 = LINE ( 'NONE', #8981, #39028 ) ;
#142429 = EDGE_CURVE ( 'NONE', #85199, #130484, #95037, .T. ) ;
#142430 = CARTESIAN_POINT ( 'NONE',  ( -14.39513766812470408, 21.75929247661548516, 21.32995629748189259 ) ) ;
#142431 = CARTESIAN_POINT ( 'NONE',  ( 29.64997294953710139, -4.461849672132299105, 4.461849672132299993 ) ) ;
#142432 = CARTESIAN_POINT ( 'NONE',  ( 2.289041571428004573, 12.44546514678316029, -26.86570989468548021 ) ) ;
#142433 = VERTEX_POINT ( 'NONE', #52286 ) ;
#142434 = ORIENTED_EDGE ( 'NONE', *, *, #50956, .T. ) ;
#142435 =( LENGTH_UNIT ( ) NAMED_UNIT ( * ) SI_UNIT ( .MILLI., .METRE. ) );
#142436 = DIRECTION ( 'NONE',  ( 1.000000000000000000, -0.000000000000000000, 0.000000000000000000 ) ) ;
#142438 = ORIENTED_EDGE ( 'NONE', *, *, #59686, .F. ) ;
#142437 = CARTESIAN_POINT ( 'NONE',  ( 34.42499999999998295, 17.97718569542920619, 5.000000000000000000 ) ) ;
#142439 = ORIENTED_EDGE ( 'NONE', *, *, #27402, .T. ) ;
#142440 = CARTESIAN_POINT ( 'NONE',  ( 7.940000000000001279, -33.26999999999999602, -8.101350000000008933 ) ) ;
#142441 = CARTESIAN_POINT ( 'NONE',  ( 9.489213562373095101, -27.52281430457062328, 5.000000000000000000 ) ) ;
#142442 = DIRECTION ( 'NONE',  ( 0.7071067811865487940, -0.7071067811865463515, 0.000000000000000000 ) ) ;
#142443 = ORIENTED_EDGE ( 'NONE', *, *, #43472, .F. ) ;
#142444 = LINE ( 'NONE', #41687, #75923 ) ;
#142445 = VERTEX_POINT ( 'NONE', #105933 ) ;
#142446 = ORIENTED_EDGE ( 'NONE', *, *, #36805, .T. ) ;
#142447 = ORIENTED_EDGE ( 'NONE', *, *, #115566, .F. ) ;
#142448 = EDGE_CURVE ( 'NONE', #24260, #119311, #6595, .T. ) ;
#142449 = CARTESIAN_POINT ( 'NONE',  ( 10.31275183893061431, -22.22500000000000142, 22.14227524773687605 ) ) ;
#142450 = DIRECTION ( 'NONE',  ( 1.000000000000000000, 0.000000000000000000, 0.000000000000000000 ) ) ;
#142451 = LINE ( 'NONE', #64171, #138770 ) ;
#142452 = DIRECTION ( 'NONE',  ( -0.7071067811865487940, 0.7071067811865463515, -0.000000000000000000 ) ) ;
#142453 = DIRECTION ( 'NONE',  ( -0.6830127018922181881, 0.6830127018922202975, -0.2588190451025214056 ) ) ;
#142454 = PLANE ( 'NONE',  #118871 ) ;
#142455 = LINE ( 'NONE', #100376, #62226 ) ;
#142457 = EDGE_CURVE ( 'NONE', #108628, #107596, #94362, .T. ) ;
#142456 = ORIENTED_EDGE ( 'NONE', *, *, #123823, .F. ) ;
#142458 = LINE ( 'NONE', #3003, #21119 ) ;
#142459 = VERTEX_POINT ( 'NONE', #95794 ) ;
#142460 = CARTESIAN_POINT ( 'NONE',  ( -34.45011844616454511, -19.48371918836232197, 5.000000000000000888 ) ) ;
#142461 = VECTOR ( 'NONE', #19132, 1000.000000000000000 ) ;
#142462 = DIRECTION ( 'NONE',  ( 0.7071067811865487940, 0.7071067811865463515, 0.000000000000000000 ) ) ;
#142463 = VERTEX_POINT ( 'NONE', #63212 ) ;
#142464 = DIRECTION ( 'NONE',  ( 0.7071067811865487940, 0.7071067811865463515, -0.000000000000000000 ) ) ;
#142465 =( BOUNDED_CURVE ( )  B_SPLINE_CURVE ( 3, ( #102752, #46254, #90435, #22998 ),
 .UNSPECIFIED., .F., .T. ) 
 B_SPLINE_CURVE_WITH_KNOTS ( ( 4, 4 ),
 ( 5.920967161967927161, 7.341195215986644484 ),
 .UNSPECIFIED. ) 
 CURVE ( )  GEOMETRIC_REPRESENTATION_ITEM ( )  RATIONAL_B_SPLINE_CURVE ( ( 1.000000000000000000, 0.8388583629366599403, 0.8388583629366599403, 1.000000000000000000 ) ) 
 REPRESENTATION_ITEM ( '' )  );
#142466 = CARTESIAN_POINT ( 'NONE',  ( -17.99999999999987210, -10.06887692260770883, 4.000000000000000000 ) ) ;
#142467 = LINE ( 'NONE', #31556, #42078 ) ;
#142468 = ORIENTED_EDGE ( 'NONE', *, *, #78922, .F. ) ;
#142469 = MANIFOLD_SOLID_BREP ( 'Fillet6', #78794 ) ;
#142470 = ORIENTED_EDGE ( 'NONE', *, *, #123242, .F. ) ;
#142471 = FACE_OUTER_BOUND ( 'NONE', #88300, .T. ) ;
#142472 = CARTESIAN_POINT ( 'NONE',  ( -18.29974487139159223, -27.71228299555219010, 4.000000000000000000 ) ) ;
#142473 = FILL_AREA_STYLE_COLOUR ( '', #135448 ) ;
#142474 = CARTESIAN_POINT ( 'NONE',  ( -34.92500000000001137, -21.28150956279555217, 4.759050581649342249 ) ) ;
#142475 = CARTESIAN_POINT ( 'NONE',  ( 70.05793019189812298, 6.110000000000001208, -1.637169565754156286 ) ) ;
#142476 = CARTESIAN_POINT ( 'NONE',  ( 14.99451991528749595, 28.92564299267948513, 4.000000000000000000 ) ) ;
#142477 = DIRECTION ( 'NONE',  ( -0.000000000000000000, -0.3543493200069152693, 0.9351131265310292928 ) ) ;
#142478 = VECTOR ( 'NONE', #50113, 1000.000000000000227 ) ;
#142479 = DIRECTION ( 'NONE',  ( -0.6830127018922180770, -0.6830127018922204085, -0.2588190451025213501 ) ) ;
#142480 = DIRECTION ( 'NONE',  ( -0.7071067811865486830, -0.7071067811865464625, 0.000000000000000000 ) ) ;
#142481 = EDGE_CURVE ( 'NONE', #112045, #132778, #40031, .T. ) ;
#142482 = EDGE_LOOP ( 'NONE', ( #49069, #101660, #128205, #43224 ) ) ;
#142483 = CARTESIAN_POINT ( 'NONE',  ( -74.99451991528749772, 28.92564299267990435, 4.000000000000000000 ) ) ;
#142484 = VERTEX_POINT ( 'NONE', #133438 ) ;
#142485 = DIRECTION ( 'NONE',  ( -0.7071067811865487940, 0.7071067811865463515, -0.000000000000000000 ) ) ;
#142486 = DIRECTION ( 'NONE',  ( 0.7071067811865487940, -0.7071067811865463515, 0.000000000000000000 ) ) ;
#142487 = EDGE_LOOP ( 'NONE', ( #90769, #122154, #68148, #124624 ) ) ;
#142488 = DIRECTION ( 'NONE',  ( 0.6830127018922181881, 0.6830127018922202975, -0.2588190451025214056 ) ) ;
#142490 = ORIENTED_EDGE ( 'NONE', *, *, #49916, .T. ) ;
#142489 = LINE ( 'NONE', #9809, #118207 ) ;
#142491 =( NAMED_UNIT ( * ) SI_UNIT ( $, .STERADIAN. ) SOLID_ANGLE_UNIT ( ) );
#142492 = EDGE_CURVE ( 'NONE', #63172, #61426, #7044, .T. ) ;
#142493 = DIRECTION ( 'NONE',  ( 0.7071067811865487940, 0.7071067811865463515, -0.000000000000000000 ) ) ;
#142494 = DIRECTION ( 'NONE',  ( -1.000000000000000000, -0.000000000000000000, 0.000000000000000000 ) ) ;
#142495 = ORIENTED_EDGE ( 'NONE', *, *, #107541, .T. ) ;
#142496 = EDGE_CURVE ( 'NONE', #39702, #64814, #44298, .T. ) ;
#142497 = ORIENTED_EDGE ( 'NONE', *, *, #63442, .F. ) ;
#142498 = DIRECTION ( 'NONE',  ( 0.3543493200069162685, -0.000000000000000000, -0.9351131265310288487 ) ) ;
#142499 = DIRECTION ( 'NONE',  ( -0.000000000000000000, -0.3543493200069152693, 0.9351131265310292928 ) ) ;
#142500 = CARTESIAN_POINT ( 'NONE',  ( 53.41205288902393278, -48.51956544822607498, 36.87500513592860329 ) ) ;
#142501 = AXIS2_PLACEMENT_3D ( 'NONE', #50678, #70344, #127522 ) ;
#142502 = DIRECTION ( 'NONE',  ( -1.000000000000000000, -1.224606353822377258E-16, -0.000000000000000000 ) ) ;
#142503 = CARTESIAN_POINT ( 'NONE',  ( 82.32919371712955581, -3.975000000000001865, 6.884901960086284411 ) ) ;
#142504 = LINE ( 'NONE', #23559, #97205 ) ;
#142505 = AXIS2_PLACEMENT_3D ( 'NONE', #88139, #18740, #11238 ) ;
#142506 = CARTESIAN_POINT ( 'NONE',  ( 34.92499999999998295, -21.72500000000000142, 5.000000000000000000 ) ) ;
#142507 = ORIENTED_EDGE ( 'NONE', *, *, #33873, .T. ) ;
#142508 = CARTESIAN_POINT ( 'NONE',  ( 85.58333333333332860, 6.884901960086290629, -3.974999999999994316 ) ) ;
#142510 = EDGE_CURVE ( 'NONE', #73074, #73177, #23200, .T. ) ;
#142509 = AXIS2_PLACEMENT_3D ( 'NONE', #94277, #37786, #138513 ) ;
#142511 = CARTESIAN_POINT ( 'NONE',  ( 0.000000000000000000, 0.000000000000000000, 0.000000000000000000 ) ) ;
#142512 = LINE ( 'NONE', #8365, #39348 ) ;
#142513 = CARTESIAN_POINT ( 'NONE',  ( 32.95833333333334281, -3.047499999999997211, -5.278424836066143655 ) ) ;
#142514 = VECTOR ( 'NONE', #5503, 1000.000000000000000 ) ;
#142515 = ORIENTED_EDGE ( 'NONE', *, *, #105591, .T. ) ;
#142516 = EDGE_CURVE ( 'NONE', #70885, #35824, #78337, .T. ) ;
#142517 = CYLINDRICAL_SURFACE ( 'NONE', #90835, 2.500000000000000000 ) ;
#142518 = EDGE_LOOP ( 'NONE', ( #143246, #19035, #579, #118541 ) ) ;
#142519 = CARTESIAN_POINT ( 'NONE',  ( 79.04209685856477563, 5.291415217122923842, -3.054999999999996163 ) ) ;
#142520 = PLANE ( 'NONE',  #133435 ) ;
#142521 = FACE_OUTER_BOUND ( 'NONE', #47665, .T. ) ;
#142522 = ORIENTED_EDGE ( 'NONE', *, *, #5464, .T. ) ;
#142523 = EDGE_CURVE ( 'NONE', #14903, #71811, #119657, .T. ) ;
#142524 = ADVANCED_FACE ( 'NONE', ( #108776 ), #39614, .T. ) ;
#142525 = LINE ( 'NONE', #120740, #14172 ) ;
#142526 = PLANE ( 'NONE',  #109009 ) ;
#142527 = CARTESIAN_POINT ( 'NONE',  ( 125.5000000000000000, 0.000000000000000000, 0.000000000000000000 ) ) ;
#142528 = DIRECTION ( 'NONE',  ( -0.000000000000000000, 0.000000000000000000, 1.000000000000000000 ) ) ;
#142530 = EDGE_LOOP ( 'NONE', ( #27306, #132931, #77989, #36193 ) ) ;
#142529 = DIRECTION ( 'NONE',  ( 0.7071067811865486830, -0.7071067811865464625, -0.000000000000000000 ) ) ;
#142531 = CARTESIAN_POINT ( 'NONE',  ( -3.792893218813427669, 0.7592924766157086447, 5.000000000000000000 ) ) ;
#142532 = DIRECTION ( 'NONE',  ( -1.000000000000000000, -1.224606353822377258E-16, -0.000000000000000000 ) ) ;
#142533 = CARTESIAN_POINT ( 'NONE',  ( 48.48921356237309510, -27.52281430457089328, 5.000000000000000000 ) ) ;
#142534 = DIRECTION ( 'NONE',  ( -0.7071067811865486830, 0.7071067811865464625, 0.000000000000000000 ) ) ;
#142535 = ORIENTED_EDGE ( 'NONE', *, *, #22533, .T. ) ;
#142536 =( BOUNDED_CURVE ( )  B_SPLINE_CURVE ( 3, ( #133736, #119952, #22772, #43872 ),
 .UNSPECIFIED., .F., .T. ) 
 B_SPLINE_CURVE_WITH_KNOTS ( ( 4, 4 ),
 ( 1.964434688349487423, 3.503810798801452187 ),
 .UNSPECIFIED. ) 
 CURVE ( )  GEOMETRIC_REPRESENTATION_ITEM ( )  RATIONAL_B_SPLINE_CURVE ( ( 1.000000000000000000, 0.8120851936182278408, 0.8120851936182278408, 1.000000000000000000 ) ) 
 REPRESENTATION_ITEM ( '' )  );
#142537 = ORIENTED_EDGE ( 'NONE', *, *, #130042, .T. ) ;
#142538 = CARTESIAN_POINT ( 'NONE',  ( 64.02126352523144703, -4.472830434245839371, -4.472830434245840259 ) ) ;
#142539 = ORIENTED_EDGE ( 'NONE', *, *, #86600, .F. ) ;
#142540 = LINE ( 'NONE', #141079, #26751 ) ;
#142541 = EDGE_CURVE ( 'NONE', #8157, #63249, #110218, .T. ) ;
#142542 = FACE_OUTER_BOUND ( 'NONE', #65864, .T. ) ;
#142543 = DIRECTION ( 'NONE',  ( -0.6830127018922180770, -0.6830127018922204085, -0.2588190451025213501 ) ) ;
#142544 = DIRECTION ( 'NONE',  ( 0.7071067811865487940, 0.7071067811865463515, 0.000000000000000000 ) ) ;
#142545 = ORIENTED_EDGE ( 'NONE', *, *, #75867, .T. ) ;
#142546 = ORIENTED_EDGE ( 'NONE', *, *, #118336, .F. ) ;
#142547 = LINE ( 'NONE', #65734, #7534 ) ;
#142548 = FACE_OUTER_BOUND ( 'NONE', #4538, .T. ) ;
#142549 = EDGE_CURVE ( 'NONE', #39048, #38617, #34126, .T. ) ;
#142550 = EDGE_CURVE ( 'NONE', #40586, #90219, #130593, .T. ) ;
#142551 = ORIENTED_EDGE ( 'NONE', *, *, #105600, .F. ) ;
#142552 = CARTESIAN_POINT ( 'NONE',  ( -18.53421140649331633, 9.121673282332597665, 4.000000000000000000 ) ) ;
#142553 = DIRECTION ( 'NONE',  ( -0.7071067811865486830, -0.7071067811865464625, 0.000000000000000000 ) ) ;
#142554 = LINE ( 'NONE', #110592, #39999 ) ;
#142555 = EDGE_CURVE ( 'NONE', #86941, #69882, #25412, .T. ) ;
#142556 = ORIENTED_EDGE ( 'NONE', *, *, #88062, .F. ) ;
#142557 = ADVANCED_FACE ( 'NONE', ( #21083 ), #42158, .F. ) ;
#142558 = FACE_BOUND ( 'NONE', #128294, .T. ) ;
#142559 = ADVANCED_FACE ( 'NONE', ( #31971 ), #97946, .T. ) ;
#142560 = DIRECTION ( 'NONE',  ( 1.000000000000000000, 1.224606353822377258E-16, 0.000000000000000000 ) ) ;
#142561 = FACE_OUTER_BOUND ( 'NONE', #9421, .T. ) ;
#142562 = CARTESIAN_POINT ( 'NONE',  ( 14.86920357848291196, -2.499999999999999112, 0.000000000000000000 ) ) ;
#142563 = LINE ( 'NONE', #19343, #85882 ) ;
#142564 = SURFACE_SIDE_STYLE ('',( #118649 ) ) ;
#142566 = ORIENTED_EDGE ( 'NONE', *, *, #17954, .F. ) ;
#142565 = AXIS2_PLACEMENT_3D ( 'NONE', #125886, #128037, #38163 ) ;
#142567 = ADVANCED_FACE ( 'NONE', ( #92755 ), #34844, .F. ) ;
#142568 = EDGE_LOOP ( 'NONE', ( #74427, #124909, #11062, #26809 ) ) ;
#142569 = CARTESIAN_POINT ( 'NONE',  ( 108.4120968585647944, 5.291415217122921177, -3.054999999999994831 ) ) ;
#142570 = VERTEX_POINT ( 'NONE', #123990 ) ;
#142571 = ADVANCED_FACE ( 'NONE', ( #26099 ), #81940, .F. ) ;
#142572 = AXIS2_PLACEMENT_3D ( 'NONE', #13951, #96312, #16638 ) ;
#142573 = EDGE_LOOP ( 'NONE', ( #1025, #116310, #121911, #13207 ) ) ;
#142574 = ADVANCED_FACE ( 'NONE', ( #123290 ), #23960, .F. ) ;
#142575 = CARTESIAN_POINT ( 'NONE',  ( 0.000000000000000000, 0.000000000000000000, 5.000000000000000000 ) ) ;
#142576 = LINE ( 'NONE', #43267, #30953 ) ;
#142577 = EDGE_LOOP ( 'NONE', ( #142938, #89055, #51150, #71973 ) ) ;
#142578 = DIRECTION ( 'NONE',  ( -1.000000000000000000, 0.000000000000000000, -0.000000000000000000 ) ) ;
#142579 = DIRECTION ( 'NONE',  ( -0.7071067811865486830, -0.7071067811865464625, 0.000000000000000000 ) ) ;
#142580 = CARTESIAN_POINT ( 'NONE',  ( -20.66652290003515446, 8.920938975803856863, 4.000000000000000000 ) ) ;
#142581 = CARTESIAN_POINT ( 'NONE',  ( 9.707013264292969623, -21.74070752338406365, 4.999753212805217117 ) ) ;
#142582 = EDGE_CURVE ( 'NONE', #62743, #43483, #68218, .T. ) ;
#142583 = DIRECTION ( 'NONE',  ( 0.000000000000000000, -0.7453559924999275665, 0.6666666666666692942 ) ) ;
#142584 = VERTEX_POINT ( 'NONE', #58781 ) ;
#142585 = LINE ( 'NONE', #96878, #65811 ) ;
#142586 = CARTESIAN_POINT ( 'NONE',  ( -9.299744871391588674, -27.71228299555212971, 4.000000000000000000 ) ) ;
#142587 = VERTEX_POINT ( 'NONE', #36265 ) ;
#142588 = ORIENTED_EDGE ( 'NONE', *, *, #41429, .F. ) ;
#142589 = EDGE_LOOP ( 'NONE', ( #40708, #129074, #95562, #119433 ) ) ;
#142590 = CARTESIAN_POINT ( 'NONE',  ( 65.47959685856477563, 6.109999999999999432, 1.637169565754164280 ) ) ;
#142591 = ADVANCED_FACE ( 'NONE', ( #67486 ), #13050, .T. ) ;
#142592 = VERTEX_POINT ( 'NONE', #124689 ) ;
#142593 = AXIS2_PLACEMENT_3D ( 'NONE', #9848, #41058, #87433 ) ;
#142594 = CARTESIAN_POINT ( 'NONE',  ( -13.49999999999989342, -11.94781430457069860, 5.000000000000000000 ) ) ;
#142595 = EDGE_CURVE ( 'NONE', #64781, #137282, #62793, .T. ) ;
#142596 = CARTESIAN_POINT ( 'NONE',  ( 24.29974487139158867, -27.71228299555223273, 4.000000000000000000 ) ) ;
#142597 = CARTESIAN_POINT ( 'NONE',  ( 104.1254301918981184, 5.291415217122919401, 3.055000000000002824 ) ) ;
#142598 = CARTESIAN_POINT ( 'NONE',  ( 6.489213562373093325, -27.52281430457059841, 5.000000000000000000 ) ) ;
#142599 = VECTOR ( 'NONE', #62189, 1000.000000000000227 ) ;
#142600 = STYLED_ITEM ( 'NONE', ( #49466 ), #39731 ) ;
#142601 = ORIENTED_EDGE ( 'NONE', *, *, #131378, .T. ) ;
#142602 = CARTESIAN_POINT ( 'NONE',  ( 14.86920357848291196, 3.821174125832445049E-16, 0.000000000000000000 ) ) ;
#142603 = VECTOR ( 'NONE', #97142, 1000.000000000000000 ) ;
#142604 = EDGE_CURVE ( 'NONE', #112363, #12102, #39711, .T. ) ;
#142605 = CARTESIAN_POINT ( 'NONE',  ( 3.000000000000000000, -4.600000000000013856, 20.40202195861967382 ) ) ;
#142606 = CARTESIAN_POINT ( 'NONE',  ( 1.499999999999994449, 4.466399257802216027, 5.000000000000000000 ) ) ;
#142607 = DIRECTION ( 'NONE',  ( 0.7071067811865486830, -0.7071067811865464625, -0.000000000000000000 ) ) ;
#142608 = ORIENTED_EDGE ( 'NONE', *, *, #88689, .T. ) ;
#142609 = CARTESIAN_POINT ( 'NONE',  ( 19.05000000000000071, 3.174999999999997158, 0.000000000000000000 ) ) ;
#142610 = ORIENTED_EDGE ( 'NONE', *, *, #90156, .T. ) ;
#142611 = ORIENTED_EDGE ( 'NONE', *, *, #133847, .F. ) ;
#142612 = EDGE_LOOP ( 'NONE', ( #69038, #128122, #120900, #9605 ) ) ;
#142613 = CARTESIAN_POINT ( 'NONE',  ( 125.6204301918981088, 3.055000000000001936, -5.291415217122916737 ) ) ;
#142614 = VERTEX_POINT ( 'NONE', #89906 ) ;
#142615 = LINE ( 'NONE', #131025, #67806 ) ;
#142616 = LINE ( 'NONE', #66490, #118078 ) ;
#142617 = ORIENTED_EDGE ( 'NONE', *, *, #5371, .F. ) ;
#142618 = CARTESIAN_POINT ( 'NONE',  ( 34.82816939922328459, 0.7592924766157034266, 4.000000000000000000 ) ) ;
#142619 = ORIENTED_EDGE ( 'NONE', *, *, #7194, .F. ) ;
#142620 = CARTESIAN_POINT ( 'NONE',  ( 12.08290314143522082, 3.967499999999992699, -6.871911579029513994 ) ) ;
#142621 = SURFACE_SIDE_STYLE ('',( #120108 ) ) ;
#142622 = DIRECTION ( 'NONE',  ( 0.7071067811865487940, 0.7071067811865463515, 0.000000000000000000 ) ) ;
#142623 = CARTESIAN_POINT ( 'NONE',  ( 16.61159235450331906, 2.500000000000001776, 0.000000000000000000 ) ) ;
#142624 = ORIENTED_EDGE ( 'NONE', *, *, #52401, .T. ) ;
#142625 = EDGE_LOOP ( 'NONE', ( #137203, #9874, #14318, #119275 ) ) ;
#142626 = ORIENTED_EDGE ( 'NONE', *, *, #73936, .T. ) ;
#142627 = CARTESIAN_POINT ( 'NONE',  ( 19.54166666666666785, 3.047499999999993214, -5.278424836066146320 ) ) ;
#142628 = DIRECTION ( 'NONE',  ( 0.7071067811865487940, 0.7071067811865463515, -0.000000000000000000 ) ) ;
#142629 = VECTOR ( 'NONE', #114995, 1000.000000000000000 ) ;
#142630 = CARTESIAN_POINT ( 'NONE',  ( -21.48921356237309155, -27.52281430457070499, 5.000000000000000000 ) ) ;
#142631 = CARTESIAN_POINT ( 'NONE',  ( 74.99451991528749772, 28.92564299267990435, 4.000000000000000000 ) ) ;
#142632 = CARTESIAN_POINT ( 'NONE',  ( 27.00000000000000355, 6.349999999999999645, 0.000000000000000000 ) ) ;
#142633 = CARTESIAN_POINT ( 'NONE',  ( 34.12543019189810423, 5.291415217122919401, 3.055000000000002824 ) ) ;
#142634 = CARTESIAN_POINT ( 'NONE',  ( 6.489213562373093325, -27.52281430457059841, 5.000000000000000000 ) ) ;
#142635 = PLANE ( 'NONE',  #23386 ) ;
#142636 = ORIENTED_EDGE ( 'NONE', *, *, #23516, .F. ) ;
#142637 = DIRECTION ( 'NONE',  ( -0.7071067811865486830, 0.7071067811865464625, 0.000000000000000000 ) ) ;
#142638 = ORIENTED_EDGE ( 'NONE', *, *, #103835, .F. ) ;
#142639 = DIRECTION ( 'NONE',  ( 0.000000000000000000, 0.000000000000000000, 1.000000000000000000 ) ) ;
#142640 = ORIENTED_EDGE ( 'NONE', *, *, #113946, .T. ) ;
#142641 = EDGE_CURVE ( 'NONE', #50766, #22876, #13754, .T. ) ;
#142642 = PLANE ( 'NONE',  #143218 ) ;
#142644 = ORIENTED_EDGE ( 'NONE', *, *, #120169, .F. ) ;
#142643 = DIRECTION ( 'NONE',  ( 0.000000000000000000, 0.000000000000000000, 1.000000000000000000 ) ) ;
#142645 = EDGE_CURVE ( 'NONE', #117995, #119169, #35583, .T. ) ;
#142646 = CARTESIAN_POINT ( 'NONE',  ( -71.99451991528749772, 28.92564299267988304, 4.000000000000000000 ) ) ;
#142647 = VERTEX_POINT ( 'NONE', #80493 ) ;
#142648 = DIRECTION ( 'NONE',  ( 0.6830127018922180770, -0.6830127018922204085, -0.2588190451025213501 ) ) ;
#142649 = EDGE_LOOP ( 'NONE', ( #88297, #75510, #97525, #7705 ) ) ;
#142650 = CARTESIAN_POINT ( 'NONE',  ( -19.05000000000000071, 3.174999999999997158, 4.000000000000000000 ) ) ;
#142651 = ORIENTED_EDGE ( 'NONE', *, *, #48723, .F. ) ;
#142652 = EDGE_CURVE ( 'NONE', #35109, #30178, #103622, .T. ) ;
#142653 = ADVANCED_FACE ( 'NONE', ( #4261 ), #1450, .F. ) ;
#142654 = VECTOR ( 'NONE', #71436, 1000.000000000000000 ) ;
#142655 = CARTESIAN_POINT ( 'NONE',  ( 112.5166937171295700, 7.950000000000001066, -2.130196079827421318 ) ) ;
#142656 = PLANE ( 'NONE',  #97086 ) ;
#142657 = CARTESIAN_POINT ( 'NONE',  ( -14.67183060077636370, 20.25929247661551358, 4.000000000000000000 ) ) ;
#142658 = VECTOR ( 'NONE', #114365, 1000.000000000000000 ) ;
#142659 = ADVANCED_FACE ( 'NONE', ( #24653 ), #79812, .F. ) ;
#142660 = DIRECTION ( 'NONE',  ( -0.000000000000000000, -0.3543493200069152693, 0.9351131265310292928 ) ) ;
#142661 = DIRECTION ( 'NONE',  ( -0.000000000000000000, 0.000000000000000000, 1.000000000000000000 ) ) ;
#142662 = CARTESIAN_POINT ( 'NONE',  ( 3.489213562373097322, -27.52281430457057709, 5.000000000000000000 ) ) ;
#142663 = CARTESIAN_POINT ( 'NONE',  ( 1.895833333333333703, 1.633150327867687324, -6.094999999999991758 ) ) ;
#142664 = CARTESIAN_POINT ( 'NONE',  ( 14.99956980810188689, -3.967499999999998028, -6.871911579029511330 ) ) ;
#142665 = LINE ( 'NONE', #119450, #51325 ) ;
#142666 = LINE ( 'NONE', #121605, #142699 ) ;
#142667 = ORIENTED_EDGE ( 'NONE', *, *, #85392, .F. ) ;
#142668 = ORIENTED_EDGE ( 'NONE', *, *, #58339, .F. ) ;
#142669 = EDGE_CURVE ( 'NONE', #123192, #27739, #135585, .T. ) ;
#142670 = CARTESIAN_POINT ( 'NONE',  ( -12.18398860626900060, 28.73617430169795739, 5.000000000000000000 ) ) ;
#142671 = ORIENTED_EDGE ( 'NONE', *, *, #2735, .F. ) ;
#142672 = AXIS2_PLACEMENT_3D ( 'NONE', #114532, #138446, #58799 ) ;
#142673 = DIRECTION ( 'NONE',  ( 0.6830127018922181881, 0.6830127018922202975, -0.2588190451025214056 ) ) ;
#142674 = CARTESIAN_POINT ( 'NONE',  ( 37.60343192894620756, -14.24070752338413293, 19.24067776001734487 ) ) ;
#142675 = DIRECTION ( 'NONE',  ( 0.7071067811865487940, 0.7071067811865463515, -0.000000000000000000 ) ) ;
#142676 = ORIENTED_EDGE ( 'NONE', *, *, #86194, .F. ) ;
#142677 = ADVANCED_FACE ( 'NONE', ( #102945 ), #3590, .T. ) ;
#142678 = DIRECTION ( 'NONE',  ( -0.7071067811865486830, -0.7071067811865464625, 0.000000000000000000 ) ) ;
#142679 = FACE_OUTER_BOUND ( 'NONE', #142862, .T. ) ;
#142680 = LINE ( 'NONE', #43372, #99816 ) ;
#142681 = VECTOR ( 'NONE', #15185, 1000.000000000000000 ) ;
#142683 = ORIENTED_EDGE ( 'NONE', *, *, #25832, .F. ) ;
#142682 = LINE ( 'NONE', #12156, #107663 ) ;
#142684 = CARTESIAN_POINT ( 'NONE',  ( 39.48921356237310221, -27.52281430457082934, 5.000000000000000000 ) ) ;
#142685 = EDGE_CURVE ( 'NONE', #133116, #34514, #18754, .T. ) ;
#142686 =( NAMED_UNIT ( * ) SI_UNIT ( $, .STERADIAN. ) SOLID_ANGLE_UNIT ( ) );
#142687 = CARTESIAN_POINT ( 'NONE',  ( 21.48921356237309155, -27.52281430457070499, 5.000000000000000000 ) ) ;
#142688 = VECTOR ( 'NONE', #26288, 1000.000000000000000 ) ;
#142689 = CARTESIAN_POINT ( 'NONE',  ( 34.47516574401890921, -7.509482387884292898, 4.998110765256834398 ) ) ;
#142690 = AXIS2_PLACEMENT_3D ( 'NONE', #44509, #88711, #132943 ) ;
#142691 = ORIENTED_EDGE ( 'NONE', *, *, #127861, .F. ) ;
#142692 = EDGE_LOOP ( 'NONE', ( #119840, #88208, #35621, #18553 ) ) ;
#142693 = ORIENTED_EDGE ( 'NONE', *, *, #95459, .F. ) ;
#142694 = AXIS2_PLACEMENT_3D ( 'NONE', #87076, #132020, #52292 ) ;
#142695 = CARTESIAN_POINT ( 'NONE',  ( 91.00043019189810423, -3.055000000000002380, 5.291415217122920289 ) ) ;
#142696 = ORIENTED_EDGE ( 'NONE', *, *, #71896, .T. ) ;
#142697 = ADVANCED_FACE ( 'NONE', ( #117348 ), #52118, .T. ) ;
#142698 = CARTESIAN_POINT ( 'NONE',  ( 123.5545056966327451, -44.02090675802679698, 34.92500000000510596 ) ) ;
#142699 = VECTOR ( 'NONE', #31067, 1000.000000000000000 ) ;
#142700 = DIRECTION ( 'NONE',  ( -0.7071067811865486830, -0.7071067811865464625, 0.000000000000000000 ) ) ;
#142701 = EDGE_LOOP ( 'NONE', ( #106315, #128073, #68766, #72916 ) ) ;
#142702 = CARTESIAN_POINT ( 'NONE',  ( 184.0335292699551246, -51.38852430739340349, 37.54101415799218699 ) ) ;
#142703 = LINE ( 'NONE', #42701, #67458 ) ;
#142704 = ADVANCED_FACE ( 'NONE', ( #105069 ), #39850, .F. ) ;
#142705 = EDGE_CURVE ( 'NONE', #28732, #55970, #27491, .T. ) ;
#142706 = CARTESIAN_POINT ( 'NONE',  ( 86.97459685856479439, 1.637169565754164058, -6.109999999999996767 ) ) ;
#142707 = EDGE_LOOP ( 'NONE', ( #14393, #33350, #124804, #80440, #2750, #124134 ) ) ;
#142708 = CARTESIAN_POINT ( 'NONE',  ( -34.17183060077622514, 12.75929247661558641, 4.000000000000000000 ) ) ;
#142709 = CARTESIAN_POINT ( 'NONE',  ( -12.70710678118645554, -0.7407075233842718154, 5.000000000000000000 ) ) ;
#142710 = EDGE_CURVE ( 'NONE', #139710, #66308, #140546, .T. ) ;
#142711 = EDGE_LOOP ( 'NONE', ( #24246, #107229, #81228 ) ) ;
#142712 = ORIENTED_EDGE ( 'NONE', *, *, #110667, .F. ) ;
#142713 = ORIENTED_EDGE ( 'NONE', *, *, #65306, .F. ) ;
#142714 = LINE ( 'NONE', #10047, #125593 ) ;
#142715 = ADVANCED_FACE ( 'NONE', ( #61605 ), #116659, .F. ) ;
#142716 = CARTESIAN_POINT ( 'NONE',  ( -22.95484226663318950, -21.74070752338405299, 21.72585301388579282 ) ) ;
#142717 = CARTESIAN_POINT ( 'NONE',  ( 18.73373647476854842, 5.808823158059035485, 5.808823158059032821 ) ) ;
#142718 = CARTESIAN_POINT ( 'NONE',  ( 20.66840764549667497, 3.061616997868385113E-16, -2.500000000000001332 ) ) ;
#142719 = CARTESIAN_POINT ( 'NONE',  ( 161.1238792263967241, 26.96999999999994202, 34.89931327300447350 ) ) ;
#142720 = CARTESIAN_POINT ( 'NONE',  ( -15.48921356237309510, -27.52281430457066236, 5.000000000000000000 ) ) ;
#142721 = AXIS2_PLACEMENT_3D ( 'NONE', #94787, #71652, #126707 ) ;
#142722 = ORIENTED_EDGE ( 'NONE', *, *, #70092, .T. ) ;
#142723 = ORIENTED_EDGE ( 'NONE', *, *, #26273, .F. ) ;
#142724 = EDGE_CURVE ( 'NONE', #86087, #52679, #71044, .T. ) ;
#142725 = LINE ( 'NONE', #55020, #50285 ) ;
#142726 = ORIENTED_EDGE ( 'NONE', *, *, #21656, .T. ) ;
#142727 = ORIENTED_EDGE ( 'NONE', *, *, #128203, .F. ) ;
#142728 = VECTOR ( 'NONE', #61765, 1000.000000000000114 ) ;
#142729 = ADVANCED_FACE ( 'NONE', ( #72496 ), #138423, .T. ) ;
#142730 =( BOUNDED_CURVE ( )  B_SPLINE_CURVE ( 2, ( #13304, #114754, #36513, #57577, #15429, #69898, #2421, #59034, #103186, #46735, #48116, #81476, #59717 ),
 .UNSPECIFIED., .F., .F. ) 
 B_SPLINE_CURVE_WITH_KNOTS ( ( 3, 2, 2, 2, 2, 2, 3 ),
 ( 0.08333333333332175463, 0.08611111111109912009, 0.08888888888887649942, 0.09166666666665385099, 0.09444444444443121645, 0.09722222222220859578, 0.09999999999998596123 ),
 .UNSPECIFIED. ) 
 CURVE ( )  GEOMETRIC_REPRESENTATION_ITEM ( )  RATIONAL_B_SPLINE_CURVE ( ( 1.000000000000141887, 0.9659258262889263147, 1.000000000000000000, 0.9659258262890683122, 1.000000000000000000, 0.9659258262890683122, 1.000000000000000000, 0.9659258262890683122, 1.000000000000000000, 0.9659258262890683122, 1.000000000000000000, 0.9659258262892406188, 0.9999999999998276934 ) ) 
 REPRESENTATION_ITEM ( '' )  );
#142731 = PLANE ( 'NONE',  #86820 ) ;
#142732 = ORIENTED_EDGE ( 'NONE', *, *, #53845, .F. ) ;
#142733 = CARTESIAN_POINT ( 'NONE',  ( 55.24999999999999289, -9.735942053221458872E-16, 7.950000000000000178 ) ) ;
#142734 = LINE ( 'NONE', #85474, #111017 ) ;
#142735 = DIRECTION ( 'NONE',  ( -0.000000000000000000, 0.3543493200069153248, 0.9351131265310292928 ) ) ;
#142736 = VECTOR ( 'NONE', #37643, 999.9999999999998863 ) ;
#142737 = DIRECTION ( 'NONE',  ( -0.7071067811865486830, -0.7071067811865464625, 0.000000000000000000 ) ) ;
#142738 =( BOUNDED_CURVE ( )  B_SPLINE_CURVE ( 3, ( #98281, #76542, #7672, #75818 ),
 .UNSPECIFIED., .F., .T. ) 
 B_SPLINE_CURVE_WITH_KNOTS ( ( 4, 4 ),
 ( 2.779374508378133601, 4.199602562396796301 ),
 .UNSPECIFIED. ) 
 CURVE ( )  GEOMETRIC_REPRESENTATION_ITEM ( )  RATIONAL_B_SPLINE_CURVE ( ( 1.000000000000000000, 0.8388583629366717087, 0.8388583629366717087, 1.000000000000000000 ) ) 
 REPRESENTATION_ITEM ( '' )  );
#142739 = CARTESIAN_POINT ( 'NONE',  ( -39.29974487139159578, -27.71228299555233576, 4.000000000000000000 ) ) ;
#142740 = EDGE_LOOP ( 'NONE', ( #11632, #47633, #20655 ) ) ;
#142741 = CARTESIAN_POINT ( 'NONE',  ( -23.99451991528749062, 28.92564299267954908, 4.000000000000000000 ) ) ;
#142742 = ORIENTED_EDGE ( 'NONE', *, *, #143059, .T. ) ;
#142743 = PLANE ( 'NONE',  #101280 ) ;
#142744 = VERTEX_POINT ( 'NONE', #83334 ) ;
#142745 = LINE ( 'NONE', #137411, #23846 ) ;
#142746 = VERTEX_POINT ( 'NONE', #127539 ) ;
#142747 = DIRECTION ( 'NONE',  ( -0.6830127018922181881, 0.6830127018922202975, -0.2588190451025214056 ) ) ;
#142748 = ORIENTED_EDGE ( 'NONE', *, *, #42904, .T. ) ;
#142749 = EDGE_LOOP ( 'NONE', ( #96613, #48965, #90908, #92261 ) ) ;
#142750 = ORIENTED_EDGE ( 'NONE', *, *, #77386, .F. ) ;
#142751 = AXIS2_PLACEMENT_3D ( 'NONE', #86431, #40781, #97244 ) ;
#142752 = DIRECTION ( 'NONE',  ( -1.000000000000000000, 0.000000000000000000, 0.000000000000000000 ) ) ;
#142753 = PLANE ( 'NONE',  #100793 ) ;
#142754 = CARTESIAN_POINT ( 'NONE',  ( 60.18398860626900415, 28.73617430169829490, 5.000000000000000000 ) ) ;
#142755 = CARTESIAN_POINT ( 'NONE',  ( 33.29974487139158867, -27.71228299555229313, 4.000000000000000000 ) ) ;
#142756 = VECTOR ( 'NONE', #16268, 999.9999999999998863 ) ;
#142757 = CARTESIAN_POINT ( 'NONE',  ( 123.8129301918981042, -1.637169565754159617, -6.110000000000001208 ) ) ;
#142758 = DIRECTION ( 'NONE',  ( -0.6830127018922181881, 0.6830127018922202975, -0.2588190451025214056 ) ) ;
#142759 = PRODUCT ( 'slotted pan head screw_iso_ISO 1580 - M5 x 25 - 25S', 'slotted pan head screw_iso_ISO 1580 - M5 x 25 - 25S', '', ( #60576 ) ) ;
#142760 = LINE ( 'NONE', #34014, #85273 ) ;
#142761 = CARTESIAN_POINT ( 'NONE',  ( 0.000000000000000000, -30.18000000000009564, 15.92499999999935945 ) ) ;
#142762 = CARTESIAN_POINT ( 'NONE',  ( -13.49999999999990408, -4.533600742197688938, 5.000000000000000000 ) ) ;
#142763 = CARTESIAN_POINT ( 'NONE',  ( -34.92500000000001137, -14.66188269655941490, 18.97781875781096872 ) ) ;
#142764 = CARTESIAN_POINT ( 'NONE',  ( -6.489213562373093325, -27.52281430457059841, 5.000000000000000000 ) ) ;
#142765 = VECTOR ( 'NONE', #44727, 1000.000000000000114 ) ;
#142766 = EDGE_LOOP ( 'NONE', ( #65574, #52376, #23236, #70229 ) ) ;
#142767 = ORIENTED_EDGE ( 'NONE', *, *, #91339, .F. ) ;
#142768 = VERTEX_POINT ( 'NONE', #49998 ) ;
#142769 = CARTESIAN_POINT ( 'NONE',  ( 30.32816939922331656, -12.74070752338415247, 4.000000000000000000 ) ) ;
#142770 = ORIENTED_EDGE ( 'NONE', *, *, #92935, .F. ) ;
#142771 = VERTEX_POINT ( 'NONE', #93489 ) ;
#142772 = LINE ( 'NONE', #133342, #141665 ) ;
#142773 = SURFACE_SIDE_STYLE ('',( #51500 ) ) ;
#142774 = LINE ( 'NONE', #121013, #98825 ) ;
#142775 = VECTOR ( 'NONE', #143239, 1000.000000000000000 ) ;
#142776 = CARTESIAN_POINT ( 'NONE',  ( -13.49999999999991473, 8.319652575858375698, -8.582050562765859425 ) ) ;
#142777 = ORIENTED_EDGE ( 'NONE', *, *, #16648, .T. ) ;
#142778 = CARTESIAN_POINT ( 'NONE',  ( 1.040834085586084257E-14, 17.96639925780208102, 5.000000000000000000 ) ) ;
#142779 = VERTEX_POINT ( 'NONE', #85439 ) ;
#142780 = CIRCLE ( 'NONE', #50190, 0.5000000000000004441 ) ;
#142782 = FILL_AREA_STYLE_COLOUR ( '', #90712 ) ;
#142781 = AXIS2_PLACEMENT_3D ( 'NONE', #70382, #113827, #80513 ) ;
#142783 = CARTESIAN_POINT ( 'NONE',  ( -50.99451991528749062, 28.92564299267973738, 4.000000000000000000 ) ) ;
#142784 = VECTOR ( 'NONE', #91177, 1000.000000000000000 ) ;
#142785 = CARTESIAN_POINT ( 'NONE',  ( 21.94206980810188057, 7.934999999999993392, 2.126176841940951689 ) ) ;
#142786 = ORIENTED_EDGE ( 'NONE', *, *, #65268, .F. ) ;
#142787 = CARTESIAN_POINT ( 'NONE',  ( 89.74543019189812298, -5.291415217122919401, -3.055000000000000604 ) ) ;
#142788 = DIRECTION ( 'NONE',  ( 0.7071067811865486830, -0.7071067811865464625, -0.000000000000000000 ) ) ;
#142789 = FACE_OUTER_BOUND ( 'NONE', #140133, .T. ) ;
#142790 = CARTESIAN_POINT ( 'NONE',  ( 20.51159235450331764, -3.851859888774471706E-31, 2.500000000000001332 ) ) ;
#142791 = ORIENTED_EDGE ( 'NONE', *, *, #15123, .F. ) ;
#142792 = DIRECTION ( 'NONE',  ( 0.000000000000000000, 0.000000000000000000, 1.000000000000000000 ) ) ;
#142793 = ORIENTED_EDGE ( 'NONE', *, *, #19814, .F. ) ;
#142794 = ORIENTED_EDGE ( 'NONE', *, *, #54914, .F. ) ;
#142795 = CARTESIAN_POINT ( 'NONE',  ( 0.000000000000000000, -8.616843969807042924, 4.000000000000000000 ) ) ;
#142796 = AXIS2_PLACEMENT_3D ( 'NONE', #55669, #130374, #110018 ) ;
#142797 = LINE ( 'NONE', #97870, #116825 ) ;
#142798 = LINE ( 'NONE', #7251, #123668 ) ;
#142799 = ORIENTED_EDGE ( 'NONE', *, *, #15469, .T. ) ;
#142800 = DIRECTION ( 'NONE',  ( -1.000000000000000000, -1.224606353822377258E-16, -0.000000000000000000 ) ) ;
#142801 = ADVANCED_FACE ( 'NONE', ( #94181 ), #74379, .T. ) ;
#142802 =( NAMED_UNIT ( * ) SI_UNIT ( $, .STERADIAN. ) SOLID_ANGLE_UNIT ( ) );
#142804 = EDGE_CURVE ( 'NONE', #131546, #25358, #7880, .T. ) ;
#142803 = CARTESIAN_POINT ( 'NONE',  ( 5.125146193092313673, -14.24070752338413293, 9.401115078912647860 ) ) ;
#142805 = EDGE_LOOP ( 'NONE', ( #119726, #117203, #6889, #2814 ) ) ;
#142806 = DIRECTION ( 'NONE',  ( 0.3543493200069162685, -0.000000000000000000, -0.9351131265310288487 ) ) ;
#142807 = DIRECTION ( 'NONE',  ( 0.6830127018922181881, 0.6830127018922202975, -0.2588190451025214056 ) ) ;
#142808 = ORIENTED_EDGE ( 'NONE', *, *, #98334, .T. ) ;
#142809 = EDGE_CURVE ( 'NONE', #68414, #126070, #137723, .T. ) ;
#142811 = ORIENTED_EDGE ( 'NONE', *, *, #70857, .F. ) ;
#142810 = CARTESIAN_POINT ( 'NONE',  ( -21.18398860626899349, 28.73617430169802134, 5.000000000000000000 ) ) ;
#142812 = VERTEX_POINT ( 'NONE', #38398 ) ;
#142813 = ADVANCED_FACE ( 'NONE', ( #16622 ), #128269, .F. ) ;
#142814 = ADVANCED_FACE ( 'NONE', ( #39108 ), #28234, .T. ) ;
#142815 = DIRECTION ( 'NONE',  ( 0.6830127018922180770, -0.6830127018922204085, -0.2588190451025213501 ) ) ;
#142817 = AXIS2_PLACEMENT_3D ( 'NONE', #126195, #82696, #127627 ) ;
#142816 = DIRECTION ( 'NONE',  ( -0.7071067811865486830, 0.7071067811865464625, 0.000000000000000000 ) ) ;
#142818 = EDGE_LOOP ( 'NONE', ( #104034, #128589, #22274, #136682 ) ) ;
#142819 = PLANE ( 'NONE',  #18876 ) ;
#142820 = ADVANCED_FACE ( 'NONE', ( #106460 ), #126806, .F. ) ;
#142821 = EDGE_CURVE ( 'NONE', #7821, #65237, #76760, .T. ) ;
#142822 = LINE ( 'NONE', #87013, #107678 ) ;
#142823 = VECTOR ( 'NONE', #67770, 1000.000000000000000 ) ;
#142824 = CARTESIAN_POINT ( 'NONE',  ( 31.92500000000001492, 9.947201970464227326E-15, -37.00000000000000000 ) ) ;
#142825 = PLANE ( 'NONE',  #27611 ) ;
#142826 = CARTESIAN_POINT ( 'NONE',  ( 0.1600000000000009748, -7.113645484598424495, 3.515717980648092045 ) ) ;
#142827 = EDGE_CURVE ( 'NONE', #57169, #27842, #119488, .T. ) ;
#142828 = DIRECTION ( 'NONE',  ( -1.000000000000000000, -0.000000000000000000, -0.000000000000000000 ) ) ;
#142829 = DIRECTION ( 'NONE',  ( -0.7071067811865486830, 0.7071067811865464625, 0.000000000000000000 ) ) ;
#142830 = DIRECTION ( 'NONE',  ( 0.7071067811865487940, 0.7071067811865463515, 0.000000000000000000 ) ) ;
#142831 = FACE_OUTER_BOUND ( 'NONE', #18187, .T. ) ;
#142833 = PRESENTATION_LAYER_ASSIGNMENT (  '', '', ( #84981 ) ) ;
#142832 = CARTESIAN_POINT ( 'NONE',  ( -19.49999999999986500, -11.94781430457070748, 5.000000000000000000 ) ) ;
#142834 = CARTESIAN_POINT ( 'NONE',  ( 35.99451991528749772, 28.92564299267963079, 4.000000000000000000 ) ) ;
#142835 = EDGE_CURVE ( 'NONE', #10226, #70306, #142703, .T. ) ;
#142836 = PLANE ( 'NONE',  #111321 ) ;
#142837 = DIRECTION ( 'NONE',  ( -0.3543493200069162685, -0.000000000000000000, -0.9351131265310288487 ) ) ;
#142838 = ORIENTED_EDGE ( 'NONE', *, *, #52520, .T. ) ;
#142839 = ORIENTED_EDGE ( 'NONE', *, *, #6036, .F. ) ;
#142841 = ADVANCED_FACE ( 'NONE', ( #44874, #107894 ), #54996, .F. ) ;
#142840 = CARTESIAN_POINT ( 'NONE',  ( 97.10416666666665719, 2.130196079827422206, 7.950000000000001954 ) ) ;
#142842 = VERTEX_POINT ( 'NONE', #87606 ) ;
#142843 = EDGE_LOOP ( 'NONE', ( #90921, #106001, #120350, #61970 ) ) ;
#142844 = VERTEX_POINT ( 'NONE', #21642 ) ;
#142845 = VECTOR ( 'NONE', #18914, 1000.000000000000000 ) ;
#142846 = CARTESIAN_POINT ( 'NONE',  ( -60.48921356237309510, -27.52281430457097500, 5.000000000000000000 ) ) ;
#142847 = DIRECTION ( 'NONE',  ( 0.7071067811865487940, -0.7071067811865463515, 0.000000000000000000 ) ) ;
#142848 = VERTEX_POINT ( 'NONE', #120937 ) ;
#142849 = CARTESIAN_POINT ( 'NONE',  ( -65.99451991528749772, 28.92564299267984396, 4.000000000000000000 ) ) ;
#142851 = VECTOR ( 'NONE', #89934, 999.9999999999998863 ) ;
#142850 = CARTESIAN_POINT ( 'NONE',  ( -13.77325839282158348, -11.24070752338416845, 18.24660765846979515 ) ) ;
#142852 = CARTESIAN_POINT ( 'NONE',  ( -3.299744871391591339, -27.71228299555208352, 4.000000000000000000 ) ) ;
#142853 = VERTEX_POINT ( 'NONE', #76016 ) ;
#142854 = CARTESIAN_POINT ( 'NONE',  ( 6.342232970832937688, 11.40363289190650065, -27.76885313926799626 ) ) ;
#142855 = DIRECTION ( 'NONE',  ( 1.000000000000000000, 0.000000000000000000, 0.000000000000000000 ) ) ;
#142856 = EDGE_CURVE ( 'NONE', #2559, #98151, #130414, .T. ) ;
#142857 = CARTESIAN_POINT ( 'NONE',  ( -11.81601139373100651, 28.73617430169779041, 5.000000000000000000 ) ) ;
#142858 = CARTESIAN_POINT ( 'NONE',  ( 23.18750000000000355, 4.461849672132297329, -4.461849672132302658 ) ) ;
#142859 = CARTESIAN_POINT ( 'NONE',  ( -4.921261423547484970E-16, -0.5999999999999994227, -3.228048788193037755 ) ) ;
#142860 = CARTESIAN_POINT ( 'NONE',  ( 28.51669371712955225, 7.950000000000001066, -2.130196079827421318 ) ) ;
#142861 = CARTESIAN_POINT ( 'NONE',  ( -44.99451991528749772, 28.92564299267969474, 4.000000000000000000 ) ) ;
#142862 = EDGE_LOOP ( 'NONE', ( #70769, #77645, #116293, #116237 ) ) ;
#142863 = ORIENTED_EDGE ( 'NONE', *, *, #108622, .F. ) ;
#142864 = CARTESIAN_POINT ( 'NONE',  ( 116.3754301918981042, -5.291415217122920289, -3.055000000000001492 ) ) ;
#142865 = CIRCLE ( 'NONE', #54817, 2.055000000000000604 ) ;
#142866 = ORIENTED_EDGE ( 'NONE', *, *, #36337, .T. ) ;
#142867 = CARTESIAN_POINT ( 'NONE',  ( -26.18753812416034421, -22.22500000000000142, 4.000000000000000000 ) ) ;
#142868 = EDGE_CURVE ( 'NONE', #80652, #112055, #97763, .T. ) ;
#142869 = CARTESIAN_POINT ( 'NONE',  ( 24.48921356237309510, -27.52281430457072631, 5.000000000000000000 ) ) ;
#142870 = CARTESIAN_POINT ( 'NONE',  ( -34.82816939922328459, -17.24070752338410628, 4.000000000000000000 ) ) ;
#142871 = DIRECTION ( 'NONE',  ( 0.7071067811865486830, -0.7071067811865464625, -0.000000000000000000 ) ) ;
#142872 = PRESENTATION_STYLE_ASSIGNMENT (( #131285 ) ) ;
#142873 = EDGE_CURVE ( 'NONE', #50863, #81209, #43396, .T. ) ;
#142874 = CARTESIAN_POINT ( 'NONE',  ( 111.3287635252314516, 0.000000000000000000, -6.109999999999998543 ) ) ;
#142875 = ORIENTED_EDGE ( 'NONE', *, *, #129670, .T. ) ;
#142876 = EDGE_CURVE ( 'NONE', #136035, #62317, #108600, .T. ) ;
#142877 = ORIENTED_EDGE ( 'NONE', *, *, #61142, .F. ) ;
#142878 = CARTESIAN_POINT ( 'NONE',  ( 70.80836038379624142, 7.949999999999996625, 2.130196079827431088 ) ) ;
#142879 = DIRECTION ( 'NONE',  ( -0.7071067811865486830, -0.7071067811865464625, -0.000000000000000000 ) ) ;
#142880 = EDGE_CURVE ( 'NONE', #13716, #56693, #11435, .T. ) ;
#142881 = ORIENTED_EDGE ( 'NONE', *, *, #99509, .F. ) ;
#142882 = VERTEX_POINT ( 'NONE', #9280 ) ;
#142883 =( GEOMETRIC_REPRESENTATION_CONTEXT ( 3 ) GLOBAL_UNCERTAINTY_ASSIGNED_CONTEXT ( ( #138754 ) ) GLOBAL_UNIT_ASSIGNED_CONTEXT ( ( #36118, #25942, #101348 ) ) REPRESENTATION_CONTEXT ( 'NONE', 'WORKASPACE' ) );
#142884 = CARTESIAN_POINT ( 'NONE',  ( 36.60459685856475431, 1.637169565754164946, -6.109999999999999432 ) ) ;
#142885 = VERTEX_POINT ( 'NONE', #141258 ) ;
#142886 = LINE ( 'NONE', #63913, #137386 ) ;
#142887 = CARTESIAN_POINT ( 'NONE',  ( 0.000000000000000000, 0.000000000000000000, 0.000000000000000000 ) ) ;
#142888 = DIRECTION ( 'NONE',  ( -0.7071067811865486830, -0.7071067811865464625, 0.000000000000000000 ) ) ;
#142889 = EDGE_CURVE ( 'NONE', #118345, #26318, #30364, .T. ) ;
#142890 = VECTOR ( 'NONE', #87736, 999.9999999999998863 ) ;
#142891 = VECTOR ( 'NONE', #4117, 1000.000000000000000 ) ;
#142892 = CONICAL_SURFACE ( 'NONE', #57237, 2.055000000000001048, 0.9599310885968758145 ) ;
#142893 = CARTESIAN_POINT ( 'NONE',  ( 38.84959685856477307, 6.109999999999996767, 1.637169565754163836 ) ) ;
#142894 = ORIENTED_EDGE ( 'NONE', *, *, #132764, .F. ) ;
#142895 = EDGE_CURVE ( 'NONE', #9148, #29128, #65893, .T. ) ;
#142896 = LINE ( 'NONE', #66769, #75736 ) ;
#142897 = ORIENTED_EDGE ( 'NONE', *, *, #38638, .F. ) ;
#142898 = EDGE_LOOP ( 'NONE', ( #28621, #47296, #36960 ) ) ;
#142899 = VECTOR ( 'NONE', #40883, 1000.000000000000000 ) ;
#142900 = EDGE_LOOP ( 'NONE', ( #56481, #101577, #69617, #68980, #27276 ) ) ;
#142901 = DIRECTION ( 'NONE',  ( -0.7071067811865486830, -0.7071067811865464625, 0.000000000000000000 ) ) ;
#142902 = ORIENTED_EDGE ( 'NONE', *, *, #45682, .F. ) ;
#142903 = DIRECTION ( 'NONE',  ( 1.000000000000000000, 1.224606353822377258E-16, 0.000000000000000000 ) ) ;
#142904 = CARTESIAN_POINT ( 'NONE',  ( 72.48921356237309510, -27.52281430457106026, 5.000000000000000000 ) ) ;
#142905 = FACE_OUTER_BOUND ( 'NONE', #79577, .T. ) ;
#142906 = PLANE ( 'NONE',  #32706 ) ;
#142907 = EDGE_CURVE ( 'NONE', #55557, #92449, #84715, .T. ) ;
#142908 = FACE_BOUND ( 'NONE', #4341, .T. ) ;
#142909 = ORIENTED_EDGE ( 'NONE', *, *, #104244, .T. ) ;
#142910 = CARTESIAN_POINT ( 'NONE',  ( -54.18398860626899705, 28.73617430169825226, 5.000000000000000000 ) ) ;
#142911 = DIRECTION ( 'NONE',  ( -0.6830127018922180770, -0.6830127018922204085, -0.2588190451025213501 ) ) ;
#142912 = LINE ( 'NONE', #43597, #2210 ) ;
#142913 = ORIENTED_EDGE ( 'NONE', *, *, #70324, .T. ) ;
#142914 = DIRECTION ( 'NONE',  ( 0.6830127018922180770, -0.6830127018922204085, -0.2588190451025213501 ) ) ;
#142915 = VERTEX_POINT ( 'NONE', #22311 ) ;
#142916 = VECTOR ( 'NONE', #51858, 1000.000000000000227 ) ;
#142917 = ORIENTED_EDGE ( 'NONE', *, *, #42385, .F. ) ;
#142918 = DIRECTION ( 'NONE',  ( -0.3543493200069162685, -0.000000000000000000, -0.9351131265310288487 ) ) ;
#142919 =( BOUNDED_CURVE ( )  B_SPLINE_CURVE ( 3, ( #84627, #128828, #61481, #136855 ),
 .UNSPECIFIED., .F., .T. ) 
 B_SPLINE_CURVE_WITH_KNOTS ( ( 4, 4 ),
 ( 1.864375635226908301, 1.933014472006540752 ),
 .UNSPECIFIED. ) 
 CURVE ( )  GEOMETRIC_REPRESENTATION_ITEM ( )  RATIONAL_B_SPLINE_CURVE ( ( 1.000000000000000000, 0.9996074310407762065, 0.9996074310407762065, 1.000000000000000000 ) ) 
 REPRESENTATION_ITEM ( '' )  );
#142920 = VERTEX_POINT ( 'NONE', #66582 ) ;
#142921 = CARTESIAN_POINT ( 'NONE',  ( 46.87043019189811588, -3.055000000000001492, 5.291415217122917625 ) ) ;
#142922 = COLOUR_RGB ( '', 0.09019608, 0.27058824, 0.51372549) ;
#142923 = ORIENTED_EDGE ( 'NONE', *, *, #38896, .F. ) ;
#142924 = CARTESIAN_POINT ( 'NONE',  ( -39.29974487139159578, -27.71228299555233576, 4.000000000000000000 ) ) ;
#142925 = CARTESIAN_POINT ( 'NONE',  ( 18.29974487139159223, -27.71228299555219010, 4.000000000000000000 ) ) ;
#142926 = DIRECTION ( 'NONE',  ( -1.000000000000000000, 0.000000000000000000, 0.000000000000000000 ) ) ;
#142927 = EDGE_LOOP ( 'NONE', ( #46648, #81840, #33714, #89826 ) ) ;
#142928 = LINE ( 'NONE', #98698, #86203 ) ;
#142929 = LINE ( 'NONE', #32027, #96718 ) ;
#142930 = VECTOR ( 'NONE', #93310, 1000.000000000000000 ) ;
#142931 = EDGE_CURVE ( 'NONE', #102772, #85411, #19488, .T. ) ;
#142932 = ADVANCED_FACE ( 'NONE', ( #52808 ), #97005, .F. ) ;
#142933 = DIRECTION ( 'NONE',  ( -0.6830127018922180770, -0.6830127018922204085, -0.2588190451025213501 ) ) ;
#142934 = DIRECTION ( 'NONE',  ( -0.000000000000000000, -0.3543493200069152693, 0.9351131265310292928 ) ) ;
#142935 = CARTESIAN_POINT ( 'NONE',  ( -8.510786437626906675, -27.52281430457049183, 5.000000000000000000 ) ) ;
#142936 = LINE ( 'NONE', #132082, #4653 ) ;
#142937 = ORIENTED_EDGE ( 'NONE', *, *, #16118, .F. ) ;
#142938 = ORIENTED_EDGE ( 'NONE', *, *, #123722, .T. ) ;
#142939 = VERTEX_POINT ( 'NONE', #89057 ) ;
#142940 = CARTESIAN_POINT ( 'NONE',  ( 18.48921356237309510, -27.52281430457068367, 5.000000000000000000 ) ) ;
#142941 = CARTESIAN_POINT ( 'NONE',  ( -29.99451991528749417, 28.92564299267958816, 4.000000000000000000 ) ) ;
#142942 = ORIENTED_EDGE ( 'NONE', *, *, #127215, .F. ) ;
#142943 = ORIENTED_EDGE ( 'NONE', *, *, #128187, .T. ) ;
#142944 = DIRECTION ( 'NONE',  ( -0.000000000000000000, 0.000000000000000000, 1.000000000000000000 ) ) ;
#142945 = EDGE_CURVE ( 'NONE', #22423, #40143, #12881, .T. ) ;
#142946 = CARTESIAN_POINT ( 'NONE',  ( 62.99451991528749772, 28.92564299267982264, 4.000000000000000000 ) ) ;
#142947 = ORIENTED_EDGE ( 'NONE', *, *, #118928, .F. ) ;
#142948 = CARTESIAN_POINT ( 'NONE',  ( -20.99999999999985789, 18.08204922493371214, 0.9627537363045357566 ) ) ;
#142949 = CARTESIAN_POINT ( 'NONE',  ( -21.48921356237309155, -27.52281430457070499, 5.000000000000000000 ) ) ;
#142950 = CARTESIAN_POINT ( 'NONE',  ( 20.33790314143522338, -6.871911579029513106, -3.967499999999993587 ) ) ;
#142951 = DIRECTION ( 'NONE',  ( 0.6830127018922180770, -0.6830127018922204085, -0.2588190451025213501 ) ) ;
#142952 = ORIENTED_EDGE ( 'NONE', *, *, #2178, .F. ) ;
#142953 = CARTESIAN_POINT ( 'NONE',  ( 116.7245968585647660, -1.637169565754161171, 6.109999999999998543 ) ) ;
#142954 =( GEOMETRIC_REPRESENTATION_CONTEXT ( 3 ) GLOBAL_UNCERTAINTY_ASSIGNED_CONTEXT ( ( #24273 ) ) GLOBAL_UNIT_ASSIGNED_CONTEXT ( ( #31307, #97225, #130639 ) ) REPRESENTATION_CONTEXT ( 'NONE', 'WORKASPACE' ) );
#142955 = DIRECTION ( 'NONE',  ( -0.7071067811865486830, -0.7071067811865464625, 0.000000000000000000 ) ) ;
#142956 = CARTESIAN_POINT ( 'NONE',  ( -16.43312800248732586, -21.74070752338406365, 6.915939825044111089 ) ) ;
#142958 = ORIENTED_EDGE ( 'NONE', *, *, #11186, .T. ) ;
#142957 = PLANE ( 'NONE',  #139801 ) ;
#142959 = DIRECTION ( 'NONE',  ( -0.6830127018922180770, -0.6830127018922204085, -0.2588190451025213501 ) ) ;
#142960 = VERTEX_POINT ( 'NONE', #122349 ) ;
#142961 = SURFACE_SIDE_STYLE ('',( #838 ) ) ;
#142962 = PLANE ( 'NONE',  #132640 ) ;
#142963 = CARTESIAN_POINT ( 'NONE',  ( 20.56494995367816614, -2.598550695876024275, 5.000000000000000000 ) ) ;
#142964 = ORIENTED_EDGE ( 'NONE', *, *, #79105, .T. ) ;
#142965 = AXIS2_PLACEMENT_3D ( 'NONE', #74944, #50318, #40863 ) ;
#142966 = LINE ( 'NONE', #128540, #30264 ) ;
#142967 = CARTESIAN_POINT ( 'NONE',  ( -34.47516574401891631, 21.02806734111560516, 4.998110765256836174 ) ) ;
#142968 = ORIENTED_EDGE ( 'NONE', *, *, #119908, .T. ) ;
#142969 = CARTESIAN_POINT ( 'NONE',  ( 13.17183060077638324, -5.240707523384225297, 4.000000000000000000 ) ) ;
#142970 = TOROIDAL_SURFACE ( 'NONE', #18244, 6.000000000000000000, 3.000000000000000000 ) ;
#142972 = EDGE_CURVE ( 'NONE', #102502, #100766, #101334, .T. ) ;
#142971 = CARTESIAN_POINT ( 'NONE',  ( 10.77958563595370833, 4.584330080086930965E-16, 0.000000000000000000 ) ) ;
#142973 = ORIENTED_EDGE ( 'NONE', *, *, #94322, .T. ) ;
#142974 = MECHANICAL_DESIGN_GEOMETRIC_PRESENTATION_REPRESENTATION (  '', ( #52724 ), #75836 ) ;
#142975 = CARTESIAN_POINT ( 'NONE',  ( 0.000000000000000000, 0.000000000000000000, -10.00000000000000000 ) ) ;
#142977 = VERTEX_POINT ( 'NONE', #136102 ) ;
#142976 = FACE_OUTER_BOUND ( 'NONE', #108430, .T. ) ;
#142978 = EDGE_CURVE ( 'NONE', #16368, #1674, #36103, .T. ) ;
#142979 = ORIENTED_EDGE ( 'NONE', *, *, #76203, .T. ) ;
#142980 = CARTESIAN_POINT ( 'NONE',  ( -9.888376381052353281, 9.759292476615614831, 17.35367589129214849 ) ) ;
#142981 = CARTESIAN_POINT ( 'NONE',  ( 12.19999999999999574, 0.000000000000000000, -40.00000000000000000 ) ) ;
#142982 = AXIS2_PLACEMENT_3D ( 'NONE', #105113, #137765, #94933 ) ;
#142983 = ORIENTED_EDGE ( 'NONE', *, *, #46571, .F. ) ;
#142984 = AXIS2_PLACEMENT_3D ( 'NONE', #120405, #122575, #132791 ) ;
#142985 = DIRECTION ( 'NONE',  ( 1.369518533665900312E-16, -1.000000000000000000, 0.000000000000000000 ) ) ;
#142986 = ADVANCED_FACE ( 'NONE', ( #1284 ), #35065, .T. ) ;
#142988 = ADVANCED_FACE ( 'NONE', ( #78174 ), #81032, .F. ) ;
#142987 = AXIS2_PLACEMENT_3D ( 'NONE', #10724, #9277, #143405 ) ;
#142989 = LINE ( 'NONE', #87184, #92357 ) ;
#142990 = CARTESIAN_POINT ( 'NONE',  ( -2.758305415748111944, 0.7592924766157069794, 14.37146558664983331 ) ) ;
#142991 = EDGE_CURVE ( 'NONE', #7775, #64329, #36784, .T. ) ;
#142992 = ORIENTED_EDGE ( 'NONE', *, *, #33053, .F. ) ;
#142993 = CARTESIAN_POINT ( 'NONE',  ( -33.18398860626899705, 28.73617430169810305, 5.000000000000000000 ) ) ;
#142994 = EDGE_CURVE ( 'NONE', #54350, #27936, #25921, .T. ) ;
#142995 = PLANE ( 'NONE',  #102271 ) ;
#142996 = DIRECTION ( 'NONE',  ( -0.000000000000000000, 0.3543493200069153248, 0.9351131265310292928 ) ) ;
#142997 = VECTOR ( 'NONE', #37523, 1000.000000000000000 ) ;
#142998 = CARTESIAN_POINT ( 'NONE',  ( -7.940000000000007496, -60.26999999999998892, -10.00000000000000178 ) ) ;
#142999 = EDGE_CURVE ( 'NONE', #8528, #69641, #91880, .T. ) ;
#143000 = CARTESIAN_POINT ( 'NONE',  ( 40.89126352523144448, -4.472830434245839371, -4.472830434245839371 ) ) ;
#143001 = PLANE ( 'NONE',  #30304 ) ;
#143002 = EDGE_LOOP ( 'NONE', ( #122985, #49035, #51001, #124993, #78472 ) ) ;
#143003 = ORIENTED_EDGE ( 'NONE', *, *, #122261, .F. ) ;
#143005 = ADVANCED_FACE ( 'NONE', ( #134711 ), #70189, .F. ) ;
#143004 = CARTESIAN_POINT ( 'NONE',  ( 126.2708333333333286, -7.949999999999999289, -2.130196079827426203 ) ) ;
#143006 = ORIENTED_EDGE ( 'NONE', *, *, #102272, .T. ) ;
#143007 = ORIENTED_EDGE ( 'NONE', *, *, #91941, .F. ) ;
#143008 = LINE ( 'NONE', #87908, #1545 ) ;
#143009 = FACE_OUTER_BOUND ( 'NONE', #62306, .T. ) ;
#143010 = EDGE_LOOP ( 'NONE', ( #79227, #55384, #26534, #112032 ) ) ;
#143011 = CARTESIAN_POINT ( 'NONE',  ( 0.2569208697893813897, 0.3999999999999995781, 2.015694669338588429 ) ) ;
#143012 = CARTESIAN_POINT ( 'NONE',  ( 17.99451991528748351, 28.92564299267950645, 4.000000000000000000 ) ) ;
#143013 = ADVANCED_FACE ( 'NONE', ( #68738 ), #23026, .F. ) ;
#143014 = PLANE ( 'NONE',  #76509 ) ;
#143015 = EDGE_CURVE ( 'NONE', #25993, #104365, #67299, .T. ) ;
#143016 = DIRECTION ( 'NONE',  ( -0.7071067811865486830, -0.7071067811865464625, 0.000000000000000000 ) ) ;
#143017 = CARTESIAN_POINT ( 'NONE',  ( 120.8962635252314186, 4.472830434245840259, -4.472830434245839371 ) ) ;
#143018 = EDGE_LOOP ( 'NONE', ( #25377, #136105, #123299, #87471 ) ) ;
#143019 = DIRECTION ( 'NONE',  ( -1.000000000000000000, -0.000000000000000000, -0.000000000000000000 ) ) ;
#143020 = DIRECTION ( 'NONE',  ( -1.000000000000000000, -0.000000000000000000, -0.000000000000000000 ) ) ;
#143021 = AXIS2_PLACEMENT_3D ( 'NONE', #58107, #123345, #113135 ) ;
#143022 = DIRECTION ( 'NONE',  ( -0.7071067811865487940, 0.7071067811865463515, -0.000000000000000000 ) ) ;
#143023 = FACE_OUTER_BOUND ( 'NONE', #105480, .T. ) ;
#143024 = DIRECTION ( 'NONE',  ( 0.7071067811865487940, 0.7071067811865463515, 0.000000000000000000 ) ) ;
#143025 = EDGE_CURVE ( 'NONE', #142433, #91556, #102781, .T. ) ;
#143026 = LINE ( 'NONE', #55318, #95432 ) ;
#143027 = CARTESIAN_POINT ( 'NONE',  ( -25.39999999999996305, 3.061616997868383141E-16, -2.500000000000000000 ) ) ;
#143028 = CARTESIAN_POINT ( 'NONE',  ( 53.16252705046288440, 7.949999999999998401, 1.460391307983218338E-15 ) ) ;
#143029 = CARTESIAN_POINT ( 'NONE',  ( 20.99999999999983658, -16.02097659208071079, -11.96015758381214056 ) ) ;
#143030 = MECHANICAL_DESIGN_GEOMETRIC_PRESENTATION_REPRESENTATION (  '', ( #36542 ), #80542 ) ;
#143031 = CARTESIAN_POINT ( 'NONE',  ( -39.29974487139159578, -27.71228299555233576, 4.000000000000000000 ) ) ;
#143032 = ORIENTED_EDGE ( 'NONE', *, *, #138710, .F. ) ;
#143033 = EDGE_LOOP ( 'NONE', ( #63903, #82331, #93692, #133576 ) ) ;
#143034 = CARTESIAN_POINT ( 'NONE',  ( 43.14583333333332860, 2.130196079827431976, -7.949999999999999289 ) ) ;
#143035 = CARTESIAN_POINT ( 'NONE',  ( 33.32816939922329169, 5.259292476615674339, 4.000000000000000000 ) ) ;
#143036 = LINE ( 'NONE', #11056, #15975 ) ;
#143037 = ORIENTED_EDGE ( 'NONE', *, *, #129091, .T. ) ;
#143038 = CARTESIAN_POINT ( 'NONE',  ( -12.18398860626900060, 28.73617430169795739, 5.000000000000000000 ) ) ;
#143039 = CARTESIAN_POINT ( 'NONE',  ( -2.277185695429367662, -21.72499999999999432, 5.000000000000000000 ) ) ;
#143040 = CARTESIAN_POINT ( 'NONE',  ( 46.22959685856476852, -6.110000000000000320, -1.637169565754161393 ) ) ;
#143041 = ORIENTED_EDGE ( 'NONE', *, *, #137581, .F. ) ;
#143042 = EDGE_CURVE ( 'NONE', #10046, #143231, #103458, .T. ) ;
#143043 = ORIENTED_EDGE ( 'NONE', *, *, #67931, .F. ) ;
#143044 = ORIENTED_EDGE ( 'NONE', *, *, #16948, .T. ) ;
#143045 = DIRECTION ( 'NONE',  ( -0.3543493200069162685, -0.000000000000000000, -0.9351131265310288487 ) ) ;
#143046 = CARTESIAN_POINT ( 'NONE',  ( 18.24525979340076276, 9.091288135747575438, 4.682346157478786353 ) ) ;
#143047 = DIRECTION ( 'NONE',  ( -1.000000000000000000, 0.000000000000000000, 0.000000000000000000 ) ) ;
#143048 = PRESENTATION_STYLE_ASSIGNMENT (( #85095 ) ) ;
#143049 = ORIENTED_EDGE ( 'NONE', *, *, #67272, .F. ) ;
#143050 = CARTESIAN_POINT ( 'NONE',  ( 63.48921356237309510, -27.52281430457099631, 5.000000000000000000 ) ) ;
#143052 = ORIENTED_EDGE ( 'NONE', *, *, #60920, .F. ) ;
#143051 = DIRECTION ( 'NONE',  ( -1.000000000000000000, -1.224606353822377258E-16, -0.000000000000000000 ) ) ;
#143053 = CARTESIAN_POINT ( 'NONE',  ( 78.16709685856476142, -3.055000000000000160, -5.291415217122921177 ) ) ;
#143054 = CARTESIAN_POINT ( 'NONE',  ( 15.60416666666666607, -1.633150327867691765, -6.094999999999989093 ) ) ;
#143055 = DIRECTION ( 'NONE',  ( -1.000000000000000000, 0.000000000000000000, 0.000000000000000000 ) ) ;
#143056 = LINE ( 'NONE', #32158, #53852 ) ;
#143057 = LINE ( 'NONE', #87256, #41648 ) ;
#143058 = CYLINDRICAL_SURFACE ( 'NONE', #106392, 28.00000000000001776 ) ;
#143059 = EDGE_CURVE ( 'NONE', #123911, #63022, #57161, .T. ) ;
#143060 = ORIENTED_EDGE ( 'NONE', *, *, #68552, .T. ) ;
#143061 = AXIS2_PLACEMENT_3D ( 'NONE', #102982, #50037, #3618 ) ;
#143062 = CARTESIAN_POINT ( 'NONE',  ( 88.01669371712955581, 7.950000000000000178, -2.130196079827421318 ) ) ;
#143063 = CARTESIAN_POINT ( 'NONE',  ( 69.47459685856475176, 1.637169565754164058, -6.109999999999996767 ) ) ;
#143064 = DIRECTION ( 'NONE',  ( 0.000000000000000000, 1.000000000000000000, 0.000000000000000000 ) ) ;
#143065 = EDGE_CURVE ( 'NONE', #20150, #34692, #133277, .T. ) ;
#143066 = DIRECTION ( 'NONE',  ( -0.000000000000000000, 0.3543493200069153248, 0.9351131265310292928 ) ) ;
#143067 = FACE_OUTER_BOUND ( 'NONE', #59531, .T. ) ;
#143068 = ORIENTED_EDGE ( 'NONE', *, *, #66473, .F. ) ;
#143069 = ORIENTED_EDGE ( 'NONE', *, *, #107656, .F. ) ;
#143070 = LINE ( 'NONE', #119854, #134882 ) ;
#143071 = DIRECTION ( 'NONE',  ( -0.6830127018922181881, 0.6830127018922202975, -0.2588190451025214056 ) ) ;
#143072 = ORIENTED_EDGE ( 'NONE', *, *, #75932, .F. ) ;
#143073 = ORIENTED_EDGE ( 'NONE', *, *, #141979, .F. ) ;
#143074 = CIRCLE ( 'NONE', #87506, 2.500000000000000888 ) ;
#143075 = EDGE_CURVE ( 'NONE', #83238, #43157, #79650, .T. ) ;
#143076 = CARTESIAN_POINT ( 'NONE',  ( -42.18398860626899705, 28.73617430169816700, 5.000000000000000000 ) ) ;
#143077 = ORIENTED_EDGE ( 'NONE', *, *, #106005, .T. ) ;
#143078 = LINE ( 'NONE', #77831, #137175 ) ;
#143079 = CARTESIAN_POINT ( 'NONE',  ( -2.000000000000000000, 2.375000000000000000, 1.069999999999998508 ) ) ;
#143080 = VECTOR ( 'NONE', #98904, 999.9999999999998863 ) ;
#143081 = CARTESIAN_POINT ( 'NONE',  ( -11.99999999999993427, -22.22500000000000142, 4.412002311789994913 ) ) ;
#143082 = AXIS2_PLACEMENT_3D ( 'NONE', #143088, #107595, #108273 ) ;
#143083 = EDGE_CURVE ( 'NONE', #94901, #83408, #24486, .T. ) ;
#143084 = FACE_BOUND ( 'NONE', #104160, .T. ) ;
#143085 = CARTESIAN_POINT ( 'NONE',  ( 24.21271579574130683, 0.1791150535437372460, 5.000000000000000000 ) ) ;
#143086 = DIRECTION ( 'NONE',  ( -0.7071067811865487940, 0.7071067811865463515, -0.000000000000000000 ) ) ;
#143087 = DIRECTION ( 'NONE',  ( 0.7071067811865486830, -0.7071067811865464625, -0.000000000000000000 ) ) ;
#143089 = VERTEX_POINT ( 'NONE', #135423 ) ;
#143088 = CARTESIAN_POINT ( 'NONE',  ( 15.48921356237309510, -27.52281430457066236, 5.000000000000000000 ) ) ;
#143090 = VECTOR ( 'NONE', #15919, 999.9999999999998863 ) ;
#143091 = CARTESIAN_POINT ( 'NONE',  ( -6.792893218813405909, 18.75929247661552779, 5.000000000000000000 ) ) ;
#143092 = ORIENTED_EDGE ( 'NONE', *, *, #109144, .T. ) ;
#143093 = EDGE_CURVE ( 'NONE', #35075, #132490, #17186, .T. ) ;
#143094 = VERTEX_POINT ( 'NONE', #138254 ) ;
#143095 = CARTESIAN_POINT ( 'NONE',  ( 73.70376352523145158, 6.109999999999998543, 1.122388791418548911E-15 ) ) ;
#143096 = VERTEX_POINT ( 'NONE', #95446 ) ;
#143097 = DIRECTION ( 'NONE',  ( 0.7071067811865487940, 0.7071067811865463515, -0.000000000000000000 ) ) ;
#143098 = CARTESIAN_POINT ( 'NONE',  ( 5.999999999999950262, -10.77435723561694836, -9.972017380717245416 ) ) ;
#143099 = ORIENTED_EDGE ( 'NONE', *, *, #137597, .T. ) ;
#143100 = LINE ( 'NONE', #55395, #118471 ) ;
#143101 = ADVANCED_FACE ( 'NONE', ( #18573 ), #138977, .F. ) ;
#143102 = LINE ( 'NONE', #7570, #17067 ) ;
#143103 = DIRECTION ( 'NONE',  ( -0.7071067811865487940, 0.7071067811865463515, -0.000000000000000000 ) ) ;
#143104 = EDGE_CURVE ( 'NONE', #137546, #86438, #82452, .T. ) ;
#143105 = CARTESIAN_POINT ( 'NONE',  ( -5.816011393731002066, 28.73617430169783304, 5.000000000000000000 ) ) ;
#143106 = FACE_OUTER_BOUND ( 'NONE', #58038, .T. ) ;
#143107 = DIRECTION ( 'NONE',  ( -1.000000000000000000, -1.224606353822377258E-16, -0.000000000000000000 ) ) ;
#143108 = LINE ( 'NONE', #107614, #46983 ) ;
#143109 = PLANE ( 'NONE',  #92551 ) ;
#143110 = VERTEX_POINT ( 'NONE', #106290 ) ;
#143111 = CARTESIAN_POINT ( 'NONE',  ( -36.48921356237310221, -27.52281430457080802, 5.000000000000000000 ) ) ;
#143112 = VERTEX_POINT ( 'NONE', #15703 ) ;
#143113 = CARTESIAN_POINT ( 'NONE',  ( 18.17159235450331778, 9.902892378096218942E-16, 0.000000000000000000 ) ) ;
#143114 = VECTOR ( 'NONE', #119777, 1000.000000000000000 ) ;
#143115 = ORIENTED_EDGE ( 'NONE', *, *, #84357, .F. ) ;
#143116 = ORIENTED_EDGE ( 'NONE', *, *, #39651, .F. ) ;
#143117 = EDGE_CURVE ( 'NONE', #5092, #60214, #40390, .T. ) ;
#143118 = PLANE ( 'NONE',  #25292 ) ;
#143119 = AXIS2_PLACEMENT_3D ( 'NONE', #61320, #31325, #53804 ) ;
#143120 = ORIENTED_EDGE ( 'NONE', *, *, #85186, .F. ) ;
#143121 = CARTESIAN_POINT ( 'NONE',  ( -8.999999999999934275, -21.03360074219752462, 5.000000000000000000 ) ) ;
#143122 = LINE ( 'NONE', #122067, #19192 ) ;
#143123 = CARTESIAN_POINT ( 'NONE',  ( 24.39997294953710139, 4.461849672132297329, -4.461849672132302658 ) ) ;
#143124 = CARTESIAN_POINT ( 'NONE',  ( -2.205225646411241414, 13.66209448022662443, -24.43382165111117033 ) ) ;
#143125 = VERTEX_POINT ( 'NONE', #26632 ) ;
#143126 = DIRECTION ( 'NONE',  ( 0.7071067811865487940, -0.7071067811865463515, 0.000000000000000000 ) ) ;
#143127 = EDGE_LOOP ( 'NONE', ( #129665, #142423, #22858, #137958, #12149 ) ) ;
#143128 = FILL_AREA_STYLE ('',( #130857 ) ) ;
#143129 = DIRECTION ( 'NONE',  ( -1.000000000000000000, -1.224606353822377258E-16, -0.000000000000000000 ) ) ;
#143130 = VECTOR ( 'NONE', #133329, 1000.000000000000227 ) ;
#143132 = VERTEX_POINT ( 'NONE', #94013 ) ;
#143131 = CARTESIAN_POINT ( 'NONE',  ( 34.45011844616453800, 18.00230414159375059, 5.000000000000001776 ) ) ;
#143133 = VERTEX_POINT ( 'NONE', #73705 ) ;
#143134 = PLANE ( 'NONE',  #132998 ) ;
#143135 =( BOUNDED_CURVE ( )  B_SPLINE_CURVE ( 3, ( #100774, #46439, #56608, #122507 ),
 .UNSPECIFIED., .F., .F. ) 
 B_SPLINE_CURVE_WITH_KNOTS ( ( 4, 4 ),
 ( 1.975938068165229655, 2.025325302527092308 ),
 .UNSPECIFIED. ) 
 CURVE ( )  GEOMETRIC_REPRESENTATION_ITEM ( )  RATIONAL_B_SPLINE_CURVE ( ( 1.000000000000000000, 0.9997967520851089862, 0.9997967520851089862, 1.000000000000000000 ) ) 
 REPRESENTATION_ITEM ( '' )  );
#143136 = CARTESIAN_POINT ( 'NONE',  ( 21.48921356237309155, -27.52281430457070499, 5.000000000000000000 ) ) ;
#143137 = DIRECTION ( 'NONE',  ( 0.7071067811865487940, 0.7071067811865463515, 0.000000000000000000 ) ) ;
#143138 = EDGE_LOOP ( 'NONE', ( #113098, #118934, #34656, #67760 ) ) ;
#143139 = CARTESIAN_POINT ( 'NONE',  ( 109.7458603837962272, 3.974999999999996980, 6.884901960086287964 ) ) ;
#143140 = VERTEX_POINT ( 'NONE', #137548 ) ;
#143141 = VERTEX_POINT ( 'NONE', #126636 ) ;
#143142 = LINE ( 'NONE', #108332, #84283 ) ;
#143143 = PLANE ( 'NONE',  #104231 ) ;
#143144 = CARTESIAN_POINT ( 'NONE',  ( -20.99999999999985079, -10.44781430457071991, 5.000000000000000000 ) ) ;
#143145 = DIRECTION ( 'NONE',  ( -0.3543493200069162685, -0.000000000000000000, -0.9351131265310288487 ) ) ;
#143146 = LINE ( 'NONE', #1022, #90823 ) ;
#143147 = DIRECTION ( 'NONE',  ( 0.3543493200069162685, -0.000000000000000000, -0.9351131265310288487 ) ) ;
#143148 = DIRECTION ( 'NONE',  ( 0.7071067811865486830, -0.7071067811865464625, -0.000000000000000000 ) ) ;
#143149 = ORIENTED_EDGE ( 'NONE', *, *, #72165, .T. ) ;
#143150 = LINE ( 'NONE', #66328, #39683 ) ;
#143151 = EDGE_LOOP ( 'NONE', ( #118124, #103051, #104724, #122377 ) ) ;
#143152 = LINE ( 'NONE', #9779, #67926 ) ;
#143153 = DIRECTION ( 'NONE',  ( -1.000000000000000000, -0.000000000000000000, -0.000000000000000000 ) ) ;
#143154 = CARTESIAN_POINT ( 'NONE',  ( 42.48921356237308800, -27.52281430457085065, 5.000000000000000000 ) ) ;
#143155 = EDGE_CURVE ( 'NONE', #10755, #107195, #136817, .T. ) ;
#143156 = ORIENTED_EDGE ( 'NONE', *, *, #21128, .F. ) ;
#143157 = CARTESIAN_POINT ( 'NONE',  ( -8.816011393731004731, 28.73617430169781173, 5.000000000000000000 ) ) ;
#143158 = VECTOR ( 'NONE', #44552, 1000.000000000000000 ) ;
#143159 = CARTESIAN_POINT ( 'NONE',  ( 0.5685132242927009028, 2.500000000000000888, 0.000000000000000000 ) ) ;
#143160 = CARTESIAN_POINT ( 'NONE',  ( 26.90840764549667696, 9.139736423841732040E-16, 0.000000000000000000 ) ) ;
#143161 = EDGE_LOOP ( 'NONE', ( #16768, #127081, #98693, #70741 ) ) ;
#143162 = EDGE_CURVE ( 'NONE', #129256, #36084, #62130, .T. ) ;
#143163 = ORIENTED_EDGE ( 'NONE', *, *, #35912, .T. ) ;
#143164 = DIRECTION ( 'NONE',  ( -0.000000000000000000, 0.3543493200069153248, 0.9351131265310292928 ) ) ;
#143165 = CARTESIAN_POINT ( 'NONE',  ( -54.18398860626899705, 28.73617430169825226, 5.000000000000000000 ) ) ;
#143166 = EDGE_CURVE ( 'NONE', #108223, #59222, #107037, .T. ) ;
#143167 = DIRECTION ( 'NONE',  ( 0.6830127018922180770, -0.6830127018922204085, -0.2588190451025213501 ) ) ;
#143168 = LINE ( 'NONE', #319, #17346 ) ;
#143169 = DIRECTION ( 'NONE',  ( -1.000000000000000000, -0.000000000000000000, -0.000000000000000000 ) ) ;
#143170 = EDGE_CURVE ( 'NONE', #98588, #69496, #4824, .T. ) ;
#143171 = CARTESIAN_POINT ( 'NONE',  ( 66.41209685856478018, 5.291415217122922066, -3.054999999999995275 ) ) ;
#143172 = CARTESIAN_POINT ( 'NONE',  ( 0.000000000000000000, 0.000000000000000000, 7.950000000000000178 ) ) ;
#143173 = DIRECTION ( 'NONE',  ( -0.7071067811865487940, 0.7071067811865463515, -0.000000000000000000 ) ) ;
#143174 = DIRECTION ( 'NONE',  ( 0.6830127018922181881, 0.6830127018922202975, -0.2588190451025214056 ) ) ;
#143175 = CARTESIAN_POINT ( 'NONE',  ( 84.70833333333332860, -3.974999999999999201, -6.884901960086287964 ) ) ;
#143176 = VERTEX_POINT ( 'NONE', #6965 ) ;
#143177 = SURFACE_STYLE_USAGE ( .BOTH. , #79406 ) ;
#143178 = ORIENTED_EDGE ( 'NONE', *, *, #110594, .T. ) ;
#143179 = CARTESIAN_POINT ( 'NONE',  ( 125.7224624600519434, -47.70829528212279769, 34.92499999999998295 ) ) ;
#143180 = LINE ( 'NONE', #85948, #103161 ) ;
#143181 = VECTOR ( 'NONE', #128822, 1000.000000000000000 ) ;
#143182 = VECTOR ( 'NONE', #34754, 1000.000000000000000 ) ;
#143183 = DIRECTION ( 'NONE',  ( -0.000000000000000000, 0.3543493200069153248, 0.9351131265310292928 ) ) ;
#143184 = CARTESIAN_POINT ( 'NONE',  ( -66.48921356237309510, -27.52281430457101763, 5.000000000000000000 ) ) ;
#143185 = CIRCLE ( 'NONE', #92248, 4.000000000000000000 ) ;
#143186 = ADVANCED_FACE ( 'NONE', ( #60736 ), #84596, .T. ) ;
#143187 = CARTESIAN_POINT ( 'NONE',  ( -6.328169399223480873, 8.259292476615636147, 4.000000000000000000 ) ) ;
#143188 = EDGE_CURVE ( 'NONE', #137381, #46584, #128106, .T. ) ;
#143189 = CARTESIAN_POINT ( 'NONE',  ( 15.18398860626900237, 28.73617430169797871, 5.000000000000000000 ) ) ;
#143190 = DIRECTION ( 'NONE',  ( 0.7071067811865487940, -0.7071067811865463515, 0.000000000000000000 ) ) ;
#143191 = VERTEX_POINT ( 'NONE', #125958 ) ;
#143192 = ORIENTED_EDGE ( 'NONE', *, *, #58748, .T. ) ;
#143193 = DIRECTION ( 'NONE',  ( -1.000000000000000000, -0.000000000000000000, -0.000000000000000000 ) ) ;
#143194 = AXIS2_PLACEMENT_3D ( 'NONE', #105135, #126867, #27554 ) ;
#143195 = AXIS2_PLACEMENT_3D ( 'NONE', #25708, #60518, #71374 ) ;
#143196 = CARTESIAN_POINT ( 'NONE',  ( 61.46640106136307935, -43.14999999999999147, 34.92499999999998295 ) ) ;
#143197 = EDGE_CURVE ( 'NONE', #58012, #64733, #6253, .T. ) ;
#143198 = CARTESIAN_POINT ( 'NONE',  ( -39.29974487139159578, -27.71228299555233576, 4.000000000000000000 ) ) ;
#143199 = CARTESIAN_POINT ( 'NONE',  ( 88.30836038379622721, 7.949999999999997513, 2.130196079827431088 ) ) ;
#143200 = LINE ( 'NONE', #127705, #46370 ) ;
#143201 = CARTESIAN_POINT ( 'NONE',  ( -7.499999999999947597, 19.39370406404967184, 1.459788787078221128 ) ) ;
#143202 = ORIENTED_EDGE ( 'NONE', *, *, #57338, .T. ) ;
#143203 = CARTESIAN_POINT ( 'NONE',  ( 80.33333333333334281, -6.884901960086287964, 3.974999999999998312 ) ) ;
#143204 = CARTESIAN_POINT ( 'NONE',  ( 0.000000000000000000, 0.000000000000000000, 5.000000000000000000 ) ) ;
#143205 = LINE ( 'NONE', #107709, #53067 ) ;
#143206 = PLANE ( 'NONE',  #68328 ) ;
#143207 = ADVANCED_FACE ( 'NONE', ( #28790 ), #76874, .T. ) ;
#143208 = ORIENTED_EDGE ( 'NONE', *, *, #72877, .F. ) ;
#143209 = FACE_OUTER_BOUND ( 'NONE', #123560, .T. ) ;
#143210 = ORIENTED_EDGE ( 'NONE', *, *, #101302, .T. ) ;
#143211 = VECTOR ( 'NONE', #128912, 1000.000000000000000 ) ;
#143212 = CARTESIAN_POINT ( 'NONE',  ( -31.49999999999978684, -17.56887692260763956, 4.000000000000000000 ) ) ;
#143213 = CARTESIAN_POINT ( 'NONE',  ( 73.06293019189811844, 1.637169565754157174, 6.110000000000002984 ) ) ;
#143214 = LINE ( 'NONE', #87419, #119509 ) ;
#143215 = EDGE_CURVE ( 'NONE', #105497, #89784, #72329, .T. ) ;
#143216 = EDGE_LOOP ( 'NONE', ( #90239, #73320, #23102, #137494 ) ) ;
#143217 = CARTESIAN_POINT ( 'NONE',  ( 51.48921356237309510, -27.52281430457091460, 5.000000000000000000 ) ) ;
#143218 = AXIS2_PLACEMENT_3D ( 'NONE', #99102, #143344, #132520 ) ;
#143219 = CARTESIAN_POINT ( 'NONE',  ( 7.499999999999951150, 16.46639925780209879, 5.000000000000000000 ) ) ;
#143220 = DIRECTION ( 'NONE',  ( 0.7071067811865487940, 0.7071067811865463515, -0.000000000000000000 ) ) ;
#143221 = VECTOR ( 'NONE', #47939, 1000.000000000000000 ) ;
#143222 = CARTESIAN_POINT ( 'NONE',  ( 18.00548008471250583, 28.92564299267925776, 4.000000000000000000 ) ) ;
#143223 = DIRECTION ( 'NONE',  ( -0.7071067811865486830, -0.7071067811865464625, -0.000000000000000000 ) ) ;
#143225 = ORIENTED_EDGE ( 'NONE', *, *, #35943, .F. ) ;
#143224 = CARTESIAN_POINT ( 'NONE',  ( 127.0000000000000000, 1.564650039245123914, 6.154215649023822010 ) ) ;
#143226 = DIRECTION ( 'NONE',  ( 0.7071067811865487940, 0.7071067811865463515, 0.000000000000000000 ) ) ;
#143227 = CARTESIAN_POINT ( 'NONE',  ( 15.18398860626900237, 28.73617430169797871, 5.000000000000000000 ) ) ;
#143228 = DIRECTION ( 'NONE',  ( -0.000000000000000000, 0.000000000000000000, 1.000000000000000000 ) ) ;
#143229 = AXIS2_PLACEMENT_3D ( 'NONE', #4217, #89861, #46417 ) ;
#143230 = CARTESIAN_POINT ( 'NONE',  ( 28.82816939922332011, -14.24070752338414003, 4.000000000000000000 ) ) ;
#143231 = VERTEX_POINT ( 'NONE', #116496 ) ;
#143232 = EDGE_CURVE ( 'NONE', #122079, #861, #105590, .T. ) ;
#143233 = ORIENTED_EDGE ( 'NONE', *, *, #29957, .F. ) ;
#143234 = CARTESIAN_POINT ( 'NONE',  ( 60.22959685856476142, -6.110000000000000320, -1.637169565754161393 ) ) ;
#143235 = ORIENTED_EDGE ( 'NONE', *, *, #84301, .F. ) ;
#143236 = CARTESIAN_POINT ( 'NONE',  ( 42.18398860626899705, 28.73617430169816700, 5.000000000000000000 ) ) ;
#143237 = DIRECTION ( 'NONE',  ( 0.000000000000000000, -1.000000000000000000, 0.000000000000000000 ) ) ;
#143238 = CARTESIAN_POINT ( 'NONE',  ( 125.0583603837962272, -7.949999999999996625, -2.130196079827426203 ) ) ;
#143239 = DIRECTION ( 'NONE',  ( -0.7071067811865486830, -0.7071067811865464625, -0.000000000000000000 ) ) ;
#143240 = VERTEX_POINT ( 'NONE', #94712 ) ;
#143241 = VERTEX_POINT ( 'NONE', #39676 ) ;
#143242 = VECTOR ( 'NONE', #128020, 1000.000000000000000 ) ;
#143243 = LINE ( 'NONE', #96840, #107091 ) ;
#143244 = DIRECTION ( 'NONE',  ( 0.000000000000000000, 0.000000000000000000, 1.000000000000000000 ) ) ;
#143245 = VECTOR ( 'NONE', #49606, 1000.000000000000000 ) ;
#143246 = ORIENTED_EDGE ( 'NONE', *, *, #18258, .F. ) ;
#143247 = EDGE_CURVE ( 'NONE', #21912, #5925, #73031, .T. ) ;
#143248 = DIRECTION ( 'NONE',  ( -0.7071067811865486830, -0.7071067811865464625, 0.000000000000000000 ) ) ;
#143249 = LINE ( 'NONE', #73710, #38587 ) ;
#143250 = CARTESIAN_POINT ( 'NONE',  ( 12.48921356237309155, -27.52281430457064104, 5.000000000000000000 ) ) ;
#143251 = VERTEX_POINT ( 'NONE', #66416 ) ;
#143252 = ADVANCED_FACE ( 'NONE', ( #63581 ), #141084, .F. ) ;
#143253 = FACE_BOUND ( 'NONE', #98810, .T. ) ;
#143254 = DIRECTION ( 'NONE',  ( -0.7071067811865487940, 0.7071067811865463515, 0.000000000000000000 ) ) ;
#143255 = DIRECTION ( 'NONE',  ( 0.7071067811865487940, 0.7071067811865463515, 0.000000000000000000 ) ) ;
#143256 = DIRECTION ( 'NONE',  ( -0.6830127018922181881, 0.6830127018922202975, -0.2588190451025214056 ) ) ;
#143257 = PLANE ( 'NONE',  #133679 ) ;
#143258 = CARTESIAN_POINT ( 'NONE',  ( -20.27718569542926730, -21.72500000000000853, 5.000000000000000000 ) ) ;
#143259 = EDGE_LOOP ( 'NONE', ( #13818, #97872, #125173, #86747, #120406 ) ) ;
#143260 = ORIENTED_EDGE ( 'NONE', *, *, #130263, .F. ) ;
#143261 = CARTESIAN_POINT ( 'NONE',  ( 113.2245968585647802, -1.637169565754160949, 6.109999999999997655 ) ) ;
#143262 = VERTEX_POINT ( 'NONE', #20014 ) ;
#143263 = ORIENTED_EDGE ( 'NONE', *, *, #90587, .F. ) ;
#143264 = LINE ( 'NONE', #34509, #79434 ) ;
#143265 = LINE ( 'NONE', #77344, #77896 ) ;
#143266 = DIRECTION ( 'NONE',  ( 0.6830127018922180770, -0.6830127018922202975, -0.2588190451025213501 ) ) ;
#143267 = ORIENTED_EDGE ( 'NONE', *, *, #69450, .F. ) ;
#143268 = CARTESIAN_POINT ( 'NONE',  ( 68.18336038379621300, -2.130196079827426203, 7.949999999999996625 ) ) ;
#143269 = LINE ( 'NONE', #118664, #142244 ) ;
#143270 = EDGE_CURVE ( 'NONE', #138233, #74016, #33101, .T. ) ;
#143271 = FACE_BOUND ( 'NONE', #127259, .T. ) ;
#143273 = PLANE ( 'NONE',  #78183 ) ;
#143272 = LINE ( 'NONE', #54863, #124498 ) ;
#143274 = PLANE ( 'NONE',  #69312 ) ;
#143275 = VECTOR ( 'NONE', #3631, 1000.000000000000000 ) ;
#143276 = CIRCLE ( 'NONE', #18232, 2.500000000000000888 ) ;
#143277 = PLANE ( 'NONE',  #23568 ) ;
#143278 = ORIENTED_EDGE ( 'NONE', *, *, #70092, .F. ) ;
#143279 = LINE ( 'NONE', #76631, #82052 ) ;
#143280 = PLANE ( 'NONE',  #25704 ) ;
#143281 = VECTOR ( 'NONE', #142049, 1000.000000000000000 ) ;
#143282 = VERTEX_POINT ( 'NONE', #51967 ) ;
#143283 = EDGE_CURVE ( 'NONE', #66785, #99513, #88163, .T. ) ;
#143284 = ORIENTED_EDGE ( 'NONE', *, *, #9786, .T. ) ;
#143285 = EDGE_CURVE ( 'NONE', #128234, #109338, #98327, .T. ) ;
#143286 = EDGE_LOOP ( 'NONE', ( #35399, #3581, #117901, #42054, #39387, #140465 ) ) ;
#143287 = EDGE_CURVE ( 'NONE', #99346, #118799, #64263, .T. ) ;
#143288 = CARTESIAN_POINT ( 'NONE',  ( 62.12543019189810423, 5.291415217122919401, 3.055000000000002824 ) ) ;
#143289 = ORIENTED_EDGE ( 'NONE', *, *, #12154, .T. ) ;
#143290 = VECTOR ( 'NONE', #92160, 1000.000000000000227 ) ;
#143291 = DIRECTION ( 'NONE',  ( -0.000000000000000000, 0.3543493200069153248, 0.9351131265310292928 ) ) ;
#143292 = DIRECTION ( 'NONE',  ( -1.000000000000000000, -1.224606353822377258E-16, -0.000000000000000000 ) ) ;
#143294 =( BOUNDED_CURVE ( )  B_SPLINE_CURVE ( 3, ( #66293, #22040, #11138, #132995 ),
 .UNSPECIFIED., .F., .T. ) 
 B_SPLINE_CURVE_WITH_KNOTS ( ( 4, 4 ),
 ( 0.1773996044403779171, 1.570796326794896558 ),
 .UNSPECIFIED. ) 
 CURVE ( )  GEOMETRIC_REPRESENTATION_ITEM ( )  RATIONAL_B_SPLINE_CURVE ( ( 1.000000000000000000, 0.8446433258982485315, 0.8446433258982485315, 1.000000000000000000 ) ) 
 REPRESENTATION_ITEM ( '' )  );
#143293 = CARTESIAN_POINT ( 'NONE',  ( 98.87543019189810423, -5.291415217122920289, -3.055000000000001492 ) ) ;
#143295 = CARTESIAN_POINT ( 'NONE',  ( 34.92499999999998295, -2.993876922608006641, 4.000000000000000000 ) ) ;
#143296 = ORIENTED_EDGE ( 'NONE', *, *, #58353, .F. ) ;
#143297 = FACE_OUTER_BOUND ( 'NONE', #7750, .T. ) ;
#143298 = VECTOR ( 'NONE', #128383, 1000.000000000000000 ) ;
#143299 = CARTESIAN_POINT ( 'NONE',  ( 25.01459476339044130, 2.945717840782780428, 4.000000000000000000 ) ) ;
#143300 = EDGE_CURVE ( 'NONE', #54903, #5088, #116158, .T. ) ;
#143301 = CARTESIAN_POINT ( 'NONE',  ( 29.99999999999979394, 14.96639925780210056, 5.000000000000000000 ) ) ;
#143302 = ORIENTED_EDGE ( 'NONE', *, *, #87534, .F. ) ;
#143303 = AXIS2_PLACEMENT_3D ( 'NONE', #92530, #40349, #117844 ) ;
#143304 = CARTESIAN_POINT ( 'NONE',  ( 34.75611968250419181, 1.705650698524030062, 4.955485411084880276 ) ) ;
#143305 = EDGE_LOOP ( 'NONE', ( #59277, #62002, #20296, #24280 ) ) ;
#143306 = ORIENTED_EDGE ( 'NONE', *, *, #80011, .T. ) ;
#143307 = ORIENTED_EDGE ( 'NONE', *, *, #77214, .F. ) ;
#143308 = CARTESIAN_POINT ( 'NONE',  ( 124.4537635252314516, -6.109999999999998543, -3.741295971395162543E-16 ) ) ;
#143309 = ORIENTED_EDGE ( 'NONE', *, *, #132256, .F. ) ;
#143310 = VECTOR ( 'NONE', #11981, 1000.000000000000000 ) ;
#143311 = AXIS2_PLACEMENT_3D ( 'NONE', #106064, #129263, #105373 ) ;
#143312 = CARTESIAN_POINT ( 'NONE',  ( 9.328169399223463998, -15.74070752338411339, 4.000000000000000000 ) ) ;
#143313 = VECTOR ( 'NONE', #21570, 1000.000000000000227 ) ;
#143314 = DIRECTION ( 'NONE',  ( -0.3543493200069162685, -0.000000000000000000, -0.9351131265310288487 ) ) ;
#143315 = VERTEX_POINT ( 'NONE', #108428 ) ;
#143316 = CARTESIAN_POINT ( 'NONE',  ( 20.20666063542138247, 21.75929247661549581, 4.998822639870702744 ) ) ;
#143317 = EDGE_LOOP ( 'NONE', ( #47960, #25598, #33414, #8722 ) ) ;
#143318 = VECTOR ( 'NONE', #123058, 1000.000000000000000 ) ;
#143319 = AXIS2_PLACEMENT_3D ( 'NONE', #133325, #22367, #90524 ) ;
#143320 = CARTESIAN_POINT ( 'NONE',  ( 11.06206980810188689, -7.934999999999991616, -2.126176841940955242 ) ) ;
#143321 = CARTESIAN_POINT ( 'NONE',  ( 4.171830600776441855, 0.7592924766157120864, 4.000000000000000000 ) ) ;
#143322 = EDGE_CURVE ( 'NONE', #13795, #91413, #131667, .T. ) ;
#143323 = CARTESIAN_POINT ( 'NONE',  ( -60.29974487139158867, -27.71228299555248142, 4.000000000000000000 ) ) ;
#143324 = CARTESIAN_POINT ( 'NONE',  ( 34.49999999999976552, 3.054329344830917670, 4.994342998332163219 ) ) ;
#143325 = ORIENTED_EDGE ( 'NONE', *, *, #23653, .F. ) ;
#143326 = EDGE_CURVE ( 'NONE', #6884, #66617, #130246, .T. ) ;
#143327 = VERTEX_POINT ( 'NONE', #120023 ) ;
#143328 = EDGE_LOOP ( 'NONE', ( #108010, #123706, #37187, #81220 ) ) ;
#143329 = CARTESIAN_POINT ( 'NONE',  ( 57.58333333333333570, 6.884901960086290629, -3.974999999999994316 ) ) ;
#143330 = UNCERTAINTY_MEASURE_WITH_UNIT (LENGTH_MEASURE( 1.000000000000000082E-05 ), #116059, 'distance_accuracy_value', 'NONE');
#143331 = AXIS2_PLACEMENT_3D ( 'NONE', #110322, #123403, #79195 ) ;
#143332 = DIRECTION ( 'NONE',  ( -0.6830127018922180770, -0.6830127018922204085, -0.2588190451025213501 ) ) ;
#143333 = CARTESIAN_POINT ( 'NONE',  ( 0.000000000000000000, 0.000000000000000000, 5.000000000000000000 ) ) ;
#143334 = EDGE_CURVE ( 'NONE', #540, #124629, #43940, .T. ) ;
#143335 = EDGE_CURVE ( 'NONE', #117466, #70361, #25815, .T. ) ;
#143336 = CARTESIAN_POINT ( 'NONE',  ( 25.34840764549667469, 9.139736423841732040E-16, 0.000000000000000000 ) ) ;
#143337 = DIRECTION ( 'NONE',  ( 1.000000000000000000, 0.000000000000000000, 0.000000000000000000 ) ) ;
#143338 = LINE ( 'NONE', #88984, #11935 ) ;
#143339 = CARTESIAN_POINT ( 'NONE',  ( -11.33153258840135358, -18.74070752338409207, 20.73178291233838522 ) ) ;
#143340 = EDGE_LOOP ( 'NONE', ( #92172, #52736, #112175, #47386 ) ) ;
#143341 = DIRECTION ( 'NONE',  ( -0.6830127018922180770, -0.6830127018922204085, -0.2588190451025213501 ) ) ;
#143342 = EDGE_LOOP ( 'NONE', ( #74590, #83044, #88892, #85758, #117417, #131353 ) ) ;
#143343 = ORIENTED_EDGE ( 'NONE', *, *, #74441, .T. ) ;
#143344 = DIRECTION ( 'NONE',  ( 0.6830127018922180770, -0.6830127018922204085, -0.2588190451025213501 ) ) ;
#143346 = EDGE_LOOP ( 'NONE', ( #129862, #18718, #71623, #83898 ) ) ;
#143345 = DIRECTION ( 'NONE',  ( -0.6830127018922180770, -0.6830127018922204085, -0.2588190451025213501 ) ) ;
#143347 = EDGE_CURVE ( 'NONE', #36014, #139082, #109222, .T. ) ;
#143348 = EDGE_CURVE ( 'NONE', #19621, #91232, #37420, .T. ) ;
#143349 = FACE_OUTER_BOUND ( 'NONE', #28465, .T. ) ;
#143350 = ORIENTED_EDGE ( 'NONE', *, *, #78572, .F. ) ;
#143351 = PLANE ( 'NONE',  #104045 ) ;
#143352 = ORIENTED_EDGE ( 'NONE', *, *, #75926, .F. ) ;
#143353 = DIRECTION ( 'NONE',  ( -0.7071067811865486830, -0.7071067811865464625, -0.000000000000000000 ) ) ;
#143354 = UNCERTAINTY_MEASURE_WITH_UNIT (LENGTH_MEASURE( 1.000000000000000082E-05 ), #87968, 'distance_accuracy_value', 'NONE');
#143355 = ORIENTED_EDGE ( 'NONE', *, *, #72231, .F. ) ;
#143356 = PLANE ( 'NONE',  #59199 ) ;
#143357 = CARTESIAN_POINT ( 'NONE',  ( 116.0166937171295416, 7.950000000000001066, -2.130196079827421318 ) ) ;
#143358 = DIRECTION ( 'NONE',  ( 0.000000000000000000, 0.000000000000000000, 1.000000000000000000 ) ) ;
#143359 = ADVANCED_FACE ( 'NONE', ( #142548 ), #123121, .T. ) ;
#143360 = CARTESIAN_POINT ( 'NONE',  ( -25.39999999999996305, 0.000000000000000000, 2.500000000000000000 ) ) ;
#143361 = LINE ( 'NONE', #37482, #100188 ) ;
#143362 = DIRECTION ( 'NONE',  ( -0.6830127018922181881, 0.6830127018922202975, -0.2588190451025214056 ) ) ;
#143363 = LINE ( 'NONE', #9995, #117838 ) ;
#143364 = CARTESIAN_POINT ( 'NONE',  ( 15.45833333333333393, -3.047499999999997211, -5.278424836066143655 ) ) ;
#143365 = CARTESIAN_POINT ( 'NONE',  ( 17.91623647476855652, -7.934999999999990727, 4.858786175617117713E-16 ) ) ;
#143366 = ADVANCED_FACE ( 'NONE', ( #10563 ), #53373, .T. ) ;
#143367 = CARTESIAN_POINT ( 'NONE',  ( 33.18398860626899705, 28.73617430169810305, 5.000000000000000000 ) ) ;
#143368 = DIRECTION ( 'NONE',  ( -0.7071067811865486830, 0.7071067811865464625, 0.000000000000000000 ) ) ;
#143369 = VERTEX_POINT ( 'NONE', #125052 ) ;
#143370 = EDGE_LOOP ( 'NONE', ( #104804, #49515, #74225, #55671 ) ) ;
#143371 = CARTESIAN_POINT ( 'NONE',  ( 31.49999999999977973, 19.39370406404970026, 1.459788787078129202 ) ) ;
#143372 = VERTEX_POINT ( 'NONE', #80862 ) ;
#143373 = AXIS2_PLACEMENT_3D ( 'NONE', #21007, #142800, #65272 ) ;
#143374 = CARTESIAN_POINT ( 'NONE',  ( -1.001930566820972812, -22.22500000000000142, 4.500000000000000888 ) ) ;
#143375 = CARTESIAN_POINT ( 'NONE',  ( 3.250000000000000000, 0.000000000000000000, 9.119999999999999218 ) ) ;
#143376 = ADVANCED_FACE ( 'NONE', ( #36613 ), #89374, .F. ) ;
#143377 = DIRECTION ( 'NONE',  ( -0.6830127018922181881, 0.6830127018922202975, -0.2588190451025214056 ) ) ;
#143378 = EDGE_LOOP ( 'NONE', ( #66580, #47890, #73961, #81170, #139611, #73923 ) ) ;
#143379 = VECTOR ( 'NONE', #17398, 1000.000000000000000 ) ;
#143380 = VECTOR ( 'NONE', #61210, 1000.000000000000000 ) ;
#143381 = COLOUR_RGB ( '', 0.40784314, 0.44705882, 0.49803922) ;
#143382 = DIRECTION ( 'NONE',  ( -0.6830127018922181881, 0.6830127018922202975, -0.2588190451025214056 ) ) ;
#143383 = CARTESIAN_POINT ( 'NONE',  ( -8.721745484314221031, 8.259292476615634371, 11.78515199841148586 ) ) ;
#143384 = AXIS2_PLACEMENT_3D ( 'NONE', #117915, #96177, #28819 ) ;
#143385 = CARTESIAN_POINT ( 'NONE',  ( -12.69999999999998153, 3.061616997868383634E-16, -2.500000000000000444 ) ) ;
#143386 = FILL_AREA_STYLE ('',( #6585 ) ) ;
#143387 = CARTESIAN_POINT ( 'NONE',  ( 0.000000000000000000, 0.5999999999999987566, 4.749999999999999112 ) ) ;
#143390 = ORIENTED_EDGE ( 'NONE', *, *, #2782, .F. ) ;
#143389 = ADVANCED_FACE ( 'NONE', ( #103988 ), #114177, .F. ) ;
#143388 = DIRECTION ( 'NONE',  ( 0.000000000000000000, -1.000000000000000000, 0.000000000000000000 ) ) ;
#143391 = LINE ( 'NONE', #11413, #118668 ) ;
#143392 = EDGE_CURVE ( 'NONE', #29382, #77043, #26464, .T. ) ;
#143393 = DIRECTION ( 'NONE',  ( 0.000000000000000000, -2.242629915582283412E-16, 1.000000000000000000 ) ) ;
#143394 = LINE ( 'NONE', #44102, #89595 ) ;
#143395 = AXIS2_PLACEMENT_3D ( 'NONE', #29590, #139831, #41925 ) ;
#143396 = VERTEX_POINT ( 'NONE', #50364 ) ;
#143397 = EDGE_CURVE ( 'NONE', #97559, #60588, #138811, .T. ) ;
#143398 = ORIENTED_EDGE ( 'NONE', *, *, #17130, .F. ) ;
#143399 = ORIENTED_EDGE ( 'NONE', *, *, #16557, .T. ) ;
#143400 = CARTESIAN_POINT ( 'NONE',  ( 89.25043019189810423, 3.055000000000002824, -5.291415217122919401 ) ) ;
#143401 = ORIENTED_EDGE ( 'NONE', *, *, #77283, .T. ) ;
#143402 = CARTESIAN_POINT ( 'NONE',  ( 14.99999999999989875, -1.209798855135680418, 4.371887122346866050 ) ) ;
#143403 = VECTOR ( 'NONE', #147, 1000.000000000000000 ) ;
#143404 = CIRCLE ( 'NONE', #46167, 5.968999999999998529 ) ;
#143405 = DIRECTION ( 'NONE',  ( 0.7071067811865487940, -0.7071067811865463515, 0.000000000000000000 ) ) ;
#143406 = ORIENTED_EDGE ( 'NONE', *, *, #17465, .T. ) ;
#143407 = CARTESIAN_POINT ( 'NONE',  ( -10.82816939922345867, 12.75929247661558641, 4.000000000000000000 ) ) ;
#143408 = CARTESIAN_POINT ( 'NONE',  ( 150.3000000000000114, 6.349999999999997868, 0.000000000000000000 ) ) ;
#143409 = VECTOR ( 'NONE', #106077, 999.9999999999998863 ) ;
#143410 = CARTESIAN_POINT ( 'NONE',  ( 90.32876352523145158, 0.000000000000000000, -6.109999999999998543 ) ) ;
#143411 = EDGE_LOOP ( 'NONE', ( #121542, #57367, #82561, #68679 ) ) ;
#143412 = DIRECTION ( 'NONE',  ( 0.7071067811865486830, -0.7071067811865464625, -0.000000000000000000 ) ) ;
#143413 = CARTESIAN_POINT ( 'NONE',  ( 114.7500000000000000, -9.735942053221458872E-16, 7.950000000000000178 ) ) ;
#143414 = VECTOR ( 'NONE', #102437, 1000.000000000000000 ) ;
#143415 = AXIS2_PLACEMENT_3D ( 'NONE', #20491, #9615, #150 ) ;
#143416 = AXIS2_PLACEMENT_3D ( 'NONE', #84872, #129080, #61036 ) ;
#143417 = ORIENTED_EDGE ( 'NONE', *, *, #43332, .T. ) ;
#143418 = ORIENTED_EDGE ( 'NONE', *, *, #31670, .T. ) ;
#143419 = ORIENTED_EDGE ( 'NONE', *, *, #63030, .T. ) ;
#143420 = CARTESIAN_POINT ( 'NONE',  ( 0.000000000000000000, 0.000000000000000000, 5.000000000000000000 ) ) ;
#143421 = LINE ( 'NONE', #44128, #124138 ) ;
#143422 = DIRECTION ( 'NONE',  ( 1.000000000000000000, 0.000000000000000000, 0.000000000000000000 ) ) ;
#143423 = VECTOR ( 'NONE', #113246, 1000.000000000000000 ) ;
#143424 = CARTESIAN_POINT ( 'NONE',  ( 8.994519915287490619, 28.92564299267944250, 4.000000000000000000 ) ) ;
#143425 = CARTESIAN_POINT ( 'NONE',  ( 6.328169399223488867, -6.740707523384212863, 4.000000000000000000 ) ) ;
#143426 = ORIENTED_EDGE ( 'NONE', *, *, #139422, .T. ) ;
#143427 = VERTEX_POINT ( 'NONE', #127189 ) ;
#143428 = CARTESIAN_POINT ( 'NONE',  ( 4.712472949537106715, 0.000000000000000000, 6.094999999999989981 ) ) ;
#143429 = VERTEX_POINT ( 'NONE', #117031 ) ;
#143430 = ORIENTED_EDGE ( 'NONE', *, *, #72407, .T. ) ;
#143431 = VECTOR ( 'NONE', #79031, 1000.000000000000000 ) ;
#143432 = DIRECTION ( 'NONE',  ( 0.3543493200069162685, -0.000000000000000000, -0.9351131265310288487 ) ) ;
#143433 = ORIENTED_EDGE ( 'NONE', *, *, #104312, .F. ) ;
#143434 = FACE_OUTER_BOUND ( 'NONE', #116020, .T. ) ;
#143435 = DIRECTION ( 'NONE',  ( 0.000000000000000000, 0.000000000000000000, 1.000000000000000000 ) ) ;
#143436 = LINE ( 'NONE', #109388, #68777 ) ;
#143437 = DIRECTION ( 'NONE',  ( 0.7071067811865487940, 0.7071067811865463515, -0.000000000000000000 ) ) ;
#143438 = CARTESIAN_POINT ( 'NONE',  ( 118.8333333333333286, -6.884901960086287964, 3.974999999999998312 ) ) ;
#143439 = ORIENTED_EDGE ( 'NONE', *, *, #127401, .T. ) ;
#143440 = LINE ( 'NONE', #101369, #106599 ) ;
#143441 = ORIENTED_EDGE ( 'NONE', *, *, #127423, .F. ) ;
#143442 = ADVANCED_FACE ( 'NONE', ( #37346 ), #127935, .T. ) ;
#143443 = CARTESIAN_POINT ( 'NONE',  ( 24.39999999999999858, -16.48000000000005016, -33.92499999999998295 ) ) ;
#143444 = VERTEX_POINT ( 'NONE', #17698 ) ;
#143445 = CARTESIAN_POINT ( 'NONE',  ( -17.54016161050249423, 18.75929247661552779, 8.305906642995445566 ) ) ;
#143446 = VERTEX_POINT ( 'NONE', #104728 ) ;
#143448 = EDGE_CURVE ( 'NONE', #72122, #4103, #15538, .T. ) ;
#143447 = DIRECTION ( 'NONE',  ( -0.3543493200069163240, 0.000000000000000000, -0.9351131265310288487 ) ) ;
#143449 = ORIENTED_EDGE ( 'NONE', *, *, #82658, .F. ) ;
#143450 = EDGE_LOOP ( 'NONE', ( #6251, #118322, #127938, #53342, #68624 ) ) ;
#143451 = ORIENTED_EDGE ( 'NONE', *, *, #6383, .F. ) ;
#143452 = B_SPLINE_CURVE_WITH_KNOTS ( 'NONE', 3,
 ( #14255, #127863, #46945, #18321 ),
 .UNSPECIFIED., .F., .F.,
 ( 4, 4 ),
 ( 0.000000000000000000, 0.001824211539880347737 ),
 .UNSPECIFIED. ) ;
#143453 = CARTESIAN_POINT ( 'NONE',  ( 3.707106781186516375, -3.740707523384250166, 5.000000000000000000 ) ) ;
#143454 = CARTESIAN_POINT ( 'NONE',  ( 0.000000000000000000, 9.735942053221458872E-16, -7.950000000000000178 ) ) ;
#143455 = PLANE ( 'NONE',  #68132 ) ;
#143456 = CARTESIAN_POINT ( 'NONE',  ( 123.2295968585647756, -6.110000000000000320, -1.637169565754161393 ) ) ;
#143457 = PLANE ( 'NONE',  #21861 ) ;
#143458 = EDGE_CURVE ( 'NONE', #65352, #121929, #84440, .T. ) ;
#143459 = DIRECTION ( 'NONE',  ( 1.000000000000000000, 0.000000000000000000, 0.000000000000000000 ) ) ;
#143460 = DIRECTION ( 'NONE',  ( 0.000000000000000000, 0.000000000000000000, -1.000000000000000000 ) ) ;
#143461 = CARTESIAN_POINT ( 'NONE',  ( -72.48921356237309510, -27.52281430457106026, 5.000000000000000000 ) ) ;
#143462 = EDGE_CURVE ( 'NONE', #5504, #57540, #51494, .T. ) ;
#143463 = CARTESIAN_POINT ( 'NONE',  ( 22.53999999999999915, 9.521314400968980422E-16, 0.000000000000000000 ) ) ;
#143464 = DIRECTION ( 'NONE',  ( 0.000000000000000000, 0.3543493200069153248, 0.9351131265310291818 ) ) ;
#143465 = LINE ( 'NONE', #77539, #107343 ) ;
#143466 = ORIENTED_EDGE ( 'NONE', *, *, #55911, .T. ) ;
#143467 = ORIENTED_EDGE ( 'NONE', *, *, #116942, .T. ) ;
#143468 = AXIS2_PLACEMENT_3D ( 'NONE', #34320, #78547, #122749 ) ;
#143469 = ORIENTED_EDGE ( 'NONE', *, *, #2699, .T. ) ;
#143470 = CARTESIAN_POINT ( 'NONE',  ( 35.99451991528749772, 28.92564299267963079, 4.000000000000000000 ) ) ;
#143472 = EDGE_CURVE ( 'NONE', #9887, #141378, #138488, .T. ) ;
#143471 = VECTOR ( 'NONE', #15954, 1000.000000000000000 ) ;
#143473 = AXIS2_PLACEMENT_3D ( 'NONE', #96067, #34960, #79196 ) ;
#143474 = EDGE_LOOP ( 'NONE', ( #102988, #30151, #8608, #21772 ) ) ;
#143475 = AXIS2_PLACEMENT_3D ( 'NONE', #8139, #85010, #66143 ) ;
#143477 = EDGE_LOOP ( 'NONE', ( #50548, #115616, #118291, #44511 ) ) ;
#143476 = AXIS2_PLACEMENT_3D ( 'NONE', #89437, #80731, #57555 ) ;
#143478 = CARTESIAN_POINT ( 'NONE',  ( 127.0000000000000000, 7.950000000000000178, 0.000000000000000000 ) ) ;
#143479 = DIRECTION ( 'NONE',  ( 0.000000000000000000, -1.000000000000000000, 0.000000000000000000 ) ) ;
#143480 = DIRECTION ( 'NONE',  ( 0.7071067811865487940, 0.7071067811865463515, -0.000000000000000000 ) ) ;
#143481 = LINE ( 'NONE', #56538, #4648 ) ;
#143482 = ORIENTED_EDGE ( 'NONE', *, *, #114676, .T. ) ;
#143483 = LINE ( 'NONE', #66661, #71871 ) ;
#143484 = EDGE_CURVE ( 'NONE', #119248, #11479, #93147, .T. ) ;
#143486 = EDGE_LOOP ( 'NONE', ( #51238, #98368, #57675, #86786 ) ) ;
#143485 = VECTOR ( 'NONE', #2487, 1000.000000000000000 ) ;
#143487 = CARTESIAN_POINT ( 'NONE',  ( -34.92499999999999005, 2.729999999999986215, -36.39086428169088094 ) ) ;
#143489 = VECTOR ( 'NONE', #91625, 999.9999999999998863 ) ;
#143488 = CARTESIAN_POINT ( 'NONE',  ( 20.19206980810188767, -7.934999999999991616, -2.126176841940955242 ) ) ;
#143490 = ORIENTED_EDGE ( 'NONE', *, *, #47699, .F. ) ;
#143491 = CARTESIAN_POINT ( 'NONE',  ( 87.41209685856478018, 5.291415217122922066, -3.054999999999995275 ) ) ;
#143492 = CARTESIAN_POINT ( 'NONE',  ( 6.404891093144800429, -9.299077053091121314, -1.947765254981038696 ) ) ;
#143493 = FACE_OUTER_BOUND ( 'NONE', #85503, .T. ) ;
#143494 = ORIENTED_EDGE ( 'NONE', *, *, #136352, .F. ) ;
#143495 = ADVANCED_FACE ( 'NONE', ( #125790 ), #136635, .F. ) ;
#143496 = EDGE_LOOP ( 'NONE', ( #42848, #78309, #121282, #20853 ) ) ;
#143497 = ORIENTED_EDGE ( 'NONE', *, *, #1876, .T. ) ;
#143499 = AXIS2_PLACEMENT_3D ( 'NONE', #56603, #2119, #80466 ) ;
#143498 = DIRECTION ( 'NONE',  ( 0.000000000000000000, -1.000000000000000000, 0.000000000000000000 ) ) ;
#143500 = FACE_OUTER_BOUND ( 'NONE', #38946, .T. ) ;
#143502 = FACE_OUTER_BOUND ( 'NONE', #96418, .T. ) ;
#143501 = VECTOR ( 'NONE', #97735, 999.9999999999998863 ) ;
#143503 = DIRECTION ( 'NONE',  ( -0.7071067811865486830, 0.7071067811865464625, 0.000000000000000000 ) ) ;
#143504 = LINE ( 'NONE', #88439, #109760 ) ;
#143505 = ORIENTED_EDGE ( 'NONE', *, *, #68956, .F. ) ;
#143506 = ADVANCED_FACE ( 'NONE', ( #48214 ), #67672, .T. ) ;
#143507 = ADVANCED_FACE ( 'NONE', ( #82292 ), #98150, .F. ) ;
#143508 = DIRECTION ( 'NONE',  ( -0.7071067811865487940, 0.7071067811865463515, -0.000000000000000000 ) ) ;
#143509 = AXIS2_PLACEMENT_3D ( 'NONE', #116475, #95427, #83882 ) ;
#143510 = SURFACE_STYLE_USAGE ( .BOTH. , #46391 ) ;
#143511 = DIRECTION ( 'NONE',  ( -1.000000000000000000, -1.224606353822377258E-16, -0.000000000000000000 ) ) ;
#143512 = EDGE_LOOP ( 'NONE', ( #7529, #12778, #105137, #87289 ) ) ;
#143513 = DIRECTION ( 'NONE',  ( -0.7071067811865486830, -0.7071067811865464625, 0.000000000000000000 ) ) ;
#143514 = CIRCLE ( 'NONE', #39334, 2.500000000000000444 ) ;
#143517 = EDGE_CURVE ( 'NONE', #124853, #137018, #94012, .T. ) ;
#143516 = VECTOR ( 'NONE', #74763, 1000.000000000000000 ) ;
#143515 = CARTESIAN_POINT ( 'NONE',  ( 47.99451991528749062, 28.92564299267971251, 4.000000000000000000 ) ) ;
#143518 = VERTEX_POINT ( 'NONE', #74994 ) ;
#143520 = EDGE_LOOP ( 'NONE', ( #54585, #137432, #123632, #49037 ) ) ;
#143519 = LINE ( 'NONE', #97885, #48705 ) ;
#143522 = VERTEX_POINT ( 'NONE', #87270 ) ;
#143521 = EDGE_CURVE ( 'NONE', #37569, #46262, #131490, .T. ) ;
#143523 = VECTOR ( 'NONE', #100630, 1000.000000000000000 ) ;
#143524 = EDGE_CURVE ( 'NONE', #81752, #77753, #30014, .T. ) ;
#143525 = FACE_OUTER_BOUND ( 'NONE', #20262, .T. ) ;
#143526 = CIRCLE ( 'NONE', #81049, 0.5000000000000004441 ) ;
#143527 = CARTESIAN_POINT ( 'NONE',  ( -4.889826771117854243, -22.22500000000000497, 4.785647885939354751 ) ) ;
#143528 = ORIENTED_EDGE ( 'NONE', *, *, #82332, .F. ) ;
#143529 = DIRECTION ( 'NONE',  ( -1.000000000000000000, -0.000000000000000000, -0.000000000000000000 ) ) ;
#143530 = CARTESIAN_POINT ( 'NONE',  ( 13.71003237941630104, 5.842153316012715258, 5.000000000000000000 ) ) ;
#143531 = DIRECTION ( 'NONE',  ( 0.3543493200069162685, -0.000000000000000000, -0.9351131265310288487 ) ) ;
#143532 = VECTOR ( 'NONE', #110436, 1000.000000000000000 ) ;
#143533 = EDGE_CURVE ( 'NONE', #80177, #127309, #118450, .T. ) ;
#143534 = CARTESIAN_POINT ( 'NONE',  ( 10.83999999999999986, 2.055000000000001492, 2.516649172247811554E-16 ) ) ;
#143535 = PLANE ( 'NONE',  #118360 ) ;
#143536 = LINE ( 'NONE', #67433, #86217 ) ;
#143537 = LINE ( 'NONE', #134105, #104978 ) ;
#143539 = VECTOR ( 'NONE', #46618, 999.9999999999998863 ) ;
#143538 = CARTESIAN_POINT ( 'NONE',  ( 22.58290314143522082, 3.967499999999992699, -6.871911579029513994 ) ) ;
#143540 = CARTESIAN_POINT ( 'NONE',  ( 7.499999999999951150, -11.94781430457070570, 5.000000000000000000 ) ) ;
#143541 = DIRECTION ( 'NONE',  ( -0.000000000000000000, 5.559056632600921604E-15, -1.000000000000000000 ) ) ;
#143542 = EDGE_CURVE ( 'NONE', #58304, #78029, #20557, .T. ) ;
#143543 = CARTESIAN_POINT ( 'NONE',  ( 111.1041666666666714, 2.130196079827422206, 7.950000000000001954 ) ) ;
#143544 = PLANE ( 'NONE',  #24615 ) ;
#143545 = ORIENTED_EDGE ( 'NONE', *, *, #121887, .T. ) ;
#143546 = VERTEX_POINT ( 'NONE', #31467 ) ;
#143547 = CARTESIAN_POINT ( 'NONE',  ( 101.0416666666666714, -3.975000000000002753, 6.884901960086286188 ) ) ;
#143548 = ORIENTED_EDGE ( 'NONE', *, *, #79847, .F. ) ;
#143549 = ORIENTED_EDGE ( 'NONE', *, *, #59867, .F. ) ;
#143550 = ORIENTED_EDGE ( 'NONE', *, *, #43374, .T. ) ;
#143551 = DIRECTION ( 'NONE',  ( 0.3543493200069162685, -0.000000000000000000, -0.9351131265310288487 ) ) ;
#143552 = LINE ( 'NONE', #45011, #104253 ) ;
#143553 = VECTOR ( 'NONE', #53825, 1000.000000000000000 ) ;
#143554 = ORIENTED_EDGE ( 'NONE', *, *, #15759, .T. ) ;
#143555 = CARTESIAN_POINT ( 'NONE',  ( 34.75611968250419181, -16.29434930147578342, 4.955485411084881164 ) ) ;
#143556 = NEXT_ASSEMBLY_USAGE_OCCURRENCE ( 'NAUO1', ' ', ' ', #82917, #37749, $ ) ;
#143557 = NEXT_ASSEMBLY_USAGE_OCCURRENCE ( 'NAUO2', ' ', ' ', #82917, #14658, $ ) ;
#143558 = NEXT_ASSEMBLY_USAGE_OCCURRENCE ( 'NAUO3', ' ', ' ', #82917, #12014, $ ) ;
#143559 = NEXT_ASSEMBLY_USAGE_OCCURRENCE ( 'NAUO4', ' ', ' ', #82917, #104142, $ ) ;
#143560 = NEXT_ASSEMBLY_USAGE_OCCURRENCE ( 'NAUO5', ' ', ' ', #82917, #104142, $ ) ;
#143561 = NEXT_ASSEMBLY_USAGE_OCCURRENCE ( 'NAUO6', ' ', ' ', #82917, #114782, $ ) ;
#143562 = NEXT_ASSEMBLY_USAGE_OCCURRENCE ( 'NAUO7', ' ', ' ', #82917, #114782, $ ) ;
#143563 = NEXT_ASSEMBLY_USAGE_OCCURRENCE ( 'NAUO8', ' ', ' ', #82917, #91726, $ ) ;
#143564 = NEXT_ASSEMBLY_USAGE_OCCURRENCE ( 'NAUO9', ' ', ' ', #82917, #87323, $ ) ;
#143565 = NEXT_ASSEMBLY_USAGE_OCCURRENCE ( 'NAUO10', ' ', ' ', #82917, #110370, $ ) ;
#143566 = NEXT_ASSEMBLY_USAGE_OCCURRENCE ( 'NAUO11', ' ', ' ', #82917, #110370, $ ) ;
#143567 = NEXT_ASSEMBLY_USAGE_OCCURRENCE ( 'NAUO12', ' ', ' ', #82917, #128095, $ ) ;
#143568 = NEXT_ASSEMBLY_USAGE_OCCURRENCE ( 'NAUO13', ' ', ' ', #82917, #128095, $ ) ;
#143569 = NEXT_ASSEMBLY_USAGE_OCCURRENCE ( 'NAUO14', ' ', ' ', #82917, #128095, $ ) ;
#143570 = NEXT_ASSEMBLY_USAGE_OCCURRENCE ( 'NAUO15', ' ', ' ', #82917, #128095, $ ) ;
#143571 = NEXT_ASSEMBLY_USAGE_OCCURRENCE ( 'NAUO16', ' ', ' ', #82917, #22636, $ ) ;
#143572 = NEXT_ASSEMBLY_USAGE_OCCURRENCE ( 'NAUO17', ' ', ' ', #82917, #117397, $ ) ;
#143573 = NEXT_ASSEMBLY_USAGE_OCCURRENCE ( 'NAUO18', ' ', ' ', #82917, #117397, $ ) ;
#143574 = NEXT_ASSEMBLY_USAGE_OCCURRENCE ( 'NAUO19', ' ', ' ', #82917, #46631, $ ) ;
#143575 = NEXT_ASSEMBLY_USAGE_OCCURRENCE ( 'NAUO20', ' ', ' ', #82917, #46631, $ ) ;
ENDSEC;
END-ISO-10303-21;
